#41789 = CARTESIAN_POINT ( 'NONE',  ( -1.193521905106661674, 2.660739321503277841E-15, -0.3464511005275191513 ) ) ;
#41790 = CARTESIAN_POINT ( 'NONE',  ( -0.03443470937339728616, 0.2929341459200028863, -1.635441089090149402 ) ) ;
#41791 = CARTESIAN_POINT ( 'NONE',  ( -0.3917322834645670104, -0.1049643490035307020, -1.774953698983938954 ) ) ;
#41792 = CARTESIAN_POINT ( 'NONE',  ( 0.9317585301837276734, 0.05413385826771626580, -0.4176697321401330321 ) ) ;
#41793 = CARTESIAN_POINT ( 'NONE',  ( 0.07217847769028949700, -0.05778040916215560624, -0.4822834645669293319 ) ) ;
#41794 = CARTESIAN_POINT ( 'NONE',  ( -0.9711286089238838626, 0.2306618581243847221, -0.2411417322834647770 ) ) ;
#41795 = CARTESIAN_POINT ( 'NONE',  ( 1.069553805774278610, -0.6692913385826771977, 0.1292274648535927661 ) ) ;
#41796 = CARTESIAN_POINT ( 'NONE',  ( 0.4199475065616805614, 0.2306618581243848609, 0.2411417322834645549 ) ) ;
#41797 = CARTESIAN_POINT ( 'NONE',  ( 0.3917322834645670104, 2.398668435337828261E-17, -0.8326771653543307838 ) ) ;
#41798 = CARTESIAN_POINT ( 'NONE',  ( -0.4527559055118102749, 0.1660481256975885056, 0.3530559997133364547 ) ) ;
#41799 = CARTESIAN_POINT ( 'NONE',  ( 0.7742782152230979209, 0.05413385826771626580, -0.4176697321401330321 ) ) ;
#41800 = CARTESIAN_POINT ( 'NONE',  ( -0.05905511811023545637, 0.1660481256975885056, 0.3530559997133364547 ) ) ;
#41801 = CARTESIAN_POINT ( 'NONE',  ( 0.7545931758530189937, 0.1771653543307087075, -0.09757992244046823083 ) ) ;
#41802 = CARTESIAN_POINT ( 'NONE',  ( -1.430446194225721390, -0.4281496062992124485, 0.4176697321401328655 ) ) ;
#41803 = CARTESIAN_POINT ( 'NONE',  ( -1.686351706036744558, 0.2952755905511810774, -0.1292274648535930714 ) ) ;
#41804 = CARTESIAN_POINT ( 'NONE',  ( 0.4527559055118117182, -0.5400638737290844871, 0.3530559997133364547 ) ) ;
#41805 = EDGE_CURVE ( 'NONE', #71856, #73064, #4911, .T. ) ;
#41806 = CARTESIAN_POINT ( 'NONE',  ( 0.2867679344610365999, 0.2867679344610365999, -2.334645669291338432 ) ) ;
#41807 = VERTEX_POINT ( 'NONE', #35373 ) ;
#41808 = VERTEX_POINT ( 'NONE', #64973 ) ;
#41809 = CARTESIAN_POINT ( 'NONE',  ( 1.161417322834646493, -0.5400638737290844871, 0.3530559997133364547 ) ) ;
#41810 = CARTESIAN_POINT ( 'NONE',  ( 0.4527559055118117182, -0.4536011799217367080, 0.2665933059059888421 ) ) ;
#41812 = DIRECTION ( 'NONE',  ( -3.491481338843132961E-15, -0.000000000000000000, 1.000000000000000000 ) ) ;
#41811 = LINE ( 'NONE', #20916, #33728 ) ;
#41813 = CARTESIAN_POINT ( 'NONE',  ( 0.2867679344610365999, 0.2867679344610365999, -0.8523622047244096001 ) ) ;
#41814 = CARTESIAN_POINT ( 'NONE',  ( -0.4744094488189106174, 1.537401574803149984, 3.908320185825790105 ) ) ;
#41815 = SURFACE_STYLE_FILL_AREA ( #9842 ) ;
#41816 = CARTESIAN_POINT ( 'NONE',  ( -0.3917322834645671215, 0.1049643490035301469, -1.377296587926508664 ) ) ;
#41817 = CARTESIAN_POINT ( 'NONE',  ( -0.3996062992125986590, 0.1070741851644051723, -2.471784776902887337 ) ) ;
#41818 = CARTESIAN_POINT ( 'NONE',  ( 0.9973753280839902091, 0.2306618581243847221, -0.2411417322834647770 ) ) ;
#41819 = CARTESIAN_POINT ( 'NONE',  ( -0.7020997375328074108, -0.05778040916215522460, 0.4822834645669289988 ) ) ;
#41820 = CARTESIAN_POINT ( 'NONE',  ( -0.8530183727034112984, -0.4281496062992127816, -0.4176697321401328100 ) ) ;
#41821 = CARTESIAN_POINT ( 'NONE',  ( 0.6758530183727039509, 0.2952755905511810774, -0.1292274648535930714 ) ) ;
#41822 = ORIENTED_EDGE ( 'NONE', *, *, #38303, .F. ) ;
#41823 = CIRCLE ( 'NONE', #47171, 1.122047244094488194 ) ;
#41824 = CARTESIAN_POINT ( 'NONE',  ( 1.259842519685040019, -0.1870078740157479769, 0.4822834645669291653 ) ) ;
#41825 = CARTESIAN_POINT ( 'NONE',  ( -1.028258860871784197, 1.383740025641660543, 0.4491090030276655432 ) ) ;
#41826 = PRODUCT_CONTEXT ( 'NONE', #9492, 'mechanical' ) ;
#41827 = DIRECTION ( 'NONE',  ( 1.000000000000000000, -0.000000000000000000, -0.000000000000000000 ) ) ;
#41828 = CARTESIAN_POINT ( 'NONE',  ( -3.937007874015748143, 2.559055118110236560, 0.3149606299212596716 ) ) ;
#41829 = CARTESIAN_POINT ( 'NONE',  ( -1.187664041994749731, -0.2845877964562159024, 0.3641732283464567677 ) ) ;
#41830 = CARTESIAN_POINT ( 'NONE',  ( -0.3917322834645669549, -0.1049643490035306603, 0.1194225721784776956 ) ) ;
#41831 = CARTESIAN_POINT ( 'NONE',  ( 0.1181102362204730916, 0.2952755905511811885, 0.000000000000000000 ) ) ;
#41833 = DIRECTION ( 'NONE',  ( -0.000000000000000000, -1.000000000000000000, -0.000000000000000000 ) ) ;
#41832 = CARTESIAN_POINT ( 'NONE',  ( 1.555118110236221041, 0.1660481256975883668, -0.3530559997133364547 ) ) ;
#41834 = CARTESIAN_POINT ( 'NONE',  ( -1.286089238845143479, -0.5023911411419708095, 0.1820866141732285504 ) ) ;
#41835 = CARTESIAN_POINT ( 'NONE',  ( 0.2230971128608932319, -0.4281496062992124485, 0.4176697321401328655 ) ) ;
#41836 = CARTESIAN_POINT ( 'NONE',  ( 1.167979002624672580, -0.004921259842519870586, -0.3153832671262229437 ) ) ;
#41837 = CARTESIAN_POINT ( 'NONE',  ( 0.1958661417322836162, -0.3392501089628018329, -1.431739214401887894 ) ) ;
#41838 = CARTESIAN_POINT ( 'NONE',  ( -1.266404199475064773, -0.2845877964562159024, 0.3641732283464567677 ) ) ;
#41839 = CARTESIAN_POINT ( 'NONE',  ( 1.568241469816273659, -0.05778040916215560624, -0.4822834645669293319 ) ) ;
#41840 = CARTESIAN_POINT ( 'NONE',  ( 0.2710477321170861043, 1.856769674693915295, 0.1570371412841552461 ) ) ;
#41841 = CARTESIAN_POINT ( 'NONE',  ( -0.3477690288713905509, -0.6692913385826771977, 0.1292274648535927661 ) ) ;
#41842 = CARTESIAN_POINT ( 'NONE',  ( -1.456692913385826182, 0.1771653543307087630, 0.000000000000000000 ) ) ;
#41843 = CARTESIAN_POINT ( 'NONE',  ( -0.5118110236220466680, -0.5511811023622047445, 6.969142054262312111E-17 ) ) ;
#41844 = VECTOR ( 'NONE', #7052, 39.37007874015748143 ) ;
#41845 = CARTESIAN_POINT ( 'NONE',  ( -0.6496062992125976043, -0.5400638737290844871, 0.3530559997133364547 ) ) ;
#41846 = CARTESIAN_POINT ( 'NONE',  ( -1.574803149606298192, -0.1870078740157480601, -0.3641732283464567677 ) ) ;
#41847 = CARTESIAN_POINT ( 'NONE',  ( -0.2867679344610367109, 0.2867679344610365444, -0.6463447750994246732 ) ) ;
#41848 = CARTESIAN_POINT ( 'NONE',  ( 0.3477690288713918276, 0.2952755905511811885, 0.1292274648535926551 ) ) ;
#41849 = DIRECTION ( 'NONE',  ( 0.000000000000000000, 1.000000000000000000, 0.000000000000000000 ) ) ;
#41850 = CARTESIAN_POINT ( 'NONE',  ( -0.2362204724409447953, -0.4091458600556404646, -2.032152230971128848 ) ) ;
#41851 = CARTESIAN_POINT ( 'NONE',  ( -1.154855643044618851, -0.6046776061558809534, -0.2411417322834644161 ) ) ;
#41852 = CARTESIAN_POINT ( 'NONE',  ( -0.6561679790026240244, -0.5023911411419708095, 0.1820866141732285504 ) ) ;
#41853 = CARTESIAN_POINT ( 'NONE',  ( 1.171093442848939681, -8.644661201599092366E-16, -0.4445507791589066171 ) ) ;
#41854 = CARTESIAN_POINT ( 'NONE',  ( 0.2230971128608932319, -0.4281496062992124485, 0.4176697321401328655 ) ) ;
#41855 = CARTESIAN_POINT ( 'NONE',  ( 0.2624671916010504757, 0.1283753931104748280, 0.1820866141732283561 ) ) ;
#41856 = CARTESIAN_POINT ( 'NONE',  ( -0.6430446194225716283, -0.3690944881889763329, 0.3153832671262228327 ) ) ;
#41857 = CARTESIAN_POINT ( 'NONE',  ( -1.332020997375327642, -0.3162353388693409650, -0.4822834645669289433 ) ) ;
#41858 = CARTESIAN_POINT ( 'NONE',  ( -1.397637795275589623, 0.1660481256975885056, 0.3530559997133364547 ) ) ;
#41859 = CARTESIAN_POINT ( 'NONE',  ( 1.318897637795276356, -0.5400638737290844871, 0.3530559997133364547 ) ) ;
#41860 = DIRECTION ( 'NONE',  ( -3.491481338843132961E-15, -0.000000000000000000, 1.000000000000000000 ) ) ;
#41861 = CARTESIAN_POINT ( 'NONE',  ( 0.5314960629921267055, -0.4536011799217367080, 0.2665933059059888421 ) ) ;
#41862 = CARTESIAN_POINT ( 'NONE',  ( 0.9645669291338591078, -0.5400638737290845981, -0.3530559997133363437 ) ) ;
#41863 = CARTESIAN_POINT ( 'NONE',  ( 0.7086614173228347191, 0.000000000000000000, 0.000000000000000000 ) ) ;
#41864 = CARTESIAN_POINT ( 'NONE',  ( 1.377952755905512472, -0.5511811023622047445, 6.969142054262312111E-17 ) ) ;
#41865 = VERTEX_POINT ( 'NONE', #61038 ) ;
#41867 = B_SPLINE_CURVE_WITH_KNOTS ( 'NONE', 3,
 ( #58980, #19847, #3401, #34974 ),
 .UNSPECIFIED., .F., .F.,
 ( 4, 4 ),
 ( 0.02793953716399259421, 0.02824248980525632252 ),
 .UNSPECIFIED. ) ;
#41866 = CARTESIAN_POINT ( 'NONE',  ( -1.056430446194224881, -0.6692913385826771977, 0.1292274648535927661 ) ) ;
#41868 = CARTESIAN_POINT ( 'NONE',  ( -0.8398950131233585692, 0.2306618581243848609, 0.2411417322834645549 ) ) ;
#41869 = CARTESIAN_POINT ( 'NONE',  ( 0.1902887139107617975, 0.2952755905511811885, 0.1292274648535926551 ) ) ;
#41870 = CARTESIAN_POINT ( 'NONE',  ( -1.279527559055116948, -0.4536011799217367080, 0.2665933059059888421 ) ) ;
#41871 = CARTESIAN_POINT ( 'NONE',  ( -0.3996062992125984925, -0.1070741851644056858, -2.169947506561679340 ) ) ;
#41872 = CARTESIAN_POINT ( 'NONE',  ( 1.535433070866142335, -0.5511811023622047445, 6.969142054262312111E-17 ) ) ;
#41873 = CARTESIAN_POINT ( 'NONE',  ( 0.5577427821522316087, -0.05778040916215522460, 0.4822834645669289988 ) ) ;
#41874 = CARTESIAN_POINT ( 'NONE',  ( 0.7152230971128614723, -0.3162353388693409650, -0.4822834645669289433 ) ) ;
#41875 = CARTESIAN_POINT ( 'NONE',  ( 1.535433070866142558, 0.2952755905511811885, 0.000000000000000000 ) ) ;
#41876 = CARTESIAN_POINT ( 'NONE',  ( 0.2925321140481932369, -0.2925321140481932369, -1.673228346456692828 ) ) ;
#41877 = CARTESIAN_POINT ( 'NONE',  ( 0.3420746716998659953, 0.1974969037888705536, -0.9186351706036742781 ) ) ;
#41878 = CARTESIAN_POINT ( 'NONE',  ( 0.3996062992125986035, 0.1070741851644054776, -2.486876640419947382 ) ) ;
#41879 = CARTESIAN_POINT ( 'NONE',  ( -0.1228903193441467367, -0.2686849592492765448, 0.1574803149606299191 ) ) ;
#41880 = CARTESIAN_POINT ( 'NONE',  ( -0.3917322834645669549, -0.1049643490035306603, -0.03805774278215218187 ) ) ;
#41881 = CARTESIAN_POINT ( 'NONE',  ( -0.1837270341207343505, -0.5023911411419708095, 0.1820866141732285504 ) ) ;
#41882 = AXIS2_PLACEMENT_3D ( 'NONE', #65852, #51518, #8185 ) ;
#41883 = CARTESIAN_POINT ( 'NONE',  ( -0.1771653543307080136, -0.5400638737290844871, 0.3530559997133364547 ) ) ;
#41884 = CARTESIAN_POINT ( 'NONE',  ( 0.8792650918635177559, -0.4281496062992127816, -0.4176697321401328100 ) ) ;
#41885 = CARTESIAN_POINT ( 'NONE',  ( -0.3949938075777409963, -7.255918531996591613E-17, -2.320866141732283339 ) ) ;
#41886 = CARTESIAN_POINT ( 'NONE',  ( -0.1902887139107604098, 0.1771653543307087075, -0.09757992244046823083 ) ) ;
#41887 = CARTESIAN_POINT ( 'NONE',  ( -1.259842519685038686, -0.1870078740157480879, -0.4822834645669291653 ) ) ;
#41888 = CARTESIAN_POINT ( 'NONE',  ( 1.135170603674541256, 0.2952755905511811885, 0.1292274648535926551 ) ) ;
#41889 = CARTESIAN_POINT ( 'NONE',  ( 0.4724409448818896462, 0.1265901696524990294, -2.329396325459317296 ) ) ;
#41890 = CARTESIAN_POINT ( 'NONE',  ( 0.3460692066303959757, -0.1998031496062991907, -1.679790026246719137 ) ) ;
#41891 = CARTESIAN_POINT ( 'NONE',  ( 0.4498537592782897998, 0.000000000000000000, -2.118110236220472675 ) ) ;
#41892 = ORIENTED_EDGE ( 'NONE', *, *, #40415, .F. ) ;
#41893 = VERTEX_POINT ( 'NONE', #45169 ) ;
#41894 = CARTESIAN_POINT ( 'NONE',  ( 0.8530183727034126306, 0.05413385826771626580, -0.4176697321401330321 ) ) ;
#41895 = CARTESIAN_POINT ( 'NONE',  ( 1.614173228346457378, 0.1771653543307087630, 0.000000000000000000 ) ) ;
#41897 = CARTESIAN_POINT ( 'NONE',  ( -1.633858267716534529, 0.1660481256975885056, 0.3530559997133364547 ) ) ;
#41896 = CARTESIAN_POINT ( 'NONE',  ( -1.469816272965878357, 0.1283753931104748280, 0.1820866141732283561 ) ) ;
#41898 = CARTESIAN_POINT ( 'NONE',  ( -0.1958661417322836718, 0.3392501089628017219, 0.2171916010498686767 ) ) ;
#41899 = FACE_OUTER_BOUND ( 'NONE', #2999, .T. ) ;
#41900 = CARTESIAN_POINT ( 'NONE',  ( 1.325459317585302665, -0.4281496062992124485, 0.4176697321401328655 ) ) ;
#41901 = CARTESIAN_POINT ( 'NONE',  ( -1.456692913385826182, -0.6692913385826771977, 8.415575281601705876E-17 ) ) ;
#41902 = CARTESIAN_POINT ( 'NONE',  ( 0.04593175853018440641, 0.2952755905511810774, -0.1292274648535930714 ) ) ;
#41903 = CARTESIAN_POINT ( 'NONE',  ( -0.7349081364829390672, 0.2306618581243847221, -0.2411417322834647770 ) ) ;
#41904 = CARTESIAN_POINT ( 'NONE',  ( -1.614173228346455824, 0.2952755905511811885, 0.000000000000000000 ) ) ;
#41905 = CARTESIAN_POINT ( 'NONE',  ( -0.3392501089628019995, 0.1958661417322832277, -0.1108923884514436548 ) ) ;
#41906 = CARTESIAN_POINT ( 'NONE',  ( 0.03937007874015806264, 0.2952755905511811885, 0.000000000000000000 ) ) ;
#41907 = CARTESIAN_POINT ( 'NONE',  ( -0.2867679344610365999, 0.2867679344610364889, -2.216535433070866201 ) ) ;
#41908 = CARTESIAN_POINT ( 'NONE',  ( -1.174540682414697335, -0.08942795157527998196, 0.3641732283464567121 ) ) ;
#41909 = ORIENTED_EDGE ( 'NONE', *, *, #30007, .F. ) ;
#41910 = CARTESIAN_POINT ( 'NONE',  ( 0.2891555358219910499, -0.2891555358219909944, -2.145669291338582862 ) ) ;
#41911 = ORIENTED_EDGE ( 'NONE', *, *, #74772, .F. ) ;
#41912 = CARTESIAN_POINT ( 'NONE',  ( 0.3149606299212184823, 2.165354330708661568, 3.924389226575471845 ) ) ;
#41913 = CARTESIAN_POINT ( 'NONE',  ( -1.568241469816272105, -0.05778040916215522460, 0.4822834645669289988 ) ) ;
#41914 = CARTESIAN_POINT ( 'NONE',  ( -0.3996062992125987146, 0.1070741851644051862, -1.135170603674540590 ) ) ;
#41915 = CARTESIAN_POINT ( 'NONE',  ( 1.646981627296588035, -0.2845877964562159024, 0.3641732283464567677 ) ) ;
#41916 = CARTESIAN_POINT ( 'NONE',  ( -1.706036745406823485, 0.2306618581243848609, 0.2411417322834645549 ) ) ;
#41917 = DIRECTION ( 'NONE',  ( 0.000000000000000000, 1.408710688920637755E-15, -1.000000000000000000 ) ) ;
#41918 = CARTESIAN_POINT ( 'NONE',  ( 0.001150535885519430191, -0.3985446848723403490, -2.755905511811024500 ) ) ;
#41919 = EDGE_CURVE ( 'NONE', #27207, #69303, #32558, .T. ) ;
#41920 = CARTESIAN_POINT ( 'NONE',  ( 0.2867679344610365999, 0.2867679344610365999, 0.09251968503937001154 ) ) ;
#41921 = CARTESIAN_POINT ( 'NONE',  ( -0.1312335958005241554, -0.5023911411419708095, -0.1820866141732282451 ) ) ;
#41922 = CARTESIAN_POINT ( 'NONE',  ( -0.8858267716535425107, 0.07958543189024071263, -0.2665933059059888421 ) ) ;
#41923 = CARTESIAN_POINT ( 'NONE',  ( -1.358267716535432434, -0.5400638737290844871, 0.3530559997133364547 ) ) ;
#41924 = EDGE_CURVE ( 'NONE', #1065, #20923, #2072, .T. ) ;
#41925 = CARTESIAN_POINT ( 'NONE',  ( 0.3805774278215230400, 0.05413385826771626580, -0.4176697321401330321 ) ) ;
#41926 = CARTESIAN_POINT ( 'NONE',  ( -1.430446194225720724, 0.05413385826771626580, -0.4176697321401330321 ) ) ;
#41927 = CARTESIAN_POINT ( 'NONE',  ( 0.3392501089628018884, -0.1958661417322834220, 0.06036745406824151755 ) ) ;
#41928 = ORIENTED_EDGE ( 'NONE', *, *, #79506, .T. ) ;
#41929 = CARTESIAN_POINT ( 'NONE',  ( -1.574803149606298192, -0.1870078740157480879, -0.4822834645669291653 ) ) ;
#41930 = CARTESIAN_POINT ( 'NONE',  ( -1.646051170424378096, 0.000000000000000000, 0.3464511005275205946 ) ) ;
#41931 = CARTESIAN_POINT ( 'NONE',  ( 5.785732909357575061E-17, -0.4724409448818898682, -1.496062992125984259 ) ) ;
#41932 = CARTESIAN_POINT ( 'NONE',  ( 2.077234194078037000, 1.326002914239475805, -0.4256865378621398355 ) ) ;
#41933 = CARTESIAN_POINT ( 'NONE',  ( 0.3917322834645669549, 0.1049643490035304660, -0.7467191601049868455 ) ) ;
#41934 = CARTESIAN_POINT ( 'NONE',  ( -0.3392501089628017219, -0.1958661417322836718, -2.656824146981627166 ) ) ;
#41935 = CARTESIAN_POINT ( 'NONE',  ( -0.7020997375328074108, -0.05778040916215522460, 0.4822834645669289988 ) ) ;
#41936 = CARTESIAN_POINT ( 'NONE',  ( 1.535433070866142558, 0.2952755905511811885, 0.000000000000000000 ) ) ;
#41938 = CARTESIAN_POINT ( 'NONE',  ( -0.4724409448818898682, -8.678599364036362592E-17, -0.1968503937007874127 ) ) ;
#41937 = CARTESIAN_POINT ( 'NONE',  ( -1.686351706036744558, 0.2952755905511810774, -0.1292274648535930714 ) ) ;
#41939 = CARTESIAN_POINT ( 'NONE',  ( -1.561679790026246017, 0.05413385826771666132, 0.4176697321401328100 ) ) ;
#41940 = CARTESIAN_POINT ( 'NONE',  ( -1.003937007874015297, -0.5400638737290845981, -0.3530559997133363437 ) ) ;
#41941 = CARTESIAN_POINT ( 'NONE',  ( -0.3917322834645669549, -7.196005306013483243E-17, -0.1194032563966385962 ) ) ;
#41942 = CARTESIAN_POINT ( 'NONE',  ( 0.03937007874015806264, 0.1771653543307087630, 0.000000000000000000 ) ) ;
#41943 = CARTESIAN_POINT ( 'NONE',  ( -0.3917322834645669549, -0.1049643490035306603, -0.4455380577427822120 ) ) ;
#41944 = CARTESIAN_POINT ( 'NONE',  ( 0.01968503937007957949, -0.4536011799217368745, -0.2665933059059886201 ) ) ;
#41945 = CARTESIAN_POINT ( 'NONE',  ( 0.9186351706036751663, -0.5023911411419708095, 0.1820866141732285504 ) ) ;
#41946 = CARTESIAN_POINT ( 'NONE',  ( 0.4986876640419954376, 0.2306618581243848609, 0.2411417322834645549 ) ) ;
#41947 = PRODUCT_DEFINITION_CONTEXT ( 'detailed design', #6766, 'design' ) ;
#41948 = CARTESIAN_POINT ( 'NONE',  ( -0.3543307086614165824, 0.1771653543307087630, 0.000000000000000000 ) ) ;
#41949 = CARTESIAN_POINT ( 'NONE',  ( 0.1049643490035303689, 0.3917322834645670104, -2.347769028871391050 ) ) ;
#41950 = CARTESIAN_POINT ( 'NONE',  ( 1.601049868766404982, 0.2306618581243848609, 0.2411417322834645549 ) ) ;
#41951 = EDGE_CURVE ( 'NONE', #8180, #55534, #13516, .T. ) ;
#41952 = CARTESIAN_POINT ( 'NONE',  ( -1.423884514435694859, -0.08942795157528024563, -0.3641732283464568787 ) ) ;
#41953 = CARTESIAN_POINT ( 'NONE',  ( 0.4724409448818898682, 2.892866454678787531E-17, -0.1948818897637795422 ) ) ;
#41954 = CARTESIAN_POINT ( 'NONE',  ( 0.2034120734908142214, 0.2952755905511810774, -0.1292274648535930714 ) ) ;
#41955 = CARTESIAN_POINT ( 'NONE',  ( -0.6299212598425188991, -0.1870078740157480879, -0.4822834645669291653 ) ) ;
#41956 = FACE_OUTER_BOUND ( 'NONE', #6941, .T. ) ;
#41957 = EDGE_CURVE ( 'NONE', #51378, #53614, #4664, .T. ) ;
#41958 = CARTESIAN_POINT ( 'NONE',  ( 0.5446194225721792126, -0.08942795157528024563, -0.3641732283464568787 ) ) ;
#41959 = CARTESIAN_POINT ( 'NONE',  ( -0.07874015748031421014, -0.1870078740157480601, -0.3641732283464567677 ) ) ;
#41960 = CARTESIAN_POINT ( 'NONE',  ( -0.5249343832020990641, 0.2306618581243848609, 0.2411417322834645549 ) ) ;
#41961 = CARTESIAN_POINT ( 'NONE',  ( -3.892860353355074299, 2.712196231959916659, 0.5314960629921260393 ) ) ;
#41962 = CARTESIAN_POINT ( 'NONE',  ( 0.1938976377952755792, -0.1938976377952756069, 0.07874015748031495954 ) ) ;
#41963 = CARTESIAN_POINT ( 'NONE',  ( 0.2624671916010504757, 0.2306618581243848609, 0.2411417322834645549 ) ) ;
#41964 = CARTESIAN_POINT ( 'NONE',  ( -0.1998031496062994405, 0.3460692066303957537, -1.507217847769029007 ) ) ;
#41965 = ADVANCED_FACE ( 'NONE', ( #11829 ), #36652, .T. ) ;
#41966 = CARTESIAN_POINT ( 'NONE',  ( 1.496062992125984703, -0.1870078740157480879, -0.4822834645669291653 ) ) ;
#41967 = CARTESIAN_POINT ( 'NONE',  ( -0.2690288713910754526, 0.1771653543307087075, -0.09757992244046823083 ) ) ;
#41968 = CARTESIAN_POINT ( 'NONE',  ( -0.6036745406824141069, 0.2306618581243848609, 0.2411417322834645549 ) ) ;
#41969 = CARTESIAN_POINT ( 'NONE',  ( -1.581364829396324945, -0.08942795157528024563, -0.3641732283464568787 ) ) ;
#41970 = CARTESIAN_POINT ( 'NONE',  ( 1.286089238845145033, -0.6046776061558809534, -0.2411417322834644161 ) ) ;
#41971 = LINE ( 'NONE', #62577, #74791 ) ;
#41972 = CARTESIAN_POINT ( 'NONE',  ( -0.7939632545931754048, -0.2845877964562159024, 0.3641732283464567677 ) ) ;
#41973 = CARTESIAN_POINT ( 'NONE',  ( 4.893765752498283308E-17, -0.3996062992125985480, -0.1555118110236220763 ) ) ;
#41974 = CARTESIAN_POINT ( 'NONE',  ( 0.1070741851644054915, -0.3996062992125986035, -0.5577427821522309426 ) ) ;
#41975 = CARTESIAN_POINT ( 'NONE',  ( -0.3949938075777409408, -0.1058382717557502933, 0.1115485564304461441 ) ) ;
#41976 = CARTESIAN_POINT ( 'NONE',  ( 1.614173228346457378, -0.5511811023622047445, 6.969142054262312111E-17 ) ) ;
#41977 = CARTESIAN_POINT ( 'NONE',  ( 1.069553805774278610, -0.5511811023622046335, 0.09757992244046803654 ) ) ;
#41978 = CARTESIAN_POINT ( 'NONE',  ( 0.9908136482939640111, 0.2952755905511810774, -0.1292274648535930714 ) ) ;
#41979 = CARTESIAN_POINT ( 'NONE',  ( 0.4596682205436344870, 0.004960608223779807216, -0.3437734562760184631 ) ) ;
#41980 = CARTESIAN_POINT ( 'NONE',  ( 0.9317585301837276734, -0.4281496062992124485, 0.4176697321401328655 ) ) ;
#41981 = CARTESIAN_POINT ( 'NONE',  ( -0.3420746716998662729, 0.1974969037888702206, -1.047900262467191590 ) ) ;
#41982 = CARTESIAN_POINT ( 'NONE',  ( 1.023622047244095334, -0.1870078740157479769, 0.3641732283464567677 ) ) ;
#41983 = CARTESIAN_POINT ( 'NONE',  ( 0.2099737532808405305, -0.6046776061558807314, 0.2411417322834647770 ) ) ;
#41984 = CARTESIAN_POINT ( 'NONE',  ( -0.6167979002624665030, -0.4281496062992127816, -0.4176697321401328100 ) ) ;
#41985 = CARTESIAN_POINT ( 'NONE',  ( 1.607611548556431069, -0.6692913385826773087, -0.1292274648535924053 ) ) ;
#41986 = CARTESIAN_POINT ( 'NONE',  ( 0.2362204724409451007, -0.4091458600556402980, -1.194225721784776928 ) ) ;
#41987 = CARTESIAN_POINT ( 'NONE',  ( 0.3996062992125986035, -0.1070741851644053111, -2.158792650918635037 ) ) ;
#41988 = CARTESIAN_POINT ( 'NONE',  ( 0.4921259842519691285, 0.07958543189024085140, 0.2665933059059887866 ) ) ;
#41989 = ORIENTED_EDGE ( 'NONE', *, *, #76459, .T. ) ;
#41990 = CARTESIAN_POINT ( 'NONE',  ( -9.594673741351313045E-17, 0.3917322834645670659, -0.3116991058080859078 ) ) ;
#41991 = ORIENTED_EDGE ( 'NONE', *, *, #13707, .F. ) ;
#41992 = CIRCLE ( 'NONE', #19156, 0.5118110236220471121 ) ;
#41993 = CARTESIAN_POINT ( 'NONE',  ( -0.5118110236220466680, -0.6692913385826771977, 8.415575281601705876E-17 ) ) ;
#41994 = CARTESIAN_POINT ( 'NONE',  ( -0.2296587926509179312, -0.05778040916215522460, 0.4822834645669289988 ) ) ;
#41995 = CARTESIAN_POINT ( 'NONE',  ( -0.4199475065616791736, -0.6046776061558807314, 0.2411417322834647770 ) ) ;
#41996 = CARTESIAN_POINT ( 'NONE',  ( 0.5905511811023629321, 0.2952755905511811885, 0.000000000000000000 ) ) ;
#41997 = CARTESIAN_POINT ( 'NONE',  ( -0.9120734908136475250, -0.6692913385826773087, -0.1292274648535924053 ) ) ;
#41998 = CARTESIAN_POINT ( 'NONE',  ( -0.2099737532808391705, -0.6046776061558809534, -0.2411417322834644161 ) ) ;
#41999 = CARTESIAN_POINT ( 'NONE',  ( 1.220472440944882386, -0.6692913385826771977, 8.415575281601705876E-17 ) ) ;
#42000 = CIRCLE ( 'NONE', #5705, 0.2165354330708659791 ) ;
#42001 = CARTESIAN_POINT ( 'NONE',  ( 0.9645669291338588858, 0.1660481256975885056, 0.3530559997133364547 ) ) ;
#42002 = CARTESIAN_POINT ( 'NONE',  ( 0.6758530183727039509, -0.6692913385826771977, 0.1292274648535927661 ) ) ;
#42003 = CARTESIAN_POINT ( 'NONE',  ( -0.1049643490035307020, 0.3917322834645669549, -1.101049868766403872 ) ) ;
#42004 = CARTESIAN_POINT ( 'NONE',  ( -0.04593175853018302557, 0.1771653543307087630, 0.09757992244046791164 ) ) ;
#42005 = EDGE_LOOP ( 'NONE', ( #32268, #44777, #53240, #31043 ) ) ;
#42006 = CARTESIAN_POINT ( 'NONE',  ( -0.2891555358219908833, -0.2891555358219912164, -1.161417322834645827 ) ) ;
#42007 = EDGE_LOOP ( 'NONE', ( #75211, #20066, #68588, #17411 ) ) ;
#42008 = CARTESIAN_POINT ( 'NONE',  ( -0.6758530183727028406, -0.5511811023622048555, -0.09757992244046775898 ) ) ;
#42009 = CARTESIAN_POINT ( 'NONE',  ( -0.6692913385826764205, 0.2952755905511811885, 0.000000000000000000 ) ) ;
#42010 = CARTESIAN_POINT ( 'NONE',  ( -2.362204724409448620, 1.929133858267716661, -0.5118110236220719811 ) ) ;
#42011 = CARTESIAN_POINT ( 'NONE',  ( -0.7414698162729651543, 0.2952755905511810774, -0.1292274648535930714 ) ) ;
#42012 = CARTESIAN_POINT ( 'NONE',  ( -0.4396325459317579898, 0.2952755905511811885, 0.1292274648535926551 ) ) ;
#42013 = CARTESIAN_POINT ( 'NONE',  ( -1.187664041994749731, -0.3162353388693405765, 0.4822834645669290543 ) ) ;
#42014 = EDGE_CURVE ( 'NONE', #15840, #4749, #64136, .T. ) ;
#42015 = CARTESIAN_POINT ( 'NONE',  ( -1.312335958005248715, -0.6046776061558809534, -0.2411417322834644161 ) ) ;
#42016 = CARTESIAN_POINT ( 'NONE',  ( 0.8923884514435703741, 0.1283753931104748280, 0.1820866141732283561 ) ) ;
#42017 = DIRECTION ( 'NONE',  ( 1.000000000000000000, -0.000000000000000000, -0.000000000000000000 ) ) ;
#42018 = PLANE ( 'NONE',  #74692 ) ;
#42019 = CARTESIAN_POINT ( 'NONE',  ( 0.2755905511811031494, -0.5511811023622047445, 6.969142054262312111E-17 ) ) ;
#42020 = CARTESIAN_POINT ( 'NONE',  ( -0.09186351706036663400, -0.4281496062992124485, 0.4176697321401328655 ) ) ;
#42021 = CARTESIAN_POINT ( 'NONE',  ( -0.1246719160104980823, -0.6692913385826773087, -0.1292274648535924053 ) ) ;
#42022 = EDGE_LOOP ( 'NONE', ( #51606, #1636 ) ) ;
#42023 = CARTESIAN_POINT ( 'NONE',  ( 0.1998031496062992740, 0.3460692066303959757, -1.719160104986876769 ) ) ;
#42024 = CARTESIAN_POINT ( 'NONE',  ( 1.076935383196057527, 2.165354330708661568, 0.3149606299212600047 ) ) ;
#42025 = EDGE_LOOP ( 'NONE', ( #48593, #29789, #20826, #57004 ) ) ;
#42026 = CARTESIAN_POINT ( 'NONE',  ( -0.3460692066303960313, 0.1998031496062989965, -1.047900262467191590 ) ) ;
#42027 = CARTESIAN_POINT ( 'NONE',  ( 1.522309711286089939, -0.6046776061558809534, -0.2411417322834644161 ) ) ;
#42028 = CARTESIAN_POINT ( 'NONE',  ( -0.8595800524934373854, -0.2845877964562161244, -0.3641732283464567121 ) ) ;
#42029 = CARTESIAN_POINT ( 'NONE',  ( -1.003937007874015297, -0.5400638737290845981, -0.3530559997133363437 ) ) ;
#42030 = CARTESIAN_POINT ( 'NONE',  ( 0.4724409448818898682, 2.892866454678787531E-17, -0.2755905511811023723 ) ) ;
#42031 =( BOUNDED_CURVE ( )  B_SPLINE_CURVE ( 3, ( #23779, #22129, #22953, #49034 ),
 .UNSPECIFIED., .F., .F. ) 
 B_SPLINE_CURVE_WITH_KNOTS ( ( 4, 4 ),
 ( 1.780411317419258177, 1.780674070178078994 ),
 .UNSPECIFIED. ) 
 CURVE ( )  GEOMETRIC_REPRESENTATION_ITEM ( )  RATIONAL_B_SPLINE_CURVE ( ( 1.000000000000000000, 0.9999999942467490133, 0.9999999942467490133, 1.000000000000000000 ) ) 
 REPRESENTATION_ITEM ( '' )  );
#42032 = CARTESIAN_POINT ( 'NONE',  ( 0.3392501089628018884, -0.1958661417322834220, -2.551837270341207109 ) ) ;
#42033 = CARTESIAN_POINT ( 'NONE',  ( -1.482939632545930975, -0.004921259842519576551, 0.3153832671262227771 ) ) ;
#42034 = CARTESIAN_POINT ( 'NONE',  ( 0.3477690288713918276, 0.2952755905511811885, 0.1292274648535926551 ) ) ;
#42035 = CARTESIAN_POINT ( 'NONE',  ( 0.6299212598425204535, -0.1870078740157480879, -0.4822834645669291653 ) ) ;
#42036 = CARTESIAN_POINT ( 'NONE',  ( -0.7152230971128602510, -0.2845877964562159024, 0.3641732283464567677 ) ) ;
#42037 = CARTESIAN_POINT ( 'NONE',  ( -0.03280839895013062252, -0.6692913385826771977, 0.1292274648535927661 ) ) ;
#42038 = CARTESIAN_POINT ( 'NONE',  ( -1.157146581871515012E-16, 0.4724409448818898682, -2.281496062992125928 ) ) ;
#42039 = CARTESIAN_POINT ( 'NONE',  ( -0.4396325459317577122, -0.5511811023622048555, -0.09757992244046775898 ) ) ;
#42040 = CARTESIAN_POINT ( 'NONE',  ( -0.5249343832020990641, -0.6046776061558809534, -0.2411417322834644161 ) ) ;
#42041 = CARTESIAN_POINT ( 'NONE',  ( 0.3949938075777409408, -0.1058382717557499186, -1.920603674540682260 ) ) ;
#42042 = CARTESIAN_POINT ( 'NONE',  ( -1.522309711286088607, 0.2306618581243847221, -0.2411417322834647770 ) ) ;
#42043 = CARTESIAN_POINT ( 'NONE',  ( -0.006561679790025524116, -0.2845877964562159024, 0.3641732283464567677 ) ) ;
#42044 = CARTESIAN_POINT ( 'NONE',  ( 1.148293963254593875, -0.5511811023622046335, 0.09757992244046803654 ) ) ;
#42045 = CARTESIAN_POINT ( 'NONE',  ( -1.312335958005248715, -0.6046776061558809534, -0.2411417322834644161 ) ) ;
#42046 = CARTESIAN_POINT ( 'NONE',  ( -0.7283464566929126471, -0.4536011799217367080, 0.2665933059059888421 ) ) ;
#42047 = CARTESIAN_POINT ( 'NONE',  ( -0.1265901696524993347, 0.4724409448818896462, -2.288057742782152015 ) ) ;
#42048 = CARTESIAN_POINT ( 'NONE',  ( -0.9711286089238838626, -0.6046776061558807314, 0.2411417322834647770 ) ) ;
#42049 = CARTESIAN_POINT ( 'NONE',  ( -0.5774278215223089816, -0.6046776061558807314, 0.2411417322834647770 ) ) ;
#42050 = CARTESIAN_POINT ( 'NONE',  ( 0.2755905511811031494, 0.2952755905511811885, 0.000000000000000000 ) ) ;
#42051 = CARTESIAN_POINT ( 'NONE',  ( 4.797336870675655290E-17, -0.3917322834645669549, -2.520978059546244765 ) ) ;
#42052 = CARTESIAN_POINT ( 'NONE',  ( -1.973869084197696910, 1.199841186584403863, -0.3336616047370135063 ) ) ;
#42053 = CARTESIAN_POINT ( 'NONE',  ( 0.4855643044619430415, -0.3690944881889765550, -0.3153832671262227771 ) ) ;
#42054 = CARTESIAN_POINT ( 'NONE',  ( 1.062992125984252745, -0.6692913385826771977, 8.415575281601705876E-17 ) ) ;
#42055 = CARTESIAN_POINT ( 'NONE',  ( -1.141732283464566011, -0.5511811023622047445, 6.969142054262312111E-17 ) ) ;
#42056 = CARTESIAN_POINT ( 'NONE',  ( 1.154855643044620184, -0.6046776061558807314, 0.2411417322834647770 ) ) ;
#42057 = CARTESIAN_POINT ( 'NONE',  ( -1.679790026246718693, 0.1283753931104746893, -0.1820866141732285504 ) ) ;
#42058 = VECTOR ( 'NONE', #40020, 39.37007874015748143 ) ;
#42059 = CARTESIAN_POINT ( 'NONE',  ( 1.601049868766404982, 0.1283753931104748280, 0.1820866141732283561 ) ) ;
#42060 = CARTESIAN_POINT ( 'NONE',  ( -1.003937007874015297, -0.5400638737290845981, -0.3530559997133363437 ) ) ;
#42061 = CARTESIAN_POINT ( 'NONE',  ( 0.03937007874015833325, -0.5511811023622047445, 6.969142054262312111E-17 ) ) ;
#42062 = FACE_OUTER_BOUND ( 'NONE', #66545, .T. ) ;
#42063 = CARTESIAN_POINT ( 'NONE',  ( 0.6233595800524939223, -0.2845877964562159024, 0.3641732283464567677 ) ) ;
#42064 = CARTESIAN_POINT ( 'NONE',  ( -0.06561679790026180015, 0.05413385826771666132, 0.4176697321401328100 ) ) ;
#42065 = CARTESIAN_POINT ( 'NONE',  ( -0.1998031496062994405, 0.3460692066303957537, -0.2473753280839895152 ) ) ;
#42066 = CARTESIAN_POINT ( 'NONE',  ( -1.233595800524933894, 0.2306618581243848609, 0.2411417322834645549 ) ) ;
#42067 = CARTESIAN_POINT ( 'NONE',  ( -9.594673741351313045E-17, 0.3917322834645670104, -1.659448818897637734 ) ) ;
#42068 = CARTESIAN_POINT ( 'NONE',  ( 1.062992125984252745, -0.5511811023622047445, 6.969142054262312111E-17 ) ) ;
#42069 = CARTESIAN_POINT ( 'NONE',  ( -0.09186351706036663400, -0.4281496062992124485, 0.4176697321401328655 ) ) ;
#42070 = CARTESIAN_POINT ( 'NONE',  ( -0.4002624671916004129, -0.3162353388693405765, 0.4822834645669290543 ) ) ;
#42071 = CARTESIAN_POINT ( 'NONE',  ( -0.3346456692913377662, 0.07958543189024071263, -0.2665933059059888421 ) ) ;
#42072 = CARTESIAN_POINT ( 'NONE',  ( 0.000000000000000000, 2.755905511811024056, 0.000000000000000000 ) ) ;
#42073 = CARTESIAN_POINT ( 'NONE',  ( -0.2755905511811015396, -0.5511811023622047445, 6.969142054262312111E-17 ) ) ;
#42074 = CARTESIAN_POINT ( 'NONE',  ( 0.3543307086614181922, -0.6692913385826771977, 8.415575281601705876E-17 ) ) ;
#42075 = CARTESIAN_POINT ( 'NONE',  ( -1.062992125984250968, 0.1771653543307087630, 0.000000000000000000 ) ) ;
#42076 = CARTESIAN_POINT ( 'NONE',  ( 0.1070741851644054776, -0.3996062992125984925, -1.106955380577427706 ) ) ;
#42077 = CARTESIAN_POINT ( 'NONE',  ( -1.345144356955379816, -0.3162353388693405765, 0.4822834645669290543 ) ) ;
#42078 = LINE ( 'NONE', #17666, #43413 ) ;
#42079 = ORIENTED_EDGE ( 'NONE', *, *, #82598, .F. ) ;
#42080 = CARTESIAN_POINT ( 'NONE',  ( -1.686351706036744558, 0.1771653543307087075, -0.09757992244046823083 ) ) ;
#42081 = CARTESIAN_POINT ( 'NONE',  ( -0.6299212598425188991, -0.1870078740157479769, 0.4822834645669291653 ) ) ;
#42082 = DIRECTION ( 'NONE',  ( 0.000000000000000000, -1.000000000000000000, 0.000000000000000000 ) ) ;
#42083 = CARTESIAN_POINT ( 'NONE',  ( -1.384514435695537005, -0.6692913385826773087, -0.1292274648535924053 ) ) ;
#42084 = CARTESIAN_POINT ( 'NONE',  ( -0.3392501089628019995, 0.1958661417322832277, -1.528215223097112885 ) ) ;
#42085 = CARTESIAN_POINT ( 'NONE',  ( 0.3594585737333455544, 0.1614515132151695398, -1.220472440944881720 ) ) ;
#42086 = CARTESIAN_POINT ( 'NONE',  ( 1.305774278215223960, -0.6692913385826771977, 0.1292274648535927661 ) ) ;
#42087 = CARTESIAN_POINT ( 'NONE',  ( 0.3412073490813655186, -0.6046776061558809534, -0.2411417322834644161 ) ) ;
#42088 = CARTESIAN_POINT ( 'NONE',  ( -0.3018372703412066094, 0.009842519685039463617, 0.3409548833797002576 ) ) ;
#42089 = CARTESIAN_POINT ( 'NONE',  ( -0.1070741851644057135, 0.3996062992125984925, -2.603018372703412187 ) ) ;
#42090 = CARTESIAN_POINT ( 'NONE',  ( -1.541994750656167090, 0.2952755905511811885, 0.1292274648535926551 ) ) ;
#42091 = CARTESIAN_POINT ( 'NONE',  ( -0.3996062992125986035, -0.1070741851644056997, -0.5183727034120735322 ) ) ;
#42092 = VERTEX_POINT ( 'NONE', #36250 ) ;
#42093 = CARTESIAN_POINT ( 'NONE',  ( -0.7349081364829387342, -0.5023911411419708095, 0.1820866141732285504 ) ) ;
#42094 = CARTESIAN_POINT ( 'NONE',  ( -0.3917322834645669549, -0.1049643490035306603, -2.242782152230970993 ) ) ;
#42095 = VERTEX_POINT ( 'NONE', #55587 ) ;
#42096 = CARTESIAN_POINT ( 'NONE',  ( 0.9383202099737536495, -0.3162353388693405765, 0.4822834645669290543 ) ) ;
#42097 = CARTESIAN_POINT ( 'NONE',  ( -0.2821522309711278487, 0.2952755905511811885, 0.1292274648535926551 ) ) ;
#42098 = CARTESIAN_POINT ( 'NONE',  ( -1.141732283464566011, 0.2952755905511811885, 0.000000000000000000 ) ) ;
#42099 = CARTESIAN_POINT ( 'NONE',  ( 1.161417322834646493, -0.5400638737290844871, 0.3530559997133364547 ) ) ;
#42100 = CARTESIAN_POINT ( 'NONE',  ( -1.292650918635170010, 0.1771653543307087075, -0.09757992244046823083 ) ) ;
#42101 = DIRECTION ( 'NONE',  ( -0.4043106043482690426, -0.6467352376403840974, -0.6467352376403910919 ) ) ;
#42102 = CARTESIAN_POINT ( 'NONE',  ( 0.4921259842519691285, -0.5400638737290845981, -0.3530559997133363437 ) ) ;
#42103 = CARTESIAN_POINT ( 'NONE',  ( -0.8464566929133852113, 0.1660481256975885056, 0.3530559997133364547 ) ) ;
#42104 = CARTESIAN_POINT ( 'NONE',  ( -0.3392501089628018329, -0.1958661417322836440, -1.392369135661730262 ) ) ;
#42105 = CARTESIAN_POINT ( 'NONE',  ( -1.266404199475064773, -0.05778040916215560624, -0.4822834645669293319 ) ) ;
#42106 = LINE ( 'NONE', #48831, #70808 ) ;
#42107 = CARTESIAN_POINT ( 'NONE',  ( 0.9514435695538062676, -0.3162353388693409650, -0.4822834645669289433 ) ) ;
#42108 = CARTESIAN_POINT ( 'NONE',  ( -0.2867679344610365999, 0.2867679344610364889, 0.1456692913385827237 ) ) ;
#42109 = CARTESIAN_POINT ( 'NONE',  ( 1.456692913385827515, -0.5511811023622047445, 6.969142054262312111E-17 ) ) ;
#42110 = ORIENTED_EDGE ( 'NONE', *, *, #39780, .F. ) ;
#42111 = CARTESIAN_POINT ( 'NONE',  ( 0.2867679344610366554, -0.2867679344610365999, -2.929809342028559360 ) ) ;
#42112 = CARTESIAN_POINT ( 'NONE',  ( -0.2690288713910754526, -0.6692913385826771977, 0.1292274648535927661 ) ) ;
#42113 = ORIENTED_EDGE ( 'NONE', *, *, #52589, .F. ) ;
#42114 = CARTESIAN_POINT ( 'NONE',  ( 0.3346456692913390985, 0.07958543189024085140, 0.2665933059059887866 ) ) ;
#42115 = CARTESIAN_POINT ( 'NONE',  ( -1.482939632545930975, -0.4281496062992127816, -0.4176697321401328100 ) ) ;
#42116 = CARTESIAN_POINT ( 'NONE',  ( 1.161417322834646271, 0.1660481256975883668, -0.3530559997133364547 ) ) ;
#42117 = CARTESIAN_POINT ( 'NONE',  ( 0.8530183727034126306, 0.05413385826771626580, -0.4176697321401330321 ) ) ;
#42118 = ADVANCED_FACE ( 'NONE', ( #10991 ), #17330, .T. ) ;
#42119 = CARTESIAN_POINT ( 'NONE',  ( -0.07217847769028813698, -0.3162353388693409650, -0.4822834645669289433 ) ) ;
#42120 = CIRCLE ( 'NONE', #5817, 0.1279527559055117503 ) ;
#42121 = CARTESIAN_POINT ( 'NONE',  ( -0.1049643490035307158, 0.3917322834645670104, -1.263142675361891731 ) ) ;
#42122 = CARTESIAN_POINT ( 'NONE',  ( -0.7939632545931750718, -0.05778040916215560624, -0.4822834645669293319 ) ) ;
#42123 = CARTESIAN_POINT ( 'NONE',  ( 0.2867679344610365999, 0.2867679344610365999, -2.427165354330708347 ) ) ;
#42124 = CARTESIAN_POINT ( 'NONE',  ( 1.607611548556431069, 0.1771653543307087630, 0.09757992244046791164 ) ) ;
#42125 = CARTESIAN_POINT ( 'NONE',  ( -1.115485564304461219, 0.05413385826771626580, -0.4176697321401330321 ) ) ;
#42126 = CARTESIAN_POINT ( 'NONE',  ( 1.443569553805774897, -0.6046776061558809534, -0.2411417322834644161 ) ) ;
#42127 = CARTESIAN_POINT ( 'NONE',  ( 0.3392501089628018884, -0.1958661417322834220, -2.931758530183726563 ) ) ;
#42128 = CARTESIAN_POINT ( 'NONE',  ( -0.8727034120734901146, -0.05778040916215560624, -0.4822834645669293319 ) ) ;
#42129 = CARTESIAN_POINT ( 'NONE',  ( -0.2925321140481930149, -0.2925321140481933480, 0.1791338582677165503 ) ) ;
#42130 = CARTESIAN_POINT ( 'NONE',  ( 0.2887139107611556010, -0.6046776061558807314, 0.2411417322834647770 ) ) ;
#42131 = CARTESIAN_POINT ( 'NONE',  ( -0.3460692066303960868, 0.1998031496062990242, -2.230971128608923770 ) ) ;
#42132 = CARTESIAN_POINT ( 'NONE',  ( -0.3543307086614165824, 0.2952755905511811885, 0.000000000000000000 ) ) ;
#42133 = CARTESIAN_POINT ( 'NONE',  ( -1.463254593175852492, 0.1771653543307087630, 0.09757992244046791164 ) ) ;
#42134 = CARTESIAN_POINT ( 'NONE',  ( 0.7545931758530189937, 0.1771653543307087075, -0.09757992244046823083 ) ) ;
#42135 = CARTESIAN_POINT ( 'NONE',  ( 1.318897637795276356, 0.1660481256975883668, -0.3530559997133364547 ) ) ;
#42136 = CARTESIAN_POINT ( 'NONE',  ( -0.4724409448818895907, -0.1265901696524993070, -1.225065616797899937 ) ) ;
#42137 = CARTESIAN_POINT ( 'NONE',  ( 0.6102362204724416372, 0.07958543189024071263, -0.2665933059059888421 ) ) ;
#42138 = CARTESIAN_POINT ( 'NONE',  ( 1.010498687664042716, 0.05413385826771626580, -0.4176697321401330321 ) ) ;
#42139 = CARTESIAN_POINT ( 'NONE',  ( 0.1974969037888706092, -0.3420746716998660508, -0.4835958005249345049 ) ) ;
#42140 = CARTESIAN_POINT ( 'NONE',  ( -0.5643044619422565855, 0.05413385826771626580, -0.4176697321401330321 ) ) ;
#42141 = DIRECTION ( 'NONE',  ( -8.805702923740138355E-17, 1.000000000000000000, 0.000000000000000000 ) ) ;
#42142 = CARTESIAN_POINT ( 'NONE',  ( 1.555118110236221041, -0.4536011799217367080, 0.2665933059059888421 ) ) ;
#42143 = CARTESIAN_POINT ( 'NONE',  ( -0.7217847769028863381, 0.05413385826771626580, -0.4176697321401330321 ) ) ;
#42144 = CARTESIAN_POINT ( 'NONE',  ( 0.2891555358219910499, 0.2891555358219910499, -0.5295275590551180578 ) ) ;
#42145 = CARTESIAN_POINT ( 'NONE',  ( 1.299212598425197429, -0.6692913385826771977, 8.415575281601705876E-17 ) ) ;
#42146 = CARTESIAN_POINT ( 'NONE',  ( 0.2230971128608929543, 0.05413385826771626580, -0.4176697321401330321 ) ) ;
#42147 = CARTESIAN_POINT ( 'NONE',  ( 0.3543307086614181922, -0.5511811023622047445, 6.969142054262312111E-17 ) ) ;
#42148 = CYLINDRICAL_SURFACE ( 'NONE', #2323, 0.1771653543307088186 ) ;
#42149 = CARTESIAN_POINT ( 'NONE',  ( -0.1377952755905504645, -0.4536011799217368745, -0.2665933059059886201 ) ) ;
#42150 = CARTESIAN_POINT ( 'NONE',  ( 0.9055118110236227702, -0.5511811023622047445, 6.969142054262312111E-17 ) ) ;
#42151 = FACE_OUTER_BOUND ( 'NONE', #38601, .T. ) ;
#42152 = CARTESIAN_POINT ( 'NONE',  ( 0.3460692066303959202, -0.1998031496062991630, -1.284120734908136496 ) ) ;
#42153 = CARTESIAN_POINT ( 'NONE',  ( 0.7480314960629927956, 0.2952755905511811885, 0.000000000000000000 ) ) ;
#42154 = CARTESIAN_POINT ( 'NONE',  ( 0.3392501089628018329, 0.1958661417322835607, -1.068241469816272771 ) ) ;
#42155 = CARTESIAN_POINT ( 'NONE',  ( 1.469816272965879911, -0.5023911411419708095, 0.1820866141732285504 ) ) ;
#42156 = CARTESIAN_POINT ( 'NONE',  ( -0.3698506310978935119, 0.1308238996069450155, -1.587495037872345741E-17 ) ) ;
#42157 = CARTESIAN_POINT ( 'NONE',  ( -0.1246719160104980823, 0.1771653543307087630, 0.09757992244046791164 ) ) ;
#42158 = B_SPLINE_CURVE_WITH_KNOTS ( 'NONE', 3,
 ( #63449, #81178, #49987, #42843 ),
 .UNSPECIFIED., .F., .F.,
 ( 4, 4 ),
 ( 0.1666213495636641451, 0.1680035684901380333 ),
 .UNSPECIFIED. ) ;
#42159 = CARTESIAN_POINT ( 'NONE',  ( 0.2952755905511819101, 0.1660481256975883668, -0.3530559997133364547 ) ) ;
#42160 = CARTESIAN_POINT ( 'NONE',  ( 1.443569553805774897, -0.5023911411419708095, -0.1820866141732282451 ) ) ;
#42161 = CARTESIAN_POINT ( 'NONE',  ( -1.476377952755905110, -0.4536011799217368745, -0.2665933059059886201 ) ) ;
#42162 = CARTESIAN_POINT ( 'NONE',  ( -1.384514435695537005, 0.2952755905511811885, 0.1292274648535926551 ) ) ;
#42163 = AXIS2_PLACEMENT_3D ( 'NONE', #70628, #26434, #1607 ) ;
#42164 = CARTESIAN_POINT ( 'NONE',  ( 0.2034120734908144990, -0.6692913385826771977, 0.1292274648535927661 ) ) ;
#42165 = CARTESIAN_POINT ( 'NONE',  ( 1.043307086614173818, 0.1660481256975885056, 0.3530559997133364547 ) ) ;
#42166 = CARTESIAN_POINT ( 'NONE',  ( 0.4724409448818898682, 2.892866454678787531E-17, -0.1948818897637795422 ) ) ;
#42167 = CARTESIAN_POINT ( 'NONE',  ( -0.05249343832020938322, -0.6046776061558809534, -0.2411417322834644161 ) ) ;
#42168 = CARTESIAN_POINT ( 'NONE',  ( 1.115485564304462551, -0.4281496062992127816, -0.4176697321401328100 ) ) ;
#42169 = CARTESIAN_POINT ( 'NONE',  ( 0.8267716535433078384, -0.6692913385826771977, 8.415575281601705876E-17 ) ) ;
#42170 = CARTESIAN_POINT ( 'NONE',  ( 0.4744094488188900782, 1.537401574803149984, 2.170146923806596906 ) ) ;
#42171 = CARTESIAN_POINT ( 'NONE',  ( 0.6167979002624679463, -0.004921259842519870586, -0.3153832671262229437 ) ) ;
#42172 = CARTESIAN_POINT ( 'NONE',  ( 1.620734908136483465, -0.6692913385826771977, 0.1292274648535927661 ) ) ;
#42173 = CARTESIAN_POINT ( 'NONE',  ( -0.03937007874015669567, -0.5511811023622047445, 6.969142054262312111E-17 ) ) ;
#42174 = CIRCLE ( 'NONE', #24679, 0.09842519685039351207 ) ;
#42175 = CARTESIAN_POINT ( 'NONE',  ( -0.05905511811023545637, 0.1660481256975885056, 0.3530559997133364547 ) ) ;
#42176 = CARTESIAN_POINT ( 'NONE',  ( 0.8333333333333340365, 0.2952755905511810774, -0.1292274648535930714 ) ) ;
#42177 = CARTESIAN_POINT ( 'NONE',  ( -0.1771653543307080136, 0.1660481256975883668, -0.3530559997133364547 ) ) ;
#42178 = CARTESIAN_POINT ( 'NONE',  ( -0.2034120734908131112, -0.5511811023622048555, -0.09757992244046775898 ) ) ;
#42179 = CARTESIAN_POINT ( 'NONE',  ( 1.003937007874016185, 0.1660481256975883668, -0.3530559997133364547 ) ) ;
#42180 = CARTESIAN_POINT ( 'NONE',  ( 0.7545931758530189937, 0.1771653543307087075, -0.09757992244046823083 ) ) ;
#42181 = CARTESIAN_POINT ( 'NONE',  ( 0.4606732211678742361, 1.778019097314512686, 0.5309055118110234117 ) ) ;
#42183 = CARTESIAN_POINT ( 'NONE',  ( -0.2925321140481930704, -0.2925321140481933480, -1.161417322834645605 ) ) ;
#42182 = CARTESIAN_POINT ( 'NONE',  ( -0.2952755905511810774, 0.000000000000000000, 0.1574803149606299191 ) ) ;
#42184 = DIRECTION ( 'NONE',  ( 1.000000000000000000, 0.000000000000000000, 0.000000000000000000 ) ) ;
#42185 = CARTESIAN_POINT ( 'NONE',  ( -1.148293963254592542, 0.2952755905511811885, 0.1292274648535926551 ) ) ;
#42186 = CARTESIAN_POINT ( 'NONE',  ( -0.4461942257217840213, 0.2306618581243848609, 0.2411417322834645549 ) ) ;
#42187 = CARTESIAN_POINT ( 'NONE',  ( 0.4724409448818898682, 2.892866454678787531E-17, -0.1181102362204724532 ) ) ;
#42188 = CARTESIAN_POINT ( 'NONE',  ( -0.1058382717557503211, 0.3949938075777409408, -2.526246719160105236 ) ) ;
#42189 = ORIENTED_EDGE ( 'NONE', *, *, #52769, .F. ) ;
#42190 = CARTESIAN_POINT ( 'NONE',  ( 0.8661417322834653598, -0.1870078740157479769, 0.3641732283464567677 ) ) ;
#42191 = CARTESIAN_POINT ( 'NONE',  ( -0.1049643490035307020, 0.3917322834645669549, -0.7860892388451442558 ) ) ;
#42192 = CARTESIAN_POINT ( 'NONE',  ( 1.187664041994751285, -0.3162353388693409650, -0.4822834645669289433 ) ) ;
#42193 = CARTESIAN_POINT ( 'NONE',  ( 0.3458507752293908943, -0.3458507752293908943, -2.303149606299212060 ) ) ;
#42194 = CARTESIAN_POINT ( 'NONE',  ( -0.03443470937339725840, 0.2755905511811023723, -1.320480459168889897 ) ) ;
#42195 = CARTESIAN_POINT ( 'NONE',  ( -1.371391076115484831, 0.1771653543307087075, -0.09757992244046823083 ) ) ;
#42196 = CARTESIAN_POINT ( 'NONE',  ( -2.795275590551184131, 1.023622047244095556, -2.654250759839014936E-16 ) ) ;
#42197 = CARTESIAN_POINT ( 'NONE',  ( 1.338582677165355062, -0.1870078740157480601, -0.3641732283464567677 ) ) ;
#42198 = CARTESIAN_POINT ( 'NONE',  ( 0.2427821522309719648, -0.05778040916215522460, 0.4822834645669289988 ) ) ;
#42199 = CARTESIAN_POINT ( 'NONE',  ( -0.1958661417322834497, -0.3392501089628018884, -0.1456499755567436105 ) ) ;
#42200 = CARTESIAN_POINT ( 'NONE',  ( 0.1640419947506569498, -0.3162353388693409650, -0.4822834645669289433 ) ) ;
#42201 = CARTESIAN_POINT ( 'NONE',  ( -0.8989501312335946848, 0.1771653543307087075, -0.09757992244046823083 ) ) ;
#42203 = EDGE_CURVE ( 'NONE', #80344, #23166, #17126, .T. ) ;
#42202 = CARTESIAN_POINT ( 'NONE',  ( 0.6167979002624678353, -0.4281496062992124485, 0.4176697321401328655 ) ) ;
#42204 = CARTESIAN_POINT ( 'NONE',  ( -0.2493438320209966919, 0.05413385826771626580, -0.4176697321401330321 ) ) ;
#42205 = CARTESIAN_POINT ( 'NONE',  ( 0.5411721830064198935, 8.471767977567108961E-16, -0.4445507791589058955 ) ) ;
#42206 = CARTESIAN_POINT ( 'NONE',  ( 0.000000000000000000, 2.677165354330708791, 0.000000000000000000 ) ) ;
#42207 = CARTESIAN_POINT ( 'NONE',  ( 0.1049643490035303967, 0.3917322834645670659, -1.564979945703099062 ) ) ;
#42208 = CARTESIAN_POINT ( 'NONE',  ( 0.8858267716535438430, 0.1660481256975885056, 0.3530559997133364547 ) ) ;
#42209 = CARTESIAN_POINT ( 'NONE',  ( -0.1574803149606292529, -0.1870078740157479769, 0.4822834645669291653 ) ) ;
#42210 = CARTESIAN_POINT ( 'NONE',  ( -1.108923884514435132, -0.05778040916215560624, -0.4822834645669293319 ) ) ;
#42211 = CARTESIAN_POINT ( 'NONE',  ( 1.272965879265092637, 0.05413385826771666132, 0.4176697321401328100 ) ) ;
#42212 = CARTESIAN_POINT ( 'NONE',  ( 0.3346456692913393205, -0.5400638737290845981, -0.3530559997133363437 ) ) ;
#42213 = CARTESIAN_POINT ( 'NONE',  ( 0.3917322834645669549, 0.1049643490035304660, -0.8392388451443569819 ) ) ;
#42214 = CARTESIAN_POINT ( 'NONE',  ( -0.5380577427821514602, -0.4281496062992127816, -0.4176697321401328100 ) ) ;
#42215 = CARTESIAN_POINT ( 'NONE',  ( 0.2755905511811031494, 0.2952755905511811885, 0.000000000000000000 ) ) ;
#42216 = CARTESIAN_POINT ( 'NONE',  ( -0.3608923884514428360, 0.2952755905511811885, 0.1292274648535926551 ) ) ;
#42217 = AXIS2_PLACEMENT_3D ( 'NONE', #73512, #35609, #65944 ) ;
#42218 = CARTESIAN_POINT ( 'NONE',  ( 0.8464566929133866546, -0.4536011799217367080, 0.2665933059059888421 ) ) ;
#42219 = CARTESIAN_POINT ( 'NONE',  ( -1.712598425196849572, 0.1660481256975885056, 0.3530559997133364547 ) ) ;
#42220 = CARTESIAN_POINT ( 'NONE',  ( 0.4855643044619428750, 0.05413385826771666132, 0.4176697321401328100 ) ) ;
#42221 = SURFACE_STYLE_FILL_AREA ( #36326 ) ;
#42222 = CARTESIAN_POINT ( 'NONE',  ( -0.1049643490035307020, 0.3917322834645669549, -2.360892388451444113 ) ) ;
#42223 = ORIENTED_EDGE ( 'NONE', *, *, #56444, .F. ) ;
#42224 = ORIENTED_EDGE ( 'NONE', *, *, #36884, .F. ) ;
#42225 = CARTESIAN_POINT ( 'NONE',  ( 0.8727034120734913358, -0.05778040916215522460, 0.4822834645669289988 ) ) ;
#42226 = CARTESIAN_POINT ( 'NONE',  ( 0.6036745406824153282, -0.5023911411419708095, 0.1820866141732285504 ) ) ;
#42228 = DIRECTION ( 'NONE',  ( 0.000000000000000000, 0.000000000000000000, -1.000000000000000000 ) ) ;
#42227 = CARTESIAN_POINT ( 'NONE',  ( 0.9552210167251751205, -9.595573933774993207E-16, 0.4281989832122458095 ) ) ;
#42229 = CARTESIAN_POINT ( 'NONE',  ( 0.3392501089628018329, 0.1958661417322835607, -0.6883202099737534274 ) ) ;
#42230 = DIRECTION ( 'NONE',  ( 0.000000000000000000, -1.000000000000000000, 0.000000000000000000 ) ) ;
#42231 =( LENGTH_UNIT ( ) NAMED_UNIT ( * ) SI_UNIT ( $, .METRE. ) );
#42232 = CARTESIAN_POINT ( 'NONE',  ( -0.3460692066303960313, 0.1998031496062989965, -2.622703412073490892 ) ) ;
#42233 = CARTESIAN_POINT ( 'NONE',  ( 0.8070866141732288002, 0.1660481256975885056, 0.3530559997133364547 ) ) ;
#42234 = CARTESIAN_POINT ( 'NONE',  ( -0.8267716535433065062, 0.2952755905511811885, 0.000000000000000000 ) ) ;
#42235 = CARTESIAN_POINT ( 'NONE',  ( -0.6299212598425188991, -0.1870078740157479769, 0.4822834645669291653 ) ) ;
#42236 = CARTESIAN_POINT ( 'NONE',  ( 0.6692913385826777528, 0.2952755905511811885, 0.000000000000000000 ) ) ;
#42237 = CARTESIAN_POINT ( 'NONE',  ( 1.410761154855643795, -0.3162353388693405765, 0.4822834645669290543 ) ) ;
#42238 = CARTESIAN_POINT ( 'NONE',  ( -1.030578161883458410, 1.368986870467494565, 0.4437799316085911383 ) ) ;
#42239 = CARTESIAN_POINT ( 'NONE',  ( 1.404199475065617708, -0.004921259842519870586, -0.3153832671262229437 ) ) ;
#42240 = LINE ( 'NONE', #47724, #37157 ) ;
#42241 = CARTESIAN_POINT ( 'NONE',  ( -1.318897637795274802, 0.07958543189024085140, 0.2665933059059887866 ) ) ;
#42242 = CARTESIAN_POINT ( 'NONE',  ( -0.1958661417322836718, 0.3392501089628017219, -0.005249343832020952200 ) ) ;
#42243 = CARTESIAN_POINT ( 'NONE',  ( -0.02624671916010428221, 0.2306618581243847221, -0.2411417322834647770 ) ) ;
#42245 = DIRECTION ( 'NONE',  ( 0.000000000000000000, 1.000000000000000000, 0.000000000000000000 ) ) ;
#42244 = CARTESIAN_POINT ( 'NONE',  ( 1.220472440944882608, 0.2952755905511811885, 0.000000000000000000 ) ) ;
#42246 = CARTESIAN_POINT ( 'NONE',  ( -1.351706036745406347, -0.004921259842519870586, -0.3153832671262229437 ) ) ;
#42247 = CARTESIAN_POINT ( 'NONE',  ( 0.4790026246719168435, -0.3162353388693409650, -0.4822834645669289433 ) ) ;
#42248 = CARTESIAN_POINT ( 'NONE',  ( 1.305774278215223960, 0.1771653543307087075, -0.09757992244046823083 ) ) ;
#42249 = CARTESIAN_POINT ( 'NONE',  ( -0.3917322834645669549, -7.196005306013483243E-17, -1.536726091042307951 ) ) ;
#42250 = CARTESIAN_POINT ( 'NONE',  ( -1.233595800524933894, 0.1283753931104748280, 0.1820866141732283561 ) ) ;
#42251 = CARTESIAN_POINT ( 'NONE',  ( 1.200787401574803681, 0.1660481256975885056, 0.3530559997133364547 ) ) ;
#42252 = CARTESIAN_POINT ( 'NONE',  ( 2.565525098582239316, 1.606100245667704929, -0.4697171261335975623 ) ) ;
#42253 = CARTESIAN_POINT ( 'NONE',  ( -0.3740157480314953431, -0.5400638737290845981, -0.3530559997133363437 ) ) ;
#42254 = CARTESIAN_POINT ( 'NONE',  ( -1.528871391076114250, -0.5511811023622046335, 0.09757992244046803654 ) ) ;
#42255 = CARTESIAN_POINT ( 'NONE',  ( -0.8070866141732276899, -0.5400638737290844871, 0.3530559997133364547 ) ) ;
#42256 = CARTESIAN_POINT ( 'NONE',  ( -1.364829396325458521, -0.5023911411419708095, 0.1820866141732285504 ) ) ;
#42257 = CARTESIAN_POINT ( 'NONE',  ( 0.1958661417322834775, 0.3392501089628018884, -0.4560560611886632087 ) ) ;
#42258 = CARTESIAN_POINT ( 'NONE',  ( 0.3280839895013130669, 0.05413385826771666132, 0.4176697321401328100 ) ) ;
#42259 = DIRECTION ( 'NONE',  ( 0.000000000000000000, 0.000000000000000000, 1.000000000000000000 ) ) ;
#42260 = CARTESIAN_POINT ( 'NONE',  ( 1.482939632545932307, 0.05413385826771626580, -0.4176697321401330321 ) ) ;
#42261 = CARTESIAN_POINT ( 'NONE',  ( 0.2362204724409449064, 0.4091458600556404646, -2.110892388451443225 ) ) ;
#42262 = CARTESIAN_POINT ( 'NONE',  ( -1.049868766404198794, 0.2306618581243847221, -0.2411417322834647770 ) ) ;
#42263 = CARTESIAN_POINT ( 'NONE',  ( -0.5249343832020990641, -0.5023911411419708095, -0.1820866141732282451 ) ) ;
#42264 = CARTESIAN_POINT ( 'NONE',  ( -0.4986876640419939388, 0.1539470093639521697, -0.1968503937007875793 ) ) ;
#42265 = CARTESIAN_POINT ( 'NONE',  ( 0.1377952755905518800, 0.1660481256975883668, -0.3530559997133364547 ) ) ;
#42266 = CARTESIAN_POINT ( 'NONE',  ( 0.2034120734908144990, -0.5511811023622046335, 0.09757992244046803654 ) ) ;
#42267 = CARTESIAN_POINT ( 'NONE',  ( -1.128608923884513837, -0.5023911411419708095, 0.1820866141732285504 ) ) ;
#42268 = CARTESIAN_POINT ( 'NONE',  ( -1.522309711286088607, 0.2306618581243847221, -0.2411417322834647770 ) ) ;
#42269 = CARTESIAN_POINT ( 'NONE',  ( 1.200787401574803681, -0.4536011799217368745, -0.2665933059059886201 ) ) ;
#42270 = CARTESIAN_POINT ( 'NONE',  ( 1.528871391076116026, 0.2952755905511811885, 0.1292274648535926551 ) ) ;
#42271 = CARTESIAN_POINT ( 'NONE',  ( -0.2262115530851587786, -2.191421614605370878E-15, 0.4445507791589071167 ) ) ;
#42272 = CARTESIAN_POINT ( 'NONE',  ( 0.3215223097112867578, -0.2845877964562161244, -0.3641732283464567121 ) ) ;
#42273 = CARTESIAN_POINT ( 'NONE',  ( 1.017060367454068803, -0.3162353388693405765, 0.4822834645669290543 ) ) ;
#42274 = CARTESIAN_POINT ( 'NONE',  ( 0.1474713956048451791, 8.471767977567108961E-16, -0.4445507791589058955 ) ) ;
#42275 = CARTESIAN_POINT ( 'NONE',  ( 1.010498687664042716, -0.004921259842519870586, -0.3153832671262229437 ) ) ;
#42276 = VERTEX_POINT ( 'NONE', #63155 ) ;
#42277 = CARTESIAN_POINT ( 'NONE',  ( -1.161417322834644716, 0.1660481256975885056, 0.3530559997133364547 ) ) ;
#42278 = CARTESIAN_POINT ( 'NONE',  ( -0.9251968503937002541, -0.5400638737290845981, -0.3530559997133363437 ) ) ;
#42279 = CARTESIAN_POINT ( 'NONE',  ( 0.1706036745406830368, 0.05413385826771666132, 0.4176697321401328100 ) ) ;
#42280 = CARTESIAN_POINT ( 'NONE',  ( 0.5404819259526921771, 1.809133623825372073E-16, -0.4118484887281974038 ) ) ;
#42281 = CARTESIAN_POINT ( 'NONE',  ( -0.1070741851644056997, 0.3996062992125984925, -2.288057742782152459 ) ) ;
#42282 = CARTESIAN_POINT ( 'NONE',  ( 0.7939632545931766261, -0.05778040916215522460, 0.4822834645669289988 ) ) ;
#42283 = CARTESIAN_POINT ( 'NONE',  ( -1.712598425196849572, 0.1660481256975885056, 0.3530559997133364547 ) ) ;
#42284 = CARTESIAN_POINT ( 'NONE',  ( -0.01312335958005186876, 0.05413385826771626580, -0.4176697321401330321 ) ) ;
#42285 = CARTESIAN_POINT ( 'NONE',  ( 0.8136482939632553313, 0.2306618581243848609, 0.2411417322834645549 ) ) ;
#42286 = CARTESIAN_POINT ( 'NONE',  ( -0.3460692066303960868, 0.1998031496062990242, -1.758530183727034180 ) ) ;
#42287 = AXIS2_PLACEMENT_3D ( 'NONE', #50571, #5558, #19011 ) ;
#42288 = CARTESIAN_POINT ( 'NONE',  ( -0.2891555358219911054, 0.2891555358219909388, -1.279527559055118280 ) ) ;
#42289 = CARTESIAN_POINT ( 'NONE',  ( 4.893765752498283924E-17, -0.3996062992125986035, -2.283464566929133799 ) ) ;
#42290 = CARTESIAN_POINT ( 'NONE',  ( -1.157146581871515012E-16, 0.4724409448818898682, -0.6299212598425196763 ) ) ;
#42291 = CARTESIAN_POINT ( 'NONE',  ( 4.797336870675656522E-17, -0.3917322834645670104, -0.2283464566929133410 ) ) ;
#42292 = CARTESIAN_POINT ( 'NONE',  ( -0.2296587926509179312, -0.2845877964562161244, -0.3641732283464567121 ) ) ;
#42293 = CARTESIAN_POINT ( 'NONE',  ( -0.7349081364829390672, 0.2306618581243847221, -0.2411417322834647770 ) ) ;
#42294 = CARTESIAN_POINT ( 'NONE',  ( 0.7480314960629927956, -0.6692913385826771977, 8.415575281601705876E-17 ) ) ;
#42295 = CARTESIAN_POINT ( 'NONE',  ( -0.3949938075777411073, 0.1058382717557497660, -2.314304461942256808 ) ) ;
#42296 = CARTESIAN_POINT ( 'NONE',  ( 0.1312335958005257930, 0.1283753931104746893, -0.1820866141732285504 ) ) ;
#42297 = CARTESIAN_POINT ( 'NONE',  ( -1.338582677165353729, -0.1870078740157479769, 0.4822834645669291653 ) ) ;
#42298 = CARTESIAN_POINT ( 'NONE',  ( 1.187664041994751285, -0.3162353388693409650, -0.4822834645669289433 ) ) ;
#42299 = CARTESIAN_POINT ( 'NONE',  ( -0.4724409448818895907, -0.1265901696524993070, -2.250656167979002920 ) ) ;
#42300 = CARTESIAN_POINT ( 'NONE',  ( -0.3996062992125986035, -0.1070741851644056997, -1.778215223097112663 ) ) ;
#42301 = CARTESIAN_POINT ( 'NONE',  ( -0.7426113562972000981, 2.793565526369265584, 0.5309055118110235227 ) ) ;
#42302 = ORIENTED_EDGE ( 'NONE', *, *, #45132, .F. ) ;
#42303 = CARTESIAN_POINT ( 'NONE',  ( 1.167979002624672580, 0.05413385826771626580, -0.4176697321401330321 ) ) ;
#42304 = CARTESIAN_POINT ( 'NONE',  ( 1.207349081364829990, -0.5023911411419708095, -0.1820866141732282451 ) ) ;
#42306 = CARTESIAN_POINT ( 'NONE',  ( -1.653543307086613234, -0.1870078740157479769, 0.4822834645669291653 ) ) ;
#42305 = CARTESIAN_POINT ( 'NONE',  ( -1.515748031496062076, -0.4536011799217367080, 0.2665933059059888421 ) ) ;
#42307 = CARTESIAN_POINT ( 'NONE',  ( 0.3917322834645669549, 0.1049643490035304660, 0.1056430446194224632 ) ) ;
#42308 = CARTESIAN_POINT ( 'NONE',  ( 1.192200019340703188, 4.598214627222820490E-16, 0.3954985857520057491 ) ) ;
#42309 = CARTESIAN_POINT ( 'NONE',  ( 1.377952755905512472, 0.2952755905511811885, 0.000000000000000000 ) ) ;
#42310 = CARTESIAN_POINT ( 'NONE',  ( -1.706036745406823485, 0.2306618581243848609, 0.2411417322834645549 ) ) ;
#42311 = CARTESIAN_POINT ( 'NONE',  ( -0.4199475065616791736, 0.2306618581243847221, -0.2411417322834647770 ) ) ;
#42312 = CARTESIAN_POINT ( 'NONE',  ( -0.7217847769028863381, 0.05413385826771626580, -0.4176697321401330321 ) ) ;
#42313 = CARTESIAN_POINT ( 'NONE',  ( 1.574803149606299746, -0.1870078740157479769, 0.4822834645669291653 ) ) ;
#42314 = CARTESIAN_POINT ( 'NONE',  ( -0.1049643490035302024, -0.3917322834645671215, 0.0006561679790025351077 ) ) ;
#42315 = CARTESIAN_POINT ( 'NONE',  ( 0.07874015748031558404, -0.1870078740157480879, -0.4822834645669291653 ) ) ;
#42316 = CARTESIAN_POINT ( 'NONE',  ( 0.1958661417322834775, 0.3392501089628018884, -2.341207349081364963 ) ) ;
#42317 = CARTESIAN_POINT ( 'NONE',  ( -1.620734908136482577, 0.1771653543307087630, 0.09757992244046791164 ) ) ;
#42318 = VERTEX_POINT ( 'NONE', #29924 ) ;
#42319 = CARTESIAN_POINT ( 'NONE',  ( 0.2891555358219910499, -0.2891555358219909944, -2.775590551181102317 ) ) ;
#42320 = EDGE_LOOP ( 'NONE', ( #28967, #3805, #11360, #34741 ) ) ;
#42321 = CARTESIAN_POINT ( 'NONE',  ( 0.4177787735907000366, 0.3937007874015748254, -1.874132239285499324 ) ) ;
#42322 = CARTESIAN_POINT ( 'NONE',  ( -1.706036745406823485, 0.2306618581243848609, 0.2411417322834645549 ) ) ;
#42323 = CARTESIAN_POINT ( 'NONE',  ( 0.2925321140481932369, -0.2925321140481932369, -0.8858267716535430658 ) ) ;
#42324 = CARTESIAN_POINT ( 'NONE',  ( 1.653543307086614789, -0.1870078740157479769, 0.3641732283464567677 ) ) ;
#42325 = LINE ( 'NONE', #4860, #15512 ) ;
#42326 = PLANE ( 'NONE',  #28839 ) ;
#42327 = CARTESIAN_POINT ( 'NONE',  ( -0.6199123404867337150, -2.191421614605370878E-15, 0.4445507791589071167 ) ) ;
#42328 = CARTESIAN_POINT ( 'NONE',  ( -0.2867679344610365999, 0.2867679344610364889, -0.1043307086614174151 ) ) ;
#42329 = CARTESIAN_POINT ( 'NONE',  ( -0.5183727034120726440, 0.1771653543307087630, 0.09757992244046791164 ) ) ;
#42330 = CARTESIAN_POINT ( 'NONE',  ( -1.043307086614172707, 0.07958543189024071263, -0.2665933059059888421 ) ) ;
#42331 = CARTESIAN_POINT ( 'NONE',  ( -0.3917322834645671215, 0.1049643490035301469, -2.794619422572177658 ) ) ;
#42332 = CARTESIAN_POINT ( 'NONE',  ( -1.469816272965878357, 0.2306618581243848609, 0.2411417322834645549 ) ) ;
#42333 = CARTESIAN_POINT ( 'NONE',  ( 0.6430446194225728496, 0.05413385826771666132, 0.4176697321401328100 ) ) ;
#42334 = CARTESIAN_POINT ( 'NONE',  ( -1.305774278215222184, 0.2952755905511811885, 0.1292274648535926551 ) ) ;
#42335 = CARTESIAN_POINT ( 'NONE',  ( 0.1049643490035304938, -0.3917322834645669549, -0.2349081364829396223 ) ) ;
#42336 = ORIENTED_EDGE ( 'NONE', *, *, #71870, .T. ) ;
#42337 = EDGE_CURVE ( 'NONE', #312, #41865, #46353, .T. ) ;
#42338 = CARTESIAN_POINT ( 'NONE',  ( -1.443569553805773564, 0.2306618581243847221, -0.2411417322834647770 ) ) ;
#42339 = CARTESIAN_POINT ( 'NONE',  ( -1.813482582612293559, 2.755905511811024056, 0.5314960629921260393 ) ) ;
#42340 = CARTESIAN_POINT ( 'NONE',  ( 0.1265901696524990294, -0.4724409448818896462, -1.502624671916010346 ) ) ;
#42341 = CARTESIAN_POINT ( 'NONE',  ( 0.1588297147722000091, 0.2491186766705762723, 0.1541304905092664712 ) ) ;
#42342 = ADVANCED_FACE ( 'NONE', ( #17733 ), #56003, .F. ) ;
#42343 = CARTESIAN_POINT ( 'NONE',  ( 0.3458507752293908943, 0.3458507752293908943, -0.9251968503937008093 ) ) ;
#42344 = CARTESIAN_POINT ( 'NONE',  ( -0.5708661417322825615, -0.5400638737290844871, 0.3530559997133364547 ) ) ;
#42345 = CARTESIAN_POINT ( 'NONE',  ( 1.614173228346457378, -0.6692913385826771977, 8.415575281601705876E-17 ) ) ;
#42347 = PLANE ( 'NONE',  #37153 ) ;
#42346 = CARTESIAN_POINT ( 'NONE',  ( 2.372150492836605294E-17, -1.268531780058464091E-17, 0.1937007874015748143 ) ) ;
#42348 = CARTESIAN_POINT ( 'NONE',  ( 1.601049868766404982, -0.6046776061558809534, -0.2411417322834644161 ) ) ;
#42349 = CARTESIAN_POINT ( 'NONE',  ( -0.8464566929133852113, -0.5400638737290845981, -0.3530559997133363437 ) ) ;
#42350 = CARTESIAN_POINT ( 'NONE',  ( -0.3392501089628018329, -0.1958661417322836440, 0.02495369898393883651 ) ) ;
#42351 = CARTESIAN_POINT ( 'NONE',  ( -0.006561679790025524116, -0.2845877964562159024, 0.3641732283464567677 ) ) ;
#42352 = CARTESIAN_POINT ( 'NONE',  ( -0.1958661417322836718, 0.3392501089628017219, -0.4127296587926510552 ) ) ;
#42353 = CARTESIAN_POINT ( 'NONE',  ( -0.1181102362204717315, -0.5511811023622047445, 6.969142054262312111E-17 ) ) ;
#42354 = CARTESIAN_POINT ( 'NONE',  ( 0.7808398950131240079, -0.2845877964562159024, 0.3641732283464567677 ) ) ;
#42355 = CARTESIAN_POINT ( 'NONE',  ( 0.5839895013123367340, -0.6692913385826773087, -0.1292274648535924053 ) ) ;
#42356 = CARTESIAN_POINT ( 'NONE',  ( -0.1902887139107604098, 0.1771653543307087075, -0.09757992244046823083 ) ) ;
#42357 = CARTESIAN_POINT ( 'NONE',  ( 0.1958661417322834775, 0.3392501089628018884, -2.498687664041994605 ) ) ;
#42358 = CARTESIAN_POINT ( 'NONE',  ( -1.653543307086613234, -0.1870078740157479769, 0.4822834645669291653 ) ) ;
#42359 = EDGE_CURVE ( 'NONE', #46767, #36200, #36137, .T. ) ;
#42360 = CARTESIAN_POINT ( 'NONE',  ( -1.043307086614172041, -0.5400638737290844871, 0.3530559997133364547 ) ) ;
#42361 = CARTESIAN_POINT ( 'NONE',  ( 0.4724409448818896462, 0.1265901696524990294, -0.8313648293963252778 ) ) ;
#42362 = CARTESIAN_POINT ( 'NONE',  ( -0.05905511811023545637, -0.5400638737290845981, -0.3530559997133363437 ) ) ;
#42363 = EDGE_CURVE ( 'NONE', #20676, #69946, #31196, .T. ) ;
#42364 = CARTESIAN_POINT ( 'NONE',  ( -0.3937007874015740483, -0.1870078740157479769, 0.4822834645669291653 ) ) ;
#42365 = CARTESIAN_POINT ( 'NONE',  ( 0.5314960629921156032, 2.755905511811024056, 0.9881811337016697117 ) ) ;
#42366 = CARTESIAN_POINT ( 'NONE',  ( 0.1377952755905518800, -0.4536011799217367080, 0.2665933059059888421 ) ) ;
#42367 = CARTESIAN_POINT ( 'NONE',  ( -0.3346456692913377662, -0.5400638737290844871, 0.3530559997133364547 ) ) ;
#42368 = CARTESIAN_POINT ( 'NONE',  ( -0.5446194225721777693, -0.05778040916215522460, 0.4822834645669289988 ) ) ;
#42369 = DIRECTION ( 'NONE',  ( -0.7071067811865461294, -0.000000000000000000, -0.7071067811865490160 ) ) ;
#42370 = CARTESIAN_POINT ( 'NONE',  ( 1.620734908136483465, -0.5511811023622046335, 0.09757992244046803654 ) ) ;
#42371 = CARTESIAN_POINT ( 'NONE',  ( 0.3215223097112867578, -0.3162353388693409650, -0.4822834645669289433 ) ) ;
#42372 = VERTEX_POINT ( 'NONE', #26927 ) ;
#42373 = CARTESIAN_POINT ( 'NONE',  ( -9.787531504996566615E-17, 0.3996062992125985480, -1.966535433070865979 ) ) ;
#42374 = DIRECTION ( 'NONE',  ( 0.000000000000000000, 0.000000000000000000, -1.000000000000000000 ) ) ;
#42375 = CARTESIAN_POINT ( 'NONE',  ( -0.7808398950131225646, -0.08942795157527998196, 0.3641732283464567121 ) ) ;
#42376 = CARTESIAN_POINT ( 'NONE',  ( -0.4921259842519677963, -0.5400638737290844871, 0.3530559997133364547 ) ) ;
#42377 = CARTESIAN_POINT ( 'NONE',  ( 1.587926509186352586, -0.4281496062992127816, -0.4176697321401328100 ) ) ;
#42378 = CARTESIAN_POINT ( 'NONE',  ( 1.535433070866142558, 0.2952755905511811885, 0.000000000000000000 ) ) ;
#42379 = LINE ( 'NONE', #49107, #68059 ) ;
#42380 = CARTESIAN_POINT ( 'NONE',  ( -1.305774278215222184, -0.5511811023622048555, -0.09757992244046775898 ) ) ;
#42381 = CARTESIAN_POINT ( 'NONE',  ( -0.2925321140481932369, 0.2925321140481930704, -0.4114173228346456046 ) ) ;
#42382 = CARTESIAN_POINT ( 'NONE',  ( -0.1998031496062991907, -0.3460692066303959757, -0.5380577427821522374 ) ) ;
#42383 = CARTESIAN_POINT ( 'NONE',  ( 0.1049643490035303967, 0.3917322834645670659, -2.824822465388138415 ) ) ;
#42384 = PLANE ( 'NONE',  #39114 ) ;
#42385 = CARTESIAN_POINT ( 'NONE',  ( 1.082677165354331228, -0.4536011799217367080, 0.2665933059059888421 ) ) ;
#42386 = CARTESIAN_POINT ( 'NONE',  ( 1.030183727034121421, -0.3162353388693409650, -0.4822834645669289433 ) ) ;
#42387 = DIRECTION ( 'NONE',  ( -1.000000000000000000, -0.000000000000000000, -0.000000000000000000 ) ) ;
#42388 = CARTESIAN_POINT ( 'NONE',  ( 0.7217847769028878924, -0.4281496062992127816, -0.4176697321401328100 ) ) ;
#42389 = CARTESIAN_POINT ( 'NONE',  ( 4.837279021331061486E-17, -0.3949938075777409963, -0.7854330708661416693 ) ) ;
#42390 = CARTESIAN_POINT ( 'NONE',  ( 1.351706036745407680, -0.004921259842519576551, 0.3153832671262227771 ) ) ;
#42391 = CARTESIAN_POINT ( 'NONE',  ( 0.1443569553805781891, 0.05413385826771626580, -0.4176697321401330321 ) ) ;
#42392 = CARTESIAN_POINT ( 'NONE',  ( -0.8727034120734901146, -0.3162353388693405765, 0.4822834645669290543 ) ) ;
#42393 = CARTESIAN_POINT ( 'NONE',  ( 1.469816272965879911, -0.6046776061558807314, 0.2411417322834647770 ) ) ;
#42394 = CARTESIAN_POINT ( 'NONE',  ( 0.4724409448818898682, 2.892866454678787531E-17, -1.062992125984252079 ) ) ;
#42395 = CARTESIAN_POINT ( 'NONE',  ( -0.1998031496062991907, -0.3460692066303959757, -2.427821522309711266 ) ) ;
#42396 = CIRCLE ( 'NONE', #66637, 1.220472440944881942 ) ;
#42397 = CARTESIAN_POINT ( 'NONE',  ( 0.5446194225721792126, -0.08942795157528024563, -0.3641732283464568787 ) ) ;
#42398 = ORIENTED_EDGE ( 'NONE', *, *, #55727, .F. ) ;
#42399 = CARTESIAN_POINT ( 'NONE',  ( 0.2867679344610366554, 0.2867679344610366554, -0.9219353262805269900 ) ) ;
#42400 = ORIENTED_EDGE ( 'NONE', *, *, #20715, .T. ) ;
#42401 = CARTESIAN_POINT ( 'NONE',  ( -0.9055118110236215490, 0.2952755905511811885, 0.000000000000000000 ) ) ;
#42402 = CARTESIAN_POINT ( 'NONE',  ( 0.006561679790026889343, -0.3162353388693409650, -0.4822834645669289433 ) ) ;
#42403 = CARTESIAN_POINT ( 'NONE',  ( -0.4855643044619415427, 0.05413385826771626580, -0.4176697321401330321 ) ) ;
#42404 = CARTESIAN_POINT ( 'NONE',  ( 0.9973753280839902091, -0.6046776061558807314, 0.2411417322834647770 ) ) ;
#42405 = CARTESIAN_POINT ( 'NONE',  ( -1.272965879265091305, 0.05413385826771626580, -0.4176697321401330321 ) ) ;
#42406 = CARTESIAN_POINT ( 'NONE',  ( -0.3149606299212590610, -0.1870078740157479769, 0.4822834645669291653 ) ) ;
#42407 = CARTESIAN_POINT ( 'NONE',  ( 1.148293963254593653, 0.2952755905511810774, -0.1292274648535930714 ) ) ;
#42408 = CARTESIAN_POINT ( 'NONE',  ( 0.4986876640419954376, 0.2306618581243848609, 0.2411417322834645549 ) ) ;
#42409 = EDGE_CURVE ( 'NONE', #19971, #26979, #16273, .T. ) ;
#42410 = CARTESIAN_POINT ( 'NONE',  ( 0.6627296587926517768, -0.6692913385826773087, -0.1292274648535924053 ) ) ;
#42411 = CARTESIAN_POINT ( 'NONE',  ( -0.2867679344610365999, 0.2867679344610364889, -1.114173228346456712 ) ) ;
#42412 = CARTESIAN_POINT ( 'NONE',  ( -0.5971128608923877978, -0.5511811023622048555, -0.09757992244046775898 ) ) ;
#42413 = ORIENTED_EDGE ( 'NONE', *, *, #37207, .F. ) ;
#42414 = CARTESIAN_POINT ( 'NONE',  ( 0.1974969037888704704, 0.3420746716998660508, -1.246719160104986734 ) ) ;
#42415 = VERTEX_POINT ( 'NONE', #77873 ) ;
#42416 = CARTESIAN_POINT ( 'NONE',  ( -0.7020997375328076329, -0.2845877964562161244, -0.3641732283464567121 ) ) ;
#42417 = CARTESIAN_POINT ( 'NONE',  ( -0.5774278215223089816, -0.6046776061558807314, 0.2411417322834647770 ) ) ;
#42418 = CARTESIAN_POINT ( 'NONE',  ( -0.2925321140481932924, 0.2925321140481931814, 0.1377952755905511584 ) ) ;
#42419 = CARTESIAN_POINT ( 'NONE',  ( -0.8595800524934373854, -0.3162353388693409650, -0.4822834645669289433 ) ) ;
#42420 = CARTESIAN_POINT ( 'NONE',  ( -0.7742782152230965886, 0.05413385826771666132, 0.4176697321401328100 ) ) ;
#42421 = CARTESIAN_POINT ( 'NONE',  ( -1.161417322834644716, 0.1660481256975885056, 0.3530559997133364547 ) ) ;
#42422 = CARTESIAN_POINT ( 'NONE',  ( -1.463254593175852492, -0.6692913385826773087, -0.1292274648535924053 ) ) ;
#42423 = CARTESIAN_POINT ( 'NONE',  ( 1.148293963254593875, -0.5511811023622046335, 0.09757992244046803654 ) ) ;
#42424 = CARTESIAN_POINT ( 'NONE',  ( 5.785732909357575061E-17, -0.4724409448818898682, -1.023622047244094446 ) ) ;
#42425 = CARTESIAN_POINT ( 'NONE',  ( 0.2362204724409451007, -0.4091458600556402980, -0.6410761154855643129 ) ) ;
#42426 = CARTESIAN_POINT ( 'NONE',  ( -0.01968503937007793844, -0.4536011799217367080, 0.2665933059059888421 ) ) ;
#42427 = CARTESIAN_POINT ( 'NONE',  ( 0.05249343832021075018, -0.6046776061558807314, 0.2411417322834647770 ) ) ;
#42428 = CARTESIAN_POINT ( 'NONE',  ( -0.2296587926509179312, -0.05778040916215522460, 0.4822834645669289988 ) ) ;
#42429 = ORIENTED_EDGE ( 'NONE', *, *, #57908, .F. ) ;
#42430 = CARTESIAN_POINT ( 'NONE',  ( -0.1070741851644051862, -0.3996062992125987146, -1.646981627296587591 ) ) ;
#42431 = CARTESIAN_POINT ( 'NONE',  ( 0.5314960629920997270, 2.755905511811024056, 2.503252890251021601 ) ) ;
#42432 = ORIENTED_EDGE ( 'NONE', *, *, #49711, .T. ) ;
#42433 = CARTESIAN_POINT ( 'NONE',  ( -0.1070741851644056997, 0.3996062992125984925, -1.185695538057742526 ) ) ;
#42434 = CARTESIAN_POINT ( 'NONE',  ( 1.581364829396326277, -0.05778040916215522460, 0.4822834645669289988 ) ) ;
#42435 = CARTESIAN_POINT ( 'NONE',  ( -0.8727034120734901146, -0.08942795157528024563, -0.3641732283464568787 ) ) ;
#42436 = CARTESIAN_POINT ( 'NONE',  ( -1.076115485564303809, 0.2306618581243848609, 0.2411417322834645549 ) ) ;
#42437 = CARTESIAN_POINT ( 'NONE',  ( -0.1265901696524993347, 0.4724409448818895907, -0.4790026246719158998 ) ) ;
#42438 = CARTESIAN_POINT ( 'NONE',  ( 0.6983222978630806432, 4.257495641787552160E-16, -0.4281993546915526805 ) ) ;
#42439 = CARTESIAN_POINT ( 'NONE',  ( 0.3917322834645669549, 0.1049643490035304660, -2.571522309711286258 ) ) ;
#42440 = CARTESIAN_POINT ( 'NONE',  ( 1.646981627296588035, -0.3162353388693405765, 0.4822834645669290543 ) ) ;
#42441 = CARTESIAN_POINT ( 'NONE',  ( 0.4133858267716541968, -0.5400638737290845981, -0.3530559997133363437 ) ) ;
#42442 = CARTESIAN_POINT ( 'NONE',  ( 0.4593175853018380828, 0.05413385826771626580, -0.4176697321401330321 ) ) ;
#42443 = CARTESIAN_POINT ( 'NONE',  ( -0.8005249343832011588, -0.004921259842519870586, -0.3153832671262229437 ) ) ;
#42444 = AXIS2_PLACEMENT_3D ( 'NONE', #49288, #74991, #68660 ) ;
#42445 = CARTESIAN_POINT ( 'NONE',  ( -0.08530183727034056085, -0.05778040916215560624, -0.4822834645669293319 ) ) ;
#42446 = CARTESIAN_POINT ( 'NONE',  ( 0.4724409448818898682, 2.892866454678787531E-17, -2.242125984251968518 ) ) ;
#42447 = CARTESIAN_POINT ( 'NONE',  ( -0.5971128608923877978, 0.2952755905511811885, 0.1292274648535926551 ) ) ;
#42448 = CARTESIAN_POINT ( 'NONE',  ( -0.3420746716998662729, 0.1974969037888702206, -1.677821522309711710 ) ) ;
#42449 = CARTESIAN_POINT ( 'NONE',  ( 1.246719160104987623, -0.3690944881889763329, 0.3153832671262228327 ) ) ;
#42450 = CARTESIAN_POINT ( 'NONE',  ( 0.2559055118110243332, -0.4536011799217368745, -0.2665933059059886201 ) ) ;
#42451 = CARTESIAN_POINT ( 'NONE',  ( 0.9973753280839902091, -0.5023911411419708095, 0.1820866141732285504 ) ) ;
#42452 = CARTESIAN_POINT ( 'NONE',  ( -1.233595800524933894, 0.2306618581243848609, 0.2411417322834645549 ) ) ;
#42453 = CARTESIAN_POINT ( 'NONE',  ( -1.351706036745406347, -0.3690944881889763329, 0.3153832671262228327 ) ) ;
#42454 = DIRECTION ( 'NONE',  ( -0.000000000000000000, -1.000000000000000000, -0.000000000000000000 ) ) ;
#42455 = CARTESIAN_POINT ( 'NONE',  ( -1.102362204724408601, -0.1870078740157479769, 0.4822834645669291653 ) ) ;
#42456 = CARTESIAN_POINT ( 'NONE',  ( -0.6102362204724400829, -0.5400638737290845981, -0.3530559997133363437 ) ) ;
#42457 = CARTESIAN_POINT ( 'NONE',  ( 0.5118110236220480003, -0.6692913385826771977, 8.415575281601705876E-17 ) ) ;
#42458 = CARTESIAN_POINT ( 'NONE',  ( 0.2867679344610365999, 0.2867679344610365999, -2.580033177656481325 ) ) ;
#42459 = CIRCLE ( 'NONE', #80109, 3.228346456692913424 ) ;
#42460 = CARTESIAN_POINT ( 'NONE',  ( -1.867828664896301616, 1.081851677178498949, 0.1334749385307871794 ) ) ;
#42461 = CARTESIAN_POINT ( 'NONE',  ( 0.2165354330708668673, -0.4536011799217367080, 0.2665933059059888421 ) ) ;
#42462 = CARTESIAN_POINT ( 'NONE',  ( -1.555118110236219930, 0.07958543189024085140, 0.2665933059059887866 ) ) ;
#42463 = CARTESIAN_POINT ( 'NONE',  ( 0.8792650918635177559, 0.05413385826771666132, 0.4176697321401328100 ) ) ;
#42464 = DIRECTION ( 'NONE',  ( -1.000000000000000000, -0.000000000000000000, -0.000000000000000000 ) ) ;
#42465 = CARTESIAN_POINT ( 'NONE',  ( 1.299212598425197429, 0.1771653543307087630, 0.000000000000000000 ) ) ;
#42466 = CARTESIAN_POINT ( 'NONE',  ( -0.9842519685039365918, -0.6692913385826771977, 8.415575281601705876E-17 ) ) ;
#42467 = CARTESIAN_POINT ( 'NONE',  ( -0.1968503937007867743, 0.1771653543307087630, 0.000000000000000000 ) ) ;
#42468 = LINE ( 'NONE', #36164, #81173 ) ;
#42469 = CARTESIAN_POINT ( 'NONE',  ( 0.5446194225721792126, -0.08942795157528024563, -0.3641732283464568787 ) ) ;
#42470 = CARTESIAN_POINT ( 'NONE',  ( -0.2034120734908128059, 0.2952755905511811885, 0.1292274648535926551 ) ) ;
#42471 = CARTESIAN_POINT ( 'NONE',  ( -0.3996062992125984925, -0.1070741851644056858, -0.7526246719160103460 ) ) ;
#42472 = CARTESIAN_POINT ( 'NONE',  ( 0.2867679344610365999, 0.2867679344610365999, -1.639763779527558807 ) ) ;
#42473 = CARTESIAN_POINT ( 'NONE',  ( 1.049868766404200127, -0.5023911411419708095, -0.1820866141732282451 ) ) ;
#42474 = CARTESIAN_POINT ( 'NONE',  ( 0.01968503937007957949, -0.5400638737290845981, -0.3530559997133363437 ) ) ;
#42475 = CARTESIAN_POINT ( 'NONE',  ( -0.3280839895013117347, 0.05413385826771626580, -0.4176697321401330321 ) ) ;
#42476 = CARTESIAN_POINT ( 'NONE',  ( -0.3608923884514428360, 0.1771653543307087630, 0.09757992244046791164 ) ) ;
#42477 = CARTESIAN_POINT ( 'NONE',  ( 0.4724409448818898682, 0.000000000000000000, -2.755905511811024056 ) ) ;
#42478 = CARTESIAN_POINT ( 'NONE',  ( -0.4986876640419939388, 0.1283753931104746893, -0.1820866141732285504 ) ) ;
#42479 = CARTESIAN_POINT ( 'NONE',  ( 0.4724409448818904789, -0.1870078740157480879, -0.4822834645669291653 ) ) ;
#42480 = EDGE_CURVE ( 'NONE', #35701, #10674, #19786, .T. ) ;
#42481 = CARTESIAN_POINT ( 'NONE',  ( -0.9645669291338575535, -0.4536011799217367080, 0.2665933059059888421 ) ) ;
#42482 = CARTESIAN_POINT ( 'NONE',  ( 0.1998031496062992463, 0.3460692066303959202, -1.480971128608923992 ) ) ;
#42483 = CARTESIAN_POINT ( 'NONE',  ( -1.548556430446193399, -0.6046776061558809534, -0.2411417322834644161 ) ) ;
#42484 = CARTESIAN_POINT ( 'NONE',  ( -0.3458507752293909498, 0.3458507752293908388, -2.224409448818897683 ) ) ;
#42485 = ORIENTED_EDGE ( 'NONE', *, *, #33290, .T. ) ;
#42486 = EDGE_CURVE ( 'NONE', #9936, #6582, #143, .T. ) ;
#42487 = CARTESIAN_POINT ( 'NONE',  ( -1.476377952755905110, -0.4536011799217368745, -0.2665933059059886201 ) ) ;
#42488 = CARTESIAN_POINT ( 'NONE',  ( -0.5052493438320203589, -0.6692913385826771977, 0.1292274648535927661 ) ) ;
#42489 = CARTESIAN_POINT ( 'NONE',  ( -1.318897637795274802, 0.1660481256975885056, 0.3530559997133364547 ) ) ;
#42490 = CARTESIAN_POINT ( 'NONE',  ( -9.594673741351313045E-17, 0.3917322834645670104, -1.659448818897637734 ) ) ;
#42491 = DIRECTION ( 'NONE',  ( 0.000000000000000000, 1.000000000000000000, 0.000000000000000000 ) ) ;
#42492 = CARTESIAN_POINT ( 'NONE',  ( 1.259842519685040019, -0.1870078740157480879, -0.4822834645669291653 ) ) ;
#42493 = CARTESIAN_POINT ( 'NONE',  ( 0.6430446194225729606, -0.4281496062992127816, -0.4176697321401328100 ) ) ;
#42494 = CARTESIAN_POINT ( 'NONE',  ( 3.908320185825791881, 1.537401574803149984, -0.4744094488188970171 ) ) ;
#42495 = CIRCLE ( 'NONE', #822, 1.122047244094488194 ) ;
#42496 = CONICAL_SURFACE ( 'NONE', #77419, 0.1771653543307085410, 1.029744258676653645 ) ;
#42498 = CARTESIAN_POINT ( 'NONE',  ( -0.3460692066303960313, 0.1998031496062989965, -2.465223097112860806 ) ) ;
#42497 = AXIS2_PLACEMENT_3D ( 'NONE', #26352, #70136, #37335 ) ;
#42499 = CARTESIAN_POINT ( 'NONE',  ( -1.673228346456691717, 0.1660481256975883668, -0.3530559997133364547 ) ) ;
#42500 = CARTESIAN_POINT ( 'NONE',  ( -0.2925321140481930704, -0.2925321140481933480, -0.8464566929133857665 ) ) ;
#42501 = VERTEX_POINT ( 'NONE', #71552 ) ;
#42502 = CARTESIAN_POINT ( 'NONE',  ( -0.9448818897637790704, -0.1870078740157480601, -0.3641732283464567677 ) ) ;
#42503 = CARTESIAN_POINT ( 'NONE',  ( 0.3917322834645670104, 2.398668435337828261E-17, -2.629921259842519898 ) ) ;
#42504 = ORIENTED_EDGE ( 'NONE', *, *, #28103, .F. ) ;
#42505 = CARTESIAN_POINT ( 'NONE',  ( 0.6561679790026253567, 0.2306618581243848609, 0.2411417322834645549 ) ) ;
#42506 = CARTESIAN_POINT ( 'NONE',  ( -0.3871391076115479057, -0.3162353388693409650, -0.4822834645669289433 ) ) ;
#42507 = CARTESIAN_POINT ( 'NONE',  ( -1.187664041994749731, -0.3162353388693405765, 0.4822834645669290543 ) ) ;
#42508 = CARTESIAN_POINT ( 'NONE',  ( 1.023622047244095334, -0.1870078740157479769, 0.4822834645669291653 ) ) ;
#42509 = CARTESIAN_POINT ( 'NONE',  ( -1.200787401574802349, -0.4536011799217367080, 0.2665933059059888421 ) ) ;
#42510 = CYLINDRICAL_SURFACE ( 'NONE', #60174, 1.122047244094488194 ) ;
#42511 = CARTESIAN_POINT ( 'NONE',  ( 0.4724409448818904789, -0.1870078740157480879, -0.4822834645669291653 ) ) ;
#42512 = CARTESIAN_POINT ( 'NONE',  ( -0.8923884514435688198, -0.6046776061558807314, 0.2411417322834647770 ) ) ;
#42513 = CARTESIAN_POINT ( 'NONE',  ( -0.1049643490035306742, 0.3917322834645668994, -1.661398007052806269 ) ) ;
#42514 = CARTESIAN_POINT ( 'NONE',  ( 1.541994750656168645, -0.6692913385826771977, 0.1292274648535927661 ) ) ;
#42515 = FACE_OUTER_BOUND ( 'NONE', #73681, .T. ) ;
#42516 =( BOUNDED_CURVE ( )  B_SPLINE_CURVE ( 1, ( #72168, #77230 ),
 .UNSPECIFIED., .F., .F. ) 
 B_SPLINE_CURVE_WITH_KNOTS ( ( 2, 2 ),
 ( 5.204170427930421283E-18, 0.002000000000000006981 ),
 .UNSPECIFIED. ) 
 CURVE ( )  GEOMETRIC_REPRESENTATION_ITEM ( )  RATIONAL_B_SPLINE_CURVE ( ( 0.9875488213027530104, 0.9875488213027530104 ) ) 
 REPRESENTATION_ITEM ( '' )  );
#42517 = CARTESIAN_POINT ( 'NONE',  ( 1.003937007874016407, -0.5400638737290844871, 0.3530559997133364547 ) ) ;
#42518 = CARTESIAN_POINT ( 'NONE',  ( -0.1958661417322834220, -0.3392501089628018884, -2.827427821522309426 ) ) ;
#42519 = CARTESIAN_POINT ( 'NONE',  ( 1.397637795275591177, 0.07958543189024071263, -0.2665933059059888421 ) ) ;
#42520 = ORIENTED_EDGE ( 'NONE', *, *, #49112, .F. ) ;
#42521 = CARTESIAN_POINT ( 'NONE',  ( -0.1049643490035302301, -0.3917322834645671770, -2.746082307907824038 ) ) ;
#42522 = CARTESIAN_POINT ( 'NONE',  ( -0.3083989501312330295, -0.3162353388693409650, -0.4822834645669289433 ) ) ;
#42523 = ORIENTED_EDGE ( 'NONE', *, *, #64962, .F. ) ;
#42525 = AXIS2_PLACEMENT_3D ( 'NONE', #76002, #69681, #18344 ) ;
#42524 = CARTESIAN_POINT ( 'NONE',  ( 0.5380577427821529035, -0.004921259842519870586, -0.3153832671262229437 ) ) ;
#42526 = CARTESIAN_POINT ( 'NONE',  ( -1.699475065616797398, 0.2952755905511811885, 0.1292274648535926551 ) ) ;
#42527 = CARTESIAN_POINT ( 'NONE',  ( 0.6561679790026253567, 0.2306618581243848609, 0.2411417322834645549 ) ) ;
#42528 = CARTESIAN_POINT ( 'NONE',  ( 0.4855643044619428750, 0.05413385826771666132, 0.4176697321401328100 ) ) ;
#42529 = CARTESIAN_POINT ( 'NONE',  ( 0.006561679790026889343, -0.05778040916215522460, 0.4822834645669289988 ) ) ;
#42530 = CARTESIAN_POINT ( 'NONE',  ( 0.3917322834645670104, 0.1049643490035304660, -1.381252911582363962 ) ) ;
#42531 = CARTESIAN_POINT ( 'NONE',  ( -0.8202099737532799750, 0.2952755905511810774, -0.1292274648535930714 ) ) ;
#42532 = CARTESIAN_POINT ( 'NONE',  ( 0.1049643490035303689, 0.3917322834645670104, -2.125328083989501682 ) ) ;
#42533 = CARTESIAN_POINT ( 'NONE',  ( -1.646981627296586703, -0.3162353388693409650, -0.4822834645669289433 ) ) ;
#42534 = CARTESIAN_POINT ( 'NONE',  ( -1.135170603674539924, 0.2952755905511810774, -0.1292274648535930714 ) ) ;
#42535 = CARTESIAN_POINT ( 'NONE',  ( 1.312335958005250269, -0.6046776061558807314, 0.2411417322834647770 ) ) ;
#42536 = CARTESIAN_POINT ( 'NONE',  ( 1.207349081364829990, 0.2306618581243848609, 0.2411417322834645549 ) ) ;
#42537 = CARTESIAN_POINT ( 'NONE',  ( -0.2925321140481932924, 0.2925321140481931814, -0.4921259842519684624 ) ) ;
#42538 = CARTESIAN_POINT ( 'NONE',  ( -0.8530183727034112984, -0.4281496062992127816, -0.4176697321401328100 ) ) ;
#42539 = CARTESIAN_POINT ( 'NONE',  ( -0.2925321140481932369, 0.2925321140481931259, 0.2185039370078740162 ) ) ;
#42540 = CARTESIAN_POINT ( 'NONE',  ( 0.4855643044619428750, 0.05413385826771666132, 0.4176697321401328100 ) ) ;
#42541 = CARTESIAN_POINT ( 'NONE',  ( 0.3996062992125986035, 2.446882876249141962E-17, -2.322834645669291209 ) ) ;
#42542 = CARTESIAN_POINT ( 'NONE',  ( -0.4790026246719152336, -0.05778040916215560624, -0.4822834645669293319 ) ) ;
#42543 = CARTESIAN_POINT ( 'NONE',  ( -1.410761154855641575, -0.2845877964562161244, -0.3641732283464567121 ) ) ;
#42544 = CARTESIAN_POINT ( 'NONE',  ( 0.7217847769028878924, -0.004921259842519576551, 0.3153832671262227771 ) ) ;
#42545 = CARTESIAN_POINT ( 'NONE',  ( 1.194225721784777594, -0.4281496062992127816, -0.4176697321401328100 ) ) ;
#42546 = CARTESIAN_POINT ( 'NONE',  ( 5.785732909357575061E-17, -0.4724409448818898682, -1.100393700787401619 ) ) ;
#42547 = CARTESIAN_POINT ( 'NONE',  ( 0.5708661417322842269, 0.07958543189024085140, 0.2665933059059887866 ) ) ;
#42548 = CARTESIAN_POINT ( 'NONE',  ( 0.6167979002624678353, -0.4281496062992124485, 0.4176697321401328655 ) ) ;
#42549 = CARTESIAN_POINT ( 'NONE',  ( -0.1058382717557503072, 0.3949938075777408852, -0.7132545931758530466 ) ) ;
#42550 = CARTESIAN_POINT ( 'NONE',  ( -0.6692913385826764205, -0.6692913385826771977, 8.415575281601705876E-17 ) ) ;
#42551 = CARTESIAN_POINT ( 'NONE',  ( 2.583694225513480713, 2.755905511811024056, 0.5314960629921260393 ) ) ;
#42552 = CARTESIAN_POINT ( 'NONE',  ( 1.220472440944882386, -0.5511811023622047445, 6.969142054262312111E-17 ) ) ;
#42553 = CARTESIAN_POINT ( 'NONE',  ( -0.6889763779527552368, -0.5400638737290845981, -0.3530559997133363437 ) ) ;
#42554 = CARTESIAN_POINT ( 'NONE',  ( 0.04593175853018440641, 0.2952755905511810774, -0.1292274648535930714 ) ) ;
#42555 = CARTESIAN_POINT ( 'NONE',  ( 0.2887139107611556010, -0.6046776061558807314, 0.2411417322834647770 ) ) ;
#42556 = CARTESIAN_POINT ( 'NONE',  ( -0.006561679790025524116, -0.08942795157528024563, -0.3641732283464568787 ) ) ;
#42557 = CARTESIAN_POINT ( 'NONE',  ( -2.647193076292303715, 1.325969025732688600, 0.4256800600601930440 ) ) ;
#42558 = CARTESIAN_POINT ( 'NONE',  ( 0.1443569553805781891, -0.004921259842519870586, -0.3153832671262229437 ) ) ;
#42559 = CARTESIAN_POINT ( 'NONE',  ( 0.8661417322834652488, -0.1870078740157480601, -0.3641732283464567677 ) ) ;
#42560 = CARTESIAN_POINT ( 'NONE',  ( -0.1109416432469456093, 1.076146463964301692, -1.548361104749216510 ) ) ;
#42561 = CARTESIAN_POINT ( 'NONE',  ( 0.1998031496062992463, 0.3460692066303959202, -1.953412073490813805 ) ) ;
#42562 = CARTESIAN_POINT ( 'NONE',  ( 0.2952755905511819101, 0.1660481256975883668, -0.3530559997133364547 ) ) ;
#42563 = CIRCLE ( 'NONE', #13011, 1.122047244094488194 ) ;
#42564 = CARTESIAN_POINT ( 'NONE',  ( 0.1049643490035303689, 0.3917322834645670104, -1.245406824146981561 ) ) ;
#42565 = AXIS2_PLACEMENT_3D ( 'NONE', #35657, #61320, #23021 ) ;
#42566 = AXIS2_PLACEMENT_3D ( 'NONE', #30510, #37641, #24187 ) ;
#42567 = CARTESIAN_POINT ( 'NONE',  ( 1.404199475065617708, -0.004921259842519870586, -0.3153832671262229437 ) ) ;
#42568 = CARTESIAN_POINT ( 'NONE',  ( 0.1049868766404206816, 0.2306618581243848609, 0.2411417322834645549 ) ) ;
#42569 = CARTESIAN_POINT ( 'NONE',  ( -0.5446194225721777693, -0.2845877964562161244, -0.3641732283464567121 ) ) ;
#42570 = CARTESIAN_POINT ( 'NONE',  ( -0.01968503937007793844, 0.1660481256975883668, -0.3530559997133364547 ) ) ;
#42571 = CARTESIAN_POINT ( 'NONE',  ( 1.377952755905512472, 0.1771653543307087630, 0.000000000000000000 ) ) ;
#42572 = CARTESIAN_POINT ( 'NONE',  ( -1.417322834645668772, -0.1870078740157479769, 0.3641732283464567677 ) ) ;
#42573 = CARTESIAN_POINT ( 'NONE',  ( -1.594488188976377563, -0.5400638737290844871, 0.3530559997133364547 ) ) ;
#42574 = CARTESIAN_POINT ( 'NONE',  ( 0.1968503937007881344, -0.6692913385826771977, 8.415575281601705876E-17 ) ) ;
#42575 = CARTESIAN_POINT ( 'NONE',  ( 1.345144356955381593, -0.05778040916215522460, 0.4822834645669289988 ) ) ;
#42576 = LINE ( 'NONE', #35867, #59890 ) ;
#42577 = CARTESIAN_POINT ( 'NONE',  ( 0.1574803149606306130, -0.1870078740157479769, 0.4822834645669291653 ) ) ;
#42578 = B_SPLINE_CURVE_WITH_KNOTS ( 'NONE', 3,
 ( #33459, #30449, #3548, #68358 ),
 .UNSPECIFIED., .F., .F.,
 ( 4, 4 ),
 ( 1.999999999897049408E-07, 0.006970199999999935128 ),
 .UNSPECIFIED. ) ;
#42579 = CARTESIAN_POINT ( 'NONE',  ( 1.496062992125985147, -0.1870078740157479769, 0.4822834645669291653 ) ) ;
#42580 = CARTESIAN_POINT ( 'NONE',  ( 1.010498687664042716, -0.4281496062992124485, 0.4176697321401328655 ) ) ;
#42581 = DIRECTION ( 'NONE',  ( 0.000000000000000000, 1.000000000000000000, 0.000000000000000000 ) ) ;
#42582 = CARTESIAN_POINT ( 'NONE',  ( 0.8136482939632553313, -0.5023911411419708095, -0.1820866141732282451 ) ) ;
#42583 = CARTESIAN_POINT ( 'NONE',  ( 1.450131233595801428, -0.6692913385826773087, -0.1292274648535924053 ) ) ;
#42584 = EDGE_CURVE ( 'NONE', #32057, #12593, #20627, .T. ) ;
#42585 = CARTESIAN_POINT ( 'NONE',  ( -0.09842519685039295696, 0.07958543189024071263, -0.2665933059059888421 ) ) ;
#42586 = CARTESIAN_POINT ( 'NONE',  ( -0.1377952755905504645, -0.5400638737290845981, -0.3530559997133363437 ) ) ;
#42587 = CARTESIAN_POINT ( 'NONE',  ( 0.8070866141732288002, 0.1660481256975885056, 0.3530559997133364547 ) ) ;
#42588 = CARTESIAN_POINT ( 'NONE',  ( -0.5380577427821514602, 0.05413385826771666132, 0.4176697321401328100 ) ) ;
#42589 = CARTESIAN_POINT ( 'NONE',  ( 0.2867679344610366554, -0.2867679344610365999, -1.984927452264778847 ) ) ;
#42590 = CARTESIAN_POINT ( 'NONE',  ( -0.2690288713910754526, 0.1771653543307087075, -0.09757992244046823083 ) ) ;
#42591 = CARTESIAN_POINT ( 'NONE',  ( 0.7480314960629927956, -0.6692913385826771977, 8.415575281601705876E-17 ) ) ;
#42592 = CARTESIAN_POINT ( 'NONE',  ( 1.102362204724410155, -0.1870078740157480601, -0.3641732283464567677 ) ) ;
#42593 = CARTESIAN_POINT ( 'NONE',  ( -1.736178228450298011, 1.299212598425196985, 0.4102808022082834460 ) ) ;
#42594 = DIRECTION ( 'NONE',  ( 0.000000000000000000, 0.000000000000000000, 1.000000000000000000 ) ) ;
#42595 = CARTESIAN_POINT ( 'NONE',  ( 2.112686649479616374, 1.697109554835843914, -0.4469779880792056348 ) ) ;
#42596 = CARTESIAN_POINT ( 'NONE',  ( -1.253280839895012377, -0.3162353388693409650, -0.4822834645669289433 ) ) ;
#42597 = CARTESIAN_POINT ( 'NONE',  ( -0.5118110236220466680, -0.6692913385826771977, 8.415575281601705876E-17 ) ) ;
#42598 = CARTESIAN_POINT ( 'NONE',  ( 0.3460692066303959757, -0.1998031496062991907, -2.939632545931758489 ) ) ;
#42599 = CARTESIAN_POINT ( 'NONE',  ( 0.1974969037888704704, 0.3420746716998660508, -2.664041994750656173 ) ) ;
#42600 = ORIENTED_EDGE ( 'NONE', *, *, #46038, .T. ) ;
#42601 = CARTESIAN_POINT ( 'NONE',  ( 0.3083989501312343062, -0.08942795157528024563, -0.3641732283464568787 ) ) ;
#42602 = CARTESIAN_POINT ( 'NONE',  ( 0.3917322834645669549, 0.1049643490035304660, -0.9041994750656167090 ) ) ;
#42603 = CARTESIAN_POINT ( 'NONE',  ( 1.220472440944882386, -0.6692913385826771977, 8.415575281601705876E-17 ) ) ;
#42604 = CARTESIAN_POINT ( 'NONE',  ( 0.4724409448818897572, -0.1265901696524988906, -2.473753280839894764 ) ) ;
#42605 = CARTESIAN_POINT ( 'NONE',  ( -1.220472440944882830, 0.2066929133858268208, 2.389277853677468338E-14 ) ) ;
#42606 = CARTESIAN_POINT ( 'NONE',  ( -1.601049868766403650, -0.5023911411419708095, 0.1820866141732285504 ) ) ;
#42607 = CARTESIAN_POINT ( 'NONE',  ( 1.627296587926509996, -0.6046776061558807314, 0.2411417322834647770 ) ) ;
#42608 = CARTESIAN_POINT ( 'NONE',  ( 1.318897637795276356, 0.07958543189024071263, -0.2665933059059888421 ) ) ;
#42609 = CARTESIAN_POINT ( 'NONE',  ( 0.5249343832021005074, -0.6046776061558807314, 0.2411417322834647770 ) ) ;
#42610 = CIRCLE ( 'NONE', #64126, 2.306288321832234978 ) ;
#42611 = CARTESIAN_POINT ( 'NONE',  ( 0.2867679344610365999, 0.2867679344610365999, -0.3753087682076623466 ) ) ;
#42612 = CARTESIAN_POINT ( 'NONE',  ( -0.1049868766404193215, -0.6046776061558807314, 0.2411417322834647770 ) ) ;
#42613 = CARTESIAN_POINT ( 'NONE',  ( -0.9514435695538050464, -0.2845877964562159024, 0.3641732283464567677 ) ) ;
#42614 = CARTESIAN_POINT ( 'NONE',  ( 0.3805774278215230400, 0.05413385826771626580, -0.4176697321401330321 ) ) ;
#42615 = CARTESIAN_POINT ( 'NONE',  ( -0.1509186351706028884, -0.05778040916215522460, 0.4822834645669289988 ) ) ;
#42616 = CARTESIAN_POINT ( 'NONE',  ( -1.614173228346457378, 2.094556775020298023, 0.1372047244094476981 ) ) ;
#42617 = VECTOR ( 'NONE', #18863, 39.37007874015748143 ) ;
#42618 = CARTESIAN_POINT ( 'NONE',  ( 0.000000000000000000, 1.929133858267716661, -2.874015748031495843 ) ) ;
#42619 = CARTESIAN_POINT ( 'NONE',  ( -0.2867679344610365444, -0.2867679344610367664, -1.788077058563991795 ) ) ;
#42620 = CARTESIAN_POINT ( 'NONE',  ( 0.6824146981627303710, -0.6046776061558807314, 0.2411417322834647770 ) ) ;
#42621 = AXIS2_PLACEMENT_3D ( 'NONE', #13564, #59005, #26173 ) ;
#42622 = AXIS2_PLACEMENT_3D ( 'NONE', #81714, #50506, #11412 ) ;
#42623 = CARTESIAN_POINT ( 'NONE',  ( -0.3477690288713905509, -0.6692913385826771977, 0.1292274648535927661 ) ) ;
#42624 = CARTESIAN_POINT ( 'NONE',  ( -1.272965879265091305, 0.05413385826771626580, -0.4176697321401330321 ) ) ;
#42625 = CARTESIAN_POINT ( 'NONE',  ( 0.9908136482939640111, 0.2952755905511810774, -0.1292274648535930714 ) ) ;
#42626 = CARTESIAN_POINT ( 'NONE',  ( 0.6758530183727039509, -0.6692913385826771977, 0.1292274648535927661 ) ) ;
#42627 = CARTESIAN_POINT ( 'NONE',  ( 0.3917322834645670104, -0.1049643490035303411, -0.9835958005249345604 ) ) ;
#42628 = CARTESIAN_POINT ( 'NONE',  ( -0.2165354330708654795, -0.5400638737290845981, -0.3530559997133363437 ) ) ;
#42629 = CARTESIAN_POINT ( 'NONE',  ( 0.1246719160104994284, 0.2952755905511810774, -0.1292274648535930714 ) ) ;
#42630 = CARTESIAN_POINT ( 'NONE',  ( -0.5314960629921250401, 0.1660481256975885056, 0.3530559997133364547 ) ) ;
#42631 = CARTESIAN_POINT ( 'NONE',  ( 0.1377952755905518800, 0.07958543189024071263, -0.2665933059059888421 ) ) ;
#42632 = CARTESIAN_POINT ( 'NONE',  ( 1.601049868766404982, -0.5023911411419708095, -0.1820866141732282451 ) ) ;
#42633 = CARTESIAN_POINT ( 'NONE',  ( -0.7210809602247715278, -2.613618158232546091E-15, -0.3464511005275220379 ) ) ;
#42634 = CARTESIAN_POINT ( 'NONE',  ( 0.4790026246719167324, -0.05778040916215522460, 0.4822834645669289988 ) ) ;
#42635 = CARTESIAN_POINT ( 'NONE',  ( 1.450131233595801428, 0.2952755905511811885, 0.1292274648535926551 ) ) ;
#42636 = CARTESIAN_POINT ( 'NONE',  ( -0.3917322834645670104, -7.196005306013484475E-17, -2.236220472440944906 ) ) ;
#42637 = EDGE_LOOP ( 'NONE', ( #72684, #41374, #33615, #75178 ) ) ;
#42638 = ORIENTED_EDGE ( 'NONE', *, *, #20291, .F. ) ;
#42639 = CARTESIAN_POINT ( 'NONE',  ( 0.8989501312335964611, 0.2952755905511811885, 0.1292274648535926551 ) ) ;
#42640 = CARTESIAN_POINT ( 'NONE',  ( 0.03280839895013198948, 0.1771653543307087630, 0.09757992244046791164 ) ) ;
#42642 = FACE_OUTER_BOUND ( 'NONE', #65624, .T. ) ;
#42641 = FACE_OUTER_BOUND ( 'NONE', #22102, .T. ) ;
#42643 = CARTESIAN_POINT ( 'NONE',  ( -0.1049643490035302024, -0.3917322834645671215, -0.6292650918635172008 ) ) ;
#42644 = CARTESIAN_POINT ( 'NONE',  ( -0.9559795740584949852, -3.764720552277026557E-15, -0.3954974714151476278 ) ) ;
#42645 = CARTESIAN_POINT ( 'NONE',  ( 0.3049517105654749871, 8.471767977567108961E-16, -0.4445507791589058955 ) ) ;
#42646 = CARTESIAN_POINT ( 'NONE',  ( -0.1998031496062991630, -0.3460692066303959202, -2.347112860892388575 ) ) ;
#42647 = CARTESIAN_POINT ( 'NONE',  ( 1.076115485564305141, -0.6046776061558807314, 0.2411417322834647770 ) ) ;
#42648 = CARTESIAN_POINT ( 'NONE',  ( -0.7414698162729651543, -0.6692913385826771977, 0.1292274648535927661 ) ) ;
#42649 = CARTESIAN_POINT ( 'NONE',  ( -0.8464566929133852113, -0.5400638737290845981, -0.3530559997133363437 ) ) ;
#42650 = CARTESIAN_POINT ( 'NONE',  ( 0.7020997375328090762, -0.05778040916215560624, -0.4822834645669293319 ) ) ;
#42651 = CARTESIAN_POINT ( 'NONE',  ( 1.469816272965879911, 0.2306618581243847221, -0.2411417322834647770 ) ) ;
#42652 = CARTESIAN_POINT ( 'NONE',  ( 1.194225721784777594, 0.009842519685039467087, 0.3409548833797002021 ) ) ;
#42653 = APPLICATION_PROTOCOL_DEFINITION ( 'draft international standard', 'automotive_design', 1998, #61604 ) ;
#42654 = CARTESIAN_POINT ( 'NONE',  ( 1.174540682414699111, -0.2845877964562159024, 0.3641732283464567677 ) ) ;
#42655 = CARTESIAN_POINT ( 'NONE',  ( -0.7020997375328074108, -0.05778040916215522460, 0.4822834645669289988 ) ) ;
#42656 = CARTESIAN_POINT ( 'NONE',  ( 1.581364829396326277, -0.3162353388693409650, -0.4822834645669289433 ) ) ;
#42657 = CARTESIAN_POINT ( 'NONE',  ( 0.1049643490035304938, -0.3917322834645669549, 0.08005249343832024356 ) ) ;
#42658 = CARTESIAN_POINT ( 'NONE',  ( 0.01968503937007957949, -0.5400638737290845981, -0.3530559997133363437 ) ) ;
#42660 = DIRECTION ( 'NONE',  ( 0.000000000000000000, 0.000000000000000000, -1.000000000000000000 ) ) ;
#42659 = CARTESIAN_POINT ( 'NONE',  ( 1.030183727034121421, -0.05778040916215522460, 0.4822834645669289988 ) ) ;
#42661 = CARTESIAN_POINT ( 'NONE',  ( -1.128608923884513837, -0.5023911411419708095, 0.1820866141732285504 ) ) ;
#42662 = CARTESIAN_POINT ( 'NONE',  ( 0.2165354330708668673, -0.5400638737290844871, 0.3530559997133364547 ) ) ;
#42663 = CARTESIAN_POINT ( 'NONE',  ( 1.417322834645670104, -0.1870078740157479769, 0.3641732283464567677 ) ) ;
#42664 = CARTESIAN_POINT ( 'NONE',  ( -0.2867679344610364334, -0.2867679344610368219, -1.556411130412386656 ) ) ;
#42665 = CARTESIAN_POINT ( 'NONE',  ( -1.397637795275589623, 0.07958543189024085140, 0.2665933059059887866 ) ) ;
#42666 = CARTESIAN_POINT ( 'NONE',  ( 1.397637795275591177, 0.1660481256975883668, -0.3530559997133364547 ) ) ;
#42667 = CARTESIAN_POINT ( 'NONE',  ( 0.2223504907588284285, 1.906774035320677685, 0.2207610229706957194 ) ) ;
#42668 = CARTESIAN_POINT ( 'NONE',  ( -0.006561679790025524116, -0.2845877964562159024, 0.3641732283464567677 ) ) ;
#42669 = CARTESIAN_POINT ( 'NONE',  ( 0.01968503937007930540, 0.1660481256975885056, 0.3530559997133364547 ) ) ;
#42670 = CARTESIAN_POINT ( 'NONE',  ( -1.371391076115484609, -0.5511811023622046335, 0.09757992244046803654 ) ) ;
#42671 = CARTESIAN_POINT ( 'NONE',  ( -0.5774278215223089816, 0.2306618581243847221, -0.2411417322834647770 ) ) ;
#42672 = CARTESIAN_POINT ( 'NONE',  ( 1.437007874015748810, -0.5400638737290845981, -0.3530559997133363437 ) ) ;
#42673 = CARTESIAN_POINT ( 'NONE',  ( -0.1958661417322833942, -0.3392501089628018884, -0.3773159037083483325 ) ) ;
#42674 = EDGE_CURVE ( 'NONE', #70238, #60047, #53373, .T. ) ;
#42675 = LINE ( 'NONE', #35963, #7675 ) ;
#42676 = CARTESIAN_POINT ( 'NONE',  ( 1.404199475065617264, -0.4281496062992124485, 0.4176697321401328655 ) ) ;
#42677 = CARTESIAN_POINT ( 'NONE',  ( -0.4724409448818899238, 0.1265901696524986686, -1.841863517060367439 ) ) ;
#42678 = CARTESIAN_POINT ( 'NONE',  ( -1.200787401574802349, 0.1660481256975883668, -0.3530559997133364547 ) ) ;
#42679 = CARTESIAN_POINT ( 'NONE',  ( -1.056430446194224881, -0.5511811023622046335, 0.09757992244046803654 ) ) ;
#42680 = CARTESIAN_POINT ( 'NONE',  ( -0.4921259842519677963, -0.4536011799217367080, 0.2665933059059888421 ) ) ;
#42681 = CARTESIAN_POINT ( 'NONE',  ( -1.204164820379008294, 2.401574803149606474, -0.4915354330708643360 ) ) ;
#42682 = CARTESIAN_POINT ( 'NONE',  ( -0.1049868766404193215, -0.6046776061558807314, 0.2411417322834647770 ) ) ;
#42683 = CARTESIAN_POINT ( 'NONE',  ( -0.1115485564304453947, -0.5511811023622046335, 0.09757992244046803654 ) ) ;
#42684 = CARTESIAN_POINT ( 'NONE',  ( -1.069553805774277722, 0.1771653543307087630, 0.09757992244046791164 ) ) ;
#42685 = CARTESIAN_POINT ( 'NONE',  ( -1.679790026246718693, 0.2306618581243847221, -0.2411417322834647770 ) ) ;
#42686 = CARTESIAN_POINT ( 'NONE',  ( 1.502624671916010790, -0.2845877964562161244, -0.3641732283464567121 ) ) ;
#42687 = EDGE_CURVE ( 'NONE', #51714, #80, #38719, .T. ) ;
#42688 = CARTESIAN_POINT ( 'NONE',  ( 1.305774278215223960, -0.6692913385826771977, 0.1292274648535927661 ) ) ;
#42689 = CARTESIAN_POINT ( 'NONE',  ( 0.3634034883589535303, 1.231066118352841521, 2.000797776986567467 ) ) ;
#42690 = CARTESIAN_POINT ( 'NONE',  ( 0.5905511811023629321, 0.1771653543307087630, 0.000000000000000000 ) ) ;
#42691 = CARTESIAN_POINT ( 'NONE',  ( 0.8858267716535438430, 0.1660481256975885056, 0.3530559997133364547 ) ) ;
#42692 = CARTESIAN_POINT ( 'NONE',  ( 1.095800524934383846, -0.2845877964562159024, 0.3641732283464567677 ) ) ;
#42693 = VERTEX_POINT ( 'NONE', #6733 ) ;
#42694 = CARTESIAN_POINT ( 'NONE',  ( -1.108923884514435132, -0.05778040916215560624, -0.4822834645669293319 ) ) ;
#42695 = CARTESIAN_POINT ( 'NONE',  ( -1.056430446194224881, -0.6692913385826771977, 0.1292274648535927661 ) ) ;
#42696 = CARTESIAN_POINT ( 'NONE',  ( 0.05905511811023681640, 0.1660481256975883668, -0.3530559997133364547 ) ) ;
#42697 = CARTESIAN_POINT ( 'NONE',  ( -2.103514684734978601, 1.710972922415816999, -0.4417590601942929518 ) ) ;
#42698 = CARTESIAN_POINT ( 'NONE',  ( 0.1070741851644054776, -0.3996062992125984925, -2.366797900262467280 ) ) ;
#42699 = CARTESIAN_POINT ( 'NONE',  ( 0.7808398950131240079, -0.3162353388693405765, 0.4822834645669290543 ) ) ;
#42700 = CARTESIAN_POINT ( 'NONE',  ( -1.653543307086613234, -0.1870078740157480879, -0.4822834645669291653 ) ) ;
#42701 = CARTESIAN_POINT ( 'NONE',  ( -0.09186351706036663400, -0.4281496062992124485, 0.4176697321401328655 ) ) ;
#42702 = CARTESIAN_POINT ( 'NONE',  ( 0.8530183727034126306, 0.05413385826771626580, -0.4176697321401330321 ) ) ;
#42703 = CARTESIAN_POINT ( 'NONE',  ( -0.1998031496062994683, 0.3460692066303958092, -1.587926509186351698 ) ) ;
#42704 = CARTESIAN_POINT ( 'NONE',  ( 0.3420746716998660508, -0.1974969037888703871, -1.049868766404199460 ) ) ;
#42705 = CARTESIAN_POINT ( 'NONE',  ( 0.2925321140481932369, 0.2925321140481932369, -2.500000000000000444 ) ) ;
#42706 = CARTESIAN_POINT ( 'NONE',  ( -0.1830245018656607436, -0.2318981092368783414, 0.1465342031617537788 ) ) ;
#42707 = CARTESIAN_POINT ( 'NONE',  ( 0.2867679344610366554, 0.2867679344610366554, -0.7598425196850391306 ) ) ;
#42708 = CARTESIAN_POINT ( 'NONE',  ( -0.4068241469816267775, -0.004921259842519870586, -0.3153832671262229437 ) ) ;
#42709 = CARTESIAN_POINT ( 'NONE',  ( -0.7742782152230965886, 0.05413385826771666132, 0.4176697321401328100 ) ) ;
#42710 = CARTESIAN_POINT ( 'NONE',  ( 0.4527559055118117182, -0.5400638737290844871, 0.3530559997133364547 ) ) ;
#42711 = CARTESIAN_POINT ( 'NONE',  ( 4.837279021331061486E-17, -0.3949938075777409963, -2.360236220472441193 ) ) ;
#42712 = CARTESIAN_POINT ( 'NONE',  ( 1.548556430446194954, -0.6046776061558807314, 0.2411417322834647770 ) ) ;
#42713 = CARTESIAN_POINT ( 'NONE',  ( 1.345144356955381593, -0.3162353388693409650, -0.4822834645669289433 ) ) ;
#42714 = CARTESIAN_POINT ( 'NONE',  ( -0.1265901696524993347, 0.4724409448818895907, -2.526246719160104792 ) ) ;
#42715 = CARTESIAN_POINT ( 'NONE',  ( -0.3460692066303960868, 0.1998031496062990242, -1.758530183727034180 ) ) ;
#42716 = DIRECTION ( 'NONE',  ( 0.000000000000000000, 0.000000000000000000, -1.000000000000000000 ) ) ;
#42717 = CARTESIAN_POINT ( 'NONE',  ( 0.9317585301837276734, -0.4281496062992124485, 0.4176697321401328655 ) ) ;
#42718 = CARTESIAN_POINT ( 'NONE',  ( 1.410761154855643795, -0.2845877964562159024, 0.3641732283464567677 ) ) ;
#42720 = CARTESIAN_POINT ( 'NONE',  ( -1.384514435695537005, -0.6692913385826773087, -0.1292274648535924053 ) ) ;
#42719 = CARTESIAN_POINT ( 'NONE',  ( 1.528871391076116026, 0.2952755905511811885, 0.1292274648535926551 ) ) ;
#42721 = CARTESIAN_POINT ( 'NONE',  ( -0.3917322834645670659, 0.1049643490035301607, -2.632526615976691353 ) ) ;
#42722 = LINE ( 'NONE', #10758, #4735 ) ;
#42723 = CARTESIAN_POINT ( 'NONE',  ( 0.8858267716535438430, 0.1660481256975885056, 0.3530559997133364547 ) ) ;
#42724 = CARTESIAN_POINT ( 'NONE',  ( 1.469816272965879911, -0.5023911411419708095, 0.1820866141732285504 ) ) ;
#42725 = CARTESIAN_POINT ( 'NONE',  ( -0.4593175853018366950, 0.05413385826771666132, 0.4176697321401328100 ) ) ;
#42726 = CARTESIAN_POINT ( 'NONE',  ( -0.6036745406824141069, 0.2306618581243848609, 0.2411417322834645549 ) ) ;
#42727 = CARTESIAN_POINT ( 'NONE',  ( 1.463254593175853824, 0.2952755905511810774, -0.1292274648535930714 ) ) ;
#42728 = CARTESIAN_POINT ( 'NONE',  ( -9.594673741351313045E-17, 0.3917322834645670104, -0.08464566929133868212 ) ) ;
#42729 = CARTESIAN_POINT ( 'NONE',  ( 0.2493438320209980519, -0.4281496062992127816, -0.4176697321401328100 ) ) ;
#42730 = CARTESIAN_POINT ( 'NONE',  ( 0.3917322834645670104, -0.1049643490035303411, -2.465879265091863282 ) ) ;
#42731 = CARTESIAN_POINT ( 'NONE',  ( 1.633858267716535639, -0.5400638737290844871, 0.3530559997133364547 ) ) ;
#42732 = EDGE_LOOP ( 'NONE', ( #81892, #83, #18514 ) ) ;
#42733 = CARTESIAN_POINT ( 'NONE',  ( 0.3949938075777409408, 0.1058382717557500574, -2.644356955380577912 ) ) ;
#42734 = ORIENTED_EDGE ( 'NONE', *, *, #75585, .F. ) ;
#42735 = LINE ( 'NONE', #42321, #75816 ) ;
#42736 = CARTESIAN_POINT ( 'NONE',  ( -1.410761154855642463, -0.05778040916215522460, 0.4822834645669289988 ) ) ;
#42737 = CARTESIAN_POINT ( 'NONE',  ( -0.1070741851644051862, -0.3996062992125987146, -1.174540682414698001 ) ) ;
#42738 = CARTESIAN_POINT ( 'NONE',  ( -3.886287458032462006, 2.755905511811024056, -0.6299212598425202314 ) ) ;
#42739 = DIRECTION ( 'NONE',  ( -3.491481338843132961E-15, -0.000000000000000000, 1.000000000000000000 ) ) ;
#42740 = FACE_OUTER_BOUND ( 'NONE', #10941, .T. ) ;
#42741 = DIRECTION ( 'NONE',  ( 0.000000000000000000, 0.000000000000000000, 1.000000000000000000 ) ) ;
#42742 = CARTESIAN_POINT ( 'NONE',  ( 4.797336870675656522E-17, -0.3917322834645670104, -0.6358267716535433989 ) ) ;
#42743 = CARTESIAN_POINT ( 'NONE',  ( -0.3083989501312330295, -0.2845877964562161244, -0.3641732283464567121 ) ) ;
#42744 = EDGE_CURVE ( 'NONE', #48835, #10673, #39559, .T. ) ;
#42745 = CARTESIAN_POINT ( 'NONE',  ( -1.332020997375327642, -0.2845877964562161244, -0.3641732283464567121 ) ) ;
#42746 = CARTESIAN_POINT ( 'NONE',  ( -1.620734908136482577, 0.2952755905511811885, 0.1292274648535926551 ) ) ;
#42747 = CARTESIAN_POINT ( 'NONE',  ( 0.4068241469816279987, -0.4281496062992127816, -0.4176697321401328100 ) ) ;
#42748 = CARTESIAN_POINT ( 'NONE',  ( -1.358267716535432434, -0.5400638737290844871, 0.3530559997133364547 ) ) ;
#42749 = CARTESIAN_POINT ( 'NONE',  ( 0.3917322834645670104, -0.1049643490035303411, -0.2611548556430445256 ) ) ;
#42750 = ORIENTED_EDGE ( 'NONE', *, *, #39775, .F. ) ;
#42751 = CARTESIAN_POINT ( 'NONE',  ( 1.482939632545932307, 0.05413385826771626580, -0.4176697321401330321 ) ) ;
#42752 = CARTESIAN_POINT ( 'NONE',  ( 0.1574803149606299746, 0.5905511811023621549, 0.000000000000000000 ) ) ;
#42753 =( NAMED_UNIT ( * ) SI_UNIT ( $, .STERADIAN. ) SOLID_ANGLE_UNIT ( ) );
#42754 = CARTESIAN_POINT ( 'NONE',  ( -0.1265901696524986964, -0.4724409448818899238, -1.804461942257217677 ) ) ;
#42755 = CARTESIAN_POINT ( 'NONE',  ( 0.1752652180395700143, 0.2378425880835044193, 0.1496354662858539741 ) ) ;
#42756 = FACE_OUTER_BOUND ( 'NONE', #75938, .T. ) ;
#42757 = CARTESIAN_POINT ( 'NONE',  ( -0.6824146981627288167, 0.2306618581243848609, 0.2411417322834645549 ) ) ;
#42758 = CARTESIAN_POINT ( 'NONE',  ( 1.476377952755906442, -0.5400638737290844871, 0.3530559997133364547 ) ) ;
#42760 = CARTESIAN_POINT ( 'NONE',  ( 0.6496062992125991586, 0.1012011053420777407, 0.2882089793578257453 ) ) ;
#42759 = CARTESIAN_POINT ( 'NONE',  ( 0.7186703366786206804, -1.374501131054255944E-15, 0.4445507791589066726 ) ) ;
#42761 = CARTESIAN_POINT ( 'NONE',  ( 1.489501312335958172, -0.3162353388693405765, 0.4822834645669290543 ) ) ;
#42762 = CARTESIAN_POINT ( 'NONE',  ( -0.6824146981627291497, -0.6046776061558809534, -0.2411417322834644161 ) ) ;
#42763 = CARTESIAN_POINT ( 'NONE',  ( 0.1958661417322834497, 0.3392501089628018329, -0.3818704479976884336 ) ) ;
#42764 = CARTESIAN_POINT ( 'NONE',  ( -0.08530183727034056085, -0.08942795157528024563, -0.3641732283464568787 ) ) ;
#42765 = CARTESIAN_POINT ( 'NONE',  ( -0.3917322834645671215, 0.1049643490035301469, -0.2749343832020998413 ) ) ;
#42766 = CARTESIAN_POINT ( 'NONE',  ( -0.006561679790025524116, -0.08942795157528024563, -0.3641732283464568787 ) ) ;
#42767 = CARTESIAN_POINT ( 'NONE',  ( 0.5380577427821529035, -0.004921259842519870586, -0.3153832671262229437 ) ) ;
#42768 = CARTESIAN_POINT ( 'NONE',  ( 0.4658792650918640033, -0.3162353388693405765, 0.4822834645669290543 ) ) ;
#42769 = CARTESIAN_POINT ( 'NONE',  ( -0.7020997375328074108, -0.08942795157527998196, 0.3641732283464567121 ) ) ;
#42770 = CARTESIAN_POINT ( 'NONE',  ( 0.3917322834645670104, -0.1049643490035303411, -2.150918635170603554 ) ) ;
#42771 = CARTESIAN_POINT ( 'NONE',  ( -1.541994750656167090, -0.6692913385826773087, -0.1292274648535924053 ) ) ;
#42772 = CARTESIAN_POINT ( 'NONE',  ( -0.9251968503937002541, -0.5400638737290845981, -0.3530559997133363437 ) ) ;
#42773 = CARTESIAN_POINT ( 'NONE',  ( -0.4724409448818895907, -0.1265901696524993070, -0.7526246719160103460 ) ) ;
#42774 = CARTESIAN_POINT ( 'NONE',  ( 0.1968503937007881344, 0.2952755905511811885, 0.000000000000000000 ) ) ;
#42775 = CARTESIAN_POINT ( 'NONE',  ( -0.6561679790026240244, 0.2306618581243847221, -0.2411417322834647770 ) ) ;
#42776 = CARTESIAN_POINT ( 'NONE',  ( 1.141732283464567788, -0.5511811023622047445, 6.969142054262312111E-17 ) ) ;
#42777 = CARTESIAN_POINT ( 'NONE',  ( 0.06561679790026316017, -0.004921259842519870586, -0.3153832671262229437 ) ) ;
#42778 = CARTESIAN_POINT ( 'NONE',  ( -0.09842519685039295696, 0.1660481256975883668, -0.3530559997133364547 ) ) ;
#42779 = CARTESIAN_POINT ( 'NONE',  ( -0.7611548556430438595, -0.6046776061558809534, -0.2411417322834644161 ) ) ;
#42780 = CARTESIAN_POINT ( 'NONE',  ( -0.5944687039322197331, 1.968503937007873850, -0.4915354330708654462 ) ) ;
#42781 = CARTESIAN_POINT ( 'NONE',  ( -1.011202504342156416, -2.294479370626195693E-15, 0.3464511005275217603 ) ) ;
#42782 =( REPRESENTATION_RELATIONSHIP ('NONE','NONE', #79348, #82043 ) REPRESENTATION_RELATIONSHIP_WITH_TRANSFORMATION ( #36345 )SHAPE_REPRESENTATION_RELATIONSHIP( ) );
#42783 = CARTESIAN_POINT ( 'NONE',  ( 0.1312335958005257930, 0.2306618581243847221, -0.2411417322834647770 ) ) ;
#42784 = EDGE_LOOP ( 'NONE', ( #45674, #31022, #5284, #60240 ) ) ;
#42785 = CARTESIAN_POINT ( 'NONE',  ( -9.787531504996566615E-17, 0.3996062992125985480, -2.124015748031495843 ) ) ;
#42786 = CARTESIAN_POINT ( 'NONE',  ( 1.135170603674541256, 0.2952755905511811885, 0.1292274648535926551 ) ) ;
#42787 = CARTESIAN_POINT ( 'NONE',  ( -0.7414698162729651543, 0.1771653543307087075, -0.09757992244046823083 ) ) ;
#42788 = CARTESIAN_POINT ( 'NONE',  ( -0.4002624671916004129, -0.05778040916215560624, -0.4822834645669293319 ) ) ;
#42789 = CARTESIAN_POINT ( 'NONE',  ( 1.253280839895013710, -0.05778040916215560624, -0.4822834645669293319 ) ) ;
#42790 = CARTESIAN_POINT ( 'NONE',  ( 0.9776902887139113929, -0.6692913385826773087, -0.1292274648535924053 ) ) ;
#42791 = CARTESIAN_POINT ( 'NONE',  ( -1.509186351706035767, -0.4281496062992124485, 0.4176697321401328655 ) ) ;
#42792 = CARTESIAN_POINT ( 'NONE',  ( -1.043307086614172707, 0.07958543189024071263, -0.2665933059059888421 ) ) ;
#42793 = CARTESIAN_POINT ( 'NONE',  ( 4.893765752498283308E-17, -0.3996062992125985480, -0.3129921259842520231 ) ) ;
#42794 = CARTESIAN_POINT ( 'NONE',  ( -0.3996062992125987146, 0.1070741851644051862, -0.6627296587926508886 ) ) ;
#42795 = CARTESIAN_POINT ( 'NONE',  ( -0.3420746716998659953, -0.1974969037888706647, 0.1049868766404198905 ) ) ;
#42796 = CARTESIAN_POINT ( 'NONE',  ( 1.607611548556431069, -0.5511811023622048555, -0.09757992244046775898 ) ) ;
#42797 = EDGE_CURVE ( 'NONE', #4140, #82716, #58919, .T. ) ;
#42798 = CARTESIAN_POINT ( 'NONE',  ( 1.010498687664042716, -0.004921259842519870586, -0.3153832671262229437 ) ) ;
#42799 = CARTESIAN_POINT ( 'NONE',  ( 0.3608923884514443348, 0.2952755905511810774, -0.1292274648535930714 ) ) ;
#42800 = CARTESIAN_POINT ( 'NONE',  ( -1.666666666666665853, 0.05413385826771626580, -0.4176697321401330321 ) ) ;
#42801 = CARTESIAN_POINT ( 'NONE',  ( -0.2891555358219909388, -0.2891555358219912164, -1.080708661417322913 ) ) ;
#42802 = CARTESIAN_POINT ( 'NONE',  ( 0.8727034120734913358, -0.08942795157527998196, 0.3641732283464567121 ) ) ;
#42803 = CARTESIAN_POINT ( 'NONE',  ( -0.4133858267716528645, -0.5400638737290844871, 0.3530559997133364547 ) ) ;
#42804 = CARTESIAN_POINT ( 'NONE',  ( -0.7874015748031489847, -0.1870078740157480879, -0.4822834645669291653 ) ) ;
#42805 = CARTESIAN_POINT ( 'NONE',  ( 1.266404199475066328, -0.3162353388693409650, -0.4822834645669289433 ) ) ;
#42806 = CARTESIAN_POINT ( 'NONE',  ( -0.4724409448818898682, -8.678599364036362592E-17, -0.9842519685039369248 ) ) ;
#42807 = CARTESIAN_POINT ( 'NONE',  ( 4.893765752498283924E-17, -0.3996062992125986035, -2.440944881889763884 ) ) ;
#42808 = CARTESIAN_POINT ( 'NONE',  ( 0.1049868766404206816, -0.5023911411419708095, -0.1820866141732282451 ) ) ;
#42809 = ORIENTED_EDGE ( 'NONE', *, *, #16767, .T. ) ;
#42810 = CARTESIAN_POINT ( 'NONE',  ( 0.3917322834645670659, -0.1049643490035303273, -0.8956886071204221977 ) ) ;
#42811 = ORIENTED_EDGE ( 'NONE', *, *, #1873, .F. ) ;
#42812 = CARTESIAN_POINT ( 'NONE',  ( -1.010498687664041384, -0.4281496062992127816, -0.4176697321401328100 ) ) ;
#42813 = CARTESIAN_POINT ( 'NONE',  ( -0.2559055118110227234, -0.5400638737290844871, 0.3530559997133364547 ) ) ;
#42814 = CARTESIAN_POINT ( 'NONE',  ( -0.4593175853018364174, -0.4281496062992127816, -0.4176697321401328100 ) ) ;
#42815 = CARTESIAN_POINT ( 'NONE',  ( 0.8530183727034128527, -0.4281496062992124485, 0.4176697321401328655 ) ) ;
#42816 = CARTESIAN_POINT ( 'NONE',  ( -0.3871391076115476282, -0.05778040916215522460, 0.4822834645669289988 ) ) ;
#42817 = CARTESIAN_POINT ( 'NONE',  ( -1.259842519685038686, -0.1870078740157480879, -0.4822834645669291653 ) ) ;
#42818 = CARTESIAN_POINT ( 'NONE',  ( -0.5249343832020990641, -0.6046776061558809534, -0.2411417322834644161 ) ) ;
#42819 = CARTESIAN_POINT ( 'NONE',  ( 0.8595800524934390507, -0.05778040916215560624, -0.4822834645669293319 ) ) ;
#42820 = CARTESIAN_POINT ( 'NONE',  ( 0.5314960629921264834, 0.1660481256975883668, -0.3530559997133364547 ) ) ;
#42821 = ADVANCED_FACE ( 'NONE', ( #57652 ), #14, .T. ) ;
#42822 = CARTESIAN_POINT ( 'NONE',  ( 0.1958661417322834775, 0.3392501089628018884, -0.9238845144356954142 ) ) ;
#42823 = CARTESIAN_POINT ( 'NONE',  ( -0.2296587926509179312, -0.08942795157527998196, 0.3641732283464567121 ) ) ;
#42824 = ORIENTED_EDGE ( 'NONE', *, *, #23015, .T. ) ;
#42825 = CARTESIAN_POINT ( 'NONE',  ( -0.1974969037888706647, 0.3420746716998658843, -1.272965879265091749 ) ) ;
#42826 = ORIENTED_EDGE ( 'NONE', *, *, #36816, .T. ) ;
#42827 = CARTESIAN_POINT ( 'NONE',  ( -1.463254593175852492, -0.5511811023622048555, -0.09757992244046775898 ) ) ;
#42828 = CARTESIAN_POINT ( 'NONE',  ( -0.4461942257217840213, -0.6046776061558809534, -0.2411417322834644161 ) ) ;
#42829 = CARTESIAN_POINT ( 'NONE',  ( 0.7773926554473647998, 8.471767977567108961E-16, -0.4445507791589058955 ) ) ;
#42830 = CARTESIAN_POINT ( 'NONE',  ( -0.8202099737532801971, -0.6692913385826771977, 0.1292274648535927661 ) ) ;
#42831 = CARTESIAN_POINT ( 'NONE',  ( -0.9317585301837263412, 0.05413385826771666132, 0.4176697321401328100 ) ) ;
#42832 = CARTESIAN_POINT ( 'NONE',  ( -1.456692913385826182, 0.2952755905511811885, 0.000000000000000000 ) ) ;
#42833 = CARTESIAN_POINT ( 'NONE',  ( -1.646981627296586703, -0.3162353388693409650, -0.4822834645669289433 ) ) ;
#42834 = CARTESIAN_POINT ( 'NONE',  ( 1.069553805774278832, 0.1771653543307087075, -0.09757992244046823083 ) ) ;
#42835 = CARTESIAN_POINT ( 'NONE',  ( 1.171093442848939681, -8.644661201599092366E-16, -0.4445507791589066171 ) ) ;
#42836 = CARTESIAN_POINT ( 'NONE',  ( 0.3917322834645669549, 0.1049643490035304660, -0.05183727034120744204 ) ) ;
#42837 = CARTESIAN_POINT ( 'NONE',  ( 0.2034120734908142214, 0.1771653543307087075, -0.09757992244046823083 ) ) ;
#42838 = CARTESIAN_POINT ( 'NONE',  ( -0.3674540682414689785, 0.2306618581243848609, 0.2411417322834645549 ) ) ;
#42839 = DIRECTION ( 'NONE',  ( -0.000000000000000000, 1.000000000000000000, -0.000000000000000000 ) ) ;
#42840 = CARTESIAN_POINT ( 'NONE',  ( -0.2362204724409440182, -0.1870078740157479769, 0.4822834645669291653 ) ) ;
#42841 = ORIENTED_EDGE ( 'NONE', *, *, #20396, .T. ) ;
#42842 = CARTESIAN_POINT ( 'NONE',  ( -0.1998031496062994683, 0.3460692066303958092, -2.060367454068241511 ) ) ;
#42843 = CARTESIAN_POINT ( 'NONE',  ( -0.5314960629921169355, 2.755905511811024056, -2.583694225513482490 ) ) ;
#42844 = ORIENTED_EDGE ( 'NONE', *, *, #1933, .T. ) ;
#42845 = CARTESIAN_POINT ( 'NONE',  ( -0.2925321140481932369, 0.2925321140481931259, -1.513779527559054872 ) ) ;
#42846 = CARTESIAN_POINT ( 'NONE',  ( 1.141392835773559211, 0.4110443821404751730, 0.9642274814428540841 ) ) ;
#42847 = CARTESIAN_POINT ( 'NONE',  ( -0.7283464566929126471, 0.07958543189024071263, -0.2665933059059888421 ) ) ;
#42848 = CARTESIAN_POINT ( 'NONE',  ( -0.9842519685039365918, -0.6692913385826771977, 8.415575281601705876E-17 ) ) ;
#42849 = CARTESIAN_POINT ( 'NONE',  ( 0.4724409448818896462, 0.1265901696524990294, -0.4396325459317584339 ) ) ;
#42850 = CARTESIAN_POINT ( 'NONE',  ( -0.4256212168908878879, 1.327274814196968133, 3.913940744879238487 ) ) ;
#42851 = CARTESIAN_POINT ( 'NONE',  ( 0.1958661417322834775, 0.3392501089628018884, -2.433727034120734878 ) ) ;
#42852 = CARTESIAN_POINT ( 'NONE',  ( 1.410761154855643795, -0.05778040916215560624, -0.4822834645669293319 ) ) ;
#42853 = CARTESIAN_POINT ( 'NONE',  ( 0.3215223097112867578, -0.05778040916215522460, 0.4822834645669289988 ) ) ;
#42854 = CARTESIAN_POINT ( 'NONE',  ( 0.4855643044619430415, -0.4281496062992127816, -0.4176697321401328100 ) ) ;
#42855 = CARTESIAN_POINT ( 'NONE',  ( -0.4986876640419939388, 0.1283753931104746893, -0.1820866141732285504 ) ) ;
#42856 = CARTESIAN_POINT ( 'NONE',  ( -0.5118110236220466680, -0.6692913385826771977, 8.415575281601705876E-17 ) ) ;
#42857 = CARTESIAN_POINT ( 'NONE',  ( -0.3458507752293906723, -0.3458507752293910609, -2.183070866141731958 ) ) ;
#42858 = CARTESIAN_POINT ( 'NONE',  ( -0.9580052493438311334, -0.4281496062992124485, 0.4176697321401328655 ) ) ;
#42859 = CARTESIAN_POINT ( 'NONE',  ( -0.1974969037888704149, -0.3420746716998661063, -2.347112860892388575 ) ) ;
#42860 = CARTESIAN_POINT ( 'NONE',  ( 1.364829396325459854, -0.5023911411419708095, -0.1820866141732282451 ) ) ;
#42861 = CARTESIAN_POINT ( 'NONE',  ( -0.2427821522309703550, -0.08942795157528024563, -0.3641732283464568787 ) ) ;
#42862 = CARTESIAN_POINT ( 'NONE',  ( 1.141732283464567788, -0.5511811023622047445, 6.969142054262312111E-17 ) ) ;
#42863 = CARTESIAN_POINT ( 'NONE',  ( -1.377952755905511140, 0.2952755905511811885, 0.000000000000000000 ) ) ;
#42864 = CARTESIAN_POINT ( 'NONE',  ( -1.227034120734907141, -0.5511811023622048555, -0.09757992244046775898 ) ) ;
#42865 = CARTESIAN_POINT ( 'NONE',  ( 0.1133856558944468795, -0.2726377952755905665, 0.1574803149606299191 ) ) ;
#42866 = CARTESIAN_POINT ( 'NONE',  ( -1.312335958005248715, -0.6046776061558809534, -0.2411417322834644161 ) ) ;
#42867 = CARTESIAN_POINT ( 'NONE',  ( -0.4461942257217840213, -0.6046776061558809534, -0.2411417322834644161 ) ) ;
#42868 = CARTESIAN_POINT ( 'NONE',  ( -2.131054703900732150, 1.408268389154270883, 0.4567427728026676181 ) ) ;
#42869 = CARTESIAN_POINT ( 'NONE',  ( 0.03280839895013198948, -0.5511811023622048555, -0.09757992244046775898 ) ) ;
#42870 = CARTESIAN_POINT ( 'NONE',  ( -1.601049868766403650, -0.5023911411419708095, 0.1820866141732285504 ) ) ;
#42871 =( BOUNDED_CURVE ( )  B_SPLINE_CURVE ( 2, ( #61564, #80936, #29975, #55639, #17783, #75850, #43417, #5139, #43825, #48922, #17380, #69115, #4716 ),
 .UNSPECIFIED., .F., .F. ) 
 B_SPLINE_CURVE_WITH_KNOTS ( ( 3, 2, 2, 2, 2, 2, 3 ),
 ( 0.1733310946348008696, 0.1742424242424242542, 0.1780303030303030387, 0.1818181818181818232, 0.1856060606060606077, 0.1893939393939393923, 0.1903052690015628601 ),
 .UNSPECIFIED. ) 
 CURVE ( )  GEOMETRIC_REPRESENTATION_ITEM ( )  RATIONAL_B_SPLINE_CURVE ( ( 0.9875488213027527884, 0.9918020599134683701, 1.000000000000000000, 0.9659258262890683122, 1.000000000000000000, 0.9659258262890683122, 1.000000000000000000, 0.9659258262890683122, 1.000000000000000000, 0.9659258262890683122, 1.000000000000000000, 0.9918020599134675930, 0.9875488213027519002 ) ) 
 REPRESENTATION_ITEM ( '' )  );
#42872 = CARTESIAN_POINT ( 'NONE',  ( 0.5905511811023629321, 0.2952755905511811885, 0.000000000000000000 ) ) ;
#42873 = CARTESIAN_POINT ( 'NONE',  ( 3.937007874015748143, 2.559055118110236560, -0.3149606299212596716 ) ) ;
#42874 = CARTESIAN_POINT ( 'NONE',  ( 1.535433070866142335, -0.5511811023622047445, 6.969142054262312111E-17 ) ) ;
#42875 = CARTESIAN_POINT ( 'NONE',  ( -0.8398950131233589023, -0.6046776061558809534, -0.2411417322834644161 ) ) ;
#42876 = CARTESIAN_POINT ( 'NONE',  ( -0.2165354330708654795, 0.07958543189024085140, 0.2665933059059887866 ) ) ;
#42877 = CARTESIAN_POINT ( 'NONE',  ( 1.141392835773559211, 1.299212598425196985, 1.318558190104271333 ) ) ;
#42878 = CARTESIAN_POINT ( 'NONE',  ( 0.1377952755905518800, -0.4536011799217367080, 0.2665933059059888421 ) ) ;
#42879 = CARTESIAN_POINT ( 'NONE',  ( -0.2755905511811015396, -0.6692913385826771977, 8.415575281601705876E-17 ) ) ;
#42880 = CARTESIAN_POINT ( 'NONE',  ( -9.787531504996566615E-17, 0.3996062992125985480, -0.8641732283464567121 ) ) ;
#42881 = CARTESIAN_POINT ( 'NONE',  ( -0.3917322834645670104, -7.196005306013484475E-17, -2.171259842519685179 ) ) ;
#42882 = CARTESIAN_POINT ( 'NONE',  ( 0.6889763779527563470, 0.07958543189024071263, -0.2665933059059888421 ) ) ;
#42883 = CARTESIAN_POINT ( 'NONE',  ( 0.07874015748031558404, -0.1870078740157479769, 0.4822834645669291653 ) ) ;
#42884 = CARTESIAN_POINT ( 'NONE',  ( -0.6758530183727028406, 0.2952755905511811885, 0.1292274648535926551 ) ) ;
#42885 = CARTESIAN_POINT ( 'NONE',  ( -0.7677165354330699465, -0.4536011799217368745, -0.2665933059059886201 ) ) ;
#42886 = CARTESIAN_POINT ( 'NONE',  ( 0.5314960629920993940, 2.716535433070866645, 2.543486866223394482 ) ) ;
#42887 = CARTESIAN_POINT ( 'NONE',  ( -0.4921259842519677963, 0.07958543189024071263, -0.2665933059059888421 ) ) ;
#42888 = CARTESIAN_POINT ( 'NONE',  ( 0.1049868766404206816, 0.2306618581243848609, 0.2411417322834645549 ) ) ;
#42889 = VECTOR ( 'NONE', #59860, 39.37007874015748143 ) ;
#42890 = CARTESIAN_POINT ( 'NONE',  ( -1.345144356955379816, -0.08942795157528024563, -0.3641732283464568787 ) ) ;
#42891 = CARTESIAN_POINT ( 'NONE',  ( 4.893765752498283308E-17, -0.3996062992125985480, -1.572834645669291431 ) ) ;
#42892 = CARTESIAN_POINT ( 'NONE',  ( -1.476377952755905110, 0.1660481256975885056, 0.3530559997133364547 ) ) ;
#42893 = VERTEX_POINT ( 'NONE', #25668 ) ;
#42894 = EDGE_CURVE ( 'NONE', #65196, #15966, #58142, .T. ) ;
#42895 = CARTESIAN_POINT ( 'NONE',  ( -1.673228346456691717, 0.07958543189024071263, -0.2665933059059888421 ) ) ;
#42896 = CARTESIAN_POINT ( 'NONE',  ( -0.3543307086614165824, -0.6692913385826771977, 8.415575281601705876E-17 ) ) ;
#42897 = CARTESIAN_POINT ( 'NONE',  ( -1.049868766404198794, -0.6046776061558807314, 0.2411417322834647770 ) ) ;
#42898 = CARTESIAN_POINT ( 'NONE',  ( 0.2867679344610365999, 0.2867679344610365999, -1.482283464566929387 ) ) ;
#42899 = CYLINDRICAL_SURFACE ( 'NONE', #25667, 0.4744094488188972947 ) ;
#42900 = CARTESIAN_POINT ( 'NONE',  ( 0.9383202099737538715, -0.05778040916215560624, -0.4822834645669293319 ) ) ;
#42901 = CARTESIAN_POINT ( 'NONE',  ( 0.5708661417322842269, 0.1660481256975885056, 0.3530559997133364547 ) ) ;
#42902 = DIRECTION ( 'NONE',  ( -0.000000000000000000, 1.000000000000000000, -0.000000000000000000 ) ) ;
#42903 = CARTESIAN_POINT ( 'NONE',  ( -0.2925321140481932369, 0.2925321140481930704, -2.301181102362204633 ) ) ;
#42904 = CARTESIAN_POINT ( 'NONE',  ( -1.706036745406823485, 0.2306618581243848609, 0.2411417322834645549 ) ) ;
#42905 = CARTESIAN_POINT ( 'NONE',  ( 0.3996062992125986590, -0.1070741851644053111, -0.8989501312335956840 ) ) ;
#42906 = ORIENTED_EDGE ( 'NONE', *, *, #41175, .T. ) ;
#42907 = CARTESIAN_POINT ( 'NONE',  ( -0.8070866141732276899, 0.07958543189024071263, -0.2665933059059888421 ) ) ;
#42908 = CARTESIAN_POINT ( 'NONE',  ( 0.3917322834645670104, -0.1049643490035303411, -2.465879265091863282 ) ) ;
#42909 = ORIENTED_EDGE ( 'NONE', *, *, #80976, .F. ) ;
#42910 = CARTESIAN_POINT ( 'NONE',  ( 0.2559055118110243332, -0.5400638737290845981, -0.3530559997133363437 ) ) ;
#42911 = CARTESIAN_POINT ( 'NONE',  ( -0.5839895013123351797, 0.2952755905511810774, -0.1292274648535930714 ) ) ;
#42912 = CARTESIAN_POINT ( 'NONE',  ( -1.246719160104985846, -0.4281496062992127816, -0.4176697321401328100 ) ) ;
#42913 = CARTESIAN_POINT ( 'NONE',  ( 1.102362204724410155, -0.1870078740157480879, -0.4822834645669291653 ) ) ;
#42914 = CARTESIAN_POINT ( 'NONE',  ( -1.148293963254592542, 0.1771653543307087630, 0.09757992244046791164 ) ) ;
#42915 = DIRECTION ( 'NONE',  ( 0.000000000000000000, -0.4999999999999998890, 0.8660254037844385966 ) ) ;
#42916 = CARTESIAN_POINT ( 'NONE',  ( 0.09186351706036827158, 0.05413385826771666132, 0.4176697321401328100 ) ) ;
#42917 = CARTESIAN_POINT ( 'NONE',  ( -1.122047244094487306, 0.1660481256975883668, -0.3530559997133364547 ) ) ;
#42918 = CARTESIAN_POINT ( 'NONE',  ( 0.3392501089628018329, 0.1958661417322835052, -1.786069923063305032 ) ) ;
#42919 = CARTESIAN_POINT ( 'NONE',  ( -1.528871391076114250, -0.6692913385826771977, 0.1292274648535927661 ) ) ;
#42920 = CARTESIAN_POINT ( 'NONE',  ( -1.614173228346456712, 0.7166040191147899918, -0.1372047244094478091 ) ) ;
#42921 = CARTESIAN_POINT ( 'NONE',  ( 0.2867679344610365999, -0.2867679344610365444, 0.06692913385826775030 ) ) ;
#42922 = CARTESIAN_POINT ( 'NONE',  ( 0.8333333333333340365, -0.5511811023622046335, 0.09757992244046803654 ) ) ;
#42923 = ORIENTED_EDGE ( 'NONE', *, *, #46991, .T. ) ;
#42924 = CARTESIAN_POINT ( 'NONE',  ( 0.3949938075777409408, 0.1058382717557500574, -0.2821522309711286813 ) ) ;
#42925 = CARTESIAN_POINT ( 'NONE',  ( -1.023622047244093558, -0.1870078740157479769, 0.4822834645669291653 ) ) ;
#42926 = ORIENTED_EDGE ( 'NONE', *, *, #16862, .F. ) ;
#42927 = CARTESIAN_POINT ( 'NONE',  ( 0.09186351706036799403, -0.3690944881889765550, -0.3153832671262227771 ) ) ;
#42928 = LINE ( 'NONE', #69449, #13955 ) ;
#42929 = CARTESIAN_POINT ( 'NONE',  ( 0.4068241469816279987, -0.4281496062992127816, -0.4176697321401328100 ) ) ;
#42930 = CARTESIAN_POINT ( 'NONE',  ( 0.6299212598425204535, -0.1870078740157479769, 0.4822834645669291653 ) ) ;
#42931 = CARTESIAN_POINT ( 'NONE',  ( -0.7808398950131225646, -0.05778040916215522460, 0.4822834645669289988 ) ) ;
#42932 = CARTESIAN_POINT ( 'NONE',  ( -0.3917322834645670659, -7.196005306013484475E-17, -1.138470759351392969 ) ) ;
#42933 = CARTESIAN_POINT ( 'NONE',  ( -0.9055118110236215490, -0.6692913385826771977, 8.415575281601705876E-17 ) ) ;
#42934 = EDGE_CURVE ( 'NONE', #18593, #949, #3132, .T. ) ;
#42935 = CARTESIAN_POINT ( 'NONE',  ( 0.3392501089628018884, -0.1958661417322834220, -2.709317585301837195 ) ) ;
#42936 = CARTESIAN_POINT ( 'NONE',  ( 1.384514435695538337, -0.5511811023622046335, 0.09757992244046803654 ) ) ;
#42937 = CARTESIAN_POINT ( 'NONE',  ( -1.167979002624671470, 0.05413385826771666132, 0.4176697321401328100 ) ) ;
#42938 = CARTESIAN_POINT ( 'NONE',  ( 0.9251968503937015864, 0.1660481256975883668, -0.3530559997133364547 ) ) ;
#42939 = CARTESIAN_POINT ( 'NONE',  ( 1.023622047244095334, -0.1870078740157479769, 0.4822834645669291653 ) ) ;
#42940 = CARTESIAN_POINT ( 'NONE',  ( 0.3996062992125986590, -0.1070741851644053111, -1.056430446194225992 ) ) ;
#42941 = CARTESIAN_POINT ( 'NONE',  ( -1.003937007874015297, -0.5400638737290845981, -0.3530559997133363437 ) ) ;
#42942 = CARTESIAN_POINT ( 'NONE',  ( -0.3996062992125984925, -0.1070741851644056858, -0.4376640419947506744 ) ) ;
#42943 = CARTESIAN_POINT ( 'NONE',  ( 0.2165354330708668673, 0.1660481256975883668, -0.3530559997133364547 ) ) ;
#42944 = CARTESIAN_POINT ( 'NONE',  ( -0.1070741851644056997, 0.3996062992125986035, -2.211286089238845065 ) ) ;
#42945 = CARTESIAN_POINT ( 'NONE',  ( -0.6102362204724400829, -0.5400638737290845981, -0.3530559997133363437 ) ) ;
#42946 = CARTESIAN_POINT ( 'NONE',  ( -1.384514435695537005, -0.5511811023622048555, -0.09757992244046775898 ) ) ;
#42947 = CARTESIAN_POINT ( 'NONE',  ( 0.4724409448818904789, -0.1870078740157480601, -0.3641732283464567677 ) ) ;
#42948 = CARTESIAN_POINT ( 'NONE',  ( 0.9186351706036751663, -0.6046776061558807314, 0.2411417322834647770 ) ) ;
#42949 = CARTESIAN_POINT ( 'NONE',  ( 0.1265901696524990294, -0.4724409448818896462, -1.264435695538057569 ) ) ;
#42950 = CARTESIAN_POINT ( 'NONE',  ( 0.9120734908136490793, 0.1771653543307087075, -0.09757992244046823083 ) ) ;
#42951 = ADVANCED_FACE ( 'NONE', ( #14742 ), #2932, .T. ) ;
#42952 = CARTESIAN_POINT ( 'NONE',  ( 0.7217847769028878924, -0.4281496062992127816, -0.4176697321401328100 ) ) ;
#42953 = CARTESIAN_POINT ( 'NONE',  ( -9.674558042662122972E-17, 0.3949938075777409963, -0.5492125984251968740 ) ) ;
#42954 = CARTESIAN_POINT ( 'NONE',  ( -0.6430446194225716283, -0.4281496062992124485, 0.4176697321401328655 ) ) ;
#42955 = CARTESIAN_POINT ( 'NONE',  ( 1.348312163386739426, 0.2929341459200028863, 0.6402614161801758463 ) ) ;
#42956 = CARTESIAN_POINT ( 'NONE',  ( 1.102362204724410155, -0.1870078740157479769, 0.3641732283464567677 ) ) ;
#42957 = CARTESIAN_POINT ( 'NONE',  ( -0.4199475065616791736, 0.2306618581243847221, -0.2411417322834647770 ) ) ;
#42958 = EDGE_CURVE ( 'NONE', #18885, #58371, #21628, .T. ) ;
#42959 = CARTESIAN_POINT ( 'NONE',  ( -0.09842519685039295696, 0.1660481256975883668, -0.3530559997133364547 ) ) ;
#42960 = CARTESIAN_POINT ( 'NONE',  ( 0.4735649329124898554, 1.569965579892641960, -1.017216587056824162 ) ) ;
#42961 = CARTESIAN_POINT ( 'NONE',  ( 0.3018372703412079971, -0.4281496062992124485, 0.4176697321401328655 ) ) ;
#42962 = CARTESIAN_POINT ( 'NONE',  ( 0.04593175853018440641, -0.5511811023622046335, 0.09757992244046803654 ) ) ;
#42963 = CARTESIAN_POINT ( 'NONE',  ( -2.867261597185507327, 1.070284760220065579, -0.08454815954496505692 ) ) ;
#42964 = CARTESIAN_POINT ( 'NONE',  ( -0.1115485564304453947, -0.5511811023622046335, 0.09757992244046803654 ) ) ;
#42965 = CARTESIAN_POINT ( 'NONE',  ( 0.9448818897637802916, -0.1870078740157479769, 0.3641732283464567677 ) ) ;
#42966 = CARTESIAN_POINT ( 'NONE',  ( -0.1021718162100117705, 1.074111179983719744, -1.580847797370428687 ) ) ;
#42967 = CARTESIAN_POINT ( 'NONE',  ( -0.3996062992125984925, -0.1070741851644056858, -1.697506561679790194 ) ) ;
#42968 = CARTESIAN_POINT ( 'NONE',  ( 0.1968503937007881344, -0.6692913385826771977, 8.415575281601705876E-17 ) ) ;
#42969 = CARTESIAN_POINT ( 'NONE',  ( -0.1049643490035302024, -0.3917322834645671215, -1.324146981627296826 ) ) ;
#42970 = CARTESIAN_POINT ( 'NONE',  ( -0.2749078412854699671, -0.2798680777847345480, 3.457013956890523347E-17 ) ) ;
#42971 = CARTESIAN_POINT ( 'NONE',  ( -0.4265091863517051496, 0.1771653543307087075, -0.09757992244046823083 ) ) ;
#42972 = CARTESIAN_POINT ( 'NONE',  ( -0.1771653543307080136, 0.1660481256975883668, -0.3530559997133364547 ) ) ;
#42973 = CARTESIAN_POINT ( 'NONE',  ( 0.8858267716535438430, 0.07958543189024085140, 0.2665933059059887866 ) ) ;
#42974 = CARTESIAN_POINT ( 'NONE',  ( 0.06247320855440641890, 1.066079912482593262, -1.120731204487458665 ) ) ;
#42975 = CARTESIAN_POINT ( 'NONE',  ( 1.325459317585302665, -0.004921259842519870586, -0.3153832671262229437 ) ) ;
#42976 = CARTESIAN_POINT ( 'NONE',  ( -0.03937007874015669567, 0.2952755905511811885, 0.000000000000000000 ) ) ;
#42977 = ADVANCED_FACE ( 'NONE', ( #21453 ), #24803, .F. ) ;
#42978 = CARTESIAN_POINT ( 'NONE',  ( 0.9776902887139113929, -0.6692913385826773087, -0.1292274648535924053 ) ) ;
#42979 = CARTESIAN_POINT ( 'NONE',  ( 0.06838555148300280717, 1.067631514832606543, -1.854691556240662731 ) ) ;
#42980 = CARTESIAN_POINT ( 'NONE',  ( 0.2099737532808405305, 0.2306618581243847221, -0.2411417322834647770 ) ) ;
#42981 = CARTESIAN_POINT ( 'NONE',  ( 1.259842519685040019, -0.1870078740157480879, -0.4822834645669291653 ) ) ;
#42982 = CARTESIAN_POINT ( 'NONE',  ( 0.5314960629921267055, -0.5400638737290844871, 0.3530559997133364547 ) ) ;
#42983 = CARTESIAN_POINT ( 'NONE',  ( -0.4724409448818898682, -8.678599364036362592E-17, -0.2736220472440945017 ) ) ;
#42984 = CARTESIAN_POINT ( 'NONE',  ( 0.7874015748031503170, -0.1870078740157480601, -0.3641732283464567677 ) ) ;
#42985 = CARTESIAN_POINT ( 'NONE',  ( 1.108923884514436686, -0.3162353388693409650, -0.4822834645669289433 ) ) ;
#42986 = EDGE_CURVE ( 'NONE', #11874, #37974, #44233, .T. ) ;
#42987 = CARTESIAN_POINT ( 'NONE',  ( 0.05905511811023681640, 0.07958543189024071263, -0.2665933059059888421 ) ) ;
#42988 = CARTESIAN_POINT ( 'NONE',  ( -0.2559055118110227234, -0.5400638737290844871, 0.3530559997133364547 ) ) ;
#42989 = CARTESIAN_POINT ( 'NONE',  ( 0.4855643044619428750, 0.05413385826771666132, 0.4176697321401328100 ) ) ;
#42990 = CARTESIAN_POINT ( 'NONE',  ( -0.7677165354330699465, -0.5400638737290845981, -0.3530559997133363437 ) ) ;
#42991 = CARTESIAN_POINT ( 'NONE',  ( -0.2230971128608915943, -0.3690944881889765550, -0.3153832671262227771 ) ) ;
#42992 = CARTESIAN_POINT ( 'NONE',  ( 0.7086614173228352742, -0.1870078740157480879, -0.4822834645669291653 ) ) ;
#42993 = CARTESIAN_POINT ( 'NONE',  ( 1.154855643044620184, -0.5023911411419708095, 0.1820866141732285504 ) ) ;
#42994 = CARTESIAN_POINT ( 'NONE',  ( -0.006561679790025524116, -0.05778040916215560624, -0.4822834645669293319 ) ) ;
#42995 =( BOUNDED_SURFACE ( )  B_SPLINE_SURFACE ( 1, 2, ( 
 ( #53949, #28287, #79662, #73335, #48056, #10189, #3453, #16512, #73758, #61523, #35026, #67022, #29120, #68665, #29934, #54788, #48464, #41343, #21978, #74165, #36261, #16093, #60690, #23212, #11004, #61930, #3869, #29528, #41738, #28705, #22807, #9766, #55191, #80898, #42155, #35437, #67850, #80079, #36663, #61102, #48882, #74582, #47640, #16927, #42567, #4273, #55598, #11837, #81724, #37490, #18956, #31165, #70724, #6329, #5098, #19373, #69889, #82943, #30765, #30347, #11422, #50110, #70300, #12652, #51337, #49702, #75807, #63165, #69073, #38313, #25261, #37077, #13078, #63988, #43373, #5503, #62765, #32002, #56016, #17744, #57661, #43782, #77041, #37899, #45023, #24, #56427, #24848, #63575, #82127, #24442, #18149, #38731, #25677, #75398, #69488, #50926, #4675, #18555, #57239, #56832, #5910, #82530, #50515, #24033, #76625, #44604, #76223, #31583, #44199, #12243, #21051, #71563, #13913, #47121, #78305, #15159, #59754, #58929, #1696, #19799, #34091, #1288, #2109, #64408, #58077, #443, #65686, #71145, #20637, #39570, #26098, #65260, #78727, #7596, #72810, #66087, #64827, #79146, #46289, #59339, #7166, #6743, #13487, #26527, #46711, #72403, #27774, #51759, #52181, #33270, #45448, #14752, #27354, #39143, #32415, #40406, #32837, #26937, #58506, #8423, #77461, #869, #53438, #20216, #21463, #14338, #77884, #45865, #52599, #71985, #39998, #8013, #33677, #53013, #29835, #10504, #28188, #60591, #61414, #74477, #54680, #10083, #66925, #42053, #15579, #2530, #34512, #29428, #55086, #47537, #74061, #28605, #53846, #80795, #47952, #73655, #23522, #80392, #74893, #36157, #35337, #3764, #79559, #61831, #61001, #4171, #40817, #60177, #21872, #67749, #73228, #66501, #8836, #41237, #34929, #22704, #15997, #29015, #2941, #48362, #9257, #54262, #41644, #55498, #42461, #67335, #3349, #79978, #22291, #16407, #23112, #9668, #35747, #48778, #81207, #16824, #68160, #49192, #30671, #75299, #11743, #56332, #50421, #24753, #31069, #62661, #75712, #4578, #31902, #82031, #12145, #24345, #42869, #76121, #51241, #50833, #18462, #82435, #50014, #17643, #37399, #18053, #44106, #69798, #56738, #5001, #43686, #30249, #57563, #69390, #37802, #63071, #68563, #63480, #17241, #76534, #5814, #5408, #10905, #31484, #57145, #82844, #83254, #18862, #43275, #25577, #25164, #44511, #68972, #36563, #23937, #70199, #12554, #38213, #63888, #62240, #6227, #55913, #81625, #49605, #11322, #36980, #59654, #27254, #32315, #26425, #343, #59239, #44922, #6643, #1599, #32736, #40308, #26839, #8326, #52913, #19693, #13811, #52497, #77361, #13391, #51657, #65988, #46609, #64309, #39044, #14235, #78627, #7494, #46188, #45350, #78206, #71047, #38631, #70619, #65581, #7915, #26000, #20537, #64728, #57978, #33576, #763, #52077, #2010, #33163, #27673, #72305, #71464, #39894, #7067, #14651, #39470, #33992, #76943, #12975, #58404, #71885, #77785, #19269, #20118, #45765, #65157, #58831, #1189, #20952, #47436, #62042, #60077, #8739, #54162, #69183, #56127, #28504, #73556, #66401, #47020, #15900, #36775, #73129, #2432, #49405, #49814, #11118, #15480, #28089, #75099, #75514, #62451, #4379, #36368, #66827, #53746, #47852, #9159, #30047, #55709, #67237, #41137, #79876, #40716, #11534, #34832, #17447, #60491, #79048, #81418, #5207, #4787, #10711, #2841, #72713, #22194, #68774, #41548, #37191, #81833, #79455, #62871, #23734, #43077, #21774, #21366, #30464, #24143, #17853, #43487, #53339, #15060, #34410, #6027, #11945, #38842, #51452, #37599, #13605, #64522, #69598, #63688, #63274, #13193, #82239, #43901, #6859, #69999, #77581, #64109, #45563, #32528, #56946, #51038, #6444, #31281, #50629, #5613, #19913, #560, #18259, #76334, #77155, #58192, #44717, #136, #82643, #32115, #24956, #75920, #24558, #19487, #45140, #18664, #57773, #44309, #12354, #70844, #38010, #31697, #39259, #70414, #64941, #26213, #25375, #51875, #57356, #71259, #76739, #30871, #56537, #50224, #83052, #25791, #19069, #12770, #38427, #52294, #1396, #72510, #65791, #78837, #27051, #14859, #14027, #45980, #8124, #21988, #8950, #33790, #27468, #20328, #985 ),
 ( #52710, #59454, #77999, #47649, #20750, #2221, #46400, #32951, #66200, #41350, #40933, #21163, #14452, #26640, #40103, #21570, #1806, #73344, #34625, #7711, #15692, #40521, #27887, #33378, #58617, #39684, #78422, #72921, #15273, #53958, #71676, #72093, #53126, #65376, #66613, #53547, #59042, #7281, #60289, #46819, #8538, #34205, #2639, #59868, #79255, #28296, #47232, #79670, #16935, #81733, #75003, #9774, #3877, #42575, #67441, #3463, #41746, #56025, #36671, #54377, #29129, #4281, #17350, #80907, #36269, #35446, #68277, #61111, #28714, #60699, #55607, #81318, #73766, #10613, #54796, #80087, #23631, #74174, #16520, #49713, #23220, #17753, #62347, #61532, #29943, #22407, #4685, #29536, #30356, #67031, #3048, #48064, #61938, #16101, #9363, #35034, #80499, #22815, #48890, #42165, #55199, #48472, #74591, #67859, #10197, #35866, #24042, #68673, #49302, #42978, #11013, #75409, #63586, #25686, #63174, #50119, #26108, #77050, #82138, #76231, #75817, #51347, #11432, #56435, #19383, #82540, #6752, #76634, #58087, #45035, #69497, #5921, #18965, #43791, #5512, #18160, #32424, #13088, #30774, #31177, #63997, #70734, #57248, #12664, #11846, #44614, #37499, #5107, #37087, #32011, #57671, #56842, #70309, #24857, #24453, #33, #50525, #18565, #51769, #82952, #77472, #38740, #37909, #6338, #44208, #64417, #31593, #452, #43382, #62773, #69898, #38324, #12252, #69084, #25270, #50937, #13923, #1706, #78316, #8024, #39580, #27362, #26538, #58515, #20646, #34521, #21472, #46300, #40007, #32846, #13496, #65694, #2118, #65269, #52191, #14760, #15171, #59764, #53022, #78736, #33279, #77895, #14347, #58940, #21059, #46719, #33687, #7605, #71994, #7175, #60188, #1298, #40416, #26947, #45458, #72411, #53856, #53447, #59348, #52609, #39152, #66097, #34102, #8433, #2539, #47130, #20225, #28197, #27784, #79155, #45874, #71155, #71572, #72821, #40827, #66512, #8845, #64837, #19809, #878, #60601, #4182, #16835, #2950, #49201, #79568, #73239, #15588, #80806, #28615, #21884, #30258, #41247, #73665, #61426, #54692, #67759, #16006, #3775, #54273, #34938, #80401, #10914, #81216, #22714, #16417, #9267, #66934, #42064, #61840, #41653, #79989, #74488, #74902, #36167, #29438, #55098, #9677, #22301, #74072, #35348, #23122, #48790, #10094, #67344, #48372, #47962, #36572, #61010, #42470, #3361, #47548, #68172, #29025, #29844, #35759, #10514, #55508, #23532, #17251, #42879, #62250, #68573, #4587, #70629, #37813, #50844, #56342, #81636, #62671, #18063, #38223, #63899, #19281, #17654, #43696, #31081, #36991, #6236, #76544, #5011, #38641, #31912, #11331, #5419, #30681, #57573, #23946, #68983, #83265, #11753, #44932, #5823, #12986, #25588, #82042, #76131, #31495, #24356, #75723, #50025, #64319, #51251, #43285, #69401, #18872, #76953, #69808, #25175, #37409, #57155, #63081, #56748, #49614, #44521, #70209, #82447, #82855, #24763, #50431, #12565, #18473, #44116, #6653, #12157, #55922, #75308, #63489, #39905, #45361, #20962, #65169, #65593, #71057, #78217, #7926, #46621, #1609, #13401, #774, #14247, #59252, #72316, #57988, #27265, #32327, #26436, #39055, #7505, #13823, #39482, #14663, #40320, #20549, #46201, #33587, #71896, #32748, #33174, #65999, #52509, #52925, #58842, #34004, #353, #8338, #59666, #26010, #71475, #64739, #78639, #7077, #51668, #77371, #19703, #58415, #52087, #77797, #20129, #45777, #1200, #26850, #44789, #18336, #11611, #30943, #6930, #5281, #38083, #32187, #49887, #77226, #45214, #18736, #64594, #69673, #44378, #63348, #82713, #25446, #70070, #43976, #75588, #19139, #38501, #64183, #70915, #5683, #19555, #32601, #56610, #13264, #43563, #31352, #69264, #37671, #58264, #37270, #57018, #38914, #6098, #24216, #57433, #76405, #82310, #12425, #17927, #12016, #76808, #31772, #6517, #24630, #63757, #62946, #50296, #210, #75994, #57843, #83126, #25033, #50706, #51111, #70485, #12842, #25863, #51523, #2292, #59106, #20814, #13676, #77650, #46469, #66264, #20399, #7349, #78906, #79319, #40583, #33855, #14518, #53193, #72163, #41004, #628, #47299, #72988, #66687, #14098, #71328, #8188, #65014 ) ),
 .UNSPECIFIED., .F., .F., .F. ) 
 B_SPLINE_SURFACE_WITH_KNOTS ( ( 2, 2 ),
 ( 3, 2, 2, 2, 2, 2, 2, 2, 2, 2, 2, 2, 2, 2, 2, 2, 2, 2, 2, 2, 2, 2, 2, 2, 2, 2, 2, 2, 2, 2, 2, 2, 2, 2, 2, 2, 2, 2, 2, 2, 2, 2, 2, 2, 2, 2, 2, 2, 2, 2, 2, 2, 2, 2, 2, 2, 2, 2, 2, 2, 2, 2, 2, 2, 2, 2, 2, 2, 2, 2, 2, 2, 2, 2, 2, 2, 2, 2, 2, 2, 2, 2, 2, 2, 2, 2, 2, 2, 2, 2, 2, 2, 2, 2, 2, 2, 2, 2, 2, 2, 2, 2, 2, 2, 2, 2, 2, 2, 2, 2, 2, 2, 2, 2, 2, 2, 2, 2, 2, 2, 2, 2, 2, 2, 2, 2, 2, 2, 2, 2, 2, 2, 2, 2, 2, 2, 2, 2, 2, 2, 2, 2, 2, 2, 2, 2, 2, 2, 2, 2, 2, 2, 2, 2, 2, 2, 2, 2, 2, 2, 2, 2, 2, 2, 2, 2, 2, 2, 2, 2, 2, 2, 2, 2, 2, 2, 2, 2, 2, 2, 2, 2, 2, 2, 2, 2, 2, 2, 2, 2, 2, 2, 2, 2, 2, 2, 2, 2, 2, 2, 2, 2, 2, 2, 2, 2, 2, 2, 2, 2, 2, 2, 2, 2, 2, 2, 2, 2, 2, 2, 2, 2, 2, 2, 2, 2, 2, 2, 2, 2, 2, 2, 2, 2, 2, 2, 2, 2, 2, 2, 2, 2, 2, 2, 2, 2, 2, 2, 2, 2, 2, 2, 2, 2, 2, 3 ),
 ( 0.000000000000000000, 1.000000000000000000 ),
 ( 0.000000000000000000, 0.003787878787878787984, 0.007575757575757575968, 0.01136363636363636395, 0.01515151515151515194, 0.01893939393939393992, 0.02272727272727272790, 0.02651515151515151589, 0.03030303030303030387, 0.03409090909090908839, 0.03787878787878787984, 0.04166666666666666435, 0.04545454545454545581, 0.04924242424242424032, 0.05303030303030303177, 0.05681818181818181629, 0.06060606060606060774, 0.06439393939393939226, 0.06818181818181817677, 0.07196969696969697516, 0.07575757575757575968, 0.07954545454545454419, 0.08333333333333332871, 0.08712121212121212710, 0.09090909090909091161, 0.09469696969696969613, 0.09848484848484848064, 0.1022727272727272790, 0.1060606060606060635, 0.1098484848484848481, 0.1136363636363636326, 0.1174242424242424310, 0.1212121212121212155, 0.1250000000000000000, 0.1287878787878787845, 0.1325757575757575690, 0.1363636363636363535, 0.1401515151515151381, 0.1439393939393939503, 0.1477272727272727348, 0.1515151515151515194, 0.1553030303030303039, 0.1590909090909090884, 0.1628787878787878729, 0.1666666666666666574, 0.1704545454545454419, 0.1742424242424242542, 0.1780303030303030387, 0.1818181818181818232, 0.1856060606060606077, 0.1893939393939393923, 0.1931818181818181768, 0.1969696969696969613, 0.2007575757575757458, 0.2045454545454545581, 0.2083333333333333426, 0.2121212121212121271, 0.2159090909090909116, 0.2196969696969696961, 0.2234848484848484806, 0.2272727272727272652, 0.2310606060606060497, 0.2348484848484848619, 0.2386363636363636465, 0.2424242424242424310, 0.2462121212121212155, 0.2500000000000000000, 0.2537878787878787845, 0.2575757575757575690, 0.2613636363636363535, 0.2651515151515151381, 0.2689393939393939226, 0.2727272727272727071, 0.2765151515151514916, 0.2803030303030302761, 0.2840909090909091161, 0.2878787878787879007, 0.2916666666666666852, 0.2954545454545454697, 0.2992424242424242542, 0.3030303030303030387, 0.3068181818181818232, 0.3106060606060606077, 0.3143939393939393923, 0.3181818181818181768, 0.3219696969696969613, 0.3257575757575757458, 0.3295454545454545303, 0.3333333333333333148, 0.3371212121212120993, 0.3409090909090908839, 0.3446969696969697239, 0.3484848484848485084, 0.3522727272727272929, 0.3560606060606060774, 0.3598484848484848619, 0.3636363636363636465, 0.3674242424242424310, 0.3712121212121212155, 0.3750000000000000000, 0.3787878787878787845, 0.3825757575757575690, 0.3863636363636363535, 0.3901515151515151381, 0.3939393939393939226, 0.3977272727272727071, 0.4015151515151514916, 0.4053030303030302761, 0.4090909090909091161, 0.4128787878787879007, 0.4166666666666666852, 0.4204545454545454697, 0.4242424242424242542, 0.4280303030303030387, 0.4318181818181818232, 0.4356060606060606077, 0.4393939393939393923, 0.4431818181818181768, 0.4469696969696969613, 0.4507575757575757458, 0.4545454545454545303, 0.4583333333333333148, 0.4621212121212120993, 0.4659090909090908839, 0.4696969696969697239, 0.4734848484848485084, 0.4772727272727272929, 0.4810606060606060774, 0.4848484848484848619, 0.4886363636363636465, 0.4924242424242424310, 0.4962121212121212155, 0.5000000000000000000, 0.5037878787878787845, 0.5075757575757575690, 0.5113636363636363535, 0.5151515151515151381, 0.5189393939393939226, 0.5227272727272727071, 0.5265151515151514916, 0.5303030303030302761, 0.5340909090909090606, 0.5378787878787878451, 0.5416666666666666297, 0.5454545454545454142, 0.5492424242424241987, 0.5530303030303029832, 0.5568181818181817677, 0.5606060606060605522, 0.5643939393939394478, 0.5681818181818182323, 0.5719696969696970168, 0.5757575757575758013, 0.5795454545454545858, 0.5833333333333333703, 0.5871212121212121549, 0.5909090909090909394, 0.5946969696969697239, 0.5984848484848485084, 0.6022727272727272929, 0.6060606060606060774, 0.6098484848484848619, 0.6136363636363636465, 0.6174242424242424310, 0.6212121212121212155, 0.6250000000000000000, 0.6287878787878787845, 0.6325757575757575690, 0.6363636363636363535, 0.6401515151515151381, 0.6439393939393939226, 0.6477272727272727071, 0.6515151515151514916, 0.6553030303030302761, 0.6590909090909090606, 0.6628787878787878451, 0.6666666666666666297, 0.6704545454545454142, 0.6742424242424241987, 0.6780303030303029832, 0.6818181818181817677, 0.6856060606060605522, 0.6893939393939394478, 0.6931818181818182323, 0.6969696969696970168, 0.7007575757575758013, 0.7045454545454545858, 0.7083333333333333703, 0.7121212121212121549, 0.7159090909090909394, 0.7196969696969697239, 0.7234848484848485084, 0.7272727272727272929, 0.7310606060606060774, 0.7348484848484848619, 0.7386363636363636465, 0.7424242424242424310, 0.7462121212121212155, 0.7500000000000000000, 0.7537878787878787845, 0.7575757575757575690, 0.7613636363636363535, 0.7651515151515151381, 0.7689393939393939226, 0.7727272727272727071, 0.7765151515151514916, 0.7803030303030302761, 0.7840909090909090606, 0.7878787878787878451, 0.7916666666666666297, 0.7954545454545454142, 0.7992424242424241987, 0.8030303030303029832, 0.8068181818181817677, 0.8106060606060605522, 0.8143939393939394478, 0.8181818181818182323, 0.8219696969696970168, 0.8257575757575758013, 0.8295454545454545858, 0.8333333333333333703, 0.8371212121212121549, 0.8409090909090909394, 0.8446969696969697239, 0.8484848484848485084, 0.8522727272727272929, 0.8560606060606060774, 0.8598484848484848619, 0.8636363636363636465, 0.8674242424242424310, 0.8712121212121212155, 0.8750000000000000000, 0.8787878787878787845, 0.8825757575757575690, 0.8863636363636363535, 0.8901515151515151381, 0.8939393939393939226, 0.8977272727272727071, 0.9015151515151514916, 0.9053030303030302761, 0.9090909090909090606, 0.9128787878787878451, 0.9166666666666666297, 0.9204545454545454142, 0.9242424242424241987, 0.9280303030303029832, 0.9318181818181817677, 0.9356060606060605522, 0.9393939393939394478, 0.9431818181818182323, 0.9469696969696970168, 0.9507575757575758013, 0.9545454545454545858, 0.9583333333333333703, 0.9621212121212121549, 0.9659090909090909394 ),
 .UNSPECIFIED. ) 
 GEOMETRIC_REPRESENTATION_ITEM ( )  RATIONAL_B_SPLINE_SURFACE ( (
 ( 1.000000000000000000, 0.9659258262890683122, 1.000000000000000000, 0.9659258262890683122, 1.000000000000000000, 0.9659258262890683122, 1.000000000000000000, 0.9659258262890683122, 1.000000000000000000, 0.9659258262890683122, 1.000000000000000000, 0.9659258262890683122, 1.000000000000000000, 0.9659258262890683122, 1.000000000000000000, 0.9659258262890683122, 1.000000000000000000, 0.9659258262890683122, 1.000000000000000000, 0.9659258262890683122, 1.000000000000000000, 0.9659258262890683122, 1.000000000000000000, 0.9659258262890683122, 1.000000000000000000, 0.9659258262890683122, 1.000000000000000000, 0.9659258262890683122, 1.000000000000000000, 0.9659258262890683122, 1.000000000000000000, 0.9659258262890683122, 1.000000000000000000, 0.9659258262890683122, 1.000000000000000000, 0.9659258262890683122, 1.000000000000000000, 0.9659258262890683122, 1.000000000000000000, 0.9659258262890683122, 1.000000000000000000, 0.9659258262890683122, 1.000000000000000000, 0.9659258262890683122, 1.000000000000000000, 0.9659258262890683122, 1.000000000000000000, 0.9659258262890683122, 1.000000000000000000, 0.9659258262890683122, 1.000000000000000000, 0.9659258262890683122, 1.000000000000000000, 0.9659258262890683122, 1.000000000000000000, 0.9659258262890683122, 1.000000000000000000, 0.9659258262890683122, 1.000000000000000000, 0.9659258262890683122, 1.000000000000000000, 0.9659258262890683122, 1.000000000000000000, 0.9659258262890683122, 1.000000000000000000, 0.9659258262890683122, 1.000000000000000000, 0.9659258262890683122, 1.000000000000000000, 0.9659258262890683122, 1.000000000000000000, 0.9659258262890683122, 1.000000000000000000, 0.9659258262890683122, 1.000000000000000000, 0.9659258262890683122, 1.000000000000000000, 0.9659258262890683122, 1.000000000000000000, 0.9659258262890683122, 1.000000000000000000, 0.9659258262890683122, 1.000000000000000000, 0.9659258262890683122, 1.000000000000000000, 0.9659258262890683122, 1.000000000000000000, 0.9659258262890683122, 1.000000000000000000, 0.9659258262890683122, 1.000000000000000000, 0.9659258262890683122, 1.000000000000000000, 0.9659258262890683122, 1.000000000000000000, 0.9659258262890683122, 1.000000000000000000, 0.9659258262890683122, 1.000000000000000000, 0.9659258262890683122, 1.000000000000000000, 0.9659258262890683122, 1.000000000000000000, 0.9659258262890683122, 1.000000000000000000, 0.9659258262890683122, 1.000000000000000000, 0.9659258262890683122, 1.000000000000000000, 0.9659258262890683122, 1.000000000000000000, 0.9659258262890683122, 1.000000000000000000, 0.9659258262890683122, 1.000000000000000000, 0.9659258262890683122, 1.000000000000000000, 0.9659258262890683122, 1.000000000000000000, 0.9659258262890683122, 1.000000000000000000, 0.9659258262890683122, 1.000000000000000000, 0.9659258262890683122, 1.000000000000000000, 0.9659258262890683122, 1.000000000000000000, 0.9659258262890683122, 1.000000000000000000, 0.9659258262890683122, 1.000000000000000000, 0.9659258262890683122, 1.000000000000000000, 0.9659258262890683122, 1.000000000000000000, 0.9659258262890683122, 1.000000000000000000, 0.9659258262890683122, 1.000000000000000000, 0.9659258262890683122, 1.000000000000000000, 0.9659258262890683122, 1.000000000000000000, 0.9659258262890683122, 1.000000000000000000, 0.9659258262890683122, 1.000000000000000000, 0.9659258262890683122, 1.000000000000000000, 0.9659258262890683122, 1.000000000000000000, 0.9659258262890683122, 1.000000000000000000, 0.9659258262890683122, 1.000000000000000000, 0.9659258262890683122, 1.000000000000000000, 0.9659258262890683122, 1.000000000000000000, 0.9659258262890683122, 1.000000000000000000, 0.9659258262890683122, 1.000000000000000000, 0.9659258262890683122, 1.000000000000000000, 0.9659258262890683122, 1.000000000000000000, 0.9659258262890683122, 1.000000000000000000, 0.9659258262890683122, 1.000000000000000000, 0.9659258262890683122, 1.000000000000000000, 0.9659258262890683122, 1.000000000000000000, 0.9659258262890683122, 1.000000000000000000, 0.9659258262890683122, 1.000000000000000000, 0.9659258262890683122, 1.000000000000000000, 0.9659258262890683122, 1.000000000000000000, 0.9659258262890683122, 1.000000000000000000, 0.9659258262890683122, 1.000000000000000000, 0.9659258262890683122, 1.000000000000000000, 0.9659258262890683122, 1.000000000000000000, 0.9659258262890683122, 1.000000000000000000, 0.9659258262890683122, 1.000000000000000000, 0.9659258262890683122, 1.000000000000000000, 0.9659258262890683122, 1.000000000000000000, 0.9659258262890683122, 1.000000000000000000, 0.9659258262890683122, 1.000000000000000000, 0.9659258262890683122, 1.000000000000000000, 0.9659258262890683122, 1.000000000000000000, 0.9659258262890683122, 1.000000000000000000, 0.9659258262890683122, 1.000000000000000000, 0.9659258262890683122, 1.000000000000000000, 0.9659258262890683122, 1.000000000000000000, 0.9659258262890683122, 1.000000000000000000, 0.9659258262890683122, 1.000000000000000000, 0.9659258262890683122, 1.000000000000000000, 0.9659258262890683122, 1.000000000000000000, 0.9659258262890683122, 1.000000000000000000, 0.9659258262890683122, 1.000000000000000000, 0.9659258262890683122, 1.000000000000000000, 0.9659258262890683122, 1.000000000000000000, 0.9659258262890683122, 1.000000000000000000, 0.9659258262890683122, 1.000000000000000000, 0.9659258262890683122, 1.000000000000000000, 0.9659258262890683122, 1.000000000000000000, 0.9659258262890683122, 1.000000000000000000, 0.9659258262890683122, 1.000000000000000000, 0.9659258262890683122, 1.000000000000000000, 0.9659258262890683122, 1.000000000000000000, 0.9659258262890683122, 1.000000000000000000, 0.9659258262890683122, 1.000000000000000000, 0.9659258262890683122, 1.000000000000000000, 0.9659258262890683122, 1.000000000000000000, 0.9659258262890683122, 1.000000000000000000, 0.9659258262890683122, 1.000000000000000000, 0.9659258262890683122, 1.000000000000000000, 0.9659258262890683122, 1.000000000000000000, 0.9659258262890683122, 1.000000000000000000, 0.9659258262890683122, 1.000000000000000000, 0.9659258262890683122, 1.000000000000000000, 0.9659258262890683122, 1.000000000000000000, 0.9659258262890683122, 1.000000000000000000, 0.9659258262890683122, 1.000000000000000000, 0.9659258262890683122, 1.000000000000000000, 0.9659258262890683122, 1.000000000000000000, 0.9659258262890683122, 1.000000000000000000, 0.9659258262890683122, 1.000000000000000000, 0.9659258262890683122, 1.000000000000000000, 0.9659258262890683122, 1.000000000000000000, 0.9659258262890683122, 1.000000000000000000, 0.9659258262890683122, 1.000000000000000000, 0.9659258262890683122, 1.000000000000000000, 0.9659258262890683122, 1.000000000000000000, 0.9659258262890683122, 1.000000000000000000, 0.9659258262890683122, 1.000000000000000000, 0.9659258262890683122, 1.000000000000000000, 0.9659258262890683122, 1.000000000000000000, 0.9659258262890683122, 1.000000000000000000, 0.9659258262890683122, 1.000000000000000000, 0.9659258262890683122, 1.000000000000000000, 0.9659258262890683122, 1.000000000000000000, 0.9659258262890683122, 1.000000000000000000, 0.9659258262890683122, 1.000000000000000000, 0.9659258262890683122, 1.000000000000000000, 0.9659258262890683122, 1.000000000000000000, 0.9659258262890683122, 1.000000000000000000, 0.9659258262890683122, 1.000000000000000000, 0.9659258262890683122, 1.000000000000000000, 0.9659258262890683122, 1.000000000000000000, 0.9659258262890683122, 1.000000000000000000, 0.9659258262890683122, 1.000000000000000000, 0.9659258262890683122, 1.000000000000000000, 0.9659258262890683122, 1.000000000000000000, 0.9659258262890683122, 1.000000000000000000, 0.9659258262890683122, 1.000000000000000000, 0.9659258262890683122, 1.000000000000000000, 0.9659258262890683122, 1.000000000000000000, 0.9659258262890683122, 1.000000000000000000, 0.9659258262890683122, 1.000000000000000000, 0.9659258262890683122, 1.000000000000000000, 0.9659258262890683122, 1.000000000000000000, 0.9659258262890683122, 1.000000000000000000, 0.9659258262890683122, 1.000000000000000000, 0.9659258262890683122, 1.000000000000000000, 0.9659258262890683122, 1.000000000000000000, 0.9659258262890683122, 1.000000000000000000, 0.9659258262890683122, 1.000000000000000000, 0.9659258262890683122, 1.000000000000000000, 0.9659258262890683122, 1.000000000000000000, 0.9659258262890683122, 1.000000000000000000, 0.9659258262890683122, 1.000000000000000000, 0.9659258262890683122, 1.000000000000000000, 0.9659258262890683122, 1.000000000000000000, 0.9659258262890683122, 1.000000000000000000, 0.9659258262890683122, 1.000000000000000000, 0.9659258262890683122, 1.000000000000000000, 0.9659258262890683122, 1.000000000000000000, 0.9659258262890683122, 1.000000000000000000, 0.9659258262890683122, 1.000000000000000000, 0.9659258262890683122, 1.000000000000000000, 0.9659258262890683122, 1.000000000000000000, 0.9659258262890683122, 1.000000000000000000, 0.9659258262890683122, 1.000000000000000000, 0.9659258262890683122, 1.000000000000000000, 0.9659258262890683122, 1.000000000000000000, 0.9659258262890683122, 1.000000000000000000, 0.9659258262890683122, 1.000000000000000000, 0.9659258262890683122, 1.000000000000000000, 0.9659258262890683122, 1.000000000000000000, 0.9659258262890683122, 1.000000000000000000, 0.9659258262890683122, 1.000000000000000000, 0.9659258262890683122, 1.000000000000000000, 0.9659258262890683122, 1.000000000000000000, 0.9659258262890683122, 1.000000000000000000, 0.9659258262890683122, 1.000000000000000000, 0.9659258262890683122, 1.000000000000000000, 0.9659258262890683122, 1.000000000000000000, 0.9659258262890683122, 1.000000000000000000, 0.9659258262890683122, 1.000000000000000000, 0.9659258262890683122, 1.000000000000000000, 0.9659258262890683122, 1.000000000000000000, 0.9659258262890683122, 1.000000000000000000, 0.9659258262890683122, 1.000000000000000000, 0.9659258262890683122, 1.000000000000000000, 0.9659258262890683122, 1.000000000000000000, 0.9659258262890683122, 1.000000000000000000, 0.9659258262890683122, 1.000000000000000000, 0.9659258262890683122, 1.000000000000000000, 0.9659258262890683122, 1.000000000000000000, 0.9659258262890683122, 1.000000000000000000, 0.9659258262890683122, 1.000000000000000000, 0.9659258262890683122, 1.000000000000000000, 0.9659258262890683122, 1.000000000000000000, 0.9659258262890683122, 1.000000000000000000, 0.9659258262890683122, 1.000000000000000000, 0.9659258262890683122, 1.000000000000000000, 0.9659258262890683122, 1.000000000000000000, 0.9659258262890683122, 1.000000000000000000, 0.9659258262890683122, 1.000000000000000000, 0.9659258262890683122, 1.000000000000000000, 0.9659258262890683122, 1.000000000000000000, 0.9659258262890683122, 1.000000000000000000, 0.9659258262890683122, 1.000000000000000000, 0.9659258262890683122, 1.000000000000000000, 0.9659258262890683122, 1.000000000000000000, 0.9659258262890683122, 1.000000000000000000, 0.9659258262890683122, 1.000000000000000000, 0.9659258262890683122, 1.000000000000000000, 0.9659258262890683122, 1.000000000000000000, 0.9659258262890683122, 1.000000000000000000, 0.9659258262890683122, 1.000000000000000000, 0.9659258262890683122, 1.000000000000000000, 0.9659258262890683122, 1.000000000000000000, 0.9659258262890683122, 1.000000000000000000, 0.9659258262890683122, 1.000000000000000000, 0.9659258262890683122, 1.000000000000000000, 0.9659258262890683122, 1.000000000000000000, 0.9659258262890683122, 1.000000000000000000, 0.9659258262890683122, 1.000000000000000000, 0.9659258262890683122, 1.000000000000000000, 0.9659258262890683122, 1.000000000000000000),
 ( 1.000000000000000000, 0.9659258262890683122, 1.000000000000000000, 0.9659258262890683122, 1.000000000000000000, 0.9659258262890683122, 1.000000000000000000, 0.9659258262890683122, 1.000000000000000000, 0.9659258262890683122, 1.000000000000000000, 0.9659258262890683122, 1.000000000000000000, 0.9659258262890683122, 1.000000000000000000, 0.9659258262890683122, 1.000000000000000000, 0.9659258262890683122, 1.000000000000000000, 0.9659258262890683122, 1.000000000000000000, 0.9659258262890683122, 1.000000000000000000, 0.9659258262890683122, 1.000000000000000000, 0.9659258262890683122, 1.000000000000000000, 0.9659258262890683122, 1.000000000000000000, 0.9659258262890683122, 1.000000000000000000, 0.9659258262890683122, 1.000000000000000000, 0.9659258262890683122, 1.000000000000000000, 0.9659258262890683122, 1.000000000000000000, 0.9659258262890683122, 1.000000000000000000, 0.9659258262890683122, 1.000000000000000000, 0.9659258262890683122, 1.000000000000000000, 0.9659258262890683122, 1.000000000000000000, 0.9659258262890683122, 1.000000000000000000, 0.9659258262890683122, 1.000000000000000000, 0.9659258262890683122, 1.000000000000000000, 0.9659258262890683122, 1.000000000000000000, 0.9659258262890683122, 1.000000000000000000, 0.9659258262890683122, 1.000000000000000000, 0.9659258262890683122, 1.000000000000000000, 0.9659258262890683122, 1.000000000000000000, 0.9659258262890683122, 1.000000000000000000, 0.9659258262890683122, 1.000000000000000000, 0.9659258262890683122, 1.000000000000000000, 0.9659258262890683122, 1.000000000000000000, 0.9659258262890683122, 1.000000000000000000, 0.9659258262890683122, 1.000000000000000000, 0.9659258262890683122, 1.000000000000000000, 0.9659258262890683122, 1.000000000000000000, 0.9659258262890683122, 1.000000000000000000, 0.9659258262890683122, 1.000000000000000000, 0.9659258262890683122, 1.000000000000000000, 0.9659258262890683122, 1.000000000000000000, 0.9659258262890683122, 1.000000000000000000, 0.9659258262890683122, 1.000000000000000000, 0.9659258262890683122, 1.000000000000000000, 0.9659258262890683122, 1.000000000000000000, 0.9659258262890683122, 1.000000000000000000, 0.9659258262890683122, 1.000000000000000000, 0.9659258262890683122, 1.000000000000000000, 0.9659258262890683122, 1.000000000000000000, 0.9659258262890683122, 1.000000000000000000, 0.9659258262890683122, 1.000000000000000000, 0.9659258262890683122, 1.000000000000000000, 0.9659258262890683122, 1.000000000000000000, 0.9659258262890683122, 1.000000000000000000, 0.9659258262890683122, 1.000000000000000000, 0.9659258262890683122, 1.000000000000000000, 0.9659258262890683122, 1.000000000000000000, 0.9659258262890683122, 1.000000000000000000, 0.9659258262890683122, 1.000000000000000000, 0.9659258262890683122, 1.000000000000000000, 0.9659258262890683122, 1.000000000000000000, 0.9659258262890683122, 1.000000000000000000, 0.9659258262890683122, 1.000000000000000000, 0.9659258262890683122, 1.000000000000000000, 0.9659258262890683122, 1.000000000000000000, 0.9659258262890683122, 1.000000000000000000, 0.9659258262890683122, 1.000000000000000000, 0.9659258262890683122, 1.000000000000000000, 0.9659258262890683122, 1.000000000000000000, 0.9659258262890683122, 1.000000000000000000, 0.9659258262890683122, 1.000000000000000000, 0.9659258262890683122, 1.000000000000000000, 0.9659258262890683122, 1.000000000000000000, 0.9659258262890683122, 1.000000000000000000, 0.9659258262890683122, 1.000000000000000000, 0.9659258262890683122, 1.000000000000000000, 0.9659258262890683122, 1.000000000000000000, 0.9659258262890683122, 1.000000000000000000, 0.9659258262890683122, 1.000000000000000000, 0.9659258262890683122, 1.000000000000000000, 0.9659258262890683122, 1.000000000000000000, 0.9659258262890683122, 1.000000000000000000, 0.9659258262890683122, 1.000000000000000000, 0.9659258262890683122, 1.000000000000000000, 0.9659258262890683122, 1.000000000000000000, 0.9659258262890683122, 1.000000000000000000, 0.9659258262890683122, 1.000000000000000000, 0.9659258262890683122, 1.000000000000000000, 0.9659258262890683122, 1.000000000000000000, 0.9659258262890683122, 1.000000000000000000, 0.9659258262890683122, 1.000000000000000000, 0.9659258262890683122, 1.000000000000000000, 0.9659258262890683122, 1.000000000000000000, 0.9659258262890683122, 1.000000000000000000, 0.9659258262890683122, 1.000000000000000000, 0.9659258262890683122, 1.000000000000000000, 0.9659258262890683122, 1.000000000000000000, 0.9659258262890683122, 1.000000000000000000, 0.9659258262890683122, 1.000000000000000000, 0.9659258262890683122, 1.000000000000000000, 0.9659258262890683122, 1.000000000000000000, 0.9659258262890683122, 1.000000000000000000, 0.9659258262890683122, 1.000000000000000000, 0.9659258262890683122, 1.000000000000000000, 0.9659258262890683122, 1.000000000000000000, 0.9659258262890683122, 1.000000000000000000, 0.9659258262890683122, 1.000000000000000000, 0.9659258262890683122, 1.000000000000000000, 0.9659258262890683122, 1.000000000000000000, 0.9659258262890683122, 1.000000000000000000, 0.9659258262890683122, 1.000000000000000000, 0.9659258262890683122, 1.000000000000000000, 0.9659258262890683122, 1.000000000000000000, 0.9659258262890683122, 1.000000000000000000, 0.9659258262890683122, 1.000000000000000000, 0.9659258262890683122, 1.000000000000000000, 0.9659258262890683122, 1.000000000000000000, 0.9659258262890683122, 1.000000000000000000, 0.9659258262890683122, 1.000000000000000000, 0.9659258262890683122, 1.000000000000000000, 0.9659258262890683122, 1.000000000000000000, 0.9659258262890683122, 1.000000000000000000, 0.9659258262890683122, 1.000000000000000000, 0.9659258262890683122, 1.000000000000000000, 0.9659258262890683122, 1.000000000000000000, 0.9659258262890683122, 1.000000000000000000, 0.9659258262890683122, 1.000000000000000000, 0.9659258262890683122, 1.000000000000000000, 0.9659258262890683122, 1.000000000000000000, 0.9659258262890683122, 1.000000000000000000, 0.9659258262890683122, 1.000000000000000000, 0.9659258262890683122, 1.000000000000000000, 0.9659258262890683122, 1.000000000000000000, 0.9659258262890683122, 1.000000000000000000, 0.9659258262890683122, 1.000000000000000000, 0.9659258262890683122, 1.000000000000000000, 0.9659258262890683122, 1.000000000000000000, 0.9659258262890683122, 1.000000000000000000, 0.9659258262890683122, 1.000000000000000000, 0.9659258262890683122, 1.000000000000000000, 0.9659258262890683122, 1.000000000000000000, 0.9659258262890683122, 1.000000000000000000, 0.9659258262890683122, 1.000000000000000000, 0.9659258262890683122, 1.000000000000000000, 0.9659258262890683122, 1.000000000000000000, 0.9659258262890683122, 1.000000000000000000, 0.9659258262890683122, 1.000000000000000000, 0.9659258262890683122, 1.000000000000000000, 0.9659258262890683122, 1.000000000000000000, 0.9659258262890683122, 1.000000000000000000, 0.9659258262890683122, 1.000000000000000000, 0.9659258262890683122, 1.000000000000000000, 0.9659258262890683122, 1.000000000000000000, 0.9659258262890683122, 1.000000000000000000, 0.9659258262890683122, 1.000000000000000000, 0.9659258262890683122, 1.000000000000000000, 0.9659258262890683122, 1.000000000000000000, 0.9659258262890683122, 1.000000000000000000, 0.9659258262890683122, 1.000000000000000000, 0.9659258262890683122, 1.000000000000000000, 0.9659258262890683122, 1.000000000000000000, 0.9659258262890683122, 1.000000000000000000, 0.9659258262890683122, 1.000000000000000000, 0.9659258262890683122, 1.000000000000000000, 0.9659258262890683122, 1.000000000000000000, 0.9659258262890683122, 1.000000000000000000, 0.9659258262890683122, 1.000000000000000000, 0.9659258262890683122, 1.000000000000000000, 0.9659258262890683122, 1.000000000000000000, 0.9659258262890683122, 1.000000000000000000, 0.9659258262890683122, 1.000000000000000000, 0.9659258262890683122, 1.000000000000000000, 0.9659258262890683122, 1.000000000000000000, 0.9659258262890683122, 1.000000000000000000, 0.9659258262890683122, 1.000000000000000000, 0.9659258262890683122, 1.000000000000000000, 0.9659258262890683122, 1.000000000000000000, 0.9659258262890683122, 1.000000000000000000, 0.9659258262890683122, 1.000000000000000000, 0.9659258262890683122, 1.000000000000000000, 0.9659258262890683122, 1.000000000000000000, 0.9659258262890683122, 1.000000000000000000, 0.9659258262890683122, 1.000000000000000000, 0.9659258262890683122, 1.000000000000000000, 0.9659258262890683122, 1.000000000000000000, 0.9659258262890683122, 1.000000000000000000, 0.9659258262890683122, 1.000000000000000000, 0.9659258262890683122, 1.000000000000000000, 0.9659258262890683122, 1.000000000000000000, 0.9659258262890683122, 1.000000000000000000, 0.9659258262890683122, 1.000000000000000000, 0.9659258262890683122, 1.000000000000000000, 0.9659258262890683122, 1.000000000000000000, 0.9659258262890683122, 1.000000000000000000, 0.9659258262890683122, 1.000000000000000000, 0.9659258262890683122, 1.000000000000000000, 0.9659258262890683122, 1.000000000000000000, 0.9659258262890683122, 1.000000000000000000, 0.9659258262890683122, 1.000000000000000000, 0.9659258262890683122, 1.000000000000000000, 0.9659258262890683122, 1.000000000000000000, 0.9659258262890683122, 1.000000000000000000, 0.9659258262890683122, 1.000000000000000000, 0.9659258262890683122, 1.000000000000000000, 0.9659258262890683122, 1.000000000000000000, 0.9659258262890683122, 1.000000000000000000, 0.9659258262890683122, 1.000000000000000000, 0.9659258262890683122, 1.000000000000000000, 0.9659258262890683122, 1.000000000000000000, 0.9659258262890683122, 1.000000000000000000, 0.9659258262890683122, 1.000000000000000000, 0.9659258262890683122, 1.000000000000000000, 0.9659258262890683122, 1.000000000000000000, 0.9659258262890683122, 1.000000000000000000, 0.9659258262890683122, 1.000000000000000000, 0.9659258262890683122, 1.000000000000000000, 0.9659258262890683122, 1.000000000000000000, 0.9659258262890683122, 1.000000000000000000, 0.9659258262890683122, 1.000000000000000000, 0.9659258262890683122, 1.000000000000000000, 0.9659258262890683122, 1.000000000000000000, 0.9659258262890683122, 1.000000000000000000, 0.9659258262890683122, 1.000000000000000000, 0.9659258262890683122, 1.000000000000000000, 0.9659258262890683122, 1.000000000000000000, 0.9659258262890683122, 1.000000000000000000, 0.9659258262890683122, 1.000000000000000000, 0.9659258262890683122, 1.000000000000000000, 0.9659258262890683122, 1.000000000000000000, 0.9659258262890683122, 1.000000000000000000, 0.9659258262890683122, 1.000000000000000000, 0.9659258262890683122, 1.000000000000000000, 0.9659258262890683122, 1.000000000000000000, 0.9659258262890683122, 1.000000000000000000, 0.9659258262890683122, 1.000000000000000000, 0.9659258262890683122, 1.000000000000000000, 0.9659258262890683122, 1.000000000000000000, 0.9659258262890683122, 1.000000000000000000, 0.9659258262890683122, 1.000000000000000000, 0.9659258262890683122, 1.000000000000000000, 0.9659258262890683122, 1.000000000000000000, 0.9659258262890683122, 1.000000000000000000, 0.9659258262890683122, 1.000000000000000000, 0.9659258262890683122, 1.000000000000000000, 0.9659258262890683122, 1.000000000000000000, 0.9659258262890683122, 1.000000000000000000, 0.9659258262890683122, 1.000000000000000000, 0.9659258262890683122, 1.000000000000000000, 0.9659258262890683122, 1.000000000000000000, 0.9659258262890683122, 1.000000000000000000, 0.9659258262890683122, 1.000000000000000000, 0.9659258262890683122, 1.000000000000000000, 0.9659258262890683122, 1.000000000000000000, 0.9659258262890683122, 1.000000000000000000) ) ) 
 REPRESENTATION_ITEM ( '' )  SURFACE ( )  );
#42996 = EDGE_CURVE ( 'NONE', #19860, #69770, #17454, .T. ) ;
#42997 = CARTESIAN_POINT ( 'NONE',  ( -1.710644741211760467, 1.192425108176624615, 0.3257230034225878645 ) ) ;
#42999 = CARTESIAN_POINT ( 'NONE',  ( -0.1070741851644051862, -0.3996062992125986590, -1.174540682414698445 ) ) ;
#42998 = DIRECTION ( 'NONE',  ( 0.000000000000000000, 0.000000000000000000, 1.000000000000000000 ) ) ;
#43000 = CARTESIAN_POINT ( 'NONE',  ( -0.3917322834645670104, -7.196005306013484475E-17, -2.236220472440944906 ) ) ;
#43001 = CARTESIAN_POINT ( 'NONE',  ( -1.437007874015747477, 0.1660481256975883668, -0.3530559997133364547 ) ) ;
#43002 = CARTESIAN_POINT ( 'NONE',  ( -0.2887139107611542133, 0.2306618581243848609, 0.2411417322834645549 ) ) ;
#43003 = CARTESIAN_POINT ( 'NONE',  ( -0.3458507752293909498, 0.3458507752293907833, -0.3346456692913385988 ) ) ;
#43004 = CARTESIAN_POINT ( 'NONE',  ( -0.3420746716998661618, 0.1974969037888702206, -2.860892388451444113 ) ) ;
#43005 = VERTEX_POINT ( 'NONE', #37198 ) ;
#43006 = CARTESIAN_POINT ( 'NONE',  ( 0.3477690288713918276, -0.5511811023622048555, -0.09757992244046775898 ) ) ;
#43007 = CARTESIAN_POINT ( 'NONE',  ( -0.1049643490035307020, 0.3917322834645669549, -1.573490813648293907 ) ) ;
#43008 = CARTESIAN_POINT ( 'NONE',  ( 0.6430446194225728496, 0.05413385826771666132, 0.4176697321401328100 ) ) ;
#43009 = CARTESIAN_POINT ( 'NONE',  ( -0.1265901696524986964, -0.4724409448818899238, -2.591863517060367439 ) ) ;
#43010 = CARTESIAN_POINT ( 'NONE',  ( 2.154527559055117170, 0.03937007874015747977, 0.4677827689124997024 ) ) ;
#43011 = CARTESIAN_POINT ( 'NONE',  ( -1.679790026246718693, 0.1283753931104746893, -0.1820866141732285504 ) ) ;
#43012 = CARTESIAN_POINT ( 'NONE',  ( 1.338582677165355062, -0.1870078740157479769, 0.4822834645669291653 ) ) ;
#43013 = CARTESIAN_POINT ( 'NONE',  ( 1.161417322834646271, 0.07958543189024071263, -0.2665933059059888421 ) ) ;
#43014 = CARTESIAN_POINT ( 'NONE',  ( 0.5314960629921267055, -0.5400638737290844871, 0.3530559997133364547 ) ) ;
#43015 = B_SPLINE_CURVE_WITH_KNOTS ( 'NONE', 3,
 ( #44718, #64111, #43489, #12355, #75515, #62452, #49815, #6028, #50225, #38012, #82644, #4788 ),
 .UNSPECIFIED., .F., .F.,
 ( 4, 2, 2, 2, 2, 4 ),
 ( 0.05454303362711803577, 0.05585633982237159234, 0.05651299291999837410, 0.05716964601762515585, 0.05848295221287872631, 0.05979625840813228982 ),
 .UNSPECIFIED. ) ;
#43016 = CARTESIAN_POINT ( 'NONE',  ( -0.2867679344610366554, 0.2867679344610365444, -0.7296394768690795951 ) ) ;
#43017 = CARTESIAN_POINT ( 'NONE',  ( -0.1968503937007867743, 0.2952755905511811885, 0.000000000000000000 ) ) ;
#43018 = CARTESIAN_POINT ( 'NONE',  ( -1.043307086614172707, 0.07958543189024071263, -0.2665933059059888421 ) ) ;
#43019 = CARTESIAN_POINT ( 'NONE',  ( 0.2493438320209980519, -0.4281496062992127816, -0.4176697321401328100 ) ) ;
#43020 = CARTESIAN_POINT ( 'NONE',  ( -0.09842519685039295696, 0.1660481256975883668, -0.3530559997133364547 ) ) ;
#43021 = CYLINDRICAL_SURFACE ( 'NONE', #73066, 0.4724409448818898682 ) ;
#43022 = CARTESIAN_POINT ( 'NONE',  ( 0.6406204526026253454, -2.592014407703319119E-15, 0.4118477457932993580 ) ) ;
#43023 = CARTESIAN_POINT ( 'NONE',  ( -0.3392501089628019995, 0.1958661417322831999, -2.227709604495750284 ) ) ;
#43024 = CARTESIAN_POINT ( 'NONE',  ( 0.3937007874015754361, -0.1870078740157479769, 0.4822834645669291653 ) ) ;
#43025 = CARTESIAN_POINT ( 'NONE',  ( -0.4396325459317579898, 0.2952755905511811885, 0.1292274648535926551 ) ) ;
#43026 = CARTESIAN_POINT ( 'NONE',  ( -1.286089238845143479, 0.2306618581243847221, -0.2411417322834647770 ) ) ;
#43027 = CARTESIAN_POINT ( 'NONE',  ( 1.213910761154856299, -0.6692913385826773087, -0.1292274648535924053 ) ) ;
#43028 = CARTESIAN_POINT ( 'NONE',  ( 0.3608923884514443348, -0.6692913385826771977, 0.1292274648535927661 ) ) ;
#43029 = CARTESIAN_POINT ( 'NONE',  ( -0.3917322834645670104, -7.196005306013484475E-17, -0.9114173228346457156 ) ) ;
#43030 = CARTESIAN_POINT ( 'NONE',  ( -0.9251968503937002541, 0.1660481256975885056, 0.3530559997133364547 ) ) ;
#43031 = CARTESIAN_POINT ( 'NONE',  ( 0.4396325459317593221, 0.2952755905511810774, -0.1292274648535930714 ) ) ;
#43032 = CARTESIAN_POINT ( 'NONE',  ( -0.4133858267716528645, -0.5400638737290844871, 0.3530559997133364547 ) ) ;
#43033 = CARTESIAN_POINT ( 'NONE',  ( 0.4133858267716541968, 0.07958543189024085140, 0.2665933059059887866 ) ) ;
#43034 = CARTESIAN_POINT ( 'NONE',  ( -1.686351706036744558, 0.2952755905511810774, -0.1292274648535930714 ) ) ;
#43035 = LINE ( 'NONE', #60344, #55725 ) ;
#43036 = CARTESIAN_POINT ( 'NONE',  ( 0.2230971128608929543, 0.05413385826771626580, -0.4176697321401330321 ) ) ;
#43037 = CARTESIAN_POINT ( 'NONE',  ( 0.000000000000000000, 0.000000000000000000, 6.062992125984251857 ) ) ;
#43038 = CARTESIAN_POINT ( 'NONE',  ( 1.404199475065617264, -0.4281496062992124485, 0.4176697321401328655 ) ) ;
#43039 = CARTESIAN_POINT ( 'NONE',  ( 0.1049643490035304938, -0.3917322834645669549, -2.597112860892388131 ) ) ;
#43040 = ORIENTED_EDGE ( 'NONE', *, *, #31271, .T. ) ;
#43041 = ORIENTED_EDGE ( 'NONE', *, *, #61425, .T. ) ;
#43042 = CARTESIAN_POINT ( 'NONE',  ( 0.7742782152230979209, 0.05413385826771626580, -0.4176697321401330321 ) ) ;
#43043 = CARTESIAN_POINT ( 'NONE',  ( 0.09842519685039434474, -0.4536011799217368745, -0.2665933059059886201 ) ) ;
#43045 = DIRECTION ( 'NONE',  ( 1.000000000000000000, 0.000000000000000000, 0.000000000000000000 ) ) ;
#43044 = DIRECTION ( 'NONE',  ( 0.000000000000000000, -1.000000000000000000, 0.000000000000000000 ) ) ;
#43046 = CARTESIAN_POINT ( 'NONE',  ( 0.3917322834645669549, 0.1049643490035304660, -0.9967191601049870675 ) ) ;
#43047 = CARTESIAN_POINT ( 'NONE',  ( -0.9563780557770518165, -3.764720552277026557E-15, -0.3791475997938235643 ) ) ;
#43048 = ADVANCED_FACE ( 'NONE', ( #68781 ), #22509, .F. ) ;
#43049 = CARTESIAN_POINT ( 'NONE',  ( -0.3996062992125984925, -0.1070741851644056858, -2.484908136482939955 ) ) ;
#43050 = CARTESIAN_POINT ( 'NONE',  ( 0.4658792650918640033, -0.3162353388693405765, 0.4822834645669290543 ) ) ;
#43051 = CARTESIAN_POINT ( 'NONE',  ( -0.6496062992125976043, 0.1660481256975883668, -0.3530559997133364547 ) ) ;
#43052 = CARTESIAN_POINT ( 'NONE',  ( -0.9317585301837263412, 0.05413385826771666132, 0.4176697321401328100 ) ) ;
#43053 = CARTESIAN_POINT ( 'NONE',  ( 0.6824146981627303710, 0.2306618581243847221, -0.2411417322834647770 ) ) ;
#43054 = CARTESIAN_POINT ( 'NONE',  ( 1.430446194225722500, 0.05413385826771666132, 0.4176697321401328100 ) ) ;
#43055 = CARTESIAN_POINT ( 'NONE',  ( 1.167979002624672580, -0.3690944881889763329, 0.3153832671262228327 ) ) ;
#43056 = CARTESIAN_POINT ( 'NONE',  ( 1.095800524934383846, -0.08942795157528024563, -0.3641732283464568787 ) ) ;
#43057 = CARTESIAN_POINT ( 'NONE',  ( -0.6692913385826764205, 0.2952755905511811885, 0.000000000000000000 ) ) ;
#43058 = CARTESIAN_POINT ( 'NONE',  ( 0.2925321140481932369, 0.2925321140481932369, -0.3720472440944882497 ) ) ;
#43059 = CARTESIAN_POINT ( 'NONE',  ( 1.528871391076116026, 0.2952755905511811885, 0.1292274648535926551 ) ) ;
#43060 = CARTESIAN_POINT ( 'NONE',  ( 0.3917322834645670104, 2.398668435337828261E-17, -0.1102362204724409156 ) ) ;
#43061 = CARTESIAN_POINT ( 'NONE',  ( -0.2427821522309703550, -0.3162353388693405765, 0.4822834645669290543 ) ) ;
#43063 = DIRECTION ( 'NONE',  ( 1.000000000000000000, 0.000000000000000000, 0.000000000000000000 ) ) ;
#43062 = CARTESIAN_POINT ( 'NONE',  ( 0.9776902887139113929, -0.6692913385826773087, -0.1292274648535924053 ) ) ;
#43064 = CARTESIAN_POINT ( 'NONE',  ( -1.200787401574802349, 0.07958543189024071263, -0.2665933059059888421 ) ) ;
#43065 = CARTESIAN_POINT ( 'NONE',  ( 0.3543307086614181922, -0.6692913385826771977, 8.415575281601705876E-17 ) ) ;
#43066 = CARTESIAN_POINT ( 'NONE',  ( 1.023622047244095112, -0.1870078740157480601, -0.3641732283464567677 ) ) ;
#43067 = CARTESIAN_POINT ( 'NONE',  ( -0.1958661417322836440, 0.3392501089628016664, -1.825440001803462886 ) ) ;
#43068 = CARTESIAN_POINT ( 'NONE',  ( -1.227034120734907585, 0.1771653543307087630, 0.09757992244046791164 ) ) ;
#43069 = CARTESIAN_POINT ( 'NONE',  ( 0.7742782152230979209, 0.05413385826771626580, -0.4176697321401330321 ) ) ;
#43070 = CARTESIAN_POINT ( 'NONE',  ( 0.000000000000000000, 0.03937007874015747977, 0.000000000000000000 ) ) ;
#43071 = CARTESIAN_POINT ( 'NONE',  ( -0.3871391076115479057, -0.2845877964562161244, -0.3641732283464567121 ) ) ;
#43072 = CARTESIAN_POINT ( 'NONE',  ( -0.2362204724409442680, -0.1870078740157480879, -0.4822834645669291653 ) ) ;
#43073 = CARTESIAN_POINT ( 'NONE',  ( -1.200787401574802349, -0.4536011799217367080, 0.2665933059059888421 ) ) ;
#43074 = CARTESIAN_POINT ( 'NONE',  ( -0.7939632545931754048, -0.3162353388693405765, 0.4822834645669290543 ) ) ;
#43075 = CARTESIAN_POINT ( 'NONE',  ( 1.358267716535433323, 0.1660481256975885056, 0.3530559997133364547 ) ) ;
#43076 = CARTESIAN_POINT ( 'NONE',  ( -0.1049643490035307158, 0.3917322834645670104, -0.4757411005587420805 ) ) ;
#43077 = CARTESIAN_POINT ( 'NONE',  ( -1.069553805774277722, -0.5511811023622048555, -0.09757992244046775898 ) ) ;
#43078 = DIRECTION ( 'NONE',  ( -0.000000000000000000, -1.000000000000000000, -0.000000000000000000 ) ) ;
#43079 = CARTESIAN_POINT ( 'NONE',  ( 1.351706036745407458, -0.4281496062992127816, -0.4176697321401328100 ) ) ;
#43080 = CARTESIAN_POINT ( 'NONE',  ( 0.4091458600556404646, -0.2362204724409448231, -1.914041994750656395 ) ) ;
#43081 = CARTESIAN_POINT ( 'NONE',  ( -1.292650918635170010, -0.6692913385826771977, 0.1292274648535927661 ) ) ;
#43082 = CARTESIAN_POINT ( 'NONE',  ( -1.292650918635170010, 0.1771653543307087075, -0.09757992244046823083 ) ) ;
#43083 = CARTESIAN_POINT ( 'NONE',  ( -0.4396325459317579898, 0.1771653543307087630, 0.09757992244046791164 ) ) ;
#43084 = CARTESIAN_POINT ( 'NONE',  ( -1.607611548556429737, 0.2952755905511810774, -0.1292274648535930714 ) ) ;
#43085 = CARTESIAN_POINT ( 'NONE',  ( 0.04593175853018440641, -0.6692913385826771977, 0.1292274648535927661 ) ) ;
#43086 = CARTESIAN_POINT ( 'NONE',  ( 0.08530183727034192087, -0.08942795157527998196, 0.3641732283464567121 ) ) ;
#43087 = CARTESIAN_POINT ( 'NONE',  ( -1.207349081364828880, 0.1283753931104746893, -0.1820866141732285504 ) ) ;
#43088 = CARTESIAN_POINT ( 'NONE',  ( -1.397637795275589623, 0.1660481256975885056, 0.3530559997133364547 ) ) ;
#43089 = CARTESIAN_POINT ( 'NONE',  ( 1.207349081364829990, -0.5023911411419708095, -0.1820866141732282451 ) ) ;
#43090 = CARTESIAN_POINT ( 'NONE',  ( 1.017060367454068803, -0.3162353388693405765, 0.4822834645669290543 ) ) ;
#43091 = CARTESIAN_POINT ( 'NONE',  ( -1.595398199321657939, 0.4829664696085548825, -0.1559797534342468039 ) ) ;
#43092 = CARTESIAN_POINT ( 'NONE',  ( 0.6233595800524942554, -0.08942795157528024563, -0.3641732283464568787 ) ) ;
#43093 = CARTESIAN_POINT ( 'NONE',  ( 0.9383202099737538715, -0.05778040916215560624, -0.4822834645669293319 ) ) ;
#43094 = CONICAL_SURFACE ( 'NONE', #53855, 0.1771653543307085410, 1.029744258676653645 ) ;
#43095 = CARTESIAN_POINT ( 'NONE',  ( 1.069553805774278610, -0.5511811023622046335, 0.09757992244046803654 ) ) ;
#43096 = VERTEX_POINT ( 'NONE', #61639 ) ;
#43097 = CARTESIAN_POINT ( 'NONE',  ( -1.095800524934382292, -0.3162353388693409650, -0.4822834645669289433 ) ) ;
#43098 = CARTESIAN_POINT ( 'NONE',  ( -0.8333333333333323711, 0.2952755905511811885, 0.1292274648535926551 ) ) ;
#43099 = CARTESIAN_POINT ( 'NONE',  ( -0.1246719160104980823, 0.2952755905511811885, 0.1292274648535926551 ) ) ;
#43100 = CARTESIAN_POINT ( 'NONE',  ( 0.5396849562100397568, 1.809133623825372073E-16, -0.3791483426435173776 ) ) ;
#43101 = CARTESIAN_POINT ( 'NONE',  ( -0.1070741851644051862, -0.3996062992125986590, -2.826115485564304475 ) ) ;
#43102 = CARTESIAN_POINT ( 'NONE',  ( 0.6627296587926515548, 0.2952755905511811885, 0.1292274648535926551 ) ) ;
#43103 = CARTESIAN_POINT ( 'NONE',  ( 1.312335958005249825, 0.1283753931104746893, -0.1820866141732285504 ) ) ;
#43104 = CARTESIAN_POINT ( 'NONE',  ( -0.05905511811023545637, 0.1660481256975885056, 0.3530559997133364547 ) ) ;
#43105 = CARTESIAN_POINT ( 'NONE',  ( 0.7874015748031503170, -0.1870078740157479769, 0.4822834645669291653 ) ) ;
#43106 = CARTESIAN_POINT ( 'NONE',  ( -0.1998031496062994683, 0.3460692066303958092, -1.902887139107611647 ) ) ;
#43107 = CARTESIAN_POINT ( 'NONE',  ( -0.3420746716998659953, -0.1974969037888706647, -1.312335958005249159 ) ) ;
#43108 = CARTESIAN_POINT ( 'NONE',  ( -0.1070741851644051862, -0.3996062992125987146, -2.906824146981627610 ) ) ;
#43109 = CARTESIAN_POINT ( 'NONE',  ( 0.4037097067573611753, 1.223219560026271499E-15, 0.4445507791589056734 ) ) ;
#43110 = CARTESIAN_POINT ( 'NONE',  ( -0.1049643490035307020, 0.3917322834645669549, -0.4711286089238844732 ) ) ;
#43111 = CARTESIAN_POINT ( 'NONE',  ( -0.6036745406824141069, 0.1283753931104748280, 0.1820866141732283561 ) ) ;
#43112 = CARTESIAN_POINT ( 'NONE',  ( -0.8989501312335946848, 0.2952755905511810774, -0.1292274648535930714 ) ) ;
#43113 = CARTESIAN_POINT ( 'NONE',  ( 0.5380577427821529035, 0.05413385826771626580, -0.4176697321401330321 ) ) ;
#43114 = CARTESIAN_POINT ( 'NONE',  ( -0.1058382717557497660, -0.3949938075777411073, -2.196194225721785021 ) ) ;
#43115 = CARTESIAN_POINT ( 'NONE',  ( 0.9645669291338591078, -0.5400638737290845981, -0.3530559997133363437 ) ) ;
#43116 = CARTESIAN_POINT ( 'NONE',  ( -1.476377952755905110, 0.1660481256975885056, 0.3530559997133364547 ) ) ;
#43117 = CARTESIAN_POINT ( 'NONE',  ( 1.384514435695538337, -0.6692913385826771977, 0.1292274648535927661 ) ) ;
#43118 = CARTESIAN_POINT ( 'NONE',  ( -0.4724409448818895907, -0.1265901696524993070, -2.565616797900262647 ) ) ;
#43119 = CARTESIAN_POINT ( 'NONE',  ( -0.1998031496062994683, 0.3460692066303958092, -2.217847769028871596 ) ) ;
#43120 = CARTESIAN_POINT ( 'NONE',  ( -0.01881781417526427053, 0.4724409448818898682, -2.754912411187758980 ) ) ;
#43121 = CARTESIAN_POINT ( 'NONE',  ( 0.9514435695538062676, -0.05778040916215522460, 0.4822834645669289988 ) ) ;
#43122 = CARTESIAN_POINT ( 'NONE',  ( 0.5446194225721792126, -0.05778040916215560624, -0.4822834645669293319 ) ) ;
#43123 = CARTESIAN_POINT ( 'NONE',  ( 1.181102362204724976, -0.1870078740157480601, -0.3641732283464567677 ) ) ;
#43125 = CARTESIAN_POINT ( 'NONE',  ( 1.541994750656168645, -0.6692913385826771977, 0.1292274648535927661 ) ) ;
#43124 = CARTESIAN_POINT ( 'NONE',  ( 1.646981627296588035, -0.3162353388693405765, 0.4822834645669290543 ) ) ;
#43126 = CARTESIAN_POINT ( 'NONE',  ( 0.1049643490035304522, -0.3917322834645668994, -2.685020054296901382 ) ) ;
#43127 = CARTESIAN_POINT ( 'NONE',  ( 0.7414698162729663755, 0.2952755905511811885, 0.1292274648535926551 ) ) ;
#43128 = CARTESIAN_POINT ( 'NONE',  ( 1.640419947506562393, -0.3690944881889763329, 0.3153832671262228327 ) ) ;
#43129 = CARTESIAN_POINT ( 'NONE',  ( -0.7086614173228339419, -0.1870078740157480879, -0.4822834645669291653 ) ) ;
#43130 = CARTESIAN_POINT ( 'NONE',  ( -0.4593175853018366950, 0.05413385826771666132, 0.4176697321401328100 ) ) ;
#43131 = VECTOR ( 'NONE', #81075, 39.37007874015748143 ) ;
#43132 = CARTESIAN_POINT ( 'NONE',  ( 1.548556430446194954, -0.6046776061558807314, 0.2411417322834647770 ) ) ;
#43133 = B_SPLINE_CURVE_WITH_KNOTS ( 'NONE', 3,
 ( #63356, #4053, #30130, #30951 ),
 .UNSPECIFIED., .F., .F.,
 ( 4, 4 ),
 ( 3.210432057656183116E-07, 0.001287787053612145412 ),
 .UNSPECIFIED. ) ;
#43134 = CARTESIAN_POINT ( 'NONE',  ( -0.3917322834645669549, -0.1049643490035306603, -0.2880577427821523484 ) ) ;
#43135 = CARTESIAN_POINT ( 'NONE',  ( 0.3392501089628018329, 0.1958661417322835607, -1.698162729658792891 ) ) ;
#43136 = CARTESIAN_POINT ( 'NONE',  ( -0.1958661417322834220, -0.3392501089628018884, -2.262467191601049699 ) ) ;
#43137 = CARTESIAN_POINT ( 'NONE',  ( -1.456692913385826182, 0.1771653543307087630, 0.000000000000000000 ) ) ;
#43138 = ORIENTED_EDGE ( 'NONE', *, *, #64406, .T. ) ;
#43139 = CARTESIAN_POINT ( 'NONE',  ( -0.3949938075777409963, -7.255918531996591613E-17, -2.716535433070866201 ) ) ;
#43140 = VERTEX_POINT ( 'NONE', #36783 ) ;
#43141 = DIRECTION ( 'NONE',  ( -0.000000000000000000, -1.000000000000000000, -0.000000000000000000 ) ) ;
#43142 = CARTESIAN_POINT ( 'NONE',  ( 1.587926509186352142, -0.004921259842519576551, 0.3153832671262227771 ) ) ;
#43143 = CARTESIAN_POINT ( 'NONE',  ( 0.3996062992125986035, 0.1070741851644054776, -1.227034120734908029 ) ) ;
#43144 = CARTESIAN_POINT ( 'NONE',  ( 0.5636006452641431075, 3.421639014772782816E-16, 0.3464511005275203726 ) ) ;
#43145 = FACE_OUTER_BOUND ( 'NONE', #72665, .T. ) ;
#43146 = DIRECTION ( 'NONE',  ( 0.000000000000000000, 1.734723475976808327E-16, -1.000000000000000000 ) ) ;
#43147 = CARTESIAN_POINT ( 'NONE',  ( -0.2908506741759562808, 1.813884536108223866, 0.1160749510518452737 ) ) ;
#43148 = CARTESIAN_POINT ( 'NONE',  ( 0.1958661417322834775, 0.3392501089628018884, -0.2290026246719160941 ) ) ;
#43149 = CARTESIAN_POINT ( 'NONE',  ( -0.6102362204724400829, -0.4536011799217368745, -0.2665933059059886201 ) ) ;
#43150 = CARTESIAN_POINT ( 'NONE',  ( -1.345144356955379816, -0.08942795157528024563, -0.3641732283464568787 ) ) ;
#43151 = CARTESIAN_POINT ( 'NONE',  ( 0.7217847769028878924, -0.4281496062992127816, -0.4176697321401328100 ) ) ;
#43152 = CARTESIAN_POINT ( 'NONE',  ( -1.259842519685038686, -0.1870078740157480879, -0.4822834645669291653 ) ) ;
#43153 = CIRCLE ( 'NONE', #69372, 3.267716535433071279 ) ;
#43154 = CARTESIAN_POINT ( 'NONE',  ( -0.1958661417322834220, -0.3392501089628018884, -0.2152230971128608339 ) ) ;
#43155 = VERTEX_POINT ( 'NONE', #29644 ) ;
#43156 = CARTESIAN_POINT ( 'NONE',  ( 1.587926509186352142, 0.05413385826771666132, 0.4176697321401328100 ) ) ;
#43157 = CARTESIAN_POINT ( 'NONE',  ( -0.4677827689124922084, 0.03937007874015747977, -2.154527559055118946 ) ) ;
#43158 = CARTESIAN_POINT ( 'NONE',  ( 0.3458507752293908943, -0.3458507752293908943, -1.673228346456692828 ) ) ;
#43159 = DIRECTION ( 'NONE',  ( -0.000000000000000000, 0.000000000000000000, 1.000000000000000000 ) ) ;
#43160 = CARTESIAN_POINT ( 'NONE',  ( 0.1958661417322836440, -0.3392501089628017219, -2.696194225721784576 ) ) ;
#43161 = CARTESIAN_POINT ( 'NONE',  ( -0.5971128608923877978, -0.6692913385826773087, -0.1292274648535924053 ) ) ;
#43162 = CARTESIAN_POINT ( 'NONE',  ( 0.8202099737532814183, -0.6692913385826773087, -0.1292274648535924053 ) ) ;
#43164 = CARTESIAN_POINT ( 'NONE',  ( -0.2362204724409447953, -0.4091458600556404646, -1.955380577427821454 ) ) ;
#43163 = CARTESIAN_POINT ( 'NONE',  ( 0.5314960629921063884, 2.729653127095272414, 1.868118615532837756 ) ) ;
#43165 = CARTESIAN_POINT ( 'NONE',  ( 1.646981627296588035, -0.3162353388693405765, 0.4822834645669290543 ) ) ;
#43166 = CARTESIAN_POINT ( 'NONE',  ( -1.122047244094487306, -0.5400638737290844871, 0.3530559997133364547 ) ) ;
#43167 = CARTESIAN_POINT ( 'NONE',  ( 0.2867679344610365999, 0.2867679344610365999, -0.3753087682076623466 ) ) ;
#43168 = CARTESIAN_POINT ( 'NONE',  ( 0.2099737532808405305, 0.1283753931104746893, -0.1820866141732285504 ) ) ;
#43169 = CARTESIAN_POINT ( 'NONE',  ( 0.3392501089628018329, 0.1958661417322835607, -1.003280839895013266 ) ) ;
#43170 = CARTESIAN_POINT ( 'NONE',  ( 8.195543980992789655E-16, -0.1870078740157480601, -0.3641732283464567677 ) ) ;
#43171 = CARTESIAN_POINT ( 'NONE',  ( 0.4330708661417329575, -0.5511811023622047445, 6.969142054262312111E-17 ) ) ;
#43172 = CARTESIAN_POINT ( 'NONE',  ( 0.5971128608923890191, -0.6692913385826771977, 0.1292274648535927661 ) ) ;
#43173 = CARTESIAN_POINT ( 'NONE',  ( -0.6299212598425188991, -0.1870078740157480601, -0.3641732283464567677 ) ) ;
#43174 = CARTESIAN_POINT ( 'NONE',  ( 0.3917322834645670104, 2.398668435337828261E-17, -2.157480314960630086 ) ) ;
#43175 = CARTESIAN_POINT ( 'NONE',  ( 1.502624671916010790, -0.3162353388693409650, -0.4822834645669289433 ) ) ;
#43176 = CARTESIAN_POINT ( 'NONE',  ( -1.036745406824146176, -0.4281496062992124485, 0.4176697321401328655 ) ) ;
#43177 = CARTESIAN_POINT ( 'NONE',  ( 0.4091458600556404646, -0.2362204724409448231, -0.8116797900262466836 ) ) ;
#43178 = CARTESIAN_POINT ( 'NONE',  ( -0.1377952755905504645, 0.1660481256975885056, 0.3530559997133364547 ) ) ;
#43179 = CARTESIAN_POINT ( 'NONE',  ( -0.6955380577427815458, 0.05413385826771666132, 0.4176697321401328100 ) ) ;
#43180 = CARTESIAN_POINT ( 'NONE',  ( 1.279527559055118724, -0.4536011799217368745, -0.2665933059059886201 ) ) ;
#43181 = CARTESIAN_POINT ( 'NONE',  ( 0.07874015748031558404, -0.1870078740157480601, -0.3641732283464567677 ) ) ;
#43182 = CARTESIAN_POINT ( 'NONE',  ( -0.3018372703412066094, 0.05413385826771666132, 0.4176697321401328100 ) ) ;
#43183 = CARTESIAN_POINT ( 'NONE',  ( -1.318897637795274802, 0.1660481256975885056, 0.3530559997133364547 ) ) ;
#43184 = CARTESIAN_POINT ( 'NONE',  ( 1.586334378693442959, 1.535433070866141447, 0.1093658747564338618 ) ) ;
#43185 = DIRECTION ( 'NONE',  ( -0.6537823813707712706, 0.7566826268715064474, 0.000000000000000000 ) ) ;
#43186 = CARTESIAN_POINT ( 'NONE',  ( 0.05905511811023709395, -0.5400638737290844871, 0.3530559997133364547 ) ) ;
#43187 = CONICAL_SURFACE ( 'NONE', #47230, 0.1181102362204724116, 0.7853981633974536081 ) ;
#43188 = ORIENTED_EDGE ( 'NONE', *, *, #14047, .T. ) ;
#43189 = CARTESIAN_POINT ( 'NONE',  ( -0.1998031496062991630, -0.3460692066303959202, -2.032152230971128848 ) ) ;
#43190 = CARTESIAN_POINT ( 'NONE',  ( 0.9645669291338588858, 0.1660481256975885056, 0.3530559997133364547 ) ) ;
#43191 = CARTESIAN_POINT ( 'NONE',  ( -0.5839895013123351797, 0.1771653543307087075, -0.09757992244046823083 ) ) ;
#43192 = CARTESIAN_POINT ( 'NONE',  ( -0.5118110236220466680, -0.6692913385826771977, 8.415575281601705876E-17 ) ) ;
#43193 = CARTESIAN_POINT ( 'NONE',  ( 1.246719160104987623, 0.05413385826771626580, -0.4176697321401330321 ) ) ;
#43194 = CARTESIAN_POINT ( 'NONE',  ( 1.030183727034121421, -0.05778040916215522460, 0.4822834645669289988 ) ) ;
#43195 = B_SPLINE_CURVE_WITH_KNOTS ( 'NONE', 3,
 ( #59981, #60400, #56854, #56447 ),
 .UNSPECIFIED., .F., .F.,
 ( 4, 4 ),
 ( 4.906538933386797396E-18, 0.001730108991777465225 ),
 .UNSPECIFIED. ) ;
#43196 = CARTESIAN_POINT ( 'NONE',  ( -1.568241469816272105, -0.3162353388693409650, -0.4822834645669289433 ) ) ;
#43197 = CARTESIAN_POINT ( 'NONE',  ( -0.9120734908136475250, 0.1771653543307087630, 0.09757992244046791164 ) ) ;
#43198 = CARTESIAN_POINT ( 'NONE',  ( 0.3460692066303958092, 0.1998031496062993018, -0.05052493438320212332 ) ) ;
#43199 = CARTESIAN_POINT ( 'NONE',  ( 4.893765752498283924E-17, -0.3996062992125986035, -0.3937007874015748254 ) ) ;
#43200 = CARTESIAN_POINT ( 'NONE',  ( -0.3420746716998661618, 0.1974969037888702206, -0.3412073490813648524 ) ) ;
#43201 = FACE_OUTER_BOUND ( 'NONE', #39202, .T. ) ;
#43202 = CARTESIAN_POINT ( 'NONE',  ( 0.5380577427821529035, -0.004921259842519870586, -0.3153832671262229437 ) ) ;
#43203 = CARTESIAN_POINT ( 'NONE',  ( 0.3805774278215230400, 0.05413385826771626580, -0.4176697321401330321 ) ) ;
#43204 = CARTESIAN_POINT ( 'NONE',  ( 0.2544983382031790753, -0.1500752278769513504, 0.1555222293686583102 ) ) ;
#43205 = CARTESIAN_POINT ( 'NONE',  ( 0.1974969037888704704, 0.3420746716998660508, -0.8510498687664042050 ) ) ;
#43206 = CARTESIAN_POINT ( 'NONE',  ( 0.8792650918635177559, -0.004921259842519576551, 0.3153832671262227771 ) ) ;
#43207 = CARTESIAN_POINT ( 'NONE',  ( -0.5052493438320203589, 0.2952755905511810774, -0.1292274648535930714 ) ) ;
#43208 = CARTESIAN_POINT ( 'NONE',  ( -0.7677165354330699465, -0.5400638737290845981, -0.3530559997133363437 ) ) ;
#43209 = CARTESIAN_POINT ( 'NONE',  ( 1.384514435695538559, 0.2952755905511810774, -0.1292274648535930714 ) ) ;
#43210 = CARTESIAN_POINT ( 'NONE',  ( 0.4091458600556404646, -0.2362204724409448231, -1.364829396325459188 ) ) ;
#43211 = CARTESIAN_POINT ( 'NONE',  ( 0.2925321140481932369, 0.2925321140481932369, -2.500000000000000000 ) ) ;
#43212 = CARTESIAN_POINT ( 'NONE',  ( -0.2624671916010490880, 0.1283753931104746893, -0.1820866141732285504 ) ) ;
#43213 = ORIENTED_EDGE ( 'NONE', *, *, #9570, .F. ) ;
#43214 = CARTESIAN_POINT ( 'NONE',  ( 0.1958661417322836718, -0.3392501089628017219, -0.8760035677503431595 ) ) ;
#43215 = ORIENTED_EDGE ( 'NONE', *, *, #33608, .F. ) ;
#43216 = CARTESIAN_POINT ( 'NONE',  ( -0.9842519685039365918, -0.6692913385826771977, 8.415575281601705876E-17 ) ) ;
#43217 = CARTESIAN_POINT ( 'NONE',  ( -0.09186351706036663400, -0.4281496062992124485, 0.4176697321401328655 ) ) ;
#43218 = CARTESIAN_POINT ( 'NONE',  ( -0.3477690288713902178, 0.2952755905511810774, -0.1292274648535930714 ) ) ;
#43219 = CARTESIAN_POINT ( 'NONE',  ( 0.3215223097112867578, -0.3162353388693409650, -0.4822834645669289433 ) ) ;
#43220 = CARTESIAN_POINT ( 'NONE',  ( -0.4068241469816264999, -0.4281496062992124485, 0.4176697321401328655 ) ) ;
#43221 = CARTESIAN_POINT ( 'NONE',  ( -1.135170603674539924, 0.2952755905511810774, -0.1292274648535930714 ) ) ;
#43222 = CARTESIAN_POINT ( 'NONE',  ( -0.8530183727034112984, -0.4281496062992127816, -0.4176697321401328100 ) ) ;
#43223 = CARTESIAN_POINT ( 'NONE',  ( 0.8858267716535438430, -0.5400638737290845981, -0.3530559997133363437 ) ) ;
#43224 = CARTESIAN_POINT ( 'NONE',  ( 0.4461942257217855201, -0.6046776061558807314, 0.2411417322834647770 ) ) ;
#43225 = EDGE_CURVE ( 'NONE', #1055, #26552, #56135, .T. ) ;
#43226 = CARTESIAN_POINT ( 'NONE',  ( 0.3392501089628018329, 0.1958661417322835607, -1.225721784776902634 ) ) ;
#43227 = CARTESIAN_POINT ( 'NONE',  ( -0.1968503937007867743, 0.1771653543307087630, 0.000000000000000000 ) ) ;
#43228 = EDGE_LOOP ( 'NONE', ( #35103, #32060, #40039, #15413, #73270, #15533 ) ) ;
#43229 = CARTESIAN_POINT ( 'NONE',  ( 0.3949938075777409408, 0.1058382717557500574, -1.384514435695538337 ) ) ;
#43230 = VERTEX_POINT ( 'NONE', #49414 ) ;
#43231 = CARTESIAN_POINT ( 'NONE',  ( -1.364829396325458521, 0.1283753931104746893, -0.1820866141732285504 ) ) ;
#43232 = CARTESIAN_POINT ( 'NONE',  ( -1.292650918635170010, 0.2952755905511810774, -0.1292274648535930714 ) ) ;
#43233 = CARTESIAN_POINT ( 'NONE',  ( -0.5314960629921250401, 0.1660481256975885056, 0.3530559997133364547 ) ) ;
#43234 = CARTESIAN_POINT ( 'NONE',  ( 0.1998031496062994405, -0.3460692066303958092, 0.06561679790026245240 ) ) ;
#43235 = CARTESIAN_POINT ( 'NONE',  ( -0.6167979002624665030, 0.05413385826771666132, 0.4176697321401328100 ) ) ;
#43236 = CARTESIAN_POINT ( 'NONE',  ( -1.023622047244094002, -0.1870078740157480879, -0.4822834645669291653 ) ) ;
#43237 = CYLINDRICAL_SURFACE ( 'NONE', #76736, 0.5118110236220471121 ) ;
#43238 = CARTESIAN_POINT ( 'NONE',  ( -1.313877454013331780, 0.2755905511811023723, 0.6999040823587869831 ) ) ;
#43239 = CARTESIAN_POINT ( 'NONE',  ( 0.5183727034120741983, -0.5511811023622046335, 0.09757992244046803654 ) ) ;
#43240 = CARTESIAN_POINT ( 'NONE',  ( 0.4768139191967642465, 1.559564387633134874, 0.5050868514466244630 ) ) ;
#43241 = CARTESIAN_POINT ( 'NONE',  ( -0.03280839895013062252, -0.5511811023622046335, 0.09757992244046803654 ) ) ;
#43242 = CARTESIAN_POINT ( 'NONE',  ( -0.3280839895013117347, 0.05413385826771626580, -0.4176697321401330321 ) ) ;
#43243 = DIRECTION ( 'NONE',  ( 0.8479387356305982948, 2.625811289636359704E-16, -0.5300942374872437135 ) ) ;
#43244 = CARTESIAN_POINT ( 'NONE',  ( -0.01312335958005186876, 0.05413385826771626580, -0.4176697321401330321 ) ) ;
#43245 = ORIENTED_EDGE ( 'NONE', *, *, #67561, .F. ) ;
#43246 = CARTESIAN_POINT ( 'NONE',  ( 0.2925321140481932369, 0.2925321140481932369, -2.027559055118109743 ) ) ;
#43247 = CARTESIAN_POINT ( 'NONE',  ( -0.8267716535433065062, 0.2066929133858268208, 0.000000000000000000 ) ) ;
#43248 = EDGE_LOOP ( 'NONE', ( #31543, #60116, #63238, #18682 ) ) ;
#43249 = CARTESIAN_POINT ( 'NONE',  ( -9.787531504996566615E-17, 0.3996062992125985480, -1.494094488188976388 ) ) ;
#43250 = CIRCLE ( 'NONE', #6971, 3.858267716535433323 ) ;
#43251 = CARTESIAN_POINT ( 'NONE',  ( 1.587926509186352142, 0.05413385826771666132, 0.4176697321401328100 ) ) ;
#43252 = CARTESIAN_POINT ( 'NONE',  ( -0.7742782152230965886, -0.004921259842519576551, 0.3153832671262227771 ) ) ;
#43253 = CARTESIAN_POINT ( 'NONE',  ( -0.9383202099737524282, -0.05778040916215522460, 0.4822834645669289988 ) ) ;
#43254 = CARTESIAN_POINT ( 'NONE',  ( -1.157146581871515012E-16, 0.4724409448818898682, -0.3149606299212598381 ) ) ;
#43255 = CARTESIAN_POINT ( 'NONE',  ( 4.821444151489972621E-16, 1.062992125984252745, 3.937007874015748143 ) ) ;
#43256 = CARTESIAN_POINT ( 'NONE',  ( -0.2867679344610364334, -0.2867679344610367109, 0.1062992125984252439 ) ) ;
#43257 = CARTESIAN_POINT ( 'NONE',  ( 1.469816272965879911, -0.6046776061558807314, 0.2411417322834647770 ) ) ;
#43258 = CARTESIAN_POINT ( 'NONE',  ( 0.6036745406824153282, -0.6046776061558807314, 0.2411417322834647770 ) ) ;
#43259 = CARTESIAN_POINT ( 'NONE',  ( 0.4396325459317593221, 0.2952755905511810774, -0.1292274648535930714 ) ) ;
#43260 = CARTESIAN_POINT ( 'NONE',  ( -0.8070866141732276899, 0.07958543189024071263, -0.2665933059059888421 ) ) ;
#43261 = CARTESIAN_POINT ( 'NONE',  ( -0.2559055118110230564, 0.1660481256975883668, -0.3530559997133364547 ) ) ;
#43262 = CARTESIAN_POINT ( 'NONE',  ( -0.4724409448818895907, -0.1265901696524993070, -2.327427821522309426 ) ) ;
#43263 = CARTESIAN_POINT ( 'NONE',  ( -0.7808398950131225646, -0.05778040916215522460, 0.4822834645669289988 ) ) ;
#43264 = CARTESIAN_POINT ( 'NONE',  ( 0.1974969037888704704, 0.3420746716998660508, -2.110892388451443225 ) ) ;
#43265 = CARTESIAN_POINT ( 'NONE',  ( 1.141732283464567566, 0.1771653543307087630, 0.000000000000000000 ) ) ;
#43266 = CARTESIAN_POINT ( 'NONE',  ( -0.4855643044619415427, -0.3690944881889763329, 0.3153832671262228327 ) ) ;
#43267 = CARTESIAN_POINT ( 'NONE',  ( 1.240157480314961314, 0.07958543189024071263, -0.2665933059059888421 ) ) ;
#43269 = EDGE_CURVE ( 'NONE', #31620, #45375, #17041, .T. ) ;
#43268 = CARTESIAN_POINT ( 'NONE',  ( -1.646981627296586703, -0.3162353388693409650, -0.4822834645669289433 ) ) ;
#43270 = CARTESIAN_POINT ( 'NONE',  ( -1.095800524934382292, -0.2845877964562161244, -0.3641732283464567121 ) ) ;
#43271 = CARTESIAN_POINT ( 'NONE',  ( 0.1450607720586929161, 2.784432375088962958E-17, -0.3464511005275205946 ) ) ;
#43272 = CARTESIAN_POINT ( 'NONE',  ( 0.5511811023622055217, -0.1870078740157479769, 0.3641732283464567677 ) ) ;
#43273 = CARTESIAN_POINT ( 'NONE',  ( -0.3018372703412066094, -0.4281496062992127816, -0.4176697321401328100 ) ) ;
#43274 = CARTESIAN_POINT ( 'NONE',  ( 0.000000000000000000, 0.07874015748031502893, 0.000000000000000000 ) ) ;
#43275 = CARTESIAN_POINT ( 'NONE',  ( -0.1771653543307080136, 0.07958543189024071263, -0.2665933059059888421 ) ) ;
#43276 = CARTESIAN_POINT ( 'NONE',  ( 0.4091458600556403535, 0.2362204724409449896, -0.9954068241469815614 ) ) ;
#43277 = CARTESIAN_POINT ( 'NONE',  ( 0.5511811023622055217, -0.1870078740157479769, 0.4822834645669291653 ) ) ;
#43278 = CARTESIAN_POINT ( 'NONE',  ( 0.4849061582275016602, 2.793565526369266028, 0.4921425059946344382 ) ) ;
#43279 = CARTESIAN_POINT ( 'NONE',  ( 1.266404199475066328, -0.08942795157527998196, 0.3641732283464567121 ) ) ;
#43280 = CARTESIAN_POINT ( 'NONE',  ( -1.023622047244094002, -0.1870078740157480879, -0.4822834645669291653 ) ) ;
#43281 = CARTESIAN_POINT ( 'NONE',  ( -0.3215223097112853146, -0.08942795157528024563, -0.3641732283464568787 ) ) ;
#43282 = DIRECTION ( 'NONE',  ( -1.734723475976806848E-16, -1.000000000000000000, 0.000000000000000000 ) ) ;
#43283 = CARTESIAN_POINT ( 'NONE',  ( 0.07874015748031558404, -0.1870078740157480601, -0.3641732283464567677 ) ) ;
#43284 = B_SPLINE_CURVE_WITH_KNOTS ( 'NONE', 3,
 ( #27434, #42438, #78388, #53096, #72064, #8094, #59838 ),
 .UNSPECIFIED., .F., .F.,
 ( 4, 3, 4 ),
 ( 1.540743955509788682E-33, 0.001246232571205247927, 0.002492492258783241162 ),
 .UNSPECIFIED. ) ;
#43285 = CARTESIAN_POINT ( 'NONE',  ( -0.5577427821522301654, -0.3162353388693405765, 0.4822834645669290543 ) ) ;
#43286 = EDGE_CURVE ( 'NONE', #28541, #1243, #81014, .T. ) ;
#43287 = CARTESIAN_POINT ( 'NONE',  ( -0.3460692066303957537, -0.1998031496062994405, -0.9166666666666666297 ) ) ;
#43288 = CARTESIAN_POINT ( 'NONE',  ( -0.2867679344610364334, -0.2867679344610367109, -2.348425196850393970 ) ) ;
#43289 = CARTESIAN_POINT ( 'NONE',  ( 0.7939632545931766261, -0.08942795157527998196, 0.3641732283464567121 ) ) ;
#43290 = CARTESIAN_POINT ( 'NONE',  ( -0.4133858267716528645, -0.5400638737290844871, 0.3530559997133364547 ) ) ;
#43291 = CARTESIAN_POINT ( 'NONE',  ( -0.5511811023622038563, -0.1870078740157479769, 0.4822834645669291653 ) ) ;
#43292 = CARTESIAN_POINT ( 'NONE',  ( -0.9317585301837263412, -0.3690944881889765550, -0.3153832671262227771 ) ) ;
#43293 = DIRECTION ( 'NONE',  ( -0.000000000000000000, -1.000000000000000000, -0.000000000000000000 ) ) ;
#43294 = CARTESIAN_POINT ( 'NONE',  ( 0.08530183727034192087, -0.05778040916215522460, 0.4822834645669289988 ) ) ;
#43295 = CARTESIAN_POINT ( 'NONE',  ( -1.043307086614172707, 0.07958543189024071263, -0.2665933059059888421 ) ) ;
#43296 = CARTESIAN_POINT ( 'NONE',  ( -1.489501312335957062, -0.05778040916215522460, 0.4822834645669289988 ) ) ;
#43297 = CARTESIAN_POINT ( 'NONE',  ( -0.2362204724409451284, 0.4091458600556402425, -2.217847769028871596 ) ) ;
#43298 = ORIENTED_EDGE ( 'NONE', *, *, #10620, .F. ) ;
#43299 = CARTESIAN_POINT ( 'NONE',  ( -1.679790026246718693, 0.1283753931104746893, -0.1820866141732285504 ) ) ;
#43300 = CARTESIAN_POINT ( 'NONE',  ( -1.161417322834644716, -0.5400638737290845981, -0.3530559997133363437 ) ) ;
#43301 = CARTESIAN_POINT ( 'NONE',  ( -0.8136482939632537770, -0.6046776061558807314, 0.2411417322834647770 ) ) ;
#43302 = CARTESIAN_POINT ( 'NONE',  ( -1.450131233595799651, 0.2952755905511810774, -0.1292274648535930714 ) ) ;
#43303 = CARTESIAN_POINT ( 'NONE',  ( 0.3392501089628018884, -0.1958661417322834220, -1.449475065616798064 ) ) ;
#43304 = DIRECTION ( 'NONE',  ( 0.000000000000000000, 0.000000000000000000, 1.000000000000000000 ) ) ;
#43305 = CARTESIAN_POINT ( 'NONE',  ( 1.122047244094488860, -0.5400638737290845981, -0.3530559997133363437 ) ) ;
#43306 = CARTESIAN_POINT ( 'NONE',  ( 0.3674540682414705883, -0.6046776061558807314, 0.2411417322834647770 ) ) ;
#43307 = CARTESIAN_POINT ( 'NONE',  ( -1.313877454013331780, 0.2755905511811023723, 0.9174237673981568975 ) ) ;
#43308 = CARTESIAN_POINT ( 'NONE',  ( 0.3996062992125984925, 0.1070741851644054499, -2.248687664041995049 ) ) ;
#43309 = CARTESIAN_POINT ( 'NONE',  ( 1.141732283464567566, 0.1771653543307087630, 0.000000000000000000 ) ) ;
#43310 = CARTESIAN_POINT ( 'NONE',  ( 4.893765752498283924E-17, -0.3996062992125986035, -1.023622047244094446 ) ) ;
#43311 = ORIENTED_EDGE ( 'NONE', *, *, #53064, .T. ) ;
#43312 = CARTESIAN_POINT ( 'NONE',  ( -1.003937007874014853, 0.07958543189024085140, 0.2665933059059887866 ) ) ;
#43313 = CARTESIAN_POINT ( 'NONE',  ( -0.1049643490035302024, -0.3917322834645671215, -2.583989501312335513 ) ) ;
#43314 = ORIENTED_EDGE ( 'NONE', *, *, #75903, .T. ) ;
#43315 = CARTESIAN_POINT ( 'NONE',  ( 0.3346456692913390985, 0.1660481256975885056, 0.3530559997133364547 ) ) ;
#43316 = CARTESIAN_POINT ( 'NONE',  ( -0.3280839895013117347, -0.4281496062992124485, 0.4176697321401328655 ) ) ;
#43317 = CARTESIAN_POINT ( 'NONE',  ( -0.9645669291338575535, 0.1660481256975883668, -0.3530559997133364547 ) ) ;
#43318 = CARTESIAN_POINT ( 'NONE',  ( 0.9317585301837276734, 0.05413385826771626580, -0.4176697321401330321 ) ) ;
#43319 = CARTESIAN_POINT ( 'NONE',  ( 1.541994750656168645, 0.2952755905511810774, -0.1292274648535930714 ) ) ;
#43320 = CARTESIAN_POINT ( 'NONE',  ( 0.07217847769028949700, -0.3162353388693405765, 0.4822834645669290543 ) ) ;
#43321 = CARTESIAN_POINT ( 'NONE',  ( -1.233595800524933894, -0.6046776061558809534, -0.2411417322834644161 ) ) ;
#43322 = CARTESIAN_POINT ( 'NONE',  ( -1.522309711286088607, -0.6046776061558807314, 0.2411417322834647770 ) ) ;
#43323 = CARTESIAN_POINT ( 'NONE',  ( 0.4252607725274244466, 1.326635381343778120, -2.647232528933507467 ) ) ;
#43324 = CARTESIAN_POINT ( 'NONE',  ( 0.3392501089628018884, -0.1958661417322834220, -2.709317585301837195 ) ) ;
#43325 = CARTESIAN_POINT ( 'NONE',  ( 0.8267716535433078384, -0.5511811023622047445, 6.969142054262312111E-17 ) ) ;
#43326 = VERTEX_POINT ( 'NONE', #42681 ) ;
#43327 = CARTESIAN_POINT ( 'NONE',  ( -0.1974969037888706647, 0.3420746716998658843, -0.01312335958005255224 ) ) ;
#43328 = CARTESIAN_POINT ( 'NONE',  ( -0.6627296587926501115, 0.2952755905511810774, -0.1292274648535930714 ) ) ;
#43329 = ORIENTED_EDGE ( 'NONE', *, *, #72867, .T. ) ;
#43330 = CARTESIAN_POINT ( 'NONE',  ( -0.01968503937007793844, -0.4536011799217367080, 0.2665933059059888421 ) ) ;
#43331 = CARTESIAN_POINT ( 'NONE',  ( -1.653543307086613234, -0.1870078740157480879, -0.4822834645669291653 ) ) ;
#43332 = CARTESIAN_POINT ( 'NONE',  ( 0.4396325459317590445, -0.6692913385826771977, 0.1292274648535927661 ) ) ;
#43333 = CARTESIAN_POINT ( 'NONE',  ( 0.4724409448818904789, -0.1870078740157479769, 0.4822834645669291653 ) ) ;
#43334 = CARTESIAN_POINT ( 'NONE',  ( -0.5577427821522301654, -0.05778040916215560624, -0.4822834645669293319 ) ) ;
#43335 = CARTESIAN_POINT ( 'NONE',  ( -0.3917322834645671770, 0.1049643490035302024, -1.131909079561366882 ) ) ;
#43336 = CARTESIAN_POINT ( 'NONE',  ( -1.358267716535432434, -0.5400638737290844871, 0.3530559997133364547 ) ) ;
#43337 = CARTESIAN_POINT ( 'NONE',  ( -0.3392501089628019995, 0.1958661417322832277, -2.788057742782152459 ) ) ;
#43338 = CARTESIAN_POINT ( 'NONE',  ( 1.246719160104987623, -0.3690944881889763329, 0.3153832671262228327 ) ) ;
#43339 = CARTESIAN_POINT ( 'NONE',  ( -1.200787401574802349, -0.5400638737290844871, 0.3530559997133364547 ) ) ;
#43340 = CARTESIAN_POINT ( 'NONE',  ( 1.043307086614173818, 0.1660481256975885056, 0.3530559997133364547 ) ) ;
#43341 = CARTESIAN_POINT ( 'NONE',  ( 1.213910761154856299, 0.2952755905511811885, 0.1292274648535926551 ) ) ;
#43342 = CARTESIAN_POINT ( 'NONE',  ( 0.3996062992125986590, -0.1070741851644053111, -0.8989501312335956840 ) ) ;
#43343 = CARTESIAN_POINT ( 'NONE',  ( -1.259842519685038686, -0.1870078740157479769, 0.4822834645669291653 ) ) ;
#43344 = CARTESIAN_POINT ( 'NONE',  ( 0.1998031496062992463, 0.3460692066303959202, -0.3786089238845143923 ) ) ;
#43345 = CARTESIAN_POINT ( 'NONE',  ( 0.2755905511811031494, -0.6692913385826771977, 8.415575281601705876E-17 ) ) ;
#43346 = CARTESIAN_POINT ( 'NONE',  ( -0.3996062992125986035, -7.340648628747425578E-17, -2.401574803149606474 ) ) ;
#43347 = CARTESIAN_POINT ( 'NONE',  ( -0.3392501089628017219, -0.1958661417322836718, -1.554461942257217899 ) ) ;
#43348 = CARTESIAN_POINT ( 'NONE',  ( -1.620734908136482577, 0.1771653543307087630, 0.09757992244046791164 ) ) ;
#43349 = CARTESIAN_POINT ( 'NONE',  ( 0.5183727034120741983, -0.5511811023622046335, 0.09757992244046803654 ) ) ;
#43350 = CARTESIAN_POINT ( 'NONE',  ( 0.9580052493438326877, 0.05413385826771666132, 0.4176697321401328100 ) ) ;
#43351 = CARTESIAN_POINT ( 'NONE',  ( 0.1265901696524989462, 0.4724409448818897572, -1.172572178477690352 ) ) ;
#43352 = CARTESIAN_POINT ( 'NONE',  ( 0.8070866141732289112, -0.4536011799217368745, -0.2665933059059886201 ) ) ;
#43353 =( BOUNDED_CURVE ( )  B_SPLINE_CURVE ( 2, ( #67890, #36298, #61972, #29567, #10227, #81765, #24075, #50560, #35894, #50154, #4311, #49744, #30804 ),
 .UNSPECIFIED., .F., .T. ) 
 B_SPLINE_CURVE_WITH_KNOTS ( ( 3, 2, 2, 2, 2, 2, 3 ),
 ( 0.3375000000000000222, 0.3416666666666666741, 0.3458333333333333259, 0.3499999999999999778, 0.3541666666666666852, 0.3583333333333333370, 0.3624999999999999889 ),
 .UNSPECIFIED. ) 
 CURVE ( )  GEOMETRIC_REPRESENTATION_ITEM ( )  RATIONAL_B_SPLINE_CURVE ( ( 1.000000000000000000, 0.9659258262890683122, 1.000000000000000000, 0.9659258262890683122, 1.000000000000000000, 0.9659258262890683122, 1.000000000000000000, 0.9659258262890683122, 1.000000000000000000, 0.9659258262890683122, 1.000000000000000000, 0.9659258262890683122, 1.000000000000000000 ) ) 
 REPRESENTATION_ITEM ( '' )  );
#43354 = CARTESIAN_POINT ( 'NONE',  ( 0.4133858267716541968, -0.5400638737290845981, -0.3530559997133363437 ) ) ;
#43355 = VECTOR ( 'NONE', #76173, 39.37007874015748854 ) ;
#43356 = CARTESIAN_POINT ( 'NONE',  ( 0.1974969037888706092, -0.3420746716998660508, -0.7985564304461942875 ) ) ;
#43357 = CARTESIAN_POINT ( 'NONE',  ( -0.6102362204724400829, 0.1660481256975885056, 0.3530559997133364547 ) ) ;
#43358 = CARTESIAN_POINT ( 'NONE',  ( 0.9285414500055708675, 1.724409448818898127, 0.6299212598425202314 ) ) ;
#43359 = CARTESIAN_POINT ( 'NONE',  ( 0.8464566929133865436, 0.07958543189024071263, -0.2665933059059888421 ) ) ;
#43360 = CARTESIAN_POINT ( 'NONE',  ( -0.01312335958005186876, -0.4281496062992124485, 0.4176697321401328655 ) ) ;
#43361 = CARTESIAN_POINT ( 'NONE',  ( 0.1377952755905518245, 0.1012011053420775880, -0.2882089793578256898 ) ) ;
#43363 = EDGE_CURVE ( 'NONE', #3487, #27293, #70527, .T. ) ;
#43362 = CARTESIAN_POINT ( 'NONE',  ( -0.3543307086614165824, -0.6692913385826771977, 8.415575281601705876E-17 ) ) ;
#43364 = CARTESIAN_POINT ( 'NONE',  ( -0.05905511811023545637, 0.07958543189024085140, 0.2665933059059887866 ) ) ;
#43365 = CARTESIAN_POINT ( 'NONE',  ( -2.619388402063342891, 1.366082762360727454, 0.4426340671871359933 ) ) ;
#43366 = CARTESIAN_POINT ( 'NONE',  ( -0.4986876640419942164, -0.6046776061558807314, 0.2411417322834647770 ) ) ;
#43367 = CARTESIAN_POINT ( 'NONE',  ( 0.8267716535433077274, 0.1771653543307087630, 0.000000000000000000 ) ) ;
#43368 = CARTESIAN_POINT ( 'NONE',  ( -0.7535225988626923499, 2.401574803149606474, 0.4915354330708645025 ) ) ;
#43369 = CARTESIAN_POINT ( 'NONE',  ( 4.893765752498283308E-17, -0.3996062992125985480, -1.730314960629921517 ) ) ;
#43370 = CARTESIAN_POINT ( 'NONE',  ( 0.5183727034120741983, -0.6692913385826771977, 0.1292274648535927661 ) ) ;
#43371 = EDGE_CURVE ( 'NONE', #41294, #46160, #71045, .T. ) ;
#43372 = CARTESIAN_POINT ( 'NONE',  ( -0.3917322834645671215, 0.1049643490035301469, -1.442257217847769057 ) ) ;
#43373 = CARTESIAN_POINT ( 'NONE',  ( 1.207349081364829990, 0.1283753931104748280, 0.1820866141732283561 ) ) ;
#43374 = CARTESIAN_POINT ( 'NONE',  ( -1.191111281560509383, -2.567464376874931580E-15, -0.4445507791589072832 ) ) ;
#43375 = CARTESIAN_POINT ( 'NONE',  ( -0.2034120734908131112, -0.5511811023622048555, -0.09757992244046775898 ) ) ;
#43376 = CARTESIAN_POINT ( 'NONE',  ( -0.7939632545931754048, -0.2845877964562159024, 0.3641732283464567677 ) ) ;
#43377 = CARTESIAN_POINT ( 'NONE',  ( -0.4855643044619415427, 0.05413385826771626580, -0.4176697321401330321 ) ) ;
#43378 = CARTESIAN_POINT ( 'NONE',  ( 1.076115485564305141, 0.1283753931104746893, -0.1820866141732285504 ) ) ;
#43379 = CARTESIAN_POINT ( 'NONE',  ( 0.4744094488189011805, 1.537401574803149984, -1.016821367227981998 ) ) ;
#43380 = CARTESIAN_POINT ( 'NONE',  ( 1.581364829396326277, -0.08942795157527998196, 0.3641732283464567121 ) ) ;
#43381 = CARTESIAN_POINT ( 'NONE',  ( 0.2165354330708668673, -0.5400638737290844871, 0.3530559997133364547 ) ) ;
#43382 = CARTESIAN_POINT ( 'NONE',  ( 0.5905511811023629321, 0.2952755905511811885, 0.000000000000000000 ) ) ;
#43383 = EDGE_CURVE ( 'NONE', #59797, #66145, #55716, .T. ) ;
#43384 = CARTESIAN_POINT ( 'NONE',  ( 0.4258029703577317915, 1.326239216270299393, -2.077409958192426132 ) ) ;
#43385 = CARTESIAN_POINT ( 'NONE',  ( 0.3543307086614179147, 0.2952755905511811885, 0.000000000000000000 ) ) ;
#43386 = CARTESIAN_POINT ( 'NONE',  ( -0.1049643490035307020, 0.3917322834645669549, -0.8786089238845143923 ) ) ;
#43387 = CARTESIAN_POINT ( 'NONE',  ( 0.6889763779527566800, -0.5400638737290844871, 0.3530559997133364547 ) ) ;
#43388 = CARTESIAN_POINT ( 'NONE',  ( 0.6889763779527566800, -0.5400638737290844871, 0.3530559997133364547 ) ) ;
#43389 = ADVANCED_FACE ( 'NONE', ( #75927 ), #13835, .T. ) ;
#43390 = CARTESIAN_POINT ( 'NONE',  ( 1.881759016064405099, 2.742776604255995565, -0.5314960629921260393 ) ) ;
#43391 = CARTESIAN_POINT ( 'NONE',  ( 0.4133858267716541968, 0.07958543189024085140, 0.2665933059059887866 ) ) ;
#43392 = CARTESIAN_POINT ( 'NONE',  ( 1.069553805774278832, 0.2952755905511810774, -0.1292274648535930714 ) ) ;
#43393 = CARTESIAN_POINT ( 'NONE',  ( 0.09842519685039434474, -0.4536011799217368745, -0.2665933059059886201 ) ) ;
#43394 = CARTESIAN_POINT ( 'NONE',  ( -0.1771653543307080136, 0.1660481256975883668, -0.3530559997133364547 ) ) ;
#43395 = CARTESIAN_POINT ( 'NONE',  ( 0.3871391076115492380, -0.05778040916215560624, -0.4822834645669293319 ) ) ;
#43396 = CARTESIAN_POINT ( 'NONE',  ( -0.5971128608923877978, -0.6692913385826773087, -0.1292274648535924053 ) ) ;
#43397 = VECTOR ( 'NONE', #30478, 39.37007874015748143 ) ;
#43398 = CARTESIAN_POINT ( 'NONE',  ( -0.4593175853018366950, -0.004921259842519576551, 0.3153832671262227771 ) ) ;
#43399 = CARTESIAN_POINT ( 'NONE',  ( 0.9383202099737536495, -0.3162353388693405765, 0.4822834645669290543 ) ) ;
#43400 = CARTESIAN_POINT ( 'NONE',  ( 1.023622047244095334, -0.1870078740157479769, 0.3641732283464567677 ) ) ;
#43401 = CARTESIAN_POINT ( 'NONE',  ( 0.006561679790026889343, -0.3162353388693409650, -0.4822834645669289433 ) ) ;
#43403 = CARTESIAN_POINT ( 'NONE',  ( -0.3460692066303958092, -0.1998031496062994683, -1.154855643044619518 ) ) ;
#43402 = CARTESIAN_POINT ( 'NONE',  ( 1.220472440944879722, 2.401574803149606474, 0.5309055118110233007 ) ) ;
#43404 = CARTESIAN_POINT ( 'NONE',  ( -0.3836918680457887532, -2.191421614605370878E-15, 0.4445507791589071167 ) ) ;
#43405 = CARTESIAN_POINT ( 'NONE',  ( -0.3392501089628017219, -0.1958661417322836718, -2.249343832020997525 ) ) ;
#43406 = CARTESIAN_POINT ( 'NONE',  ( -1.030183727034119867, -0.3162353388693405765, 0.4822834645669290543 ) ) ;
#43407 = B_SPLINE_CURVE_WITH_KNOTS ( 'NONE', 3,
 ( #25678, #24443, #12653, #11423, #37900, #63576, #38314 ),
 .UNSPECIFIED., .F., .F.,
 ( 4, 3, 4 ),
 ( 3.642919299551295515E-17, 0.001246232571205268744, 0.002492492258783277591 ),
 .UNSPECIFIED. ) ;
#43408 = CARTESIAN_POINT ( 'NONE',  ( -0.7874015748031489847, -0.1870078740157479769, 0.4822834645669291653 ) ) ;
#43409 = CARTESIAN_POINT ( 'NONE',  ( -1.157146581871515012E-16, 0.4724409448818898682, -0.1574803149606299191 ) ) ;
#43410 = CARTESIAN_POINT ( 'NONE',  ( 0.2891555358219910499, 0.2891555358219910499, -2.814960629921259727 ) ) ;
#43411 = ORIENTED_EDGE ( 'NONE', *, *, #51390, .T. ) ;
#43412 = CARTESIAN_POINT ( 'NONE',  ( 0.2690288713910767848, 0.1771653543307087630, 0.09757992244046791164 ) ) ;
#43414 = CARTESIAN_POINT ( 'NONE',  ( -0.1958661417322834220, -0.3392501089628018884, -1.475065616797900381 ) ) ;
#43413 = VECTOR ( 'NONE', #80821, 39.37007874015748143 ) ;
#43415 = CARTESIAN_POINT ( 'NONE',  ( 0.4921259842519691285, 0.1660481256975885056, 0.3530559997133364547 ) ) ;
#43416 = CARTESIAN_POINT ( 'NONE',  ( 0.4724409448818898682, 2.892866454678787531E-17, -2.322834645669291209 ) ) ;
#43417 = CARTESIAN_POINT ( 'NONE',  ( 0.9842519685039375910, 0.2952755905511811885, 0.000000000000000000 ) ) ;
#43418 = ADVANCED_FACE ( 'NONE', ( #18268 ), #38434, .T. ) ;
#43419 = SURFACE_STYLE_FILL_AREA ( #55640 ) ;
#43420 = CARTESIAN_POINT ( 'NONE',  ( 1.371391076115485941, 0.2952755905511811885, 0.1292274648535926551 ) ) ;
#43421 = CARTESIAN_POINT ( 'NONE',  ( 1.502624671916010790, -0.2845877964562161244, -0.3641732283464567121 ) ) ;
#43422 = CARTESIAN_POINT ( 'NONE',  ( -0.08530183727034056085, -0.3162353388693405765, 0.4822834645669290543 ) ) ;
#43423 = CARTESIAN_POINT ( 'NONE',  ( 0.1958661417322836162, -0.3392501089628018329, -0.8018179545593683288 ) ) ;
#43424 = CARTESIAN_POINT ( 'NONE',  ( -0.4002624671916004129, -0.3162353388693405765, 0.4822834645669290543 ) ) ;
#43425 = CARTESIAN_POINT ( 'NONE',  ( -0.8005249343832013809, -0.3690944881889763329, 0.3153832671262228327 ) ) ;
#43426 = CARTESIAN_POINT ( 'NONE',  ( 0.5511811023622054106, -0.1870078740157480879, -0.4822834645669291653 ) ) ;
#43427 = CARTESIAN_POINT ( 'NONE',  ( -0.4855643044619415427, -0.4281496062992124485, 0.4176697321401328655 ) ) ;
#43428 = DIRECTION ( 'NONE',  ( 0.000000000000000000, 1.000000000000000000, 0.000000000000000000 ) ) ;
#43429 = CARTESIAN_POINT ( 'NONE',  ( -0.01706770257043029385, 1.062992125984252967, -1.850393700787401619 ) ) ;
#43430 = ORIENTED_EDGE ( 'NONE', *, *, #43522, .F. ) ;
#43431 = CARTESIAN_POINT ( 'NONE',  ( -0.3917322834645670659, -7.196005306013484475E-17, -2.083352649115172373 ) ) ;
#43432 = CARTESIAN_POINT ( 'NONE',  ( 0.3477690288713918276, -0.6692913385826773087, -0.1292274648535924053 ) ) ;
#43433 = CARTESIAN_POINT ( 'NONE',  ( -0.5183727034120726440, -0.6692913385826773087, -0.1292274648535924053 ) ) ;
#43434 = CARTESIAN_POINT ( 'NONE',  ( -1.627296587926508442, 0.2306618581243848609, 0.2411417322834645549 ) ) ;
#43435 = CARTESIAN_POINT ( 'NONE',  ( 0.6233595800524939223, -0.3162353388693405765, 0.4822834645669290543 ) ) ;
#43436 = CARTESIAN_POINT ( 'NONE',  ( 0.4133858267716541968, 0.1660481256975885056, 0.3530559997133364547 ) ) ;
#43437 = CARTESIAN_POINT ( 'NONE',  ( -0.3392501089628019995, 0.1958661417322832277, -1.213254593175852936 ) ) ;
#43438 = CARTESIAN_POINT ( 'NONE',  ( -0.9645669291338575535, -0.5400638737290844871, 0.3530559997133364547 ) ) ;
#43439 = CARTESIAN_POINT ( 'NONE',  ( 0.1837270341207357105, -0.6046776061558809534, -0.2411417322834644161 ) ) ;
#43440 = CARTESIAN_POINT ( 'NONE',  ( -0.4658792650918627265, -0.3162353388693409650, -0.4822834645669289433 ) ) ;
#43441 = CARTESIAN_POINT ( 'NONE',  ( 0.4593175853018380828, -0.004921259842519870586, -0.3153832671262229437 ) ) ;
#43442 = CARTESIAN_POINT ( 'NONE',  ( -1.679790026246718693, 0.2306618581243847221, -0.2411417322834647770 ) ) ;
#43443 = CARTESIAN_POINT ( 'NONE',  ( -0.2952755905511810774, -0.01200600163628312393, 5.879133660591331356 ) ) ;
#43444 = CARTESIAN_POINT ( 'NONE',  ( 0.03937007874015806264, 0.2952755905511811885, 0.000000000000000000 ) ) ;
#43445 = CARTESIAN_POINT ( 'NONE',  ( 3.909109051758220321, 1.617477308826748228, -0.4678760369123936003 ) ) ;
#43446 = EDGE_CURVE ( 'NONE', #21338, #55552, #51045, .T. ) ;
#43447 = CARTESIAN_POINT ( 'NONE',  ( -1.548556430446193399, -0.6046776061558809534, -0.2411417322834644161 ) ) ;
#43448 = CARTESIAN_POINT ( 'NONE',  ( 0.1049643490035304938, -0.3917322834645669549, -2.912073490813647858 ) ) ;
#43449 = ORIENTED_EDGE ( 'NONE', *, *, #47486, .F. ) ;
#43450 = VERTEX_POINT ( 'NONE', #18671 ) ;
#43451 = CARTESIAN_POINT ( 'NONE',  ( 0.8923884514435703741, 0.2306618581243848609, 0.2411417322834645549 ) ) ;
#43452 = CARTESIAN_POINT ( 'NONE',  ( 0.1181102362204730916, -0.5511811023622047445, 6.969142054262312111E-17 ) ) ;
#43454 = CARTESIAN_POINT ( 'NONE',  ( -1.586052503253847057, 1.574803149606300412, 0.1653254495020574921 ) ) ;
#43453 = CARTESIAN_POINT ( 'NONE',  ( -1.033875059083676939, 1.724409448818897905, 0.4359958488159718093 ) ) ;
#43455 = CARTESIAN_POINT ( 'NONE',  ( 0.2867679344610365999, -0.2867679344610365444, -1.285433070866141669 ) ) ;
#43456 = CARTESIAN_POINT ( 'NONE',  ( -0.9573014326657163231, -2.609869883881465018E-15, -0.3464511005275220379 ) ) ;
#43457 = CARTESIAN_POINT ( 'NONE',  ( 0.3025410870193226964, 2.784432375088962958E-17, -0.3464511005275205946 ) ) ;
#43458 = CARTESIAN_POINT ( 'NONE',  ( 0.2925321140481932369, -0.2925321140481931814, -2.694881889763780070 ) ) ;
#43459 = CARTESIAN_POINT ( 'NONE',  ( 0.6692913385826777528, 0.2952755905511811885, 0.000000000000000000 ) ) ;
#43460 = CARTESIAN_POINT ( 'NONE',  ( -1.292650918635170010, 0.2952755905511810774, -0.1292274648535930714 ) ) ;
#43461 = AXIS2_PLACEMENT_3D ( 'NONE', #1198, #44519, #51250 ) ;
#43462 = CARTESIAN_POINT ( 'NONE',  ( -1.318897637795274802, -0.5400638737290845981, -0.3530559997133363437 ) ) ;
#43463 = CARTESIAN_POINT ( 'NONE',  ( 0.3937007874015754361, -0.1870078740157480879, -0.4822834645669291653 ) ) ;
#43464 = CARTESIAN_POINT ( 'NONE',  ( 1.135170603674541256, 0.2952755905511811885, 0.1292274648535926551 ) ) ;
#43465 = CARTESIAN_POINT ( 'NONE',  ( 1.233595800524935227, 0.1283753931104746893, -0.1820866141732285504 ) ) ;
#43466 = CARTESIAN_POINT ( 'NONE',  ( 1.384514435695538559, 0.1771653543307087075, -0.09757992244046823083 ) ) ;
#43467 = CARTESIAN_POINT ( 'NONE',  ( -0.9908136482939626788, 0.2952755905511811885, 0.1292274648535926551 ) ) ;
#43468 = CARTESIAN_POINT ( 'NONE',  ( 0.1070741851644054776, -0.3996062992125984925, -0.4770341207349080848 ) ) ;
#43469 = CARTESIAN_POINT ( 'NONE',  ( 1.640419947506562393, -0.4281496062992124485, 0.4176697321401328655 ) ) ;
#43470 = EDGE_CURVE ( 'NONE', #27293, #65491, #35339, .T. ) ;
#43471 = CARTESIAN_POINT ( 'NONE',  ( -0.1049643490035302024, -0.3917322834645671215, -0.06430446194225715451 ) ) ;
#43472 = CARTESIAN_POINT ( 'NONE',  ( -0.2099737532808391705, 0.2306618581243848609, 0.2411417322834645549 ) ) ;
#43474 = CARTESIAN_POINT ( 'NONE',  ( 0.5314960629920921775, 2.716535433070866645, 3.224202737261820939 ) ) ;
#43473 = CARTESIAN_POINT ( 'NONE',  ( 1.141732283464567788, -0.6692913385826771977, 8.415575281601705876E-17 ) ) ;
#43475 = CARTESIAN_POINT ( 'NONE',  ( -1.587926509186350810, -0.3690944881889763329, 0.3153832671262228327 ) ) ;
#43476 = CARTESIAN_POINT ( 'NONE',  ( 0.5774278215223104249, 0.2306618581243848609, 0.2411417322834645549 ) ) ;
#43477 = CARTESIAN_POINT ( 'NONE',  ( 0.9186351706036751663, -0.5023911411419708095, 0.1820866141732285504 ) ) ;
#43478 = CARTESIAN_POINT ( 'NONE',  ( -1.377952755905511140, 0.1771653543307087630, 0.000000000000000000 ) ) ;
#43479 = CARTESIAN_POINT ( 'NONE',  ( 0.8070866141732289112, -0.5400638737290845981, -0.3530559997133363437 ) ) ;
#43480 = CARTESIAN_POINT ( 'NONE',  ( -0.5118110236220466680, 0.2952755905511811885, 0.000000000000000000 ) ) ;
#43481 = CARTESIAN_POINT ( 'NONE',  ( -0.5314960629921254842, -0.4536011799217368745, -0.2665933059059886201 ) ) ;
#43482 = CARTESIAN_POINT ( 'NONE',  ( -0.6758530183727028406, -0.6692913385826773087, -0.1292274648535924053 ) ) ;
#43483 = CARTESIAN_POINT ( 'NONE',  ( 1.463254593175853824, -0.6692913385826771977, 0.1292274648535927661 ) ) ;
#43484 = CARTESIAN_POINT ( 'NONE',  ( -0.8398950131233589023, -0.6046776061558809534, -0.2411417322834644161 ) ) ;
#43485 = CARTESIAN_POINT ( 'NONE',  ( 1.568241469816273659, -0.05778040916215560624, -0.4822834645669293319 ) ) ;
#43486 = CARTESIAN_POINT ( 'NONE',  ( 0.1958661417322836718, -0.3392501089628017219, -0.7185232527897132959 ) ) ;
#43487 = CARTESIAN_POINT ( 'NONE',  ( -1.108923884514435132, -0.08942795157528024563, -0.3641732283464568787 ) ) ;
#43488 =( BOUNDED_CURVE ( )  B_SPLINE_CURVE ( 2, ( #31197, #50545, #76249 ),
 .UNSPECIFIED., .F., .F. ) 
 B_SPLINE_CURVE_WITH_KNOTS ( ( 3, 3 ),
 ( 0.4625000000000001332, 0.4631378855240345094 ),
 .UNSPECIFIED. ) 
 CURVE ( )  GEOMETRIC_REPRESENTATION_ITEM ( )  RATIONAL_B_SPLINE_CURVE ( ( 0.9999999999999991118, 0.9947834986831257664, 0.9911642120907997455 ) ) 
 REPRESENTATION_ITEM ( '' )  );
#43489 = CARTESIAN_POINT ( 'NONE',  ( 2.556694656352263006, 1.572145545125845922, 0.4734416007054421116 ) ) ;
#43490 = CARTESIAN_POINT ( 'NONE',  ( 1.397637795275591177, -0.5400638737290844871, 0.3530559997133364547 ) ) ;
#43491 = CARTESIAN_POINT ( 'NONE',  ( 0.4724409448818897572, -0.1265901696524988906, -1.920603674540682038 ) ) ;
#43492 = CARTESIAN_POINT ( 'NONE',  ( -0.08983781461629233855, 1.809133623825372073E-16, -0.3954985857520062487 ) ) ;
#43493 = CARTESIAN_POINT ( 'NONE',  ( -1.541994750656167090, -0.5511811023622048555, -0.09757992244046775898 ) ) ;
#43494 = CARTESIAN_POINT ( 'NONE',  ( -0.4724409448818890911, -0.1870078740157479769, 0.3641732283464567677 ) ) ;
#43495 = CARTESIAN_POINT ( 'NONE',  ( -1.587926509186350810, 0.05413385826771626580, -0.4176697321401330321 ) ) ;
#43496 = CARTESIAN_POINT ( 'NONE',  ( -0.5314960629921250401, 0.1660481256975885056, 0.3530559997133364547 ) ) ;
#43497 = CARTESIAN_POINT ( 'NONE',  ( 0.06561679790026316017, -0.3690944881889763329, 0.3153832671262228327 ) ) ;
#43498 = CARTESIAN_POINT ( 'NONE',  ( -1.108923884514435132, -0.2845877964562159024, 0.3641732283464567677 ) ) ;
#43499 = CARTESIAN_POINT ( 'NONE',  ( 1.456692913385827515, 0.1771653543307087630, 0.000000000000000000 ) ) ;
#43500 = CARTESIAN_POINT ( 'NONE',  ( 0.9186351706036752773, 0.2306618581243847221, -0.2411417322834647770 ) ) ;
#43501 = LINE ( 'NONE', #25805, #78419 ) ;
#43502 = CARTESIAN_POINT ( 'NONE',  ( 0.5577427821522316087, -0.08942795157527998196, 0.3641732283464567121 ) ) ;
#43503 = CARTESIAN_POINT ( 'NONE',  ( 0.2624671916010504757, 0.2306618581243848609, 0.2411417322834645549 ) ) ;
#43504 = CARTESIAN_POINT ( 'NONE',  ( 0.8136482939632553313, 0.1283753931104748280, 0.1820866141732283561 ) ) ;
#43505 = EDGE_LOOP ( 'NONE', ( #27726, #39100, #6529, #75981 ) ) ;
#43506 = CARTESIAN_POINT ( 'NONE',  ( -1.417322834645668772, -0.1870078740157480879, -0.4822834645669291653 ) ) ;
#43507 = CARTESIAN_POINT ( 'NONE',  ( -1.266404199475064773, -0.05778040916215560624, -0.4822834645669293319 ) ) ;
#43508 = CARTESIAN_POINT ( 'NONE',  ( -0.09842519685039295696, 0.1660481256975883668, -0.3530559997133364547 ) ) ;
#43509 = CARTESIAN_POINT ( 'NONE',  ( -2.152711368484068188, 1.622209144264166847, -0.4670403427556032994 ) ) ;
#43510 = CARTESIAN_POINT ( 'NONE',  ( 0.3460692066303958092, 0.1998031496062993018, -2.570209973753280863 ) ) ;
#43511 = CARTESIAN_POINT ( 'NONE',  ( 0.6496062992125991586, 0.1660481256975885056, 0.3530559997133364547 ) ) ;
#43512 = CARTESIAN_POINT ( 'NONE',  ( 1.450131233595801428, 0.1771653543307087630, 0.09757992244046791164 ) ) ;
#43513 = CARTESIAN_POINT ( 'NONE',  ( -0.1443569553805765515, -0.4281496062992127816, -0.4176697321401328100 ) ) ;
#43514 = CARTESIAN_POINT ( 'NONE',  ( 0.5380577427821529035, 0.05413385826771626580, -0.4176697321401330321 ) ) ;
#43515 = ADVANCED_FACE ( 'NONE', ( #30878 ), #5406, .F. ) ;
#43516 = CARTESIAN_POINT ( 'NONE',  ( -0.2925321140481930704, -0.2925321140481933480, -2.106299212598425452 ) ) ;
#43517 = CARTESIAN_POINT ( 'NONE',  ( -0.3949938075777409963, -7.255918531996591613E-17, -1.614173228346456934 ) ) ;
#43518 = CARTESIAN_POINT ( 'NONE',  ( 0.1998031496062992740, 0.3460692066303959757, -2.821522309711286258 ) ) ;
#43519 = FACE_OUTER_BOUND ( 'NONE', #53478, .T. ) ;
#43520 = AXIS2_PLACEMENT_3D ( 'NONE', #59099, #57832, #70060 ) ;
#43521 = CARTESIAN_POINT ( 'NONE',  ( -0.3917322834645671215, 0.1049643490035301469, -0.8123359580052490481 ) ) ;
#43522 = EDGE_CURVE ( 'NONE', #78156, #895, #366, .T. ) ;
#43523 = CARTESIAN_POINT ( 'NONE',  ( -0.4593175853018366950, -0.004921259842519576551, 0.3153832671262227771 ) ) ;
#43524 = CARTESIAN_POINT ( 'NONE',  ( -0.7480314960629914633, 0.2952755905511811885, 0.000000000000000000 ) ) ;
#43525 = CARTESIAN_POINT ( 'NONE',  ( 0.2887139107611556010, -0.6046776061558807314, 0.2411417322834647770 ) ) ;
#43526 = CARTESIAN_POINT ( 'NONE',  ( -0.3949938075777409963, -7.255918531996591613E-17, -2.635826771653543954 ) ) ;
#43527 = CARTESIAN_POINT ( 'NONE',  ( 0.7874015748031503170, -0.1870078740157480879, -0.4822834645669291653 ) ) ;
#43528 = CARTESIAN_POINT ( 'NONE',  ( 1.522309711286089939, -0.6046776061558809534, -0.2411417322834644161 ) ) ;
#43529 = CARTESIAN_POINT ( 'NONE',  ( 0.7283464566929140904, -0.5400638737290845981, -0.3530559997133363437 ) ) ;
#43530 = CARTESIAN_POINT ( 'NONE',  ( 0.4724409448818898682, 2.892866454678787531E-17, -2.795275590551181022 ) ) ;
#43531 = CARTESIAN_POINT ( 'NONE',  ( 0.2925321140481932369, 0.2925321140481932369, -2.027559055118109743 ) ) ;
#43532 = CARTESIAN_POINT ( 'NONE',  ( 1.476377952755906442, -0.5400638737290844871, 0.3530559997133364547 ) ) ;
#43533 = CARTESIAN_POINT ( 'NONE',  ( 0.8005249343832027131, 0.05413385826771666132, 0.4176697321401328100 ) ) ;
#43534 = CARTESIAN_POINT ( 'NONE',  ( 0.5839895013123367340, -0.6692913385826773087, -0.1292274648535924053 ) ) ;
#43535 = CIRCLE ( 'NONE', #54305, 0.5118110236220471121 ) ;
#43536 = CARTESIAN_POINT ( 'NONE',  ( 1.043307086614173818, -0.4536011799217368745, -0.2665933059059886201 ) ) ;
#43538 = CARTESIAN_POINT ( 'NONE',  ( 1.522309711286089939, -0.6046776061558809534, -0.2411417322834644161 ) ) ;
#43537 = CARTESIAN_POINT ( 'NONE',  ( -1.646981627296586703, -0.08942795157527998196, 0.3641732283464567121 ) ) ;
#43539 = CARTESIAN_POINT ( 'NONE',  ( 0.3917322834645670104, 2.398668435337828261E-17, -0.2027559055118111353 ) ) ;
#43540 = FACE_OUTER_BOUND ( 'NONE', #56500, .T. ) ;
#43541 = CARTESIAN_POINT ( 'NONE',  ( 0.8464566929133866546, -0.5400638737290844871, 0.3530559997133364547 ) ) ;
#43542 = CARTESIAN_POINT ( 'NONE',  ( 1.482939632545932307, -0.3690944881889763329, 0.3153832671262228327 ) ) ;
#43543 = CARTESIAN_POINT ( 'NONE',  ( -0.5577427821522301654, -0.05778040916215560624, -0.4822834645669293319 ) ) ;
#43544 = CARTESIAN_POINT ( 'NONE',  ( -0.8923884514435688198, 0.2306618581243847221, -0.2411417322834647770 ) ) ;
#43545 = CARTESIAN_POINT ( 'NONE',  ( 1.076115485564305141, -0.6046776061558807314, 0.2411417322834647770 ) ) ;
#43546 = CARTESIAN_POINT ( 'NONE',  ( -0.1049643490035307020, 0.3917322834645669549, -0.4061679790026246351 ) ) ;
#43547 = CARTESIAN_POINT ( 'NONE',  ( 0.3917322834645670104, -0.1049643490035303411, -1.363517060367453793 ) ) ;
#43548 = CARTESIAN_POINT ( 'NONE',  ( 0.1958661417322834775, 0.3392501089628018884, -2.813648293963254776 ) ) ;
#43549 = CARTESIAN_POINT ( 'NONE',  ( 1.607611548556431069, -0.6692913385826773087, -0.1292274648535924053 ) ) ;
#43550 = ORIENTED_EDGE ( 'NONE', *, *, #30143, .T. ) ;
#43551 = CARTESIAN_POINT ( 'NONE',  ( -0.3949938075777409408, -0.1058382717557502933, -2.880577427821522374 ) ) ;
#43552 = VERTEX_POINT ( 'NONE', #24801 ) ;
#43553 = DIRECTION ( 'NONE',  ( 0.000000000000000000, 0.000000000000000000, 1.000000000000000000 ) ) ;
#43554 = CARTESIAN_POINT ( 'NONE',  ( 1.509186351706037543, -0.3690944881889765550, -0.3153832671262227771 ) ) ;
#43555 = CARTESIAN_POINT ( 'NONE',  ( 0.1070741851644053527, 0.3996062992125986590, -1.253280839895013044 ) ) ;
#43556 = CARTESIAN_POINT ( 'NONE',  ( 0.000000000000000000, 0.000000000000000000, -2.755905511811024056 ) ) ;
#43557 = CARTESIAN_POINT ( 'NONE',  ( -0.5314960629921323676, 2.729664787007372695, 1.840814861705235783 ) ) ;
#43558 = DIRECTION ( 'NONE',  ( 0.000000000000000000, -1.000000000000000000, 0.000000000000000000 ) ) ;
#43559 = CARTESIAN_POINT ( 'NONE',  ( 0.000000000000000000, 2.716535433070866645, 0.000000000000000000 ) ) ;
#43560 = CARTESIAN_POINT ( 'NONE',  ( 0.2867679344610365999, 0.2867679344610365999, -0.5374015748031496509 ) ) ;
#43561 = CARTESIAN_POINT ( 'NONE',  ( -0.8989501312335946848, -0.5511811023622046335, 0.09757992244046803654 ) ) ;
#43562 = CARTESIAN_POINT ( 'NONE',  ( -1.200787401574802349, 0.07958543189024071263, -0.2665933059059888421 ) ) ;
#43563 = CARTESIAN_POINT ( 'NONE',  ( -1.272965879265091305, 0.05413385826771626580, -0.4176697321401330321 ) ) ;
#43564 = CARTESIAN_POINT ( 'NONE',  ( -0.1049868766404193215, 0.2306618581243847221, -0.2411417322834647770 ) ) ;
#43565 = CARTESIAN_POINT ( 'NONE',  ( -1.391076115485563314, -0.6046776061558809534, -0.2411417322834644161 ) ) ;
#43566 = EDGE_LOOP ( 'NONE', ( #631, #82072, #31838, #53075 ) ) ;
#43567 = CARTESIAN_POINT ( 'NONE',  ( 1.614173228346457378, 0.2952755905511811885, 0.000000000000000000 ) ) ;
#43568 = CARTESIAN_POINT ( 'NONE',  ( -1.148293963254592542, 0.2066929133858267931, 0.1054918080437490802 ) ) ;
#43569 = CARTESIAN_POINT ( 'NONE',  ( 0.4724409448818896462, 0.1265901696524990294, -2.171916010498687211 ) ) ;
#43570 = LINE ( 'NONE', #69271, #3546 ) ;
#43571 = CARTESIAN_POINT ( 'NONE',  ( -0.3674540682414689785, 0.1283753931104748280, 0.1820866141732283561 ) ) ;
#43572 = CARTESIAN_POINT ( 'NONE',  ( -1.082677165354329896, -0.5400638737290845981, -0.3530559997133363437 ) ) ;
#43573 = CARTESIAN_POINT ( 'NONE',  ( 1.141732283464567788, -0.6692913385826771977, 8.415575281601705876E-17 ) ) ;
#43574 = ORIENTED_EDGE ( 'NONE', *, *, #50670, .F. ) ;
#43576 = PLANE ( 'NONE',  #70737 ) ;
#43575 = DIRECTION ( 'NONE',  ( -1.408710688920637755E-15, 1.000000000000000000, -4.918487082195260922E-30 ) ) ;
#43577 = CARTESIAN_POINT ( 'NONE',  ( 1.679790026246720025, 0.2306618581243848609, 0.2411417322834645549 ) ) ;
#43578 = CARTESIAN_POINT ( 'NONE',  ( -1.194225721784776262, 0.05413385826771626580, -0.4176697321401330321 ) ) ;
#43579 = CARTESIAN_POINT ( 'NONE',  ( -0.3392501089628018329, -0.1958661417322836440, -0.2900069309373210502 ) ) ;
#43580 = CARTESIAN_POINT ( 'NONE',  ( -0.03280839895013062252, -0.5511811023622046335, 0.09757992244046803654 ) ) ;
#43581 = CARTESIAN_POINT ( 'NONE',  ( -0.1049643490035301885, -0.3917322834645671215, -0.7867454068241470644 ) ) ;
#43582 = CIRCLE ( 'NONE', #14058, 0.3149606299212597271 ) ;
#43583 = CARTESIAN_POINT ( 'NONE',  ( 0.07874015748031558404, -0.1870078740157479769, 0.3641732283464567677 ) ) ;
#43584 = CARTESIAN_POINT ( 'NONE',  ( 0.3937007874015754361, -0.1870078740157480601, -0.3641732283464567677 ) ) ;
#43585 = CARTESIAN_POINT ( 'NONE',  ( 0.4461942257217855201, -0.6046776061558807314, 0.2411417322834647770 ) ) ;
#43586 = CARTESIAN_POINT ( 'NONE',  ( -0.7677165354330699465, -0.4536011799217368745, -0.2665933059059886201 ) ) ;
#43587 = CARTESIAN_POINT ( 'NONE',  ( 4.797336870675656522E-17, -0.3917322834645670104, -2.590551181102362044 ) ) ;
#43588 = CARTESIAN_POINT ( 'NONE',  ( 1.358267716535433323, -0.5400638737290845981, -0.3530559997133363437 ) ) ;
#43589 = CARTESIAN_POINT ( 'NONE',  ( -1.076115485564303809, -0.6046776061558809534, -0.2411417322834644161 ) ) ;
#43590 = CARTESIAN_POINT ( 'NONE',  ( 0.1265901696524990294, -0.4724409448818896462, -0.9494750656167976199 ) ) ;
#43591 = CARTESIAN_POINT ( 'NONE',  ( 0.1246719160104994284, -0.6692913385826771977, 0.1292274648535927661 ) ) ;
#43592 = CARTESIAN_POINT ( 'NONE',  ( -0.5839895013123351797, -0.6692913385826771977, 0.1292274648535927661 ) ) ;
#43593 = CARTESIAN_POINT ( 'NONE',  ( 1.128608923884515169, -0.5023911411419708095, -0.1820866141732282451 ) ) ;
#43594 = CARTESIAN_POINT ( 'NONE',  ( -0.07217847769028813698, -0.2845877964562161244, -0.3641732283464567121 ) ) ;
#43595 = CARTESIAN_POINT ( 'NONE',  ( -0.3412073490813641308, -0.6046776061558807314, 0.2411417322834647770 ) ) ;
#43596 = CARTESIAN_POINT ( 'NONE',  ( -1.003937007874014853, 0.1660481256975885056, 0.3530559997133364547 ) ) ;
#43597 = CARTESIAN_POINT ( 'NONE',  ( 1.595398199321655275, 0.7375059713363275593, -0.1559797534342494130 ) ) ;
#43598 = CARTESIAN_POINT ( 'NONE',  ( 1.568241469816273659, -0.08942795157528024563, -0.3641732283464568787 ) ) ;
#43599 = CARTESIAN_POINT ( 'NONE',  ( -0.2034120734908128059, 0.2952755905511811885, 0.1292274648535926551 ) ) ;
#43600 = CARTESIAN_POINT ( 'NONE',  ( -1.095800524934382292, -0.05778040916215522460, 0.4822834645669289988 ) ) ;
#43601 = VERTEX_POINT ( 'NONE', #49655 ) ;
#43602 = CARTESIAN_POINT ( 'NONE',  ( 0.3460692066303958092, 0.1998031496062993018, -2.097769028871391050 ) ) ;
#43603 = CARTESIAN_POINT ( 'NONE',  ( 1.049868766404200127, -0.6046776061558809534, -0.2411417322834644161 ) ) ;
#43604 = CARTESIAN_POINT ( 'NONE',  ( -0.5708661417322828946, 0.07958543189024071263, -0.2665933059059888421 ) ) ;
#43605 = CARTESIAN_POINT ( 'NONE',  ( -0.4986876640419942164, -0.6046776061558807314, 0.2411417322834647770 ) ) ;
#43606 = CARTESIAN_POINT ( 'NONE',  ( 1.469816272965879911, -0.6046776061558807314, 0.2411417322834647770 ) ) ;
#43607 = CARTESIAN_POINT ( 'NONE',  ( 0.8923884514435703741, 0.2306618581243848609, 0.2411417322834645549 ) ) ;
#43608 = CARTESIAN_POINT ( 'NONE',  ( -1.437007874015747477, 0.1660481256975883668, -0.3530559997133364547 ) ) ;
#43609 = CARTESIAN_POINT ( 'NONE',  ( -0.9580052493438311334, -0.3690944881889763329, 0.3153832671262228327 ) ) ;
#43611 = ADVANCED_FACE ( 'NONE', ( #23572 ), #69845, .F. ) ;
#43610 = CARTESIAN_POINT ( 'NONE',  ( 0.2925321140481931814, 0.2925321140481931814, -0.5295275590551181688 ) ) ;
#43612 = CARTESIAN_POINT ( 'NONE',  ( -0.1070741851644056997, 0.3996062992125986035, -0.9514435695538056015 ) ) ;
#43613 = CARTESIAN_POINT ( 'NONE',  ( 0.1058382717557500713, -0.3949938075777409408, -0.4002624671916010235 ) ) ;
#43614 = CARTESIAN_POINT ( 'NONE',  ( 0.2405914015988345200, 1.128524939042355069, -1.573041762559489687 ) ) ;
#43615 = CARTESIAN_POINT ( 'NONE',  ( 1.167979002624672580, -0.3690944881889763329, 0.3153832671262228327 ) ) ;
#43616 = CARTESIAN_POINT ( 'NONE',  ( 0.6496062992125991586, 0.07958543189024085140, 0.2665933059059887866 ) ) ;
#43617 = CARTESIAN_POINT ( 'NONE',  ( 0.5511811023622054106, -0.1870078740157480879, -0.4822834645669291653 ) ) ;
#43618 = FACE_OUTER_BOUND ( 'NONE', #18486, .T. ) ;
#43619 = CARTESIAN_POINT ( 'NONE',  ( 0.3949938075777408852, 0.1058382717557500435, -1.461286089238844843 ) ) ;
#43620 = CARTESIAN_POINT ( 'NONE',  ( 1.010498687664042716, -0.3690944881889763329, 0.3153832671262228327 ) ) ;
#43621 = CARTESIAN_POINT ( 'NONE',  ( -0.3477690288713902178, 0.2952755905511810774, -0.1292274648535930714 ) ) ;
#43622 = CARTESIAN_POINT ( 'NONE',  ( -0.8202099737532799750, 0.2952755905511810774, -0.1292274648535930714 ) ) ;
#43623 = CARTESIAN_POINT ( 'NONE',  ( 1.194225721784777594, 0.05413385826771666132, 0.4176697321401328100 ) ) ;
#43624 = CARTESIAN_POINT ( 'NONE',  ( 0.3458507752293908943, -0.3458507752293908943, -1.043307086614173151 ) ) ;
#43625 = CARTESIAN_POINT ( 'NONE',  ( -0.03280839895013062252, -0.5511811023622046335, 0.09757992244046803654 ) ) ;
#43626 = EDGE_LOOP ( 'NONE', ( #16681, #41506, #57184, #37740, #1124, #65059, #10125 ) ) ;
#43627 = ORIENTED_EDGE ( 'NONE', *, *, #3457, .T. ) ;
#43628 = CARTESIAN_POINT ( 'NONE',  ( -0.9448818897637790704, -0.1870078740157479769, 0.4822834645669291653 ) ) ;
#43629 = CARTESIAN_POINT ( 'NONE',  ( -0.3215223097112853146, -0.05778040916215560624, -0.4822834645669293319 ) ) ;
#43630 = CARTESIAN_POINT ( 'NONE',  ( -0.4068241469816264999, -0.4281496062992124485, 0.4176697321401328655 ) ) ;
#43631 = AXIS2_PLACEMENT_3D ( 'NONE', #63354, #57024, #6103 ) ;
#43632 = CARTESIAN_POINT ( 'NONE',  ( 0.5052493438320218022, -0.6692913385826773087, -0.1292274648535924053 ) ) ;
#43633 = CARTESIAN_POINT ( 'NONE',  ( -0.4724409448818890911, -0.1870078740157480879, -0.4822834645669291653 ) ) ;
#43634 = CARTESIAN_POINT ( 'NONE',  ( -1.496062992125983815, -0.1870078740157479769, 0.4822834645669291653 ) ) ;
#43635 = CARTESIAN_POINT ( 'NONE',  ( -0.9645669291338575535, -0.5400638737290844871, 0.3530559997133364547 ) ) ;
#43636 = CARTESIAN_POINT ( 'NONE',  ( 0.7283464566929140904, -0.5400638737290845981, -0.3530559997133363437 ) ) ;
#43637 = CARTESIAN_POINT ( 'NONE',  ( -0.3392501089628017219, -0.1958661417322836718, -0.9895013123359579499 ) ) ;
#43638 = CARTESIAN_POINT ( 'NONE',  ( -0.2034120734908128059, 0.1771653543307087630, 0.09757992244046791164 ) ) ;
#43639 = ORIENTED_EDGE ( 'NONE', *, *, #31494, .F. ) ;
#43640 = CARTESIAN_POINT ( 'NONE',  ( -0.3949938075777409963, -7.255918531996591613E-17, -1.299212598425196985 ) ) ;
#43641 = VERTEX_POINT ( 'NONE', #5050 ) ;
#43642 = CARTESIAN_POINT ( 'NONE',  ( -1.141732283464566011, -0.5511811023622047445, 6.969142054262312111E-17 ) ) ;
#43643 = CARTESIAN_POINT ( 'NONE',  ( -0.8792650918635160906, -0.4281496062992124485, 0.4176697321401328655 ) ) ;
#43644 = CARTESIAN_POINT ( 'NONE',  ( -0.9842519685039360366, 0.2952755905511811885, 0.000000000000000000 ) ) ;
#43645 = CARTESIAN_POINT ( 'NONE',  ( 0.1998031496062994405, -0.3460692066303958092, -0.2493438320209973857 ) ) ;
#43646 = CARTESIAN_POINT ( 'NONE',  ( -0.6364829396325453192, -0.3162353388693405765, 0.4822834645669290543 ) ) ;
#43647 = CARTESIAN_POINT ( 'NONE',  ( -0.9055118110236215490, 0.2952755905511811885, 0.000000000000000000 ) ) ;
#43648 = DIRECTION ( 'NONE',  ( -3.096699300667737957E-16, 1.000000000000000000, -0.000000000000000000 ) ) ;
#43649 = CARTESIAN_POINT ( 'NONE',  ( -0.7137454485294953965, 2.001539355558159983, -0.4917280318828584074 ) ) ;
#43650 = CIRCLE ( 'NONE', #10108, 3.858267716535433323 ) ;
#43651 = CARTESIAN_POINT ( 'NONE',  ( 0.4199475065616805614, 0.1283753931104748280, 0.1820866141732283561 ) ) ;
#43652 = CARTESIAN_POINT ( 'NONE',  ( 0.000000000000000000, 0.5905511811023621549, 0.000000000000000000 ) ) ;
#43653 = CARTESIAN_POINT ( 'NONE',  ( -0.1049643490035302024, -0.3917322834645671215, -0.1568241469816273603 ) ) ;
#43654 = CARTESIAN_POINT ( 'NONE',  ( -0.1246719160104980823, 0.1771653543307087630, 0.09757992244046791164 ) ) ;
#43655 = CARTESIAN_POINT ( 'NONE',  ( -0.2034120734908128059, 0.2952755905511811885, 0.1292274648535926551 ) ) ;
#43656 = CARTESIAN_POINT ( 'NONE',  ( 1.174540682414699111, -0.05778040916215560624, -0.4822834645669293319 ) ) ;
#43657 = CARTESIAN_POINT ( 'NONE',  ( -0.2099737532808391705, 0.2306618581243848609, 0.2411417322834645549 ) ) ;
#43658 = ORIENTED_EDGE ( 'NONE', *, *, #67228, .F. ) ;
#43659 = CARTESIAN_POINT ( 'NONE',  ( -0.1070741851644056997, 0.3996062992125986035, -2.211286089238845065 ) ) ;
#43660 = CARTESIAN_POINT ( 'NONE',  ( 0.000000000000000000, 2.755905511811024056, 0.000000000000000000 ) ) ;
#43661 = EDGE_LOOP ( 'NONE', ( #9835, #5559, #44801, #11696 ) ) ;
#43662 = CARTESIAN_POINT ( 'NONE',  ( 0.3996062992125986035, -0.1070741851644052972, -1.763123359580051952 ) ) ;
#43663 = PLANE ( 'NONE',  #47578 ) ;
#43664 = CARTESIAN_POINT ( 'NONE',  ( -1.049868766404198794, 0.1283753931104746893, -0.1820866141732285504 ) ) ;
#43665 = CARTESIAN_POINT ( 'NONE',  ( -1.541994750656167090, 0.2952755905511811885, 0.1292274648535926551 ) ) ;
#43666 = CARTESIAN_POINT ( 'NONE',  ( 0.1265901696524990294, -0.4724409448818896462, -0.4002624671916010235 ) ) ;
#43667 = DIRECTION ( 'NONE',  ( 0.000000000000000000, -1.000000000000000000, 0.000000000000000000 ) ) ;
#43668 = CARTESIAN_POINT ( 'NONE',  ( -0.1958661417322836718, 0.3392501089628017219, -0.005249343832020950465 ) ) ;
#43669 = CARTESIAN_POINT ( 'NONE',  ( 1.456692913385827515, -0.6692913385826771977, 8.415575281601705876E-17 ) ) ;
#43670 = CARTESIAN_POINT ( 'NONE',  ( 0.3805774278215230400, 0.05413385826771626580, -0.4176697321401330321 ) ) ;
#43671 = CARTESIAN_POINT ( 'NONE',  ( 0.2099737532808405305, -0.6046776061558807314, 0.2411417322834647770 ) ) ;
#43672 = CARTESIAN_POINT ( 'NONE',  ( -0.9973753280839886548, 0.1283753931104748280, 0.1820866141732283561 ) ) ;
#43673 = CARTESIAN_POINT ( 'NONE',  ( -0.2099737532808391705, -0.6046776061558809534, -0.2411417322834644161 ) ) ;
#43674 = CARTESIAN_POINT ( 'NONE',  ( -0.3458507752293909498, 0.3458507752293907833, -2.143700787401574548 ) ) ;
#43675 = CARTESIAN_POINT ( 'NONE',  ( -0.9055118110236215490, 0.2952755905511811885, 0.000000000000000000 ) ) ;
#43676 = CARTESIAN_POINT ( 'NONE',  ( 4.837279021331061486E-17, -0.3949938075777409963, -2.360236220472441193 ) ) ;
#43677 = CARTESIAN_POINT ( 'NONE',  ( 1.233595800524935227, -0.5023911411419708095, 0.1820866141732285504 ) ) ;
#43678 = CARTESIAN_POINT ( 'NONE',  ( -0.1706036745406816491, -0.3690944881889763329, 0.3153832671262228327 ) ) ;
#43679 = CARTESIAN_POINT ( 'NONE',  ( 1.102362204724410155, -0.1870078740157480601, -0.3641732283464567677 ) ) ;
#43680 = CARTESIAN_POINT ( 'NONE',  ( -1.555118110236219930, 0.1660481256975885056, 0.3530559997133364547 ) ) ;
#43681 = CARTESIAN_POINT ( 'NONE',  ( -1.010498687664041384, -0.004921259842519576551, 0.3153832671262227771 ) ) ;
#43682 = CARTESIAN_POINT ( 'NONE',  ( -0.9881811337016640495, 2.559055118110236560, 0.5314960629921260393 ) ) ;
#43683 = CARTESIAN_POINT ( 'NONE',  ( 0.3543307086614181922, -0.5511811023622047445, 6.969142054262312111E-17 ) ) ;
#43684 = CARTESIAN_POINT ( 'NONE',  ( -0.4921259842519677963, 0.1660481256975883668, -0.3530559997133364547 ) ) ;
#43685 = CARTESIAN_POINT ( 'NONE',  ( 0.2952755905511819101, 0.1660481256975883391, -0.3530559997133364547 ) ) ;
#43686 = CARTESIAN_POINT ( 'NONE',  ( -0.05905511811023545637, 0.07958543189024085140, 0.2665933059059887866 ) ) ;
#43687 = CARTESIAN_POINT ( 'NONE',  ( -0.2362204724409451284, 0.4091458600556402425, -1.034776902887139194 ) ) ;
#43688 = CARTESIAN_POINT ( 'NONE',  ( 0.7217847769028878924, 0.05413385826771666132, 0.4176697321401328100 ) ) ;
#43689 = LINE ( 'NONE', #50424, #46521 ) ;
#43690 = CARTESIAN_POINT ( 'NONE',  ( 1.489501312335958172, -0.08942795157528024563, -0.3641732283464568787 ) ) ;
#43691 = CARTESIAN_POINT ( 'NONE',  ( -1.135170603674539924, -0.6692913385826771977, 0.1292274648535927661 ) ) ;
#43692 = CARTESIAN_POINT ( 'NONE',  ( -0.1181102362204717315, -0.5511811023622047445, 6.969142054262312111E-17 ) ) ;
#43693 = LINE ( 'NONE', #5008, #24665 ) ;
#43694 = CARTESIAN_POINT ( 'NONE',  ( 0.2099737532808405305, 0.1283753931104746893, -0.1820866141732285504 ) ) ;
#43695 = CARTESIAN_POINT ( 'NONE',  ( -1.036745406824146176, 0.05413385826771626580, -0.4176697321401330321 ) ) ;
#43696 = CARTESIAN_POINT ( 'NONE',  ( -0.3740157480314953431, 0.1660481256975885056, 0.3530559997133364547 ) ) ;
#43697 = CARTESIAN_POINT ( 'NONE',  ( -0.2925321140481930149, -0.2925321140481933480, -0.6082677165354329896 ) ) ;
#43698 = EDGE_CURVE ( 'NONE', #19860, #38268, #37030, .T. ) ;
#43699 = CARTESIAN_POINT ( 'NONE',  ( 0.1049643490035303689, 0.3917322834645670104, -2.282808398950130879 ) ) ;
#43700 = CARTESIAN_POINT ( 'NONE',  ( 0.6758530183727039509, 0.1771653543307087075, -0.09757992244046823083 ) ) ;
#43701 = CARTESIAN_POINT ( 'NONE',  ( -0.3412073490813641308, 0.2306618581243847221, -0.2411417322834647770 ) ) ;
#43702 = TOROIDAL_SURFACE ( 'NONE', #34367, 0.1574803149606295860, 0.01968503937007873988 ) ;
#43703 = CARTESIAN_POINT ( 'NONE',  ( -0.7020997375328074108, -0.05778040916215522460, 0.4822834645669289988 ) ) ;
#43704 = CARTESIAN_POINT ( 'NONE',  ( -0.9842519685039360366, 0.1771653543307087630, 0.000000000000000000 ) ) ;
#43705 = CARTESIAN_POINT ( 'NONE',  ( -3.911274423169837089, 1.384680224527505166, 0.4494265461045906518 ) ) ;
#43706 = CARTESIAN_POINT ( 'NONE',  ( -0.2034120734908128059, 0.2952755905511811885, 0.1292274648535926551 ) ) ;
#43707 = DIRECTION ( 'NONE',  ( -3.096699300667737957E-16, 1.000000000000000000, -0.000000000000000000 ) ) ;
#43708 = CARTESIAN_POINT ( 'NONE',  ( -1.437007874015747477, 0.1660481256975883668, -0.3530559997133364547 ) ) ;
#43709 = CARTESIAN_POINT ( 'NONE',  ( -3.250800430253136586, 2.742781091603911925, 0.5314960629921260393 ) ) ;
#43710 = EDGE_CURVE ( 'NONE', #17817, #57422, #31293, .T. ) ;
#43711 = ORIENTED_EDGE ( 'NONE', *, *, #76884, .T. ) ;
#43712 = CARTESIAN_POINT ( 'NONE',  ( -1.614173228346456712, 2.401574803149606474, -0.1372047244094478091 ) ) ;
#43713 = CARTESIAN_POINT ( 'NONE',  ( -1.423884514435694859, -0.3162353388693405765, 0.4822834645669290543 ) ) ;
#43714 = CARTESIAN_POINT ( 'NONE',  ( -0.7611548556430438595, 0.2306618581243848609, 0.2411417322834645549 ) ) ;
#43715 = CARTESIAN_POINT ( 'NONE',  ( 1.555118110236221041, -0.5400638737290844871, 0.3530559997133364547 ) ) ;
#43716 = CARTESIAN_POINT ( 'NONE',  ( 0.3917322834645670104, -0.1049643490035303411, -1.456036745406824151 ) ) ;
#43717 = CARTESIAN_POINT ( 'NONE',  ( 0.06912221444360695799, 0.3857315817373091482, -1.220472440944881498 ) ) ;
#43718 = CARTESIAN_POINT ( 'NONE',  ( 0.9120734908136490793, 0.2952755905511810774, -0.1292274648535930714 ) ) ;
#43719 = CARTESIAN_POINT ( 'NONE',  ( 0.3937007874015754361, -0.1870078740157479769, 0.4822834645669291653 ) ) ;
#43720 = FACE_OUTER_BOUND ( 'NONE', #71504, .T. ) ;
#43721 = CARTESIAN_POINT ( 'NONE',  ( 0.2925321140481931814, 0.2925321140481931814, -2.576771653543307394 ) ) ;
#43722 = CARTESIAN_POINT ( 'NONE',  ( 1.272965879265092637, -0.004921259842519576551, 0.3153832671262227771 ) ) ;
#43723 = CARTESIAN_POINT ( 'NONE',  ( 0.3460692066303959202, 0.1998031496062993295, -1.076115485564304475 ) ) ;
#43724 = ORIENTED_EDGE ( 'NONE', *, *, #632, .F. ) ;
#43725 = CARTESIAN_POINT ( 'NONE',  ( 0.1958661417322836440, -0.3392501089628017219, -2.446194225721784576 ) ) ;
#43726 = ORIENTED_EDGE ( 'NONE', *, *, #58635, .F. ) ;
#43727 = CARTESIAN_POINT ( 'NONE',  ( 0.4199475065616803948, -0.6046776061558809534, -0.2411417322834644161 ) ) ;
#43728 = CARTESIAN_POINT ( 'NONE',  ( -0.7152230971128602510, -0.05778040916215560624, -0.4822834645669293319 ) ) ;
#43729 = CARTESIAN_POINT ( 'NONE',  ( -1.568241469816272105, -0.3162353388693409650, -0.4822834645669289433 ) ) ;
#43730 = CARTESIAN_POINT ( 'NONE',  ( 0.9580052493438327987, -0.4281496062992127816, -0.4176697321401328100 ) ) ;
#43731 = CARTESIAN_POINT ( 'NONE',  ( 1.522309711286089939, 0.2306618581243848609, 0.2411417322834645549 ) ) ;
#43732 = FACE_OUTER_BOUND ( 'NONE', #75476, .T. ) ;
#43733 = CARTESIAN_POINT ( 'NONE',  ( -0.03937007874015669567, 0.2952755905511811885, 0.000000000000000000 ) ) ;
#43734 = CARTESIAN_POINT ( 'NONE',  ( -1.371391076115484609, -0.6692913385826771977, 0.1292274648535927661 ) ) ;
#43735 = CARTESIAN_POINT ( 'NONE',  ( -1.653543307086613234, -0.1870078740157479769, 0.4822834645669291653 ) ) ;
#43736 = CARTESIAN_POINT ( 'NONE',  ( 1.410761154855643795, -0.05778040916215560624, -0.4822834645669293319 ) ) ;
#43737 = CARTESIAN_POINT ( 'NONE',  ( -0.3392501089628017219, -0.1958661417322836718, -2.814304461942257252 ) ) ;
#43738 = CARTESIAN_POINT ( 'NONE',  ( 0.9055118110236227702, 0.1771653543307087630, 0.000000000000000000 ) ) ;
#43739 = VERTEX_POINT ( 'NONE', #30719 ) ;
#43740 = CARTESIAN_POINT ( 'NONE',  ( -0.2891555358219908833, -0.2891555358219912164, -0.2165354330708662567 ) ) ;
#43741 = ORIENTED_EDGE ( 'NONE', *, *, #24425, .F. ) ;
#43742 = CARTESIAN_POINT ( 'NONE',  ( -0.2099737532808391705, -0.5023911411419708095, -0.1820866141732282451 ) ) ;
#43743 = CARTESIAN_POINT ( 'NONE',  ( -1.686351706036744558, 0.2952755905511810774, -0.1292274648535930714 ) ) ;
#43744 = CARTESIAN_POINT ( 'NONE',  ( 0.4002624671916016896, -0.3162353388693409650, -0.4822834645669289433 ) ) ;
#43745 = CARTESIAN_POINT ( 'NONE',  ( 0.5511811023622054106, -0.1870078740157480879, -0.4822834645669291653 ) ) ;
#43746 = CARTESIAN_POINT ( 'NONE',  ( -0.7349081364829390672, 0.2306618581243847221, -0.2411417322834647770 ) ) ;
#43747 = CARTESIAN_POINT ( 'NONE',  ( -0.3917322834645670659, -7.196005306013484475E-17, -1.610911704233282560 ) ) ;
#43748 = CARTESIAN_POINT ( 'NONE',  ( -1.351706036745406347, -0.4281496062992124485, 0.4176697321401328655 ) ) ;
#43749 = CARTESIAN_POINT ( 'NONE',  ( -0.3392501089628017219, -0.1958661417322836718, -2.656824146981627166 ) ) ;
#43750 = CARTESIAN_POINT ( 'NONE',  ( 1.377952755905512472, -0.5511811023622047445, 6.969142054262312111E-17 ) ) ;
#43751 = CARTESIAN_POINT ( 'NONE',  ( -0.8923884514435688198, -0.6046776061558807314, 0.2411417322834647770 ) ) ;
#43752 = CARTESIAN_POINT ( 'NONE',  ( 0.9842519685039378130, -0.6692913385826771977, 8.415575281601705876E-17 ) ) ;
#43753 = CARTESIAN_POINT ( 'NONE',  ( 1.049868766404200349, 0.2306618581243848609, 0.2411417322834645549 ) ) ;
#43754 = CARTESIAN_POINT ( 'NONE',  ( 0.3996062992125986590, -0.1070741851644053111, -0.7414698162729659314 ) ) ;
#43755 = CARTESIAN_POINT ( 'NONE',  ( -1.253280839895012377, -0.05778040916215522460, 0.4822834645669289988 ) ) ;
#43756 = CARTESIAN_POINT ( 'NONE',  ( 0.1998031496062994128, -0.3460692066303957537, -0.4835958005249343938 ) ) ;
#43757 = CARTESIAN_POINT ( 'NONE',  ( 0.4068241469816279987, -0.4281496062992127816, -0.4176697321401328100 ) ) ;
#43758 = CARTESIAN_POINT ( 'NONE',  ( 0.1998031496062994405, -0.3460692066303958092, -2.139107611548556331 ) ) ;
#43759 = CARTESIAN_POINT ( 'NONE',  ( -0.2867679344610364334, -0.2867679344610367109, -1.561023622047243986 ) ) ;
#43760 = VECTOR ( 'NONE', #27948, 39.37007874015748143 ) ;
#43761 = CARTESIAN_POINT ( 'NONE',  ( -1.371391076115484609, -0.5511811023622046335, 0.09757992244046803654 ) ) ;
#43762 = CARTESIAN_POINT ( 'NONE',  ( 0.2821522309711292364, 0.1771653543307087075, -0.09757992244046823083 ) ) ;
#43763 = CARTESIAN_POINT ( 'NONE',  ( 0.8202099737532813073, 0.2952755905511811885, 0.1292274648535926551 ) ) ;
#43764 = CARTESIAN_POINT ( 'NONE',  ( -0.2362204724409451284, 0.4091458600556402425, -1.034776902887139194 ) ) ;
#43765 = CARTESIAN_POINT ( 'NONE',  ( 0.6167979002624679463, -0.004921259842519870586, -0.3153832671262229437 ) ) ;
#43766 = CARTESIAN_POINT ( 'NONE',  ( 0.3412073490813655186, 0.2306618581243848609, 0.2411417322834645549 ) ) ;
#43767 = CARTESIAN_POINT ( 'NONE',  ( 0.2891555358219910499, -0.2891555358219909944, -1.120078740157480324 ) ) ;
#43768 = ADVANCED_FACE ( 'NONE', ( #16877 ), #28018, .F. ) ;
#43769 = CARTESIAN_POINT ( 'NONE',  ( -0.6955380577427815458, -0.4281496062992127816, -0.4176697321401328100 ) ) ;
#43770 = DIRECTION ( 'NONE',  ( 0.000000000000000000, 0.000000000000000000, 1.000000000000000000 ) ) ;
#43771 = DIMENSIONAL_EXPONENTS ( 1.000000000000000000, 0.000000000000000000, 0.000000000000000000, 0.000000000000000000, 0.000000000000000000, 0.000000000000000000, 0.000000000000000000 ) ;
#43772 = CARTESIAN_POINT ( 'NONE',  ( 1.003937007874016185, 0.07958543189024071263, -0.2665933059059888421 ) ) ;
#43773 = DIRECTION ( 'NONE',  ( 0.000000000000000000, 0.000000000000000000, 1.000000000000000000 ) ) ;
#43774 = CARTESIAN_POINT ( 'NONE',  ( -0.2165354330708654795, -0.5400638737290845981, -0.3530559997133363437 ) ) ;
#43775 = CARTESIAN_POINT ( 'NONE',  ( 0.1640419947506569498, -0.2845877964562161244, -0.3641732283464567121 ) ) ;
#43776 = CARTESIAN_POINT ( 'NONE',  ( -2.872342878167415403, 1.064797240280314083, -0.04222672046125293399 ) ) ;
#43777 = CARTESIAN_POINT ( 'NONE',  ( -0.4724409448818890911, -0.1870078740157479769, 0.4822834645669291653 ) ) ;
#43778 = CARTESIAN_POINT ( 'NONE',  ( 0.8005249343832027131, -0.004921259842519576551, 0.3153832671262227771 ) ) ;
#43779 = B_SPLINE_CURVE_WITH_KNOTS ( 'NONE', 3,
 ( #2860, #34433, #47455, #8346 ),
 .UNSPECIFIED., .F., .F.,
 ( 4, 4 ),
 ( 0.02918618983606361197, 0.02943414011348784165 ),
 .UNSPECIFIED. ) ;
#43780 = CARTESIAN_POINT ( 'NONE',  ( 0.2925321140481932369, 0.2925321140481932369, -1.631889763779527325 ) ) ;
#43781 = CARTESIAN_POINT ( 'NONE',  ( 0.2493438320209980519, 0.05413385826771666132, 0.4176697321401328100 ) ) ;
#43782 = CARTESIAN_POINT ( 'NONE',  ( 1.161417322834646493, -0.4536011799217367080, 0.2665933059059888421 ) ) ;
#43783 = CARTESIAN_POINT ( 'NONE',  ( -0.3503937007874015630, 0.3733313776025731778, -1.512162153811850596 ) ) ;
#43784 = CARTESIAN_POINT ( 'NONE',  ( -0.2362204724409442680, -0.1870078740157480601, -0.3641732283464567677 ) ) ;
#43785 = CARTESIAN_POINT ( 'NONE',  ( -0.6692913385826764205, -0.5511811023622047445, 6.969142054262312111E-17 ) ) ;
#43786 = CARTESIAN_POINT ( 'NONE',  ( -0.2624671916010490880, -0.6046776061558807314, 0.2411417322834647770 ) ) ;
#43787 = CARTESIAN_POINT ( 'NONE',  ( 0.4921259842519691285, 0.1660481256975885056, 0.3530559997133364547 ) ) ;
#43788 = CARTESIAN_POINT ( 'NONE',  ( 0.9186351706036752773, 0.1283753931104746893, -0.1820866141732285504 ) ) ;
#43789 = CARTESIAN_POINT ( 'NONE',  ( -1.666666666666665853, -0.004921259842519870586, -0.3153832671262229437 ) ) ;
#43790 = CARTESIAN_POINT ( 'NONE',  ( -1.686351706036744558, 0.2952755905511810774, -0.1292274648535930714 ) ) ;
#43791 = CARTESIAN_POINT ( 'NONE',  ( 0.8202099737532814183, -0.6692913385826773087, -0.1292274648535924053 ) ) ;
#43792 = LINE ( 'NONE', #62774, #80056 ) ;
#43793 = CARTESIAN_POINT ( 'NONE',  ( -0.06561679790026180015, -0.4281496062992127816, -0.4176697321401328100 ) ) ;
#43794 = CIRCLE ( 'NONE', #72082, 0.3129921259842521897 ) ;
#43795 = CARTESIAN_POINT ( 'NONE',  ( -0.3917322834645669549, -0.1049643490035306603, -1.075459317585301777 ) ) ;
#43796 = CARTESIAN_POINT ( 'NONE',  ( 0.8989501312335964611, 0.2952755905511811885, 0.1292274648535926551 ) ) ;
#43797 = AXIS2_PLACEMENT_3D ( 'NONE', #72599, #71347, #14945 ) ;
#43798 = CARTESIAN_POINT ( 'NONE',  ( 0.3740157480314966754, -0.5400638737290844871, 0.3530559997133364547 ) ) ;
#43799 = CARTESIAN_POINT ( 'NONE',  ( -0.4744094488188833059, 1.537401574803149984, -3.908320185825793658 ) ) ;
#43800 = CARTESIAN_POINT ( 'NONE',  ( 0.4527559055118117182, 0.07958543189024071263, -0.2665933059059888421 ) ) ;
#43801 = CARTESIAN_POINT ( 'NONE',  ( 1.003937007874016407, -0.5400638737290844871, 0.3530559997133364547 ) ) ;
#43802 = CARTESIAN_POINT ( 'NONE',  ( 0.1049868766404206816, -0.5023911411419708095, -0.1820866141732282451 ) ) ;
#43803 = CARTESIAN_POINT ( 'NONE',  ( -0.4724409448818890911, -0.1870078740157480879, -0.4822834645669291653 ) ) ;
#43804 = PLANE ( 'NONE',  #46127 ) ;
#43805 = CARTESIAN_POINT ( 'NONE',  ( 0.06561679790026316017, 0.05413385826771626580, -0.4176697321401330321 ) ) ;
#43806 = CARTESIAN_POINT ( 'NONE',  ( -0.9186351706036736120, -0.6046776061558809534, -0.2411417322834644161 ) ) ;
#43807 = CARTESIAN_POINT ( 'NONE',  ( -0.3412073490813641308, -0.5023911411419708095, 0.1820866141732285504 ) ) ;
#43808 = CARTESIAN_POINT ( 'NONE',  ( 0.3018372703412079971, -0.4281496062992124485, 0.4176697321401328655 ) ) ;
#43809 = CARTESIAN_POINT ( 'NONE',  ( 0.8070866141732289112, -0.4536011799217368745, -0.2665933059059886201 ) ) ;
#43810 = CARTESIAN_POINT ( 'NONE',  ( -0.2690288713910754526, -0.6692913385826771977, 0.1292274648535927661 ) ) ;
#43812 = CARTESIAN_POINT ( 'NONE',  ( 1.417322834645670104, -0.1870078740157479769, 0.4822834645669291653 ) ) ;
#43811 = DIRECTION ( 'NONE',  ( -0.000000000000000000, -1.000000000000000000, -0.000000000000000000 ) ) ;
#43813 = CARTESIAN_POINT ( 'NONE',  ( 1.679790026246720025, 0.2306618581243848609, 0.2411417322834645549 ) ) ;
#43814 = CARTESIAN_POINT ( 'NONE',  ( -0.1958661417322836718, 0.3392501089628017219, -2.209973753280840114 ) ) ;
#43816 = CIRCLE ( 'NONE', #38490, 3.444881889763779625 ) ;
#43815 = CARTESIAN_POINT ( 'NONE',  ( -1.056430446194224881, -0.6692913385826771977, 0.1292274648535927661 ) ) ;
#43817 = CARTESIAN_POINT ( 'NONE',  ( -0.7414698162729651543, 0.2952755905511810774, -0.1292274648535930714 ) ) ;
#43818 = CARTESIAN_POINT ( 'NONE',  ( 5.785732909357575061E-17, -0.4724409448818898682, -0.5511811023622047445 ) ) ;
#43819 = CARTESIAN_POINT ( 'NONE',  ( -0.3949938075777409963, -7.255918531996591613E-17, -2.874015748031495843 ) ) ;
#43820 = ORIENTED_EDGE ( 'NONE', *, *, #52674, .F. ) ;
#43821 = CARTESIAN_POINT ( 'NONE',  ( 0.4265091863517067594, 0.1771653543307087630, 0.09757992244046791164 ) ) ;
#43822 = CARTESIAN_POINT ( 'NONE',  ( -0.1049643490035307020, 0.3917322834645669549, -1.416010498687664043 ) ) ;
#43823 = CARTESIAN_POINT ( 'NONE',  ( 0.7874015748031503170, -0.1870078740157479769, 0.4822834645669291653 ) ) ;
#43824 = CARTESIAN_POINT ( 'NONE',  ( 0.3458507752293908943, 0.3458507752293908943, -2.342519685039369914 ) ) ;
#43825 = CARTESIAN_POINT ( 'NONE',  ( 0.9711286089238851948, 0.2306618581243848609, 0.2411417322834645549 ) ) ;
#43826 = CARTESIAN_POINT ( 'NONE',  ( -0.5118110236220466680, 0.1771653543307087630, 0.000000000000000000 ) ) ;
#43827 = DIRECTION ( 'NONE',  ( 0.000000000000000000, 0.000000000000000000, 1.000000000000000000 ) ) ;
#43828 = CARTESIAN_POINT ( 'NONE',  ( 1.003937007874016407, -0.5400638737290844871, 0.3530559997133364547 ) ) ;
#43829 = ADVANCED_FACE ( 'NONE', ( #76807 ), #19403, .F. ) ;
#43830 = CARTESIAN_POINT ( 'NONE',  ( 1.509186351706037543, -0.3690944881889765550, -0.3153832671262227771 ) ) ;
#43831 = CARTESIAN_POINT ( 'NONE',  ( 0.1902887139107617975, -0.6692913385826773087, -0.1292274648535924053 ) ) ;
#43832 = ADVANCED_FACE ( 'NONE', ( #739, #26814 ), #77759, .T. ) ;
#43833 = CARTESIAN_POINT ( 'NONE',  ( -0.1049643490035306742, 0.3917322834645668994, -0.8739964322496570626 ) ) ;
#43834 = CARTESIAN_POINT ( 'NONE',  ( -0.5708661417322825615, -0.5400638737290844871, 0.3530559997133364547 ) ) ;
#43835 = CARTESIAN_POINT ( 'NONE',  ( -1.299212598425196097, -0.5511811023622047445, 6.969142054262312111E-17 ) ) ;
#43837 = EDGE_CURVE ( 'NONE', #71206, #65960, #75436, .T. ) ;
#43836 = CARTESIAN_POINT ( 'NONE',  ( -0.4593175853018366950, 0.05413385826771666132, 0.4176697321401328100 ) ) ;
#43838 = CARTESIAN_POINT ( 'NONE',  ( -0.03443470937339728616, 1.062992125984252079, -1.537015892239756099 ) ) ;
#43839 = CARTESIAN_POINT ( 'NONE',  ( 4.725015209308685971E-16, 0.07874015748031502893, -3.858267716535433323 ) ) ;
#43840 = ORIENTED_EDGE ( 'NONE', *, *, #29666, .T. ) ;
#43841 = CARTESIAN_POINT ( 'NONE',  ( 0.1049643490035303967, 0.3917322834645670659, -2.194901205545618961 ) ) ;
#43842 = CARTESIAN_POINT ( 'NONE',  ( 0.3149606299212606708, -0.1870078740157480879, -0.4822834645669291653 ) ) ;
#43843 = VERTEX_POINT ( 'NONE', #67210 ) ;
#43844 = CARTESIAN_POINT ( 'NONE',  ( -0.2952755905511804668, 0.1660481256975885056, 0.3530559997133364547 ) ) ;
#43845 = CARTESIAN_POINT ( 'NONE',  ( -1.489501312335957062, -0.05778040916215522460, 0.4822834645669289988 ) ) ;
#43846 = CARTESIAN_POINT ( 'NONE',  ( 0.5643044619422579178, -0.4281496062992127816, -0.4176697321401328100 ) ) ;
#43847 = CARTESIAN_POINT ( 'NONE',  ( 0.1049868766404206816, 0.2306618581243848609, 0.2411417322834645549 ) ) ;
#43848 = CARTESIAN_POINT ( 'NONE',  ( 0.1049643490035304938, -0.3917322834645669549, -1.587270341207349222 ) ) ;
#43849 = CARTESIAN_POINT ( 'NONE',  ( -0.9514435695538050464, -0.3162353388693405765, 0.4822834645669290543 ) ) ;
#43850 = CARTESIAN_POINT ( 'NONE',  ( 0.3149606299212606708, -0.1870078740157480879, -0.4822834645669291653 ) ) ;
#43851 = CARTESIAN_POINT ( 'NONE',  ( -0.2821522309711278487, -0.6692913385826773087, -0.1292274648535924053 ) ) ;
#43852 = CARTESIAN_POINT ( 'NONE',  ( 0.1968503937007881344, -0.5511811023622047445, 6.969142054262312111E-17 ) ) ;
#43853 = CARTESIAN_POINT ( 'NONE',  ( -0.2746809754671077908, -0.1088096450009771038, 5.561685372298315500 ) ) ;
#43854 = CARTESIAN_POINT ( 'NONE',  ( -0.1181102362204717315, 0.2952755905511811885, 0.000000000000000000 ) ) ;
#43855 = CARTESIAN_POINT ( 'NONE',  ( 1.614173228346457378, 0.2753471884572480932, -0.1372047244094471152 ) ) ;
#43856 = CARTESIAN_POINT ( 'NONE',  ( -1.587926509186350810, 0.05413385826771626580, -0.4176697321401330321 ) ) ;
#43857 = CARTESIAN_POINT ( 'NONE',  ( -0.1958661417322836718, 0.3392501089628017219, -2.682414698162729483 ) ) ;
#43858 = ORIENTED_EDGE ( 'NONE', *, *, #46418, .T. ) ;
#43859 = EDGE_CURVE ( 'NONE', #43552, #57099, #9544, .T. ) ;
#43860 = ORIENTED_EDGE ( 'NONE', *, *, #47547, .F. ) ;
#43861 = AXIS2_PLACEMENT_3D ( 'NONE', #5600, #58180, #62857 ) ;
#43862 = CARTESIAN_POINT ( 'NONE',  ( 0.8005249343832028242, -0.4281496062992127816, -0.4176697321401328100 ) ) ;
#43863 = CARTESIAN_POINT ( 'NONE',  ( 0.01312335958005323398, -0.004921259842519576551, 0.3153832671262227771 ) ) ;
#43864 = AXIS2_PLACEMENT_3D ( 'NONE', #41555, #65589, #79883 ) ;
#43865 = AXIS2_PLACEMENT_3D ( 'NONE', #59114, #59527, #20822 ) ;
#43867 = DIRECTION ( 'NONE',  ( 0.000000000000000000, 0.000000000000000000, -1.000000000000000000 ) ) ;
#43866 = CARTESIAN_POINT ( 'NONE',  ( 1.279527559055118724, -0.4536011799217368745, -0.2665933059059886201 ) ) ;
#43868 = CARTESIAN_POINT ( 'NONE',  ( -9.594673741351313045E-17, 0.3917322834645670104, -1.344488188976378007 ) ) ;
#43869 = DIRECTION ( 'NONE',  ( 0.000000000000000000, 0.000000000000000000, 1.000000000000000000 ) ) ;
#43870 = CARTESIAN_POINT ( 'NONE',  ( 0.4177787735907000366, 0.000000000000000000, -1.559171609364239375 ) ) ;
#43871 = CARTESIAN_POINT ( 'NONE',  ( -0.3996062992125984925, -0.1070741851644056858, -2.642388451443570041 ) ) ;
#43872 =( REPRESENTATION_RELATIONSHIP ('NONE','NONE', #79348, #27201 ) REPRESENTATION_RELATIONSHIP_WITH_TRANSFORMATION ( #17013 )SHAPE_REPRESENTATION_RELATIONSHIP( ) );
#43873 = CARTESIAN_POINT ( 'NONE',  ( 0.4133858267716541968, -0.5400638737290845981, -0.3530559997133363437 ) ) ;
#43874 = CARTESIAN_POINT ( 'NONE',  ( -1.082677165354329896, -0.5400638737290845981, -0.3530559997133363437 ) ) ;
#43875 = CARTESIAN_POINT ( 'NONE',  ( -1.082677165354329896, 0.1660481256975885056, 0.3530559997133364547 ) ) ;
#43876 = CARTESIAN_POINT ( 'NONE',  ( 0.2165354330708668673, 0.1660481256975883668, -0.3530559997133364547 ) ) ;
#43877 = CARTESIAN_POINT ( 'NONE',  ( 1.030183727034121421, -0.3162353388693409650, -0.4822834645669289433 ) ) ;
#43878 = CARTESIAN_POINT ( 'NONE',  ( 1.312335958005250269, -0.5023911411419708095, 0.1820866141732285504 ) ) ;
#43879 = ITEM_DEFINED_TRANSFORMATION ( 'NONE', 'NONE', #22161,  #22098 ) ;
#43880 = CARTESIAN_POINT ( 'NONE',  ( 1.154855643044620184, -0.5023911411419708095, 0.1820866141732285504 ) ) ;
#43881 = CARTESIAN_POINT ( 'NONE',  ( -0.8792650918635160906, -0.4281496062992124485, 0.4176697321401328655 ) ) ;
#43882 = CARTESIAN_POINT ( 'NONE',  ( 4.893765752498283308E-17, -0.3996062992125985480, -0.3129921259842520231 ) ) ;
#43883 = CARTESIAN_POINT ( 'NONE',  ( -1.581364829396324945, -0.08942795157528024563, -0.3641732283464568787 ) ) ;
#43884 = CARTESIAN_POINT ( 'NONE',  ( 0.2867679344610365999, -0.2867679344610365444, -0.09055118110236216877 ) ) ;
#43885 = CARTESIAN_POINT ( 'NONE',  ( -0.07217847769028787330, -0.05778040916215522460, 0.4822834645669289988 ) ) ;
#43886 = AXIS2_PLACEMENT_3D ( 'NONE', #15348, #28372, #79326 ) ;
#43888 = DIRECTION ( 'NONE',  ( 0.000000000000000000, 0.000000000000000000, 1.000000000000000000 ) ) ;
#43887 = CARTESIAN_POINT ( 'NONE',  ( 1.358267716535433323, 0.1660481256975885056, 0.3530559997133364547 ) ) ;
#43889 = CARTESIAN_POINT ( 'NONE',  ( -1.437007874015747477, -0.4536011799217367080, 0.2665933059059888421 ) ) ;
#43890 = CARTESIAN_POINT ( 'NONE',  ( 8.195543980992789655E-16, -0.1870078740157480879, -0.4822834645669291653 ) ) ;
#43891 = CARTESIAN_POINT ( 'NONE',  ( 0.6824146981627303710, 0.1283753931104746893, -0.1820866141732285504 ) ) ;
#43892 = CARTESIAN_POINT ( 'NONE',  ( -1.614173228346456268, -0.5511811023622047445, 6.969142054262312111E-17 ) ) ;
#43893 = CARTESIAN_POINT ( 'NONE',  ( 0.8858267716535438430, 0.1660481256975885056, 0.3530559997133364547 ) ) ;
#43894 = CARTESIAN_POINT ( 'NONE',  ( 0.000000000000000000, 2.716535433070866645, 0.000000000000000000 ) ) ;
#43895 = CARTESIAN_POINT ( 'NONE',  ( -0.6561679790026240244, -0.5023911411419708095, 0.1820866141732285504 ) ) ;
#43896 = CARTESIAN_POINT ( 'NONE',  ( -0.7217847769028863381, 0.05413385826771626580, -0.4176697321401330321 ) ) ;
#43897 = CARTESIAN_POINT ( 'NONE',  ( 1.482939632545932307, -0.4281496062992124485, 0.4176697321401328655 ) ) ;
#43898 = CARTESIAN_POINT ( 'NONE',  ( -1.292650918635170010, -0.6692913385826771977, 0.1292274648535927661 ) ) ;
#43899 = CARTESIAN_POINT ( 'NONE',  ( 1.200787401574803681, 0.1660481256975885056, 0.3530559997133364547 ) ) ;
#43900 = CARTESIAN_POINT ( 'NONE',  ( -0.1049643490035307158, 0.3917322834645670104, -0.9481820454406320042 ) ) ;
#43901 = CARTESIAN_POINT ( 'NONE',  ( -1.213910761154854745, -0.5511811023622046335, 0.09757992244046803654 ) ) ;
#43902 = CARTESIAN_POINT ( 'NONE',  ( -1.646051170424378096, 0.8346805926620876059, -0.5309055118110233007 ) ) ;
#43903 = CARTESIAN_POINT ( 'NONE',  ( 1.259842519685040019, -0.1870078740157479769, 0.4822834645669291653 ) ) ;
#43904 = CARTESIAN_POINT ( 'NONE',  ( 0.2362204724409451007, -0.4091458600556402980, -2.530839895013123453 ) ) ;
#43905 = CARTESIAN_POINT ( 'NONE',  ( -1.476377952755905110, -0.5400638737290845981, -0.3530559997133363437 ) ) ;
#43906 = CARTESIAN_POINT ( 'NONE',  ( -1.587926509186350810, -0.004921259842519870586, -0.3153832671262229437 ) ) ;
#43907 = CARTESIAN_POINT ( 'NONE',  ( -1.056430446194224881, 0.1771653543307087075, -0.09757992244046823083 ) ) ;
#43908 = CARTESIAN_POINT ( 'NONE',  ( -0.5314960629921224866, 0.000000000000000000, -0.9881811337016660479 ) ) ;
#43909 = CARTESIAN_POINT ( 'NONE',  ( -0.3346456692913377662, 0.1660481256975883668, -0.3530559997133364547 ) ) ;
#43910 = CARTESIAN_POINT ( 'NONE',  ( -0.05249343832020911260, 0.1283753931104748280, 0.1820866141732283561 ) ) ;
#43911 = CARTESIAN_POINT ( 'NONE',  ( -1.358267716535432434, 0.07958543189024071263, -0.2665933059059888421 ) ) ;
#43913 = B_SPLINE_CURVE_WITH_KNOTS ( 'NONE', 3,
 ( #11086, #61601, #30433, #56098, #36743, #18231, #12324 ),
 .UNSPECIFIED., .F., .F.,
 ( 4, 3, 4 ),
 ( 0.000000000000000000, 0.001246232571205272213, 0.002492492258783270652 ),
 .UNSPECIFIED. ) ;
#43912 = CARTESIAN_POINT ( 'NONE',  ( 1.292650918635171564, 0.1771653543307087630, 0.09757992244046791164 ) ) ;
#43914 = CARTESIAN_POINT ( 'NONE',  ( 1.056430446194226658, 0.2952755905511811885, 0.1292274648535926551 ) ) ;
#43915 = FACE_OUTER_BOUND ( 'NONE', #71821, .T. ) ;
#43916 = CARTESIAN_POINT ( 'NONE',  ( 0.07217847769028949700, -0.2845877964562159024, 0.3641732283464567677 ) ) ;
#43917 = CARTESIAN_POINT ( 'NONE',  ( 0.4724409448818904789, -0.1870078740157480879, -0.4822834645669291653 ) ) ;
#43918 = CARTESIAN_POINT ( 'NONE',  ( 1.108923884514436242, -0.08942795157527998196, 0.3641732283464567121 ) ) ;
#43919 = ORIENTED_EDGE ( 'NONE', *, *, #65648, .T. ) ;
#43921 = CARTESIAN_POINT ( 'NONE',  ( 1.469816272965879911, 0.2306618581243847221, -0.2411417322834647770 ) ) ;
#43920 = CIRCLE ( 'NONE', #29345, 0.09842519685039372024 ) ;
#43922 = EDGE_CURVE ( 'NONE', #29775, #44273, #3641, .T. ) ;
#43923 = CARTESIAN_POINT ( 'NONE',  ( -1.391076115485563314, -0.6046776061558809534, -0.2411417322834644161 ) ) ;
#43924 = CARTESIAN_POINT ( 'NONE',  ( -0.2559055118110230564, 0.1660481256975883668, -0.3530559997133364547 ) ) ;
#43925 = AXIS2_PLACEMENT_3D ( 'NONE', #27255, #48576, #20953 ) ;
#43926 = CARTESIAN_POINT ( 'NONE',  ( 0.2925321140481932369, 0.2925321140481932369, -0.1377952755905512139 ) ) ;
#43927 = CARTESIAN_POINT ( 'NONE',  ( 0.3460692066303959202, -0.1998031496062991630, -2.701443569553806157 ) ) ;
#43928 = CARTESIAN_POINT ( 'NONE',  ( 0.5839895013123367340, -0.6692913385826773087, -0.1292274648535924053 ) ) ;
#43929 = CARTESIAN_POINT ( 'NONE',  ( 1.089238845144357537, -0.3690944881889763329, 0.3153832671262228327 ) ) ;
#43930 = CONICAL_SURFACE ( 'NONE', #7678, 0.09842519685039351207, 1.029744258676651647 ) ;
#43931 = AXIS2_PLACEMENT_3D ( 'NONE', #63717, #69219, #18698 ) ;
#43932 = CARTESIAN_POINT ( 'NONE',  ( -0.1049868766404193215, -0.6046776061558807314, 0.2411417322834647770 ) ) ;
#43933 = CARTESIAN_POINT ( 'NONE',  ( 0.4658792650918640033, -0.3162353388693405765, 0.4822834645669290543 ) ) ;
#43934 = CARTESIAN_POINT ( 'NONE',  ( -0.1998031496062991907, -0.3460692066303959757, -2.112860892388451539 ) ) ;
#43935 = CARTESIAN_POINT ( 'NONE',  ( -0.3420746716998659953, -0.1974969037888706647, -1.469816272965879245 ) ) ;
#43936 = CARTESIAN_POINT ( 'NONE',  ( -0.3132167369146011682, 1.180756483954326752, 1.077514311222549814 ) ) ;
#43937 = CARTESIAN_POINT ( 'NONE',  ( 3.908320185825791881, 1.569734778958133514, 0.4744094488188976277 ) ) ;
#43938 = CARTESIAN_POINT ( 'NONE',  ( 0.1049643490035304799, -0.3917322834645669549, -0.7073490813648293241 ) ) ;
#43939 = CARTESIAN_POINT ( 'NONE',  ( -0.5183727034120726440, -0.5511811023622048555, -0.09757992244046775898 ) ) ;
#43940 = CARTESIAN_POINT ( 'NONE',  ( -0.9186351706036736120, 0.2306618581243848609, 0.2411417322834645549 ) ) ;
#43941 = CARTESIAN_POINT ( 'NONE',  ( 4.837279021331061486E-17, -0.3949938075777409963, -2.517716535433071279 ) ) ;
#43942 = CARTESIAN_POINT ( 'NONE',  ( 0.7086614173228353852, -0.1870078740157479769, 0.4822834645669291653 ) ) ;
#43943 = CARTESIAN_POINT ( 'NONE',  ( -1.489501312335957062, -0.05778040916215522460, 0.4822834645669289988 ) ) ;
#43944 = CARTESIAN_POINT ( 'NONE',  ( 0.8792650918635177559, -0.4281496062992127816, -0.4176697321401328100 ) ) ;
#43945 = CARTESIAN_POINT ( 'NONE',  ( 0.3458507752293908943, -0.3458507752293908943, -2.775590551181101429 ) ) ;
#43946 = CARTESIAN_POINT ( 'NONE',  ( 0.2925321140481932369, 0.2925321140481932369, -2.342519685039369914 ) ) ;
#43947 = CARTESIAN_POINT ( 'NONE',  ( 1.509186351706037543, 0.05413385826771666132, 0.4176697321401328100 ) ) ;
#43948 = CARTESIAN_POINT ( 'NONE',  ( 1.056430446194226436, -0.6692913385826773087, -0.1292274648535924053 ) ) ;
#43949 = CARTESIAN_POINT ( 'NONE',  ( 0.4133858267716541968, -0.5400638737290845981, -0.3530559997133363437 ) ) ;
#43950 = CARTESIAN_POINT ( 'NONE',  ( 1.417322834645670104, -0.1870078740157479769, 0.3641732283464567677 ) ) ;
#43951 = CARTESIAN_POINT ( 'NONE',  ( 1.279527559055118724, -0.5400638737290845981, -0.3530559997133363437 ) ) ;
#43952 = CARTESIAN_POINT ( 'NONE',  ( -9.594673741351313045E-17, 0.3917322834645670104, -0.08464566929133868212 ) ) ;
#43953 = CARTESIAN_POINT ( 'NONE',  ( -0.3149606299212458493, 2.165354330708661568, -3.937007874015763242 ) ) ;
#43954 = CARTESIAN_POINT ( 'NONE',  ( 1.003937007874016407, -0.5400638737290844871, 0.3530559997133364547 ) ) ;
#43955 = CARTESIAN_POINT ( 'NONE',  ( 1.646981627296588035, -0.2845877964562159024, 0.3641732283464567677 ) ) ;
#43956 = CARTESIAN_POINT ( 'NONE',  ( -0.4658792650918627265, -0.05778040916215522460, 0.4822834645669289988 ) ) ;
#43957 = CARTESIAN_POINT ( 'NONE',  ( -1.122047244094487306, -0.5400638737290844871, 0.3530559997133364547 ) ) ;
#43958 = CARTESIAN_POINT ( 'NONE',  ( 1.305774278215223960, 0.2952755905511810774, -0.1292274648535930714 ) ) ;
#43959 = CARTESIAN_POINT ( 'NONE',  ( -0.3392501089628017219, -0.1958661417322836718, -0.6095800524934383846 ) ) ;
#43960 = CARTESIAN_POINT ( 'NONE',  ( 4.797336870675656522E-17, -0.3917322834645670104, -1.645669291338582640 ) ) ;
#43961 = CARTESIAN_POINT ( 'NONE',  ( 4.797336870675656522E-17, -0.3917322834645670104, -2.905511811023621771 ) ) ;
#43962 = CARTESIAN_POINT ( 'NONE',  ( 1.614173228346457378, -0.6692913385826771977, 8.415575281601705876E-17 ) ) ;
#43963 = ORIENTED_EDGE ( 'NONE', *, *, #76698, .T. ) ;
#43964 = CARTESIAN_POINT ( 'NONE',  ( 0.3949938075777409963, 2.418639510665530435E-17, -2.637795275590551380 ) ) ;
#43965 = VERTEX_POINT ( 'NONE', #55792 ) ;
#43966 = CARTESIAN_POINT ( 'NONE',  ( -1.614173228346457378, 0.4410134679336882302, 0.1372047244094476981 ) ) ;
#43967 = CARTESIAN_POINT ( 'NONE',  ( 1.404199475065617264, -0.3690944881889763329, 0.3153832671262228327 ) ) ;
#43968 = CARTESIAN_POINT ( 'NONE',  ( -0.1070741851644051862, -0.3996062992125987146, -1.489501312335957950 ) ) ;
#43969 = CARTESIAN_POINT ( 'NONE',  ( 1.469816272965879911, -0.5023911411419708095, 0.1820866141732285504 ) ) ;
#43970 = CARTESIAN_POINT ( 'NONE',  ( 0.6195821328811250694, 1.702998256715020864E-15, -0.4281989832122452544 ) ) ;
#43971 = CARTESIAN_POINT ( 'NONE',  ( 0.4665770185116075996, 1.519790403714398552, 0.5309055118110234117 ) ) ;
#43972 = DIRECTION ( 'NONE',  ( -3.491481338843132961E-15, -0.000000000000000000, 1.000000000000000000 ) ) ;
#43973 = CARTESIAN_POINT ( 'NONE',  ( -0.2867679344610364334, -0.2867679344610367109, -0.6161417322834646937 ) ) ;
#43974 = CARTESIAN_POINT ( 'NONE',  ( -0.6955380577427815458, -0.004921259842519576551, 0.3153832671262227771 ) ) ;
#43975 = CARTESIAN_POINT ( 'NONE',  ( -1.246719160104986512, -0.004921259842519576551, 0.3153832671262227771 ) ) ;
#43976 = CARTESIAN_POINT ( 'NONE',  ( -1.200787401574802349, -0.5400638737290844871, 0.3530559997133364547 ) ) ;
#43977 = CARTESIAN_POINT ( 'NONE',  ( 0.3018372703412079971, -0.4281496062992124485, 0.4176697321401328655 ) ) ;
#43978 = CARTESIAN_POINT ( 'NONE',  ( 1.574803149606299746, -0.1870078740157479769, 0.4822834645669291653 ) ) ;
#43979 = ORIENTED_EDGE ( 'NONE', *, *, #26454, .F. ) ;
#43980 = CARTESIAN_POINT ( 'NONE',  ( 1.318897637795276356, 0.1660481256975883668, -0.3530559997133364547 ) ) ;
#43981 = CARTESIAN_POINT ( 'NONE',  ( 0.5314960629921156032, 2.559055118110236560, 0.9881811337016696006 ) ) ;
#43982 = DIRECTION ( 'NONE',  ( 0.6771895334375255260, 0.000000000000000000, 0.7358086271597165107 ) ) ;
#43983 = CARTESIAN_POINT ( 'NONE',  ( -0.2362204724409451284, 0.4091458600556402425, -2.217847769028871596 ) ) ;
#43984 = CARTESIAN_POINT ( 'NONE',  ( -1.586052503253848167, 1.023622047244095556, -0.1653254495020564929 ) ) ;
#43985 = CARTESIAN_POINT ( 'NONE',  ( -0.5511811023622038563, -0.1870078740157479769, 0.3641732283464567677 ) ) ;
#43986 = VECTOR ( 'NONE', #28090, 39.37007874015748143 ) ;
#43987 = CARTESIAN_POINT ( 'NONE',  ( -1.030183727034119867, -0.3162353388693405765, 0.4822834645669290543 ) ) ;
#43988 = CARTESIAN_POINT ( 'NONE',  ( 1.167979002624672580, -0.4281496062992124485, 0.4176697321401328655 ) ) ;
#43989 = CIRCLE ( 'NONE', #77604, 0.1771653543307088186 ) ;
#43990 = ORIENTED_EDGE ( 'NONE', *, *, #4442, .F. ) ;
#43992 = CARTESIAN_POINT ( 'NONE',  ( -0.4091458600556402980, -0.2362204724409451284, -2.648950131233595684 ) ) ;
#43991 = DIRECTION ( 'NONE',  ( -1.000000000000000000, 0.000000000000000000, 0.000000000000000000 ) ) ;
#43993 = EDGE_CURVE ( 'NONE', #38787, #36842, #63502, .T. ) ;
#43994 = CARTESIAN_POINT ( 'NONE',  ( -1.586052503253848167, 1.023622047244095556, -0.1653254495020564929 ) ) ;
#43995 = CARTESIAN_POINT ( 'NONE',  ( -1.056430446194224881, 0.2952755905511810774, -0.1292274648535930714 ) ) ;
#43996 = CARTESIAN_POINT ( 'NONE',  ( -0.1049643490035306742, 0.3917322834645668994, -0.2440751724071372475 ) ) ;
#43997 = CARTESIAN_POINT ( 'NONE',  ( -0.5314960629921254842, -0.4536011799217368745, -0.2665933059059886201 ) ) ;
#43998 = CARTESIAN_POINT ( 'NONE',  ( -0.1958661417322836718, 0.3392501089628017219, -0.8851706036745407014 ) ) ;
#43999 = ADVANCED_FACE ( 'NONE', ( #66800, #2816 ), #22168, .T. ) ;
#44000 = CARTESIAN_POINT ( 'NONE',  ( -0.3871391076115476282, -0.08942795157527998196, 0.3641732283464567121 ) ) ;
#44001 = CARTESIAN_POINT ( 'NONE',  ( 0.3608923884514443348, 0.1771653543307087075, -0.09757992244046823083 ) ) ;
#44002 = CARTESIAN_POINT ( 'NONE',  ( 0.05249343832021075018, 0.2306618581243847221, -0.2411417322834647770 ) ) ;
#44003 = CARTESIAN_POINT ( 'NONE',  ( -0.5839895013123351797, -0.5511811023622046335, 0.09757992244046803654 ) ) ;
#44004 = CARTESIAN_POINT ( 'NONE',  ( -0.2867679344610364334, -0.2867679344610367109, -2.885826771653543066 ) ) ;
#44005 = CARTESIAN_POINT ( 'NONE',  ( 0.9711286089238851948, 0.2306618581243848609, 0.2411417322834645549 ) ) ;
#44006 = CARTESIAN_POINT ( 'NONE',  ( -1.135170603674539924, 0.2952755905511810774, -0.1292274648535930714 ) ) ;
#44007 = CARTESIAN_POINT ( 'NONE',  ( 0.4724409448818896462, 0.1265901696524990294, -0.9888451443569553634 ) ) ;
#44008 = CARTESIAN_POINT ( 'NONE',  ( -0.5511811023622041894, -0.1870078740157480879, -0.4822834645669291653 ) ) ;
#44009 = CARTESIAN_POINT ( 'NONE',  ( -0.8136482939632537770, 0.2306618581243847221, -0.2411417322834647770 ) ) ;
#44010 = CARTESIAN_POINT ( 'NONE',  ( 1.194225721784777594, -0.004921259842519576551, 0.3153832671262227771 ) ) ;
#44011 = CARTESIAN_POINT ( 'NONE',  ( 0.1837270341207354329, 0.1283753931104748280, 0.1820866141732283561 ) ) ;
#44012 = CARTESIAN_POINT ( 'NONE',  ( -0.7677165354330699465, 0.1660481256975885056, 0.3530559997133364547 ) ) ;
#44013 = CARTESIAN_POINT ( 'NONE',  ( -1.200787401574802349, -0.5400638737290844871, 0.3530559997133364547 ) ) ;
#44014 = CARTESIAN_POINT ( 'NONE',  ( -0.7974104941589342799, -2.567464376874931580E-15, -0.4445507791589072832 ) ) ;
#44015 = CARTESIAN_POINT ( 'NONE',  ( 0.2362204724409449064, 0.4091458600556404646, -0.3018372703412073310 ) ) ;
#44016 = CARTESIAN_POINT ( 'NONE',  ( -0.3871391076115476282, -0.05778040916215522460, 0.4822834645669289988 ) ) ;
#44017 = CARTESIAN_POINT ( 'NONE',  ( -1.030183727034119867, -0.05778040916215560624, -0.4822834645669293319 ) ) ;
#44018 = VERTEX_POINT ( 'NONE', #42339 ) ;
#44019 = EDGE_CURVE ( 'NONE', #78139, #25753, #36645, .T. ) ;
#44020 = CARTESIAN_POINT ( 'NONE',  ( -0.2925321140481932369, 0.2925321140481931259, -2.143700787401574548 ) ) ;
#44021 = CARTESIAN_POINT ( 'NONE',  ( 1.213910761154856299, -0.6692913385826773087, -0.1292274648535924053 ) ) ;
#44022 = CARTESIAN_POINT ( 'NONE',  ( -0.4921259842519677963, -0.4536011799217367080, 0.2665933059059888421 ) ) ;
#44023 = CARTESIAN_POINT ( 'NONE',  ( -0.7874015748031489847, -0.1870078740157479769, 0.4822834645669291653 ) ) ;
#44024 = CARTESIAN_POINT ( 'NONE',  ( 1.095800524934383846, -0.05778040916215560624, -0.4822834645669293319 ) ) ;
#44025 = CARTESIAN_POINT ( 'NONE',  ( 0.7349081364829403995, 0.2306618581243848609, 0.2411417322834645549 ) ) ;
#44026 = CARTESIAN_POINT ( 'NONE',  ( 0.3458507752293908943, -0.3458507752293908943, -0.09842519685039370636 ) ) ;
#44027 = CARTESIAN_POINT ( 'NONE',  ( -0.9186351706036736120, 0.1283753931104748280, 0.1820866141732283561 ) ) ;
#44028 = CARTESIAN_POINT ( 'NONE',  ( 0.2925321140481931814, 0.2925321140481931814, -0.8444881889763780070 ) ) ;
#44030 = ADVANCED_FACE ( 'NONE', ( #79851, #28893 ), #81086, .T. ) ;
#44029 = CARTESIAN_POINT ( 'NONE',  ( -0.1998031496062994683, 0.3460692066303958092, -1.115485564304461885 ) ) ;
#44031 = CARTESIAN_POINT ( 'NONE',  ( -0.2891555358219908833, -0.2891555358219912164, -0.3740157480314962313 ) ) ;
#44032 = CARTESIAN_POINT ( 'NONE',  ( 0.000000000000000000, 0.4374015748031496176, 0.000000000000000000 ) ) ;
#44033 = CARTESIAN_POINT ( 'NONE',  ( 1.148293963254593875, -0.5511811023622046335, 0.09757992244046803654 ) ) ;
#44034 = CARTESIAN_POINT ( 'NONE',  ( 0.7414698162729663755, -0.5511811023622048555, -0.09757992244046775898 ) ) ;
#44035 = CARTESIAN_POINT ( 'NONE',  ( 0.6364829396325465405, -0.05778040916215522460, 0.4822834645669289988 ) ) ;
#44036 = CARTESIAN_POINT ( 'NONE',  ( 0.3458507752293908943, -0.3458507752293908943, -2.379921259842519898 ) ) ;
#44037 = CARTESIAN_POINT ( 'NONE',  ( 0.1974969037888706092, -0.3420746716998660508, -1.113517060367454015 ) ) ;
#44038 = CARTESIAN_POINT ( 'NONE',  ( 0.9055118110236227702, 0.1771653543307087630, 0.000000000000000000 ) ) ;
#44039 = CARTESIAN_POINT ( 'NONE',  ( -0.3937007874015740483, -0.1870078740157479769, 0.4822834645669291653 ) ) ;
#44040 = CARTESIAN_POINT ( 'NONE',  ( -1.332020997375327642, -0.05778040916215522460, 0.4822834645669289988 ) ) ;
#44041 = CARTESIAN_POINT ( 'NONE',  ( 1.417322834645670104, -0.1870078740157480879, -0.4822834645669291653 ) ) ;
#44042 = CARTESIAN_POINT ( 'NONE',  ( -0.3458507752293909498, 0.3458507752293907833, -1.437007874015747921 ) ) ;
#44043 = VECTOR ( 'NONE', #53864, 39.37007874015748143 ) ;
#44044 = LINE ( 'NONE', #69736, #66742 ) ;
#44045 = CARTESIAN_POINT ( 'NONE',  ( -0.02624671916010428221, -0.5023911411419708095, 0.1820866141732285504 ) ) ;
#44046 = ORIENTED_EDGE ( 'NONE', *, *, #42996, .F. ) ;
#44047 = ORIENTED_EDGE ( 'NONE', *, *, #74342, .F. ) ;
#44048 = CARTESIAN_POINT ( 'NONE',  ( -0.8202099737532801971, -0.6692913385826771977, 0.1292274648535927661 ) ) ;
#44049 = CARTESIAN_POINT ( 'NONE',  ( -0.5183727034120726440, 0.2952755905511811885, 0.1292274648535926551 ) ) ;
#44050 = CARTESIAN_POINT ( 'NONE',  ( -0.7020997375328074108, -0.05778040916215522460, 0.4822834645669289988 ) ) ;
#44051 = CARTESIAN_POINT ( 'NONE',  ( 0.3871391076115493490, -0.3162353388693405765, 0.4822834645669290543 ) ) ;
#44052 = CARTESIAN_POINT ( 'NONE',  ( -0.3083989501312330295, -0.3162353388693409650, -0.4822834645669289433 ) ) ;
#44053 = CARTESIAN_POINT ( 'NONE',  ( -1.535433070866141225, -0.6692913385826771977, 8.415575281601705876E-17 ) ) ;
#44054 = CARTESIAN_POINT ( 'NONE',  ( -0.6955380577427815458, -0.4281496062992127816, -0.4176697321401328100 ) ) ;
#44055 = CARTESIAN_POINT ( 'NONE',  ( 0.8464566929133865436, 0.1660481256975883668, -0.3530559997133364547 ) ) ;
#44056 = CARTESIAN_POINT ( 'NONE',  ( -0.3392501089628017219, -0.1958661417322836718, -1.304461942257217899 ) ) ;
#44057 = CARTESIAN_POINT ( 'NONE',  ( -0.4921259842519677963, 0.07958543189024071263, -0.2665933059059888421 ) ) ;
#44058 = ORIENTED_EDGE ( 'NONE', *, *, #67062, .F. ) ;
#44059 = CARTESIAN_POINT ( 'NONE',  ( -0.3949938075777409408, -0.1058382717557502933, -1.305774278215223072 ) ) ;
#44060 = ORIENTED_EDGE ( 'NONE', *, *, #81623, .T. ) ;
#44061 = CARTESIAN_POINT ( 'NONE',  ( -1.259842519685038686, -0.1870078740157479769, 0.3641732283464567677 ) ) ;
#44062 = CARTESIAN_POINT ( 'NONE',  ( -1.181102362204723644, -0.1870078740157479769, 0.4822834645669291653 ) ) ;
#44063 = CARTESIAN_POINT ( 'NONE',  ( -0.8989501312335946848, -0.6692913385826771977, 0.1292274648535927661 ) ) ;
#44064 = CARTESIAN_POINT ( 'NONE',  ( -0.1070741851644051862, -0.3996062992125987146, -0.07217847769028871985 ) ) ;
#44065 = CARTESIAN_POINT ( 'NONE',  ( -1.272965879265091305, -0.4281496062992124485, 0.4176697321401328655 ) ) ;
#44066 = CARTESIAN_POINT ( 'NONE',  ( -0.9448818897637790704, -0.1870078740157479769, 0.4822834645669291653 ) ) ;
#44067 = FACE_OUTER_BOUND ( 'NONE', #38790, .T. ) ;
#44068 = CARTESIAN_POINT ( 'NONE',  ( 0.1181102362204724532, 0.09842519685039372024, -1.432673802628665356E-17 ) ) ;
#44069 = B_SPLINE_CURVE_WITH_KNOTS ( 'NONE', 3,
 ( #14677, #40333, #79073, #34018, #59678, #21389, #71490, #72737, #60102, #15501, #2034, #47458, #28114, #27699, #8761, #21795 ),
 .UNSPECIFIED., .F., .F.,
 ( 4, 2, 2, 2, 2, 2, 2, 4 ),
 ( 0.000000000000000000, 0.0003923911760484627724, 0.0007847823520969255447, 0.001177173528145388209, 0.001569564704193851089, 0.001961955880242313970, 0.002354347056290776417, 0.003139129408387686133 ),
 .UNSPECIFIED. ) ;
#44070 = CARTESIAN_POINT ( 'NONE',  ( 0.5708661417322842269, 0.07958543189024085140, 0.2665933059059887866 ) ) ;
#44071 = FACE_OUTER_BOUND ( 'NONE', #78580, .T. ) ;
#44072 = CARTESIAN_POINT ( 'NONE',  ( 0.3392501089628018329, 0.1958661417322835607, -0.05839895013123368173 ) ) ;
#44073 = CARTESIAN_POINT ( 'NONE',  ( 0.2559055118110243332, -0.4536011799217368745, -0.2665933059059886201 ) ) ;
#44074 = CARTESIAN_POINT ( 'NONE',  ( -0.4002624671916004129, -0.3162353388693405765, 0.4822834645669290543 ) ) ;
#44075 = CARTESIAN_POINT ( 'NONE',  ( 1.279527559055118724, 0.1660481256975885056, 0.3530559997133364547 ) ) ;
#44076 = CARTESIAN_POINT ( 'NONE',  ( -0.6692913385826764205, 0.2952755905511811885, 0.000000000000000000 ) ) ;
#44077 = VERTEX_POINT ( 'NONE', #54553 ) ;
#44078 = CARTESIAN_POINT ( 'NONE',  ( 0.2925321140481932369, -0.2925321140481932369, -2.145669291338581974 ) ) ;
#44079 = CARTESIAN_POINT ( 'NONE',  ( -0.8202099737532798640, 0.2066929133858267098, -0.1054918080437494132 ) ) ;
#44080 = ORIENTED_EDGE ( 'NONE', *, *, #33686, .T. ) ;
#44081 = CARTESIAN_POINT ( 'NONE',  ( 0.1070741851644054776, -0.3996062992125984925, -1.579396325459317296 ) ) ;
#44082 = CARTESIAN_POINT ( 'NONE',  ( 1.108923884514436242, -0.05778040916215522460, 0.4822834645669289988 ) ) ;
#44083 = CARTESIAN_POINT ( 'NONE',  ( -0.9448818897637790704, -0.1870078740157479769, 0.3641732283464567677 ) ) ;
#44084 = CARTESIAN_POINT ( 'NONE',  ( -1.187664041994750175, -0.05778040916215560624, -0.4822834645669293319 ) ) ;
#44085 = CARTESIAN_POINT ( 'NONE',  ( -0.3458507752293906723, -0.3458507752293910609, -1.003937007874015741 ) ) ;
#44086 = CARTESIAN_POINT ( 'NONE',  ( -0.5314960629921122726, 2.755905511811024056, -3.937007874015763687 ) ) ;
#44087 = CARTESIAN_POINT ( 'NONE',  ( 0.1958661417322834775, 0.3392501089628018884, -2.748687664041994605 ) ) ;
#44088 = CARTESIAN_POINT ( 'NONE',  ( 1.509186351706037543, 0.05413385826771666132, 0.4176697321401328100 ) ) ;
#44089 = CARTESIAN_POINT ( 'NONE',  ( 0.2867679344610366554, 0.2867679344610366554, -2.112204724409449064 ) ) ;
#44090 = CARTESIAN_POINT ( 'NONE',  ( 0.1312335958005257930, 0.2306618581243847221, -0.2411417322834647770 ) ) ;
#44091 = CARTESIAN_POINT ( 'NONE',  ( -0.9776902887139098386, 0.1771653543307087075, -0.09757992244046823083 ) ) ;
#44092 = CARTESIAN_POINT ( 'NONE',  ( -0.3674540682414692561, -0.6046776061558809534, -0.2411417322834644161 ) ) ;
#44093 = CARTESIAN_POINT ( 'NONE',  ( -0.4091458600556405756, 0.2362204724409446288, -2.622703412073490892 ) ) ;
#44094 = CARTESIAN_POINT ( 'NONE',  ( -0.7677165354330699465, 0.1660481256975885056, 0.3530559997133364547 ) ) ;
#44095 = ADVANCED_FACE ( 'NONE', ( #74354 ), #36039, .T. ) ;
#44096 = CARTESIAN_POINT ( 'NONE',  ( 0.2891555358219910499, -0.2891555358219909944, -2.064960629921260171 ) ) ;
#44097 = CARTESIAN_POINT ( 'NONE',  ( 1.102362204724410155, -0.1870078740157479769, 0.3641732283464567677 ) ) ;
#44098 = CARTESIAN_POINT ( 'NONE',  ( -0.1509186351706028884, -0.08942795157527998196, 0.3641732283464567121 ) ) ;
#44099 = CARTESIAN_POINT ( 'NONE',  ( 0.9383202099737538715, -0.08942795157528024563, -0.3641732283464568787 ) ) ;
#44100 = CARTESIAN_POINT ( 'NONE',  ( -1.502624671916009680, -0.05778040916215560624, -0.4822834645669293319 ) ) ;
#44101 = CARTESIAN_POINT ( 'NONE',  ( -0.1265901696524986964, -0.4724409448818899238, -2.196194225721784576 ) ) ;
#44102 = CARTESIAN_POINT ( 'NONE',  ( 0.5708661417322842269, 0.07958543189024085140, 0.2665933059059887866 ) ) ;
#44103 = CARTESIAN_POINT ( 'NONE',  ( -0.9055118110236215490, -0.6692913385826771977, 8.415575281601705876E-17 ) ) ;
#44104 = CIRCLE ( 'NONE', #77718, 0.5120078740157480990 ) ;
#44105 = CARTESIAN_POINT ( 'NONE',  ( 0.5314960629920993940, 2.716535433070866645, 2.543486866223394482 ) ) ;
#44106 = CARTESIAN_POINT ( 'NONE',  ( -0.03280839895013062252, 0.1771653543307087075, -0.09757992244046823083 ) ) ;
#44107 = CARTESIAN_POINT ( 'NONE',  ( -1.699475065616797398, 0.1771653543307087630, 0.09757992244046791164 ) ) ;
#44108 = CARTESIAN_POINT ( 'NONE',  ( 0.6758530183727039509, -0.6692913385826771977, 0.1292274648535927661 ) ) ;
#44109 = CARTESIAN_POINT ( 'NONE',  ( 0.2726377952755905665, 0.1133856558944469489, 0.1574803149606299191 ) ) ;
#44110 = CARTESIAN_POINT ( 'NONE',  ( 1.325459317585302665, -0.004921259842519870586, -0.3153832671262229437 ) ) ;
#44111 = CARTESIAN_POINT ( 'NONE',  ( -1.410761154855642463, -0.05778040916215522460, 0.4822834645669289988 ) ) ;
#44112 = CARTESIAN_POINT ( 'NONE',  ( -0.4002624671916004129, -0.2845877964562159024, 0.3641732283464567677 ) ) ;
#44113 = CYLINDRICAL_SURFACE ( 'NONE', #67713, 0.3937007874015748254 ) ;
#44114 = CARTESIAN_POINT ( 'NONE',  ( 0.02624671916010564918, 0.1283753931104748280, 0.1820866141732283561 ) ) ;
#44115 = CARTESIAN_POINT ( 'NONE',  ( -1.253280839895012377, -0.05778040916215522460, 0.4822834645669289988 ) ) ;
#44116 = CARTESIAN_POINT ( 'NONE',  ( -0.6824146981627288167, 0.2306618581243848609, 0.2411417322834645549 ) ) ;
#44117 = CARTESIAN_POINT ( 'NONE',  ( -0.1070741851644056997, 0.3996062992125984925, -0.5557742782152230721 ) ) ;
#44118 = CARTESIAN_POINT ( 'NONE',  ( -0.1958661417322836718, 0.3392501089628017219, -2.302493438320210029 ) ) ;
#44119 = CARTESIAN_POINT ( 'NONE',  ( 0.6955380577427828781, -0.004921259842519870586, -0.3153832671262229437 ) ) ;
#44120 = CARTESIAN_POINT ( 'NONE',  ( -0.5380577427821514602, 0.05413385826771666132, 0.4176697321401328100 ) ) ;
#44121 = CARTESIAN_POINT ( 'NONE',  ( -0.5380577427821514602, 0.05413385826771666132, 0.4176697321401328100 ) ) ;
#44122 = CARTESIAN_POINT ( 'NONE',  ( -0.8070866141732276899, 0.07958543189024071263, -0.2665933059059888421 ) ) ;
#44123 = CARTESIAN_POINT ( 'NONE',  ( -3.920805145893436539, 1.223994253877878302, -0.3574943889377464323 ) ) ;
#44124 = CARTESIAN_POINT ( 'NONE',  ( 0.1443569553805781891, 0.05413385826771626580, -0.4176697321401330321 ) ) ;
#44125 = CARTESIAN_POINT ( 'NONE',  ( 1.614173228346457156, 1.929133858267716661, -0.5309055118110239668 ) ) ;
#44126 = CARTESIAN_POINT ( 'NONE',  ( -1.430446194225720724, 0.05413385826771626580, -0.4176697321401330321 ) ) ;
#44127 = CARTESIAN_POINT ( 'NONE',  ( -0.4359958488159755841, 1.724409448818897905, 1.033875059083675163 ) ) ;
#44128 = CARTESIAN_POINT ( 'NONE',  ( 0.3392501089628018329, 0.1958661417322835607, -2.175216166175539811 ) ) ;
#44129 = ORIENTED_EDGE ( 'NONE', *, *, #42894, .T. ) ;
#44130 = CARTESIAN_POINT ( 'NONE',  ( 1.614173228346457378, 1.055049524192302579, -0.1372047244094476148 ) ) ;
#44131 = CARTESIAN_POINT ( 'NONE',  ( -1.154855643044618851, -0.6046776061558809534, -0.2411417322834644161 ) ) ;
#44132 = CARTESIAN_POINT ( 'NONE',  ( -1.023622047244094002, -0.1870078740157480879, -0.4822834645669291653 ) ) ;
#44133 = CARTESIAN_POINT ( 'NONE',  ( -1.607611548556429737, 0.2952755905511810774, -0.1292274648535930714 ) ) ;
#44134 = CARTESIAN_POINT ( 'NONE',  ( -0.1958661417322834220, -0.3392501089628018884, -2.040026246719160330 ) ) ;
#44135 = CARTESIAN_POINT ( 'NONE',  ( 3.937007874015748143, 1.537401574803149984, 2.901595197523589142E-16 ) ) ;
#44136 = CARTESIAN_POINT ( 'NONE',  ( 0.7480314960629927956, 0.2952755905511811885, 0.000000000000000000 ) ) ;
#44137 = CARTESIAN_POINT ( 'NONE',  ( 0.1771653543307093182, -0.5400638737290845981, -0.3530559997133363437 ) ) ;
#44138 = CARTESIAN_POINT ( 'NONE',  ( 0.000000000000000000, 0.5905511811023621549, 0.000000000000000000 ) ) ;
#44139 = LINE ( 'NONE', #12180, #8940 ) ;
#44140 = CARTESIAN_POINT ( 'NONE',  ( 1.397637795275591177, -0.4536011799217367080, 0.2665933059059888421 ) ) ;
#44141 = CARTESIAN_POINT ( 'NONE',  ( -0.1070741851644051862, -0.3996062992125987146, -0.8595800524934383846 ) ) ;
#44142 = EDGE_LOOP ( 'NONE', ( #12435, #8466, #60350, #43658, #34154, #13273 ) ) ;
#44143 = CARTESIAN_POINT ( 'NONE',  ( -9.594673741351313045E-17, 0.3917322834645670104, -2.826771653543306506 ) ) ;
#44144 = ORIENTED_EDGE ( 'NONE', *, *, #49461, .F. ) ;
#44145 = CARTESIAN_POINT ( 'NONE',  ( 0.2624671916010504757, -0.6046776061558809534, -0.2411417322834644161 ) ) ;
#44146 = CARTESIAN_POINT ( 'NONE',  ( -0.8136482939632537770, -0.6046776061558807314, 0.2411417322834647770 ) ) ;
#44147 = CARTESIAN_POINT ( 'NONE',  ( -1.430446194225720724, 0.05413385826771626580, -0.4176697321401330321 ) ) ;
#44148 = CARTESIAN_POINT ( 'NONE',  ( 0.5314960629921267055, -0.5400638737290844871, 0.3530559997133364547 ) ) ;
#44149 = CARTESIAN_POINT ( 'NONE',  ( 1.463254593175853824, -0.6692913385826771977, 0.1292274648535927661 ) ) ;
#44150 = CARTESIAN_POINT ( 'NONE',  ( 1.541994750656168645, -0.6692913385826771977, 0.1292274648535927661 ) ) ;
#44151 = CARTESIAN_POINT ( 'NONE',  ( 0.01968503937007957949, -0.5400638737290845981, -0.3530559997133363437 ) ) ;
#44152 = CARTESIAN_POINT ( 'NONE',  ( -1.279527559055116948, 0.1660481256975883668, -0.3530559997133364547 ) ) ;
#44153 = CARTESIAN_POINT ( 'NONE',  ( 1.594488188976378673, 0.1660481256975885056, 0.3530559997133364547 ) ) ;
#44154 = CARTESIAN_POINT ( 'NONE',  ( 1.633858267716535639, -0.5400638737290844871, 0.3530559997133364547 ) ) ;
#44155 = CARTESIAN_POINT ( 'NONE',  ( 0.1049643490035303689, 0.3917322834645670104, -0.3005249343832020470 ) ) ;
#44156 = CARTESIAN_POINT ( 'NONE',  ( 1.030183727034121421, -0.08942795157527998196, 0.3641732283464567121 ) ) ;
#44157 = VERTEX_POINT ( 'NONE', #9135 ) ;
#44158 = CARTESIAN_POINT ( 'NONE',  ( 4.837279021331060870E-17, -0.3949938075777409963, -0.3937007874015748810 ) ) ;
#44159 = ORIENTED_EDGE ( 'NONE', *, *, #16637, .F. ) ;
#44160 = CARTESIAN_POINT ( 'NONE',  ( 0.1640419947506569498, -0.08942795157527998196, 0.3641732283464567121 ) ) ;
#44161 = DIRECTION ( 'NONE',  ( -1.000000000000000000, 0.000000000000000000, 1.692413147294446216E-16 ) ) ;
#44162 = CARTESIAN_POINT ( 'NONE',  ( 0.4330708661417329575, -0.6692913385826771977, 8.415575281601705876E-17 ) ) ;
#44163 = CARTESIAN_POINT ( 'NONE',  ( 0.2165354330708668673, 0.1660481256975883668, -0.3530559997133364547 ) ) ;
#44164 = CARTESIAN_POINT ( 'NONE',  ( -0.4724409448818890911, -0.1870078740157479769, 0.4822834645669291653 ) ) ;
#44165 = CARTESIAN_POINT ( 'NONE',  ( 0.3917322834645670659, -0.1049643490035303273, -1.840570496884201379 ) ) ;
#44166 = CARTESIAN_POINT ( 'NONE',  ( -1.305774278215222184, 0.2952755905511811885, 0.1292274648535926551 ) ) ;
#44167 = CARTESIAN_POINT ( 'NONE',  ( 4.797336870675656522E-17, -0.3917322834645670104, -2.840551181102362044 ) ) ;
#44168 = CARTESIAN_POINT ( 'NONE',  ( 1.364829396325459854, -0.5023911411419708095, -0.1820866141732282451 ) ) ;
#44169 = CARTESIAN_POINT ( 'NONE',  ( -1.410761154855641575, -0.3162353388693409650, -0.4822834645669289433 ) ) ;
#44170 = CARTESIAN_POINT ( 'NONE',  ( 0.7611548556430454138, 0.2306618581243847221, -0.2411417322834647770 ) ) ;
#44171 = CARTESIAN_POINT ( 'NONE',  ( 1.174540682414699111, -0.3162353388693405765, 0.4822834645669290543 ) ) ;
#44172 = CARTESIAN_POINT ( 'NONE',  ( -0.1070741851644056997, 0.3996062992125986035, -0.9514435695538056015 ) ) ;
#44173 = CARTESIAN_POINT ( 'NONE',  ( -1.410761154855642463, -0.05778040916215522460, 0.4822834645669289988 ) ) ;
#44174 = CARTESIAN_POINT ( 'NONE',  ( -0.1070741851644056997, 0.3996062992125984925, -0.3982939632545932085 ) ) ;
#44175 = CARTESIAN_POINT ( 'NONE',  ( 0.1998031496062992463, 0.3460692066303959202, -0.06364829396325462352 ) ) ;
#44176 = CARTESIAN_POINT ( 'NONE',  ( -0.2690288713910754526, 0.2952755905511810774, -0.1292274648535930714 ) ) ;
#44177 = CARTESIAN_POINT ( 'NONE',  ( -0.1998031496062994683, 0.3460692066303958092, -2.847769028871391050 ) ) ;
#44178 = EDGE_CURVE ( 'NONE', #55060, #26586, #24569, .T. ) ;
#44179 = CARTESIAN_POINT ( 'NONE',  ( 0.1049643490035304938, -0.3917322834645669549, -1.587270341207349222 ) ) ;
#44180 = CARTESIAN_POINT ( 'NONE',  ( 1.535433070866142558, 0.2952755905511811885, 0.000000000000000000 ) ) ;
#44181 = CARTESIAN_POINT ( 'NONE',  ( -0.01312335958005186876, -0.004921259842519870586, -0.3153832671262229437 ) ) ;
#44182 = CARTESIAN_POINT ( 'NONE',  ( 0.7283464566929140904, -0.5400638737290845981, -0.3530559997133363437 ) ) ;
#44183 = CARTESIAN_POINT ( 'NONE',  ( -0.2362204724409451284, 0.4091458600556402425, -1.349737532808398921 ) ) ;
#44184 = CARTESIAN_POINT ( 'NONE',  ( 0.4855643044619430415, -0.3690944881889765550, -0.3153832671262227771 ) ) ;
#44185 = CARTESIAN_POINT ( 'NONE',  ( 0.5446194225721792126, -0.05778040916215560624, -0.4822834645669293319 ) ) ;
#44186 = EDGE_CURVE ( 'NONE', #5541, #82322, #9955, .T. ) ;
#44187 = CARTESIAN_POINT ( 'NONE',  ( -0.2891555358219909388, -0.2891555358219912164, -1.080708661417322913 ) ) ;
#44188 = CARTESIAN_POINT ( 'NONE',  ( -0.9776902887139098386, -0.6692913385826771977, 0.1292274648535927661 ) ) ;
#44189 = CARTESIAN_POINT ( 'NONE',  ( -0.4091458600556402980, -0.2362204724409451284, -1.074146981627296604 ) ) ;
#44190 = CARTESIAN_POINT ( 'NONE',  ( 0.7349081364829402885, -0.5023911411419708095, -0.1820866141732282451 ) ) ;
#44191 = CARTESIAN_POINT ( 'NONE',  ( -1.112371124080194340, -2.567464376874931580E-15, -0.4445507791589072832 ) ) ;
#44192 = CARTESIAN_POINT ( 'NONE',  ( -0.3740157480314953431, -0.5400638737290845981, -0.3530559997133363437 ) ) ;
#44193 = CARTESIAN_POINT ( 'NONE',  ( 0.1902887139107617975, -0.5511811023622048555, -0.09757992244046775898 ) ) ;
#44194 = CARTESIAN_POINT ( 'NONE',  ( -2.873989802184792719, 1.063020117359138705, 0.01785754392583522449 ) ) ;
#44195 = CARTESIAN_POINT ( 'NONE',  ( -0.1377952755905504645, 0.1660481256975885056, 0.3530559997133364547 ) ) ;
#44196 = CARTESIAN_POINT ( 'NONE',  ( 0.2952755905511816326, -0.4536011799217367080, 0.2665933059059888421 ) ) ;
#44197 = CARTESIAN_POINT ( 'NONE',  ( 4.893765752498283308E-17, -0.3996062992125985480, -1.887795275590551158 ) ) ;
#44198 = CARTESIAN_POINT ( 'NONE',  ( 0.2559055118110243332, 0.1660481256975885056, 0.3530559997133364547 ) ) ;
#44199 = CARTESIAN_POINT ( 'NONE',  ( 0.9776902887139113929, -0.5511811023622048555, -0.09757992244046775898 ) ) ;
#44200 = DIRECTION ( 'NONE',  ( -0.000000000000000000, -1.000000000000000000, -0.000000000000000000 ) ) ;
#44201 = CARTESIAN_POINT ( 'NONE',  ( -0.2887139107611542133, 0.1283753931104748280, 0.1820866141732283561 ) ) ;
#44202 = CARTESIAN_POINT ( 'NONE',  ( -0.8530183727034112984, -0.3690944881889765550, -0.3153832671262227771 ) ) ;
#44203 = CARTESIAN_POINT ( 'NONE',  ( -0.4002624671916004129, -0.3162353388693405765, 0.4822834645669290543 ) ) ;
#44204 = CARTESIAN_POINT ( 'NONE',  ( 0.2230971128608929543, 0.05413385826771626580, -0.4176697321401330321 ) ) ;
#44205 = CARTESIAN_POINT ( 'NONE',  ( 1.049868766404200349, 0.1283753931104748280, 0.1820866141732283561 ) ) ;
#44206 = DIRECTION ( 'NONE',  ( -3.491481338843133355E-15, -0.000000000000000000, 1.000000000000000000 ) ) ;
#44207 = CARTESIAN_POINT ( 'NONE',  ( -1.732283464566928277, -0.1870078740157479769, 0.4822834645669291653 ) ) ;
#44208 = CARTESIAN_POINT ( 'NONE',  ( 0.6167979002624679463, 0.05413385826771626580, -0.4176697321401330321 ) ) ;
#44209 = CARTESIAN_POINT ( 'NONE',  ( -1.614173228346456712, 1.818966223839196816, -0.1372047244094478091 ) ) ;
#44210 = CARTESIAN_POINT ( 'NONE',  ( -0.4396325459317579898, 0.2952755905511811885, 0.1292274648535926551 ) ) ;
#44211 = CARTESIAN_POINT ( 'NONE',  ( -0.3917322834645671215, 0.1049643490035301469, -1.062335958005249603 ) ) ;
#44212 = CARTESIAN_POINT ( 'NONE',  ( 0.8661417322834653598, -0.1870078740157479769, 0.4822834645669291653 ) ) ;
#44213 = CARTESIAN_POINT ( 'NONE',  ( 0.4265091863517067594, 0.2952755905511811885, 0.1292274648535926551 ) ) ;
#44214 = CARTESIAN_POINT ( 'NONE',  ( 1.868118615532832649, 2.729653127095272414, -0.5314960629921260393 ) ) ;
#44215 = CARTESIAN_POINT ( 'NONE',  ( 0.3149606299212606708, -0.1870078740157480601, -0.3641732283464567677 ) ) ;
#44216 = CARTESIAN_POINT ( 'NONE',  ( 1.220472440944882608, 0.2952755905511811885, 0.000000000000000000 ) ) ;
#44217 = CARTESIAN_POINT ( 'NONE',  ( -0.4461942257217840213, 0.1283753931104748280, 0.1820866141732283561 ) ) ;
#44218 = CARTESIAN_POINT ( 'NONE',  ( -0.2165354330708654795, 0.1660481256975885056, 0.3530559997133364547 ) ) ;
#44219 = DIRECTION ( 'NONE',  ( 0.000000000000000000, -0.4999999999999998335, -0.8660254037844385966 ) ) ;
#44220 = CARTESIAN_POINT ( 'NONE',  ( 0.3543307086614179147, 0.2952755905511811885, 0.000000000000000000 ) ) ;
#44221 = CARTESIAN_POINT ( 'NONE',  ( -0.6299212598425188991, -0.1870078740157480879, -0.4822834645669291653 ) ) ;
#44222 = CARTESIAN_POINT ( 'NONE',  ( -0.6824146981627291497, -0.5023911411419708095, -0.1820866141732282451 ) ) ;
#44223 = CARTESIAN_POINT ( 'NONE',  ( 0.5905511811023629321, -0.6692913385826771977, 8.415575281601705876E-17 ) ) ;
#44224 = CARTESIAN_POINT ( 'NONE',  ( -1.299212598425196097, -0.6692913385826771977, 8.415575281601705876E-17 ) ) ;
#44225 = CARTESIAN_POINT ( 'NONE',  ( -0.1640419947506553400, -0.05778040916215560624, -0.4822834645669293319 ) ) ;
#44226 = CARTESIAN_POINT ( 'NONE',  ( 1.128608923884514947, 0.1539470093639523085, 0.1968503937007873850 ) ) ;
#44228 = CARTESIAN_POINT ( 'NONE',  ( 1.246719160104987623, -0.4281496062992124485, 0.4176697321401328655 ) ) ;
#44227 = FACE_OUTER_BOUND ( 'NONE', #76300, .T. ) ;
#44229 = CARTESIAN_POINT ( 'NONE',  ( 1.187664041994751285, -0.05778040916215522460, 0.4822834645669289988 ) ) ;
#44230 = CARTESIAN_POINT ( 'NONE',  ( -9.594673741351313045E-17, 0.3917322834645670104, -2.196850393700787496 ) ) ;
#44231 = PLANE ( 'NONE',  #44825 ) ;
#44232 = CARTESIAN_POINT ( 'NONE',  ( -0.9973753280839886548, -0.6046776061558809534, -0.2411417322834644161 ) ) ;
#44233 = B_SPLINE_CURVE_WITH_KNOTS ( 'NONE', 3,
 ( #69193, #62459, #62879, #73866, #48170, #48997, #74278 ),
 .UNSPECIFIED., .F., .F.,
 ( 4, 3, 4 ),
 ( 3.469446951953614189E-18, 0.001246230184515571739, 0.002492489877932648097 ),
 .UNSPECIFIED. ) ;
#44234 = CARTESIAN_POINT ( 'NONE',  ( -0.4724409448818899238, 0.1265901696524986686, -0.5052493438320209140 ) ) ;
#44235 = CARTESIAN_POINT ( 'NONE',  ( -0.3949938075777409408, -0.1058382717557502933, -2.723097112860892732 ) ) ;
#44236 = EDGE_LOOP ( 'NONE', ( #65340, #22729, #56790, #72850 ) ) ;
#44237 = CARTESIAN_POINT ( 'NONE',  ( -0.2887139107611542133, -0.5023911411419708095, -0.1820866141732282451 ) ) ;
#44238 = CARTESIAN_POINT ( 'NONE',  ( -0.3392501089628017219, -0.1958661417322836718, -1.461942257217847763 ) ) ;
#44239 = CARTESIAN_POINT ( 'NONE',  ( 0.5314960629921264834, 0.1660481256975883668, -0.3530559997133364547 ) ) ;
#44240 = CARTESIAN_POINT ( 'NONE',  ( -0.3458507752293909498, 0.3458507752293907833, -2.854330708661417138 ) ) ;
#44241 = CARTESIAN_POINT ( 'NONE',  ( -0.5411721830064186722, -2.191421614605370878E-15, 0.4445507791589071167 ) ) ;
#44242 = CARTESIAN_POINT ( 'NONE',  ( -0.5249343832020990641, 0.1283753931104748280, 0.1820866141732283561 ) ) ;
#44243 = CYLINDRICAL_SURFACE ( 'NONE', #45366, 0.4744094488188972947 ) ;
#44244 = CARTESIAN_POINT ( 'NONE',  ( 1.161417322834646493, -0.5400638737290844871, 0.3530559997133364547 ) ) ;
#44245 = CARTESIAN_POINT ( 'NONE',  ( 0.7874015748031503170, -0.1870078740157479769, 0.3641732283464567677 ) ) ;
#44246 = CARTESIAN_POINT ( 'NONE',  ( -0.1837270341207340729, 0.2306618581243847221, -0.2411417322834647770 ) ) ;
#44247 = CARTESIAN_POINT ( 'NONE',  ( 0.3917322834645668994, 0.1049643490035304522, -0.6771460385488696776 ) ) ;
#44248 = CARTESIAN_POINT ( 'NONE',  ( -0.3608923884514428360, 0.2952755905511811885, 0.1292274648535926551 ) ) ;
#44249 = CARTESIAN_POINT ( 'NONE',  ( -1.515748031496062076, 0.07958543189024071263, -0.2665933059059888421 ) ) ;
#44250 = CARTESIAN_POINT ( 'NONE',  ( -0.5118110236220466680, -0.6692913385826771977, 8.415575281601705876E-17 ) ) ;
#44251 = CARTESIAN_POINT ( 'NONE',  ( 1.666666666666667185, 0.05413385826771666132, 0.4176697321401328100 ) ) ;
#44252 = CARTESIAN_POINT ( 'NONE',  ( -0.2516118885077178735, 1.134065313995066493, -1.915546005056554035 ) ) ;
#44253 = ORIENTED_EDGE ( 'NONE', *, *, #61823, .F. ) ;
#44254 = CARTESIAN_POINT ( 'NONE',  ( -0.3392501089628017219, -0.1958661417322836995, -2.253956323655855076 ) ) ;
#44255 = CARTESIAN_POINT ( 'NONE',  ( 0.6102362204724416372, 0.1660481256975883668, -0.3530559997133364547 ) ) ;
#44256 = ORIENTED_EDGE ( 'NONE', *, *, #80061, .F. ) ;
#44257 = CARTESIAN_POINT ( 'NONE',  ( -0.9711286089238838626, -0.6046776061558807314, 0.2411417322834647770 ) ) ;
#44258 = CARTESIAN_POINT ( 'NONE',  ( 1.614173228346457378, 0.2952755905511811885, 0.000000000000000000 ) ) ;
#44259 = CARTESIAN_POINT ( 'NONE',  ( 0.5052493438320215802, 0.2952755905511811885, 0.1292274648535926551 ) ) ;
#44260 = CARTESIAN_POINT ( 'NONE',  ( -0.09842519685039295696, -0.5400638737290844871, 0.3530559997133364547 ) ) ;
#44261 = CARTESIAN_POINT ( 'NONE',  ( -0.1049643490035307020, 0.3917322834645669549, -1.508530183727033736 ) ) ;
#44262 = CARTESIAN_POINT ( 'NONE',  ( -0.7020997375328076329, -0.3162353388693409650, -0.4822834645669289433 ) ) ;
#44263 = CARTESIAN_POINT ( 'NONE',  ( -0.1509186351706028884, -0.3162353388693409650, -0.4822834645669289433 ) ) ;
#44264 = CARTESIAN_POINT ( 'NONE',  ( -0.8136482939632537770, 0.2306618581243847221, -0.2411417322834647770 ) ) ;
#44265 = CARTESIAN_POINT ( 'NONE',  ( 0.2624671916010504757, 0.1283753931104748280, 0.1820866141732283561 ) ) ;
#44266 = CARTESIAN_POINT ( 'NONE',  ( -0.2430399508222474692, -0.1677739497468299645, 5.760042173782278674 ) ) ;
#44267 = CARTESIAN_POINT ( 'NONE',  ( -0.03280839895013062252, -0.6692913385826771977, 0.1292274648535927661 ) ) ;
#44268 = DIRECTION ( 'NONE',  ( 0.000000000000000000, 1.000000000000000000, -0.000000000000000000 ) ) ;
#44269 = CARTESIAN_POINT ( 'NONE',  ( 1.312335958005249825, 0.2306618581243847221, -0.2411417322834647770 ) ) ;
#44270 = CARTESIAN_POINT ( 'NONE',  ( -0.3392501089628017219, -0.1958661417322836718, -2.879265091863516979 ) ) ;
#44271 = ORIENTED_EDGE ( 'NONE', *, *, #35758, .T. ) ;
#44272 = EDGE_CURVE ( 'NONE', #28560, #64172, #2222, .T. ) ;
#44273 = VERTEX_POINT ( 'NONE', #49487 ) ;
#44274 = CARTESIAN_POINT ( 'NONE',  ( 0.2165354330708668673, -0.5400638737290844871, 0.3530559997133364547 ) ) ;
#44275 = CARTESIAN_POINT ( 'NONE',  ( 0.1968503937007881344, 0.1771653543307087630, 0.000000000000000000 ) ) ;
#44277 = CARTESIAN_POINT ( 'NONE',  ( -0.4091458600556402980, -0.2362204724409451284, -0.3674540682414698112 ) ) ;
#44276 = CARTESIAN_POINT ( 'NONE',  ( 1.469816272965879911, -0.5023911411419708095, 0.1820866141732285504 ) ) ;
#44278 = CARTESIAN_POINT ( 'NONE',  ( 0.3917322834645669549, 0.1049643490035304660, -1.154199475065616820 ) ) ;
#44279 = CARTESIAN_POINT ( 'NONE',  ( -0.2362204724409447953, -0.4091458600556404646, 0.01509186351706036204 ) ) ;
#44280 = PLANE ( 'NONE',  #64720 ) ;
#44281 = CARTESIAN_POINT ( 'NONE',  ( 1.548556430446194954, -0.6046776061558807314, 0.2411417322834647770 ) ) ;
#44282 = CARTESIAN_POINT ( 'NONE',  ( -0.1998031496062991630, -0.3460692066303959202, -2.819553805774277944 ) ) ;
#44283 = CARTESIAN_POINT ( 'NONE',  ( 0.5249343832021003964, 0.2306618581243847221, -0.2411417322834647770 ) ) ;
#44284 = CARTESIAN_POINT ( 'NONE',  ( -1.036745406824146176, -0.4281496062992124485, 0.4176697321401328655 ) ) ;
#44285 = CARTESIAN_POINT ( 'NONE',  ( -1.213910761154854745, 0.2952755905511810774, -0.1292274648535930714 ) ) ;
#44286 = CARTESIAN_POINT ( 'NONE',  ( 0.2099737532808405305, 0.2306618581243847221, -0.2411417322834647770 ) ) ;
#44287 = CARTESIAN_POINT ( 'NONE',  ( 1.082677165354331228, -0.5400638737290844871, 0.3530559997133364547 ) ) ;
#44288 = CARTESIAN_POINT ( 'NONE',  ( 1.391076115485564868, 0.1283753931104746893, -0.1820866141732285504 ) ) ;
#44289 = CARTESIAN_POINT ( 'NONE',  ( 0.6364829396325465405, -0.2845877964562161244, -0.3641732283464567121 ) ) ;
#44290 = CARTESIAN_POINT ( 'NONE',  ( -0.9580052493438311334, 0.05413385826771626580, -0.4176697321401330321 ) ) ;
#44291 = CARTESIAN_POINT ( 'NONE',  ( 0.3996062992125984925, 0.1070741851644054637, -0.6738845144356955252 ) ) ;
#44292 = CARTESIAN_POINT ( 'NONE',  ( 1.463254593175853824, -0.6692913385826771977, 0.1292274648535927661 ) ) ;
#44293 = CARTESIAN_POINT ( 'NONE',  ( 4.797336870675656522E-17, -0.3917322834645670104, -0.2283464566929133410 ) ) ;
#44295 = CARTESIAN_POINT ( 'NONE',  ( 1.604771003085129433, 0.7690346235818160681, -0.1466069496707749498 ) ) ;
#44294 = CARTESIAN_POINT ( 'NONE',  ( 0.8202099737532814183, -0.6692913385826773087, -0.1292274648535924053 ) ) ;
#44296 = CARTESIAN_POINT ( 'NONE',  ( -1.594488188976377563, -0.4536011799217367080, 0.2665933059059888421 ) ) ;
#44297 = CARTESIAN_POINT ( 'NONE',  ( 0.07217847769028949700, -0.3162353388693405765, 0.4822834645669290543 ) ) ;
#44298 = CARTESIAN_POINT ( 'NONE',  ( 1.062992125984252745, -0.5511811023622047445, 6.969142054262312111E-17 ) ) ;
#44299 = CARTESIAN_POINT ( 'NONE',  ( -1.732283464566928277, -0.1870078740157479769, 0.3641732283464567677 ) ) ;
#44300 = CARTESIAN_POINT ( 'NONE',  ( 0.8333333333333340365, -0.6692913385826771977, 0.1292274648535927661 ) ) ;
#44301 = DIRECTION ( 'NONE',  ( -3.491481338843132961E-15, -0.000000000000000000, 1.000000000000000000 ) ) ;
#44302 = CARTESIAN_POINT ( 'NONE',  ( -0.6889763779527552368, -0.4536011799217368745, -0.2665933059059886201 ) ) ;
#44303 = CARTESIAN_POINT ( 'NONE',  ( -0.6167979002624665030, 0.05413385826771666132, 0.4176697321401328100 ) ) ;
#44304 = CARTESIAN_POINT ( 'NONE',  ( 1.515748031496063408, 0.1660481256975885056, 0.3530559997133364547 ) ) ;
#44305 = ADVANCED_FACE ( 'NONE', ( #73528 ), #48245, .F. ) ;
#44306 = CARTESIAN_POINT ( 'NONE',  ( -1.325459317585300889, -0.4281496062992127816, -0.4176697321401328100 ) ) ;
#44307 = CARTESIAN_POINT ( 'NONE',  ( 1.351706036745407680, 0.05413385826771666132, 0.4176697321401328100 ) ) ;
#44308 = CARTESIAN_POINT ( 'NONE',  ( 4.797336870675656522E-17, -0.3917322834645670659, -0.8628802081702905413 ) ) ;
#44309 = CARTESIAN_POINT ( 'NONE',  ( -1.410761154855641575, -0.2845877964562161244, -0.3641732283464567121 ) ) ;
#44310 = DIRECTION ( 'NONE',  ( 1.000000000000000000, 0.000000000000000000, 0.000000000000000000 ) ) ;
#44311 = CARTESIAN_POINT ( 'NONE',  ( 1.135170603674541256, 0.2952755905511811885, 0.1292274648535926551 ) ) ;
#44312 = CARTESIAN_POINT ( 'NONE',  ( -0.4091458600556405756, 0.2362204724409446288, -2.465223097112860806 ) ) ;
#44313 = CARTESIAN_POINT ( 'NONE',  ( -1.614173228346456268, -0.6692913385826771977, 8.415575281601705876E-17 ) ) ;
#44314 = CARTESIAN_POINT ( 'NONE',  ( -1.496062992125983815, -0.1870078740157479769, 0.3641732283464567677 ) ) ;
#44315 = CARTESIAN_POINT ( 'NONE',  ( -0.9908136482939626788, -0.5511811023622048555, -0.09757992244046775898 ) ) ;
#44316 = CARTESIAN_POINT ( 'NONE',  ( 1.170403185795211742, -4.479759449472349425E-16, -0.4118484887281964046 ) ) ;
#44317 = CARTESIAN_POINT ( 'NONE',  ( -0.5774278215223089816, -0.6046776061558807314, 0.2411417322834647770 ) ) ;
#44318 = CARTESIAN_POINT ( 'NONE',  ( -0.1246719160104980823, -0.5511811023622048555, -0.09757992244046775898 ) ) ;
#44319 = CARTESIAN_POINT ( 'NONE',  ( -1.627296587926508442, -0.5023911411419708095, -0.1820866141732282451 ) ) ;
#44320 = CARTESIAN_POINT ( 'NONE',  ( 0.9120734908136489683, -0.5511811023622046335, 0.09757992244046803654 ) ) ;
#44321 = CARTESIAN_POINT ( 'NONE',  ( 0.7808398950131241190, -0.05778040916215560624, -0.4822834645669293319 ) ) ;
#44322 = CARTESIAN_POINT ( 'NONE',  ( 1.541994750656168645, -0.6692913385826771977, 0.1292274648535927661 ) ) ;
#44323 = CARTESIAN_POINT ( 'NONE',  ( 0.1312335958005257930, 0.1283753931104746893, -0.1820866141732285504 ) ) ;
#44324 = CARTESIAN_POINT ( 'NONE',  ( 0.4921259842519691285, -0.5400638737290845981, -0.3530559997133363437 ) ) ;
#44325 = CARTESIAN_POINT ( 'NONE',  ( 0.3937007874015754361, -0.1870078740157480601, -0.3641732283464567677 ) ) ;
#44326 = ORIENTED_EDGE ( 'NONE', *, *, #35131, .T. ) ;
#44327 = CARTESIAN_POINT ( 'NONE',  ( -1.568241469816272105, -0.3162353388693409650, -0.4822834645669289433 ) ) ;
#44328 = EDGE_CURVE ( 'NONE', #66982, #69770, #17117, .T. ) ;
#44329 = CARTESIAN_POINT ( 'NONE',  ( -1.325459317585300889, 0.05413385826771666132, 0.4176697321401328100 ) ) ;
#44330 = CARTESIAN_POINT ( 'NONE',  ( -0.5839895013123351797, 0.2952755905511810774, -0.1292274648535930714 ) ) ;
#44331 = CARTESIAN_POINT ( 'NONE',  ( 0.1998031496062994405, -0.3460692066303958092, -0.4068241469816273326 ) ) ;
#44332 = CARTESIAN_POINT ( 'NONE',  ( 0.1998031496062992463, 0.3460692066303959202, -2.583333333333333481 ) ) ;
#44333 = CARTESIAN_POINT ( 'NONE',  ( 0.4002624671916016896, -0.3162353388693409650, -0.4822834645669289433 ) ) ;
#44334 = CARTESIAN_POINT ( 'NONE',  ( 0.9711286089238851948, 0.1283753931104748280, 0.1820866141732283561 ) ) ;
#44335 = CARTESIAN_POINT ( 'NONE',  ( -0.3477690288713902178, 0.2952755905511810774, -0.1292274648535930714 ) ) ;
#44336 = CARTESIAN_POINT ( 'NONE',  ( 0.1509186351706042484, -0.3162353388693405765, 0.4822834645669290543 ) ) ;
#44337 = CARTESIAN_POINT ( 'NONE',  ( -0.3460692066303960868, 0.1998031496062990242, -2.073490813648294129 ) ) ;
#44338 = CARTESIAN_POINT ( 'NONE',  ( 0.3420746716998659953, 0.1974969037888705536, -1.391076115485564424 ) ) ;
#44339 = CARTESIAN_POINT ( 'NONE',  ( 0.1070741851644054915, -0.3996062992125986035, -2.762467191601049255 ) ) ;
#44340 = DIRECTION ( 'NONE',  ( -0.000000000000000000, -0.6853444168423467042, -0.7282190812544145908 ) ) ;
#44341 = CARTESIAN_POINT ( 'NONE',  ( 0.1958661417322836440, -0.3392501089628017219, -0.7139107611548556331 ) ) ;
#44342 = CARTESIAN_POINT ( 'NONE',  ( -0.7349081364829390672, 0.1283753931104746893, -0.1820866141732285504 ) ) ;
#44343 = CARTESIAN_POINT ( 'NONE',  ( -1.161417322834644716, -0.5400638737290845981, -0.3530559997133363437 ) ) ;
#44344 = CARTESIAN_POINT ( 'NONE',  ( 0.2891555358219910499, -0.2891555358219909944, -2.379921259842519898 ) ) ;
#44345 = CARTESIAN_POINT ( 'NONE',  ( 0.6627296587926517768, -0.6692913385826773087, -0.1292274648535924053 ) ) ;
#44346 = CARTESIAN_POINT ( 'NONE',  ( 1.286089238845145033, 0.2306618581243848609, 0.2411417322834645549 ) ) ;
#44347 = CARTESIAN_POINT ( 'NONE',  ( 0.9580052493438326877, 0.05413385826771666132, 0.4176697321401328100 ) ) ;
#44348 = CARTESIAN_POINT ( 'NONE',  ( 0.4724409448818898682, 2.892866454678787531E-17, -0.03740157480314962313 ) ) ;
#44349 = CARTESIAN_POINT ( 'NONE',  ( 0.1070741851644054915, -0.3996062992125986035, -2.132545931758530244 ) ) ;
#44350 = CARTESIAN_POINT ( 'NONE',  ( 1.515748031496063408, 0.1660481256975885056, 0.3530559997133364547 ) ) ;
#44351 = CARTESIAN_POINT ( 'NONE',  ( 0.7742782152230978099, -0.4281496062992124485, 0.4176697321401328655 ) ) ;
#44352 = CARTESIAN_POINT ( 'NONE',  ( 0.4593175853018379162, -0.4281496062992124485, 0.4176697321401328655 ) ) ;
#44353 = CARTESIAN_POINT ( 'NONE',  ( 0.7545931758530188826, -0.5511811023622046335, 0.09757992244046803654 ) ) ;
#44354 = CARTESIAN_POINT ( 'NONE',  ( 1.135170603674541256, -0.6692913385826773087, -0.1292274648535924053 ) ) ;
#44355 = CARTESIAN_POINT ( 'NONE',  ( 0.3917322834645670104, -0.1049643490035303411, -0.1961942257217848817 ) ) ;
#44356 = SURFACE_STYLE_FILL_AREA ( #17085 ) ;
#44357 = CARTESIAN_POINT ( 'NONE',  ( 0.6036745406824154392, 0.2306618581243847221, -0.2411417322834647770 ) ) ;
#44358 = CARTESIAN_POINT ( 'NONE',  ( 1.660104986876641320, -0.08942795157527998196, 0.3641732283464567121 ) ) ;
#44359 = CARTESIAN_POINT ( 'NONE',  ( -0.7939632545931754048, -0.3162353388693405765, 0.4822834645669290543 ) ) ;
#44360 = CARTESIAN_POINT ( 'NONE',  ( -0.9711286089238838626, -0.6046776061558807314, 0.2411417322834647770 ) ) ;
#44361 = CARTESIAN_POINT ( 'NONE',  ( 1.240157480314961314, -0.5400638737290844871, 0.3530559997133364547 ) ) ;
#44362 = CARTESIAN_POINT ( 'NONE',  ( 0.1958661417322836440, -0.3392501089628017219, -0.4914698162729659869 ) ) ;
#44363 = CARTESIAN_POINT ( 'NONE',  ( 0.2867679344610365999, -0.2867679344610365444, -1.350393700787401619 ) ) ;
#44364 = CARTESIAN_POINT ( 'NONE',  ( 0.3917322834645670104, 2.398668435337828261E-17, -2.787401574803149096 ) ) ;
#44365 = ORIENTED_EDGE ( 'NONE', *, *, #20359, .T. ) ;
#44366 = CARTESIAN_POINT ( 'NONE',  ( -0.1070741851644051862, -0.3996062992125987146, 0.08530183727034119923 ) ) ;
#44367 = ORIENTED_EDGE ( 'NONE', *, *, #14488, .T. ) ;
#44368 = CARTESIAN_POINT ( 'NONE',  ( 1.594488188976378673, -0.5400638737290845981, -0.3530559997133363437 ) ) ;
#44369 = CARTESIAN_POINT ( 'NONE',  ( 1.430446194225722500, -0.004921259842519576551, 0.3153832671262227771 ) ) ;
#44370 = CARTESIAN_POINT ( 'NONE',  ( 0.2925321140481932369, 0.2925321140481932369, -1.555118110236220597 ) ) ;
#44371 = CARTESIAN_POINT ( 'NONE',  ( 1.259842519685040019, -0.1870078740157480601, -0.3641732283464567677 ) ) ;
#44372 = CARTESIAN_POINT ( 'NONE',  ( 0.4606732211678798428, 1.541615089183433485, -0.5309055118110237448 ) ) ;
#44373 = DIRECTION ( 'NONE',  ( -3.096699300667737957E-16, 1.000000000000000000, -0.000000000000000000 ) ) ;
#44374 = CARTESIAN_POINT ( 'NONE',  ( -0.01578888928619379128, 1.954428616053096146, 0.3129921259842520787 ) ) ;
#44375 = CARTESIAN_POINT ( 'NONE',  ( -0.3917322834645671215, 0.1049643490035301469, -0.7473753280839893209 ) ) ;
#44376 = CARTESIAN_POINT ( 'NONE',  ( -0.5774278215223089816, -0.5023911411419708095, 0.1820866141732285504 ) ) ;
#44377 = CARTESIAN_POINT ( 'NONE',  ( -1.561679790026246017, -0.004921259842519576551, 0.3153832671262227771 ) ) ;
#44378 = CARTESIAN_POINT ( 'NONE',  ( -1.167979002624671470, 0.05413385826771666132, 0.4176697321401328100 ) ) ;
#44379 = CARTESIAN_POINT ( 'NONE',  ( 0.2099737532808405305, 0.2306618581243847221, -0.2411417322834647770 ) ) ;
#44380 = CARTESIAN_POINT ( 'NONE',  ( 1.358267716535433323, -0.5400638737290845981, -0.3530559997133363437 ) ) ;
#44381 = ORIENTED_EDGE ( 'NONE', *, *, #58316, .F. ) ;
#44382 = DIRECTION ( 'NONE',  ( 1.000000000000000000, 0.000000000000000000, 0.000000000000000000 ) ) ;
#44383 = CARTESIAN_POINT ( 'NONE',  ( -0.3458507752293906723, -0.3458507752293910609, -2.106299212598425452 ) ) ;
#44384 = FACE_OUTER_BOUND ( 'NONE', #18916, .T. ) ;
#44385 =( BOUNDED_SURFACE ( )  B_SPLINE_SURFACE ( 1, 2, ( 
 ( #57786, #11548, #24571, #6040, #38026, #18677, #31295, #6458, #37204, #62885, #51051, #44322, #63288, #64535, #5220, #56551, #82252, #63701, #69612, #150, #57372, #12367, #56959, #50237, #573, #83067, #11958, #75933, #70857, #24971, #32128, #37613, #25388, #5628, #50643, #70012, #70427, #19082, #44731, #12783, #51466, #58206, #19500, #13208, #45154, #38855, #8138, #27899, #45578, #79268, #27481, #72524, #46413, #26226, #53139, #65805, #66626, #21583, #59055, #60302, #1820, #8964, #19928, #39272, #52307, #71271, #1409, #33803, #47246, #78013, #20341, #65389, #78850, #34638, #7724, #58631, #51890, #27065, #59881, #77594, #33393, #40947, #53560, #21177, #72935, #20763, #13618, #64956, #59468, #7294, #46832, #52724, #15287, #32964, #999, #14873, #26653, #45993, #71690, #40534, #8552, #66213, #14041, #34218, #2235, #78436, #39698, #72107, #14465, #40117, #48901, #53971, #68287, #35876, #73777, #2652, #10623, #79684, #60710, #42176, #74184, #29140, #67452, #42587, #22001, #47661, #3887, #54806, #16113, #17360, #73356, #15704, #41361, #16531, #54388, #36279, #67870, #48483, #9786, #67042, #36682, #10208, #80099, #9374, #23642, #35457, #16945, #28727, #61543, #48075, #22418, #3059, #23230, #35045, #28309, #74602, #41757, #11025, #61122, #49312, #29547, #3473, #55209, #4291, #80510, #55618, #80917, #61951, #22825, #29953, #81328, #75014, #42989, #68683, #11858, #13100, #37922, #45048, #56036, #75421, #5118, #24054, #37511, #5525, #12264, #82964, #38337, #43395, #70323, #31190, #63186, #62358, #44220, #63598, #18978, #46, #82150, #5935, #56855, #31605, #69095, #44627, #11443, #64012, #25699, #37099, #57265, #4695, #62784, #50131, #50539, #76243, #24871, #18577, #30369, #69910, #30785, #25282, #19397, #81744, #70749, #77063, #56448, #50950, #49724, #17764, #69509, #24466, #75831, #82553, #51360, #18172, #12678, #32024, #76647, #6353, #43805, #57684, #60915, #13509, #13936, #28927, #19822, #28519, #73568, #34844, #60507, #79889, #54175, #28106, #15493, #3266, #6765, #34428, #60093, #77908, #45887, #79471, #48279, #21787, #47449, #80305, #54596, #7621, #2855, #77487, #53760, #73144, #41151, #15913, #32437, #66839, #22207, #73977, #9582, #22620, #38754, #58100, #894, #26122, #9173, #67250, #47864, #41561, #45471, #64431, #35251, #71169, #64850, #52204, #465, #20239, #51783, #39165, #7187, #32860, #58528, #26551, #71585, #39594, #65282, #2448, #55828, #81536, #35663, #61327, #3681, #42788, #75630, #24259, #36898, #74810, #36482, #80713, #23855, #49932, #50340, #29346, #55005, #23028, #36077, #42376, #43605, #17968, #43192, #37315, #10822, #16323, #82354, #49522, #48694, #75215, #81123, #62988, #74392, #69307, #68888, #67661, #41968, #9998, #4916, #81946, #17560, #24672, #11238, #11657, #17155, #5327, #16736, #62574, #62157, #30584, #68075, #30985, #56250, #4085, #10419, #56653, #61748, #29753, #55416, #4498, #68483, #23440, #49104, #30165, #44023, #77273, #19185, #6142, #7403, #69716, #12060, #37718, #64227, #44422, #678, #6561, #38547, #57477, #31398, #26754, #57891, #70117, #63392, #13726, #83171, #6979, #18779, #32233, #38130, #12468, #76452, #13306, #57063, #76037, #38958, #18382, #1103, #5727, #39380, #258, #82756, #25910, #77699, #25078, #45680, #19602, #64642, #12887, #50752, #45265, #51570, #33072, #71376, #25491, #63804, #70961, #58741, #31817, #51157, #76852, #44834, #70532, #32648, #58313, #26332, #51994, #20029, #65065, #78963, #53249, #52409, #34328, #28005, #9078, #59991, #47770, #20869, #46520, #8242, #53665, #60818, #33908, #1516, #78118, #21282, #2760, #3170, #59572, #67154, #22110, #66318, #21691, #1928, #46937, #73469, #27170, #27591, #41469, #33496, #41054, #28419, #47354, #73043, #34749, #66740, #40636, #79372, #15820, #20451, #72629, #14977, #8657, #2349, #15392, #46104, #60409, #54079, #9483, #35158, #79794, #71797, #7829, #14150, #39804, #65497, #59158, #52832, #78544, #72221, #14572, #40224, #65906, #69212, #80210, #74297, #16225, #42700, #56155, #68799, #75127, #35570, #49839, #30074, #61233, #54917, #42283, #81858, #67981, #30490 ),
 ( #55325, #4814, #36803, #49433, #3999, #49017, #9898, #68397, #62479, #62897, #73885, #48188, #41872, #48601, #80623, #24170, #75538, #16643, #55737, #29663, #81445, #3587, #11144, #29253, #17878, #43512, #22935, #4406, #54498, #10324, #35988, #17061, #10736, #74714, #36393, #28834, #62067, #61658, #23760, #11561, #22526, #37218, #67566, #81034, #17472, #23346, #43103, #76359, #24582, #5639, #38036, #70868, #6882, #32138, #18286, #76763, #50657, #13218, #50249, #51475, #44742, #30896, #5232, #75945, #57795, #162, #51063, #56563, #19093, #77178, #63711, #45163, #82264, #19509, #70437, #38864, #69625, #64545, #6468, #6051, #43929, #32552, #37625, #18691, #64134, #38450, #12794, #57384, #11970, #56970, #31306, #63301, #25815, #82668, #24983, #12378, #70025, #31723, #44334, #83078, #25399, #10997, #42965, #61925, #35849, #31162, #62332, #74577, #42150, #18144, #4267, #11417, #23206, #68659, #42559, #48877, #80893, #17738, #61518, #80486, #43367, #22800, #5500, #16507, #43778, #36657, #48459, #4669, #82123, #67845, #50105, #81719, #69067, #17335, #74159, #24029, #30342, #37487, #75802, #29929, #10184, #56008, #63161, #3863, #29523, #16922, #55185, #55592, #23618, #49697, #37072, #56423, #68263, #5093, #49287, #81304, #10599, #75393, #62757, #30761, #24438, #69481, #36255, #74990, #11834, #58073, #65254, #12647, #5907, #82526, #57657, #7161, #7591, #38309, #71558, #58500, #439, #77879, #51333, #56829, #39565, #64403, #63983, #31579, #24844, #19, #32832, #50511, #6320, #13907, #864, #26094, #20210, #77037, #76215, #18551, #6739, #12240, #32410, #31997, #45860, #44196, #26521, #51754, #69886, #37896, #63572, #45444, #39139, #13071, #57235, #77457, #64820, #25673, #52176, #82936, #19792, #19369, #71140, #25258, #50922, #13482, #44600, #76622, #18953, #70295, #45019, #38726, #70719, #79451, #8323, #66398, #40713, #74683, #23315, #35957, #72710, #34406, #78625, #53743, #48984, #49399, #59236, #33574, #27252, #33989, #40305, #42668, #36361, #59651, #15476, #15057, #41133, #20949, #81001, #46606, #17029, #62036, #72302, #73126, #39892, #14648, #2007, #2429, #28085, #60074, #21771, #14232, #47433, #65985, #66824, #55703, #65579, #81411, #30041, #27669, #10290, #23728, #7913, #21363, #1597, #53335, #8736, #4373, #52911, #55292, #68367, #61626, #3968, #79044, #29631, #47016, #10705, #50218, #64103, #56121, #63682, #25369, #69993, #12348, #31691, #6020, #63266, #50623, #12764, #43071, #69592, #11938, #30865, #82233, #68768, #49807, #31275, #24552, #75508, #37593, #70408, #11112, #36769, #76328, #18253, #5201, #6438, #62445, #4781, #30457, #5607, #43481, #83046, #56940, #82637, #56530, #81827, #25785, #24950, #69177, #24137, #38421, #75914, #57350, #17847, #18658, #37185, #11528, #62864, #38004, #43895, #75093, #51032, #17441, #130, #44302, #32110, #76731, #19063, #44711, #57768, #70839, #21159, #52706, #14448, #71671, #51446, #78417, #7707, #8533, #46815, #980, #2217, #27046, #34201, #45135, #64516, #77576, #13188, #26636, #77995, #1392, #72089, #27464, #32523, #59449, #20323, #52290, #77150, #33374, #20746, #8120, #59038, #72506, #19908, #45558, #7276, #46396, #59864, #32947, #555, #19482, #45976, #1801, #38837, #58613, #66196, #53122, #40099, #14855, #14023, #6853, #58185, #65787, #26208, #33785, #39680, #40516, #51870, #78833, #71254, #13600, #39254, #64936, #65372, #10194, #67437, #36266, #35442, #35863, #3045, #55196, #61935, #74170, #22404, #16517, #79251, #61528, #61108, #15689, #27883, #3874, #48469, #29533, #8946, #80903, #54374, #28710, #53543, #9771, #3460, #67856, #29125, #23217, #79667, #21984, #67028, #54793, #21566, #9360, #60286, #47228, #80084, #48887, #72918, #35031, #42572, #74588, #80496, #16932, #48061, #15269, #10609, #22812, #66610, #42161, #60695, #68274, #40930, #34622, #2636, #28293, #53954, #47646, #73341, #41347, #73763, #16098, #41743, #12250, #62771, #31591, #12660, #50523, #82135, #76229, #55603, #69896, #37497, #75404, #4278, #37906, #81315, #62343, #43789, #37085, #4682, #50117, #82950, #23628, #49299, #5510, #30772, #17750, #18963 ) ),
 .UNSPECIFIED., .F., .F., .F. ) 
 B_SPLINE_SURFACE_WITH_KNOTS ( ( 2, 2 ),
 ( 3, 2, 2, 2, 2, 2, 2, 2, 2, 2, 2, 2, 2, 2, 2, 2, 2, 2, 2, 2, 2, 2, 2, 2, 2, 2, 2, 2, 2, 2, 2, 2, 2, 2, 2, 2, 2, 2, 2, 2, 2, 2, 2, 2, 2, 2, 2, 2, 2, 2, 2, 2, 2, 2, 2, 2, 2, 2, 2, 2, 2, 2, 2, 2, 2, 2, 2, 2, 2, 2, 2, 2, 2, 2, 2, 2, 2, 2, 2, 2, 2, 2, 2, 2, 2, 2, 2, 2, 2, 2, 2, 2, 2, 2, 2, 2, 2, 2, 2, 2, 2, 2, 2, 2, 2, 2, 2, 2, 2, 2, 2, 2, 2, 2, 2, 2, 2, 2, 2, 2, 2, 2, 2, 2, 2, 2, 2, 2, 2, 2, 2, 2, 2, 2, 2, 2, 2, 2, 2, 2, 2, 2, 2, 2, 2, 2, 2, 2, 2, 2, 2, 2, 2, 2, 2, 2, 2, 2, 2, 2, 2, 2, 2, 2, 2, 2, 2, 2, 2, 2, 2, 2, 2, 2, 2, 2, 2, 2, 2, 2, 2, 2, 2, 2, 2, 2, 2, 2, 2, 2, 2, 2, 2, 2, 2, 2, 2, 2, 2, 2, 2, 2, 2, 2, 2, 2, 2, 2, 2, 2, 2, 2, 2, 2, 2, 2, 2, 2, 2, 2, 2, 2, 2, 2, 2, 2, 2, 2, 2, 2, 2, 2, 2, 2, 2, 2, 2, 2, 2, 2, 2, 2, 2, 2, 2, 2, 2, 2, 2, 2, 2, 2, 2, 2, 2, 3 ),
 ( 0.000000000000000000, 1.000000000000000000 ),
 ( 0.000000000000000000, 0.003787878787878787984, 0.007575757575757575968, 0.01136363636363636395, 0.01515151515151515194, 0.01893939393939393992, 0.02272727272727272790, 0.02651515151515151589, 0.03030303030303030387, 0.03409090909090908839, 0.03787878787878787984, 0.04166666666666666435, 0.04545454545454545581, 0.04924242424242424032, 0.05303030303030303177, 0.05681818181818181629, 0.06060606060606060774, 0.06439393939393939226, 0.06818181818181817677, 0.07196969696969697516, 0.07575757575757575968, 0.07954545454545454419, 0.08333333333333332871, 0.08712121212121212710, 0.09090909090909091161, 0.09469696969696969613, 0.09848484848484848064, 0.1022727272727272790, 0.1060606060606060635, 0.1098484848484848481, 0.1136363636363636326, 0.1174242424242424310, 0.1212121212121212155, 0.1250000000000000000, 0.1287878787878787845, 0.1325757575757575690, 0.1363636363636363535, 0.1401515151515151381, 0.1439393939393939503, 0.1477272727272727348, 0.1515151515151515194, 0.1553030303030303039, 0.1590909090909090884, 0.1628787878787878729, 0.1666666666666666574, 0.1704545454545454419, 0.1742424242424242542, 0.1780303030303030387, 0.1818181818181818232, 0.1856060606060606077, 0.1893939393939393923, 0.1931818181818181768, 0.1969696969696969613, 0.2007575757575757458, 0.2045454545454545581, 0.2083333333333333426, 0.2121212121212121271, 0.2159090909090909116, 0.2196969696969696961, 0.2234848484848484806, 0.2272727272727272652, 0.2310606060606060497, 0.2348484848484848619, 0.2386363636363636465, 0.2424242424242424310, 0.2462121212121212155, 0.2500000000000000000, 0.2537878787878787845, 0.2575757575757575690, 0.2613636363636363535, 0.2651515151515151381, 0.2689393939393939226, 0.2727272727272727071, 0.2765151515151514916, 0.2803030303030302761, 0.2840909090909091161, 0.2878787878787879007, 0.2916666666666666852, 0.2954545454545454697, 0.2992424242424242542, 0.3030303030303030387, 0.3068181818181818232, 0.3106060606060606077, 0.3143939393939393923, 0.3181818181818181768, 0.3219696969696969613, 0.3257575757575757458, 0.3295454545454545303, 0.3333333333333333148, 0.3371212121212120993, 0.3409090909090908839, 0.3446969696969697239, 0.3484848484848485084, 0.3522727272727272929, 0.3560606060606060774, 0.3598484848484848619, 0.3636363636363636465, 0.3674242424242424310, 0.3712121212121212155, 0.3750000000000000000, 0.3787878787878787845, 0.3825757575757575690, 0.3863636363636363535, 0.3901515151515151381, 0.3939393939393939226, 0.3977272727272727071, 0.4015151515151514916, 0.4053030303030302761, 0.4090909090909091161, 0.4128787878787879007, 0.4166666666666666852, 0.4204545454545454697, 0.4242424242424242542, 0.4280303030303030387, 0.4318181818181818232, 0.4356060606060606077, 0.4393939393939393923, 0.4431818181818181768, 0.4469696969696969613, 0.4507575757575757458, 0.4545454545454545303, 0.4583333333333333148, 0.4621212121212120993, 0.4659090909090908839, 0.4696969696969697239, 0.4734848484848485084, 0.4772727272727272929, 0.4810606060606060774, 0.4848484848484848619, 0.4886363636363636465, 0.4924242424242424310, 0.4962121212121212155, 0.5000000000000000000, 0.5037878787878787845, 0.5075757575757575690, 0.5113636363636363535, 0.5151515151515151381, 0.5189393939393939226, 0.5227272727272727071, 0.5265151515151514916, 0.5303030303030302761, 0.5340909090909090606, 0.5378787878787878451, 0.5416666666666666297, 0.5454545454545454142, 0.5492424242424241987, 0.5530303030303029832, 0.5568181818181817677, 0.5606060606060605522, 0.5643939393939394478, 0.5681818181818182323, 0.5719696969696970168, 0.5757575757575758013, 0.5795454545454545858, 0.5833333333333333703, 0.5871212121212121549, 0.5909090909090909394, 0.5946969696969697239, 0.5984848484848485084, 0.6022727272727272929, 0.6060606060606060774, 0.6098484848484848619, 0.6136363636363636465, 0.6174242424242424310, 0.6212121212121212155, 0.6250000000000000000, 0.6287878787878787845, 0.6325757575757575690, 0.6363636363636363535, 0.6401515151515151381, 0.6439393939393939226, 0.6477272727272727071, 0.6515151515151514916, 0.6553030303030302761, 0.6590909090909090606, 0.6628787878787878451, 0.6666666666666666297, 0.6704545454545454142, 0.6742424242424241987, 0.6780303030303029832, 0.6818181818181817677, 0.6856060606060605522, 0.6893939393939394478, 0.6931818181818182323, 0.6969696969696970168, 0.7007575757575758013, 0.7045454545454545858, 0.7083333333333333703, 0.7121212121212121549, 0.7159090909090909394, 0.7196969696969697239, 0.7234848484848485084, 0.7272727272727272929, 0.7310606060606060774, 0.7348484848484848619, 0.7386363636363636465, 0.7424242424242424310, 0.7462121212121212155, 0.7500000000000000000, 0.7537878787878787845, 0.7575757575757575690, 0.7613636363636363535, 0.7651515151515151381, 0.7689393939393939226, 0.7727272727272727071, 0.7765151515151514916, 0.7803030303030302761, 0.7840909090909090606, 0.7878787878787878451, 0.7916666666666666297, 0.7954545454545454142, 0.7992424242424241987, 0.8030303030303029832, 0.8068181818181817677, 0.8106060606060605522, 0.8143939393939394478, 0.8181818181818182323, 0.8219696969696970168, 0.8257575757575758013, 0.8295454545454545858, 0.8333333333333333703, 0.8371212121212121549, 0.8409090909090909394, 0.8446969696969697239, 0.8484848484848485084, 0.8522727272727272929, 0.8560606060606060774, 0.8598484848484848619, 0.8636363636363636465, 0.8674242424242424310, 0.8712121212121212155, 0.8750000000000000000, 0.8787878787878787845, 0.8825757575757575690, 0.8863636363636363535, 0.8901515151515151381, 0.8939393939393939226, 0.8977272727272727071, 0.9015151515151514916, 0.9053030303030302761, 0.9090909090909090606, 0.9128787878787878451, 0.9166666666666666297, 0.9204545454545454142, 0.9242424242424241987, 0.9280303030303029832, 0.9318181818181817677, 0.9356060606060605522, 0.9393939393939394478, 0.9431818181818182323, 0.9469696969696970168, 0.9507575757575758013, 0.9545454545454545858, 0.9583333333333333703, 0.9621212121212121549, 0.9659090909090909394 ),
 .UNSPECIFIED. ) 
 GEOMETRIC_REPRESENTATION_ITEM ( )  RATIONAL_B_SPLINE_SURFACE ( (
 ( 1.000000000000000000, 0.9659258262890683122, 1.000000000000000000, 0.9659258262890683122, 1.000000000000000000, 0.9659258262890683122, 1.000000000000000000, 0.9659258262890683122, 1.000000000000000000, 0.9659258262890683122, 1.000000000000000000, 0.9659258262890683122, 1.000000000000000000, 0.9659258262890683122, 1.000000000000000000, 0.9659258262890683122, 1.000000000000000000, 0.9659258262890683122, 1.000000000000000000, 0.9659258262890683122, 1.000000000000000000, 0.9659258262890683122, 1.000000000000000000, 0.9659258262890683122, 1.000000000000000000, 0.9659258262890683122, 1.000000000000000000, 0.9659258262890683122, 1.000000000000000000, 0.9659258262890683122, 1.000000000000000000, 0.9659258262890683122, 1.000000000000000000, 0.9659258262890683122, 1.000000000000000000, 0.9659258262890683122, 1.000000000000000000, 0.9659258262890683122, 1.000000000000000000, 0.9659258262890683122, 1.000000000000000000, 0.9659258262890683122, 1.000000000000000000, 0.9659258262890683122, 1.000000000000000000, 0.9659258262890683122, 1.000000000000000000, 0.9659258262890683122, 1.000000000000000000, 0.9659258262890683122, 1.000000000000000000, 0.9659258262890683122, 1.000000000000000000, 0.9659258262890683122, 1.000000000000000000, 0.9659258262890683122, 1.000000000000000000, 0.9659258262890683122, 1.000000000000000000, 0.9659258262890683122, 1.000000000000000000, 0.9659258262890683122, 1.000000000000000000, 0.9659258262890683122, 1.000000000000000000, 0.9659258262890683122, 1.000000000000000000, 0.9659258262890683122, 1.000000000000000000, 0.9659258262890683122, 1.000000000000000000, 0.9659258262890683122, 1.000000000000000000, 0.9659258262890683122, 1.000000000000000000, 0.9659258262890683122, 1.000000000000000000, 0.9659258262890683122, 1.000000000000000000, 0.9659258262890683122, 1.000000000000000000, 0.9659258262890683122, 1.000000000000000000, 0.9659258262890683122, 1.000000000000000000, 0.9659258262890683122, 1.000000000000000000, 0.9659258262890683122, 1.000000000000000000, 0.9659258262890683122, 1.000000000000000000, 0.9659258262890683122, 1.000000000000000000, 0.9659258262890683122, 1.000000000000000000, 0.9659258262890683122, 1.000000000000000000, 0.9659258262890683122, 1.000000000000000000, 0.9659258262890683122, 1.000000000000000000, 0.9659258262890683122, 1.000000000000000000, 0.9659258262890683122, 1.000000000000000000, 0.9659258262890683122, 1.000000000000000000, 0.9659258262890683122, 1.000000000000000000, 0.9659258262890683122, 1.000000000000000000, 0.9659258262890683122, 1.000000000000000000, 0.9659258262890683122, 1.000000000000000000, 0.9659258262890683122, 1.000000000000000000, 0.9659258262890683122, 1.000000000000000000, 0.9659258262890683122, 1.000000000000000000, 0.9659258262890683122, 1.000000000000000000, 0.9659258262890683122, 1.000000000000000000, 0.9659258262890683122, 1.000000000000000000, 0.9659258262890683122, 1.000000000000000000, 0.9659258262890683122, 1.000000000000000000, 0.9659258262890683122, 1.000000000000000000, 0.9659258262890683122, 1.000000000000000000, 0.9659258262890683122, 1.000000000000000000, 0.9659258262890683122, 1.000000000000000000, 0.9659258262890683122, 1.000000000000000000, 0.9659258262890683122, 1.000000000000000000, 0.9659258262890683122, 1.000000000000000000, 0.9659258262890683122, 1.000000000000000000, 0.9659258262890683122, 1.000000000000000000, 0.9659258262890683122, 1.000000000000000000, 0.9659258262890683122, 1.000000000000000000, 0.9659258262890683122, 1.000000000000000000, 0.9659258262890683122, 1.000000000000000000, 0.9659258262890683122, 1.000000000000000000, 0.9659258262890683122, 1.000000000000000000, 0.9659258262890683122, 1.000000000000000000, 0.9659258262890683122, 1.000000000000000000, 0.9659258262890683122, 1.000000000000000000, 0.9659258262890683122, 1.000000000000000000, 0.9659258262890683122, 1.000000000000000000, 0.9659258262890683122, 1.000000000000000000, 0.9659258262890683122, 1.000000000000000000, 0.9659258262890683122, 1.000000000000000000, 0.9659258262890683122, 1.000000000000000000, 0.9659258262890683122, 1.000000000000000000, 0.9659258262890683122, 1.000000000000000000, 0.9659258262890683122, 1.000000000000000000, 0.9659258262890683122, 1.000000000000000000, 0.9659258262890683122, 1.000000000000000000, 0.9659258262890683122, 1.000000000000000000, 0.9659258262890683122, 1.000000000000000000, 0.9659258262890683122, 1.000000000000000000, 0.9659258262890683122, 1.000000000000000000, 0.9659258262890683122, 1.000000000000000000, 0.9659258262890683122, 1.000000000000000000, 0.9659258262890683122, 1.000000000000000000, 0.9659258262890683122, 1.000000000000000000, 0.9659258262890683122, 1.000000000000000000, 0.9659258262890683122, 1.000000000000000000, 0.9659258262890683122, 1.000000000000000000, 0.9659258262890683122, 1.000000000000000000, 0.9659258262890683122, 1.000000000000000000, 0.9659258262890683122, 1.000000000000000000, 0.9659258262890683122, 1.000000000000000000, 0.9659258262890683122, 1.000000000000000000, 0.9659258262890683122, 1.000000000000000000, 0.9659258262890683122, 1.000000000000000000, 0.9659258262890683122, 1.000000000000000000, 0.9659258262890683122, 1.000000000000000000, 0.9659258262890683122, 1.000000000000000000, 0.9659258262890683122, 1.000000000000000000, 0.9659258262890683122, 1.000000000000000000, 0.9659258262890683122, 1.000000000000000000, 0.9659258262890683122, 1.000000000000000000, 0.9659258262890683122, 1.000000000000000000, 0.9659258262890683122, 1.000000000000000000, 0.9659258262890683122, 1.000000000000000000, 0.9659258262890683122, 1.000000000000000000, 0.9659258262890683122, 1.000000000000000000, 0.9659258262890683122, 1.000000000000000000, 0.9659258262890683122, 1.000000000000000000, 0.9659258262890683122, 1.000000000000000000, 0.9659258262890683122, 1.000000000000000000, 0.9659258262890683122, 1.000000000000000000, 0.9659258262890683122, 1.000000000000000000, 0.9659258262890683122, 1.000000000000000000, 0.9659258262890683122, 1.000000000000000000, 0.9659258262890683122, 1.000000000000000000, 0.9659258262890683122, 1.000000000000000000, 0.9659258262890683122, 1.000000000000000000, 0.9659258262890683122, 1.000000000000000000, 0.9659258262890683122, 1.000000000000000000, 0.9659258262890683122, 1.000000000000000000, 0.9659258262890683122, 1.000000000000000000, 0.9659258262890683122, 1.000000000000000000, 0.9659258262890683122, 1.000000000000000000, 0.9659258262890683122, 1.000000000000000000, 0.9659258262890683122, 1.000000000000000000, 0.9659258262890683122, 1.000000000000000000, 0.9659258262890683122, 1.000000000000000000, 0.9659258262890683122, 1.000000000000000000, 0.9659258262890683122, 1.000000000000000000, 0.9659258262890683122, 1.000000000000000000, 0.9659258262890683122, 1.000000000000000000, 0.9659258262890683122, 1.000000000000000000, 0.9659258262890683122, 1.000000000000000000, 0.9659258262890683122, 1.000000000000000000, 0.9659258262890683122, 1.000000000000000000, 0.9659258262890683122, 1.000000000000000000, 0.9659258262890683122, 1.000000000000000000, 0.9659258262890683122, 1.000000000000000000, 0.9659258262890683122, 1.000000000000000000, 0.9659258262890683122, 1.000000000000000000, 0.9659258262890683122, 1.000000000000000000, 0.9659258262890683122, 1.000000000000000000, 0.9659258262890683122, 1.000000000000000000, 0.9659258262890683122, 1.000000000000000000, 0.9659258262890683122, 1.000000000000000000, 0.9659258262890683122, 1.000000000000000000, 0.9659258262890683122, 1.000000000000000000, 0.9659258262890683122, 1.000000000000000000, 0.9659258262890683122, 1.000000000000000000, 0.9659258262890683122, 1.000000000000000000, 0.9659258262890683122, 1.000000000000000000, 0.9659258262890683122, 1.000000000000000000, 0.9659258262890683122, 1.000000000000000000, 0.9659258262890683122, 1.000000000000000000, 0.9659258262890683122, 1.000000000000000000, 0.9659258262890683122, 1.000000000000000000, 0.9659258262890683122, 1.000000000000000000, 0.9659258262890683122, 1.000000000000000000, 0.9659258262890683122, 1.000000000000000000, 0.9659258262890683122, 1.000000000000000000, 0.9659258262890683122, 1.000000000000000000, 0.9659258262890683122, 1.000000000000000000, 0.9659258262890683122, 1.000000000000000000, 0.9659258262890683122, 1.000000000000000000, 0.9659258262890683122, 1.000000000000000000, 0.9659258262890683122, 1.000000000000000000, 0.9659258262890683122, 1.000000000000000000, 0.9659258262890683122, 1.000000000000000000, 0.9659258262890683122, 1.000000000000000000, 0.9659258262890683122, 1.000000000000000000, 0.9659258262890683122, 1.000000000000000000, 0.9659258262890683122, 1.000000000000000000, 0.9659258262890683122, 1.000000000000000000, 0.9659258262890683122, 1.000000000000000000, 0.9659258262890683122, 1.000000000000000000, 0.9659258262890683122, 1.000000000000000000, 0.9659258262890683122, 1.000000000000000000, 0.9659258262890683122, 1.000000000000000000, 0.9659258262890683122, 1.000000000000000000, 0.9659258262890683122, 1.000000000000000000, 0.9659258262890683122, 1.000000000000000000, 0.9659258262890683122, 1.000000000000000000, 0.9659258262890683122, 1.000000000000000000, 0.9659258262890683122, 1.000000000000000000, 0.9659258262890683122, 1.000000000000000000, 0.9659258262890683122, 1.000000000000000000, 0.9659258262890683122, 1.000000000000000000, 0.9659258262890683122, 1.000000000000000000, 0.9659258262890683122, 1.000000000000000000, 0.9659258262890683122, 1.000000000000000000, 0.9659258262890683122, 1.000000000000000000, 0.9659258262890683122, 1.000000000000000000, 0.9659258262890683122, 1.000000000000000000, 0.9659258262890683122, 1.000000000000000000, 0.9659258262890683122, 1.000000000000000000, 0.9659258262890683122, 1.000000000000000000, 0.9659258262890683122, 1.000000000000000000, 0.9659258262890683122, 1.000000000000000000, 0.9659258262890683122, 1.000000000000000000, 0.9659258262890683122, 1.000000000000000000, 0.9659258262890683122, 1.000000000000000000, 0.9659258262890683122, 1.000000000000000000, 0.9659258262890683122, 1.000000000000000000, 0.9659258262890683122, 1.000000000000000000, 0.9659258262890683122, 1.000000000000000000, 0.9659258262890683122, 1.000000000000000000, 0.9659258262890683122, 1.000000000000000000, 0.9659258262890683122, 1.000000000000000000, 0.9659258262890683122, 1.000000000000000000, 0.9659258262890683122, 1.000000000000000000, 0.9659258262890683122, 1.000000000000000000, 0.9659258262890683122, 1.000000000000000000, 0.9659258262890683122, 1.000000000000000000, 0.9659258262890683122, 1.000000000000000000, 0.9659258262890683122, 1.000000000000000000, 0.9659258262890683122, 1.000000000000000000, 0.9659258262890683122, 1.000000000000000000, 0.9659258262890683122, 1.000000000000000000, 0.9659258262890683122, 1.000000000000000000, 0.9659258262890683122, 1.000000000000000000, 0.9659258262890683122, 1.000000000000000000, 0.9659258262890683122, 1.000000000000000000, 0.9659258262890683122, 1.000000000000000000, 0.9659258262890683122, 1.000000000000000000, 0.9659258262890683122, 1.000000000000000000, 0.9659258262890683122, 1.000000000000000000, 0.9659258262890683122, 1.000000000000000000, 0.9659258262890683122, 1.000000000000000000, 0.9659258262890683122, 1.000000000000000000, 0.9659258262890683122, 1.000000000000000000, 0.9659258262890683122, 1.000000000000000000, 0.9659258262890683122, 1.000000000000000000, 0.9659258262890683122, 1.000000000000000000, 0.9659258262890683122, 1.000000000000000000, 0.9659258262890683122, 1.000000000000000000, 0.9659258262890683122, 1.000000000000000000, 0.9659258262890683122, 1.000000000000000000),
 ( 1.000000000000000000, 0.9659258262890683122, 1.000000000000000000, 0.9659258262890683122, 1.000000000000000000, 0.9659258262890683122, 1.000000000000000000, 0.9659258262890683122, 1.000000000000000000, 0.9659258262890683122, 1.000000000000000000, 0.9659258262890683122, 1.000000000000000000, 0.9659258262890683122, 1.000000000000000000, 0.9659258262890683122, 1.000000000000000000, 0.9659258262890683122, 1.000000000000000000, 0.9659258262890683122, 1.000000000000000000, 0.9659258262890683122, 1.000000000000000000, 0.9659258262890683122, 1.000000000000000000, 0.9659258262890683122, 1.000000000000000000, 0.9659258262890683122, 1.000000000000000000, 0.9659258262890683122, 1.000000000000000000, 0.9659258262890683122, 1.000000000000000000, 0.9659258262890683122, 1.000000000000000000, 0.9659258262890683122, 1.000000000000000000, 0.9659258262890683122, 1.000000000000000000, 0.9659258262890683122, 1.000000000000000000, 0.9659258262890683122, 1.000000000000000000, 0.9659258262890683122, 1.000000000000000000, 0.9659258262890683122, 1.000000000000000000, 0.9659258262890683122, 1.000000000000000000, 0.9659258262890683122, 1.000000000000000000, 0.9659258262890683122, 1.000000000000000000, 0.9659258262890683122, 1.000000000000000000, 0.9659258262890683122, 1.000000000000000000, 0.9659258262890683122, 1.000000000000000000, 0.9659258262890683122, 1.000000000000000000, 0.9659258262890683122, 1.000000000000000000, 0.9659258262890683122, 1.000000000000000000, 0.9659258262890683122, 1.000000000000000000, 0.9659258262890683122, 1.000000000000000000, 0.9659258262890683122, 1.000000000000000000, 0.9659258262890683122, 1.000000000000000000, 0.9659258262890683122, 1.000000000000000000, 0.9659258262890683122, 1.000000000000000000, 0.9659258262890683122, 1.000000000000000000, 0.9659258262890683122, 1.000000000000000000, 0.9659258262890683122, 1.000000000000000000, 0.9659258262890683122, 1.000000000000000000, 0.9659258262890683122, 1.000000000000000000, 0.9659258262890683122, 1.000000000000000000, 0.9659258262890683122, 1.000000000000000000, 0.9659258262890683122, 1.000000000000000000, 0.9659258262890683122, 1.000000000000000000, 0.9659258262890683122, 1.000000000000000000, 0.9659258262890683122, 1.000000000000000000, 0.9659258262890683122, 1.000000000000000000, 0.9659258262890683122, 1.000000000000000000, 0.9659258262890683122, 1.000000000000000000, 0.9659258262890683122, 1.000000000000000000, 0.9659258262890683122, 1.000000000000000000, 0.9659258262890683122, 1.000000000000000000, 0.9659258262890683122, 1.000000000000000000, 0.9659258262890683122, 1.000000000000000000, 0.9659258262890683122, 1.000000000000000000, 0.9659258262890683122, 1.000000000000000000, 0.9659258262890683122, 1.000000000000000000, 0.9659258262890683122, 1.000000000000000000, 0.9659258262890683122, 1.000000000000000000, 0.9659258262890683122, 1.000000000000000000, 0.9659258262890683122, 1.000000000000000000, 0.9659258262890683122, 1.000000000000000000, 0.9659258262890683122, 1.000000000000000000, 0.9659258262890683122, 1.000000000000000000, 0.9659258262890683122, 1.000000000000000000, 0.9659258262890683122, 1.000000000000000000, 0.9659258262890683122, 1.000000000000000000, 0.9659258262890683122, 1.000000000000000000, 0.9659258262890683122, 1.000000000000000000, 0.9659258262890683122, 1.000000000000000000, 0.9659258262890683122, 1.000000000000000000, 0.9659258262890683122, 1.000000000000000000, 0.9659258262890683122, 1.000000000000000000, 0.9659258262890683122, 1.000000000000000000, 0.9659258262890683122, 1.000000000000000000, 0.9659258262890683122, 1.000000000000000000, 0.9659258262890683122, 1.000000000000000000, 0.9659258262890683122, 1.000000000000000000, 0.9659258262890683122, 1.000000000000000000, 0.9659258262890683122, 1.000000000000000000, 0.9659258262890683122, 1.000000000000000000, 0.9659258262890683122, 1.000000000000000000, 0.9659258262890683122, 1.000000000000000000, 0.9659258262890683122, 1.000000000000000000, 0.9659258262890683122, 1.000000000000000000, 0.9659258262890683122, 1.000000000000000000, 0.9659258262890683122, 1.000000000000000000, 0.9659258262890683122, 1.000000000000000000, 0.9659258262890683122, 1.000000000000000000, 0.9659258262890683122, 1.000000000000000000, 0.9659258262890683122, 1.000000000000000000, 0.9659258262890683122, 1.000000000000000000, 0.9659258262890683122, 1.000000000000000000, 0.9659258262890683122, 1.000000000000000000, 0.9659258262890683122, 1.000000000000000000, 0.9659258262890683122, 1.000000000000000000, 0.9659258262890683122, 1.000000000000000000, 0.9659258262890683122, 1.000000000000000000, 0.9659258262890683122, 1.000000000000000000, 0.9659258262890683122, 1.000000000000000000, 0.9659258262890683122, 1.000000000000000000, 0.9659258262890683122, 1.000000000000000000, 0.9659258262890683122, 1.000000000000000000, 0.9659258262890683122, 1.000000000000000000, 0.9659258262890683122, 1.000000000000000000, 0.9659258262890683122, 1.000000000000000000, 0.9659258262890683122, 1.000000000000000000, 0.9659258262890683122, 1.000000000000000000, 0.9659258262890683122, 1.000000000000000000, 0.9659258262890683122, 1.000000000000000000, 0.9659258262890683122, 1.000000000000000000, 0.9659258262890683122, 1.000000000000000000, 0.9659258262890683122, 1.000000000000000000, 0.9659258262890683122, 1.000000000000000000, 0.9659258262890683122, 1.000000000000000000, 0.9659258262890683122, 1.000000000000000000, 0.9659258262890683122, 1.000000000000000000, 0.9659258262890683122, 1.000000000000000000, 0.9659258262890683122, 1.000000000000000000, 0.9659258262890683122, 1.000000000000000000, 0.9659258262890683122, 1.000000000000000000, 0.9659258262890683122, 1.000000000000000000, 0.9659258262890683122, 1.000000000000000000, 0.9659258262890683122, 1.000000000000000000, 0.9659258262890683122, 1.000000000000000000, 0.9659258262890683122, 1.000000000000000000, 0.9659258262890683122, 1.000000000000000000, 0.9659258262890683122, 1.000000000000000000, 0.9659258262890683122, 1.000000000000000000, 0.9659258262890683122, 1.000000000000000000, 0.9659258262890683122, 1.000000000000000000, 0.9659258262890683122, 1.000000000000000000, 0.9659258262890683122, 1.000000000000000000, 0.9659258262890683122, 1.000000000000000000, 0.9659258262890683122, 1.000000000000000000, 0.9659258262890683122, 1.000000000000000000, 0.9659258262890683122, 1.000000000000000000, 0.9659258262890683122, 1.000000000000000000, 0.9659258262890683122, 1.000000000000000000, 0.9659258262890683122, 1.000000000000000000, 0.9659258262890683122, 1.000000000000000000, 0.9659258262890683122, 1.000000000000000000, 0.9659258262890683122, 1.000000000000000000, 0.9659258262890683122, 1.000000000000000000, 0.9659258262890683122, 1.000000000000000000, 0.9659258262890683122, 1.000000000000000000, 0.9659258262890683122, 1.000000000000000000, 0.9659258262890683122, 1.000000000000000000, 0.9659258262890683122, 1.000000000000000000, 0.9659258262890683122, 1.000000000000000000, 0.9659258262890683122, 1.000000000000000000, 0.9659258262890683122, 1.000000000000000000, 0.9659258262890683122, 1.000000000000000000, 0.9659258262890683122, 1.000000000000000000, 0.9659258262890683122, 1.000000000000000000, 0.9659258262890683122, 1.000000000000000000, 0.9659258262890683122, 1.000000000000000000, 0.9659258262890683122, 1.000000000000000000, 0.9659258262890683122, 1.000000000000000000, 0.9659258262890683122, 1.000000000000000000, 0.9659258262890683122, 1.000000000000000000, 0.9659258262890683122, 1.000000000000000000, 0.9659258262890683122, 1.000000000000000000, 0.9659258262890683122, 1.000000000000000000, 0.9659258262890683122, 1.000000000000000000, 0.9659258262890683122, 1.000000000000000000, 0.9659258262890683122, 1.000000000000000000, 0.9659258262890683122, 1.000000000000000000, 0.9659258262890683122, 1.000000000000000000, 0.9659258262890683122, 1.000000000000000000, 0.9659258262890683122, 1.000000000000000000, 0.9659258262890683122, 1.000000000000000000, 0.9659258262890683122, 1.000000000000000000, 0.9659258262890683122, 1.000000000000000000, 0.9659258262890683122, 1.000000000000000000, 0.9659258262890683122, 1.000000000000000000, 0.9659258262890683122, 1.000000000000000000, 0.9659258262890683122, 1.000000000000000000, 0.9659258262890683122, 1.000000000000000000, 0.9659258262890683122, 1.000000000000000000, 0.9659258262890683122, 1.000000000000000000, 0.9659258262890683122, 1.000000000000000000, 0.9659258262890683122, 1.000000000000000000, 0.9659258262890683122, 1.000000000000000000, 0.9659258262890683122, 1.000000000000000000, 0.9659258262890683122, 1.000000000000000000, 0.9659258262890683122, 1.000000000000000000, 0.9659258262890683122, 1.000000000000000000, 0.9659258262890683122, 1.000000000000000000, 0.9659258262890683122, 1.000000000000000000, 0.9659258262890683122, 1.000000000000000000, 0.9659258262890683122, 1.000000000000000000, 0.9659258262890683122, 1.000000000000000000, 0.9659258262890683122, 1.000000000000000000, 0.9659258262890683122, 1.000000000000000000, 0.9659258262890683122, 1.000000000000000000, 0.9659258262890683122, 1.000000000000000000, 0.9659258262890683122, 1.000000000000000000, 0.9659258262890683122, 1.000000000000000000, 0.9659258262890683122, 1.000000000000000000, 0.9659258262890683122, 1.000000000000000000, 0.9659258262890683122, 1.000000000000000000, 0.9659258262890683122, 1.000000000000000000, 0.9659258262890683122, 1.000000000000000000, 0.9659258262890683122, 1.000000000000000000, 0.9659258262890683122, 1.000000000000000000, 0.9659258262890683122, 1.000000000000000000, 0.9659258262890683122, 1.000000000000000000, 0.9659258262890683122, 1.000000000000000000, 0.9659258262890683122, 1.000000000000000000, 0.9659258262890683122, 1.000000000000000000, 0.9659258262890683122, 1.000000000000000000, 0.9659258262890683122, 1.000000000000000000, 0.9659258262890683122, 1.000000000000000000, 0.9659258262890683122, 1.000000000000000000, 0.9659258262890683122, 1.000000000000000000, 0.9659258262890683122, 1.000000000000000000, 0.9659258262890683122, 1.000000000000000000, 0.9659258262890683122, 1.000000000000000000, 0.9659258262890683122, 1.000000000000000000, 0.9659258262890683122, 1.000000000000000000, 0.9659258262890683122, 1.000000000000000000, 0.9659258262890683122, 1.000000000000000000, 0.9659258262890683122, 1.000000000000000000, 0.9659258262890683122, 1.000000000000000000, 0.9659258262890683122, 1.000000000000000000, 0.9659258262890683122, 1.000000000000000000, 0.9659258262890683122, 1.000000000000000000, 0.9659258262890683122, 1.000000000000000000, 0.9659258262890683122, 1.000000000000000000, 0.9659258262890683122, 1.000000000000000000, 0.9659258262890683122, 1.000000000000000000, 0.9659258262890683122, 1.000000000000000000, 0.9659258262890683122, 1.000000000000000000, 0.9659258262890683122, 1.000000000000000000, 0.9659258262890683122, 1.000000000000000000, 0.9659258262890683122, 1.000000000000000000, 0.9659258262890683122, 1.000000000000000000, 0.9659258262890683122, 1.000000000000000000, 0.9659258262890683122, 1.000000000000000000, 0.9659258262890683122, 1.000000000000000000, 0.9659258262890683122, 1.000000000000000000, 0.9659258262890683122, 1.000000000000000000, 0.9659258262890683122, 1.000000000000000000, 0.9659258262890683122, 1.000000000000000000, 0.9659258262890683122, 1.000000000000000000, 0.9659258262890683122, 1.000000000000000000, 0.9659258262890683122, 1.000000000000000000, 0.9659258262890683122, 1.000000000000000000, 0.9659258262890683122, 1.000000000000000000, 0.9659258262890683122, 1.000000000000000000, 0.9659258262890683122, 1.000000000000000000) ) ) 
 REPRESENTATION_ITEM ( '' )  SURFACE ( )  );
#44386 = CARTESIAN_POINT ( 'NONE',  ( -0.4527559055118102749, -0.4536011799217368745, -0.2665933059059886201 ) ) ;
#44387 = CARTESIAN_POINT ( 'NONE',  ( -1.003937007874014853, 0.1660481256975885056, 0.3530559997133364547 ) ) ;
#44388 = CARTESIAN_POINT ( 'NONE',  ( 0.9711286089238851948, -0.6046776061558809534, -0.2411417322834644161 ) ) ;
#44389 = ORIENTED_EDGE ( 'NONE', *, *, #22408, .T. ) ;
#44391 = CARTESIAN_POINT ( 'NONE',  ( -0.4724409448818898682, -8.678599364036362592E-17, -2.635826771653543066 ) ) ;
#44390 = PLANE ( 'NONE',  #46299 ) ;
#44392 = B_SPLINE_CURVE_WITH_KNOTS ( 'NONE', 3,
 ( #63925, #13424, #52947, #52533, #32770, #26032, #64343 ),
 .UNSPECIFIED., .F., .F.,
 ( 4, 3, 4 ),
 ( 7.459310946700270506E-17, 0.001246232571205254649, 0.002492492258783168303 ),
 .UNSPECIFIED. ) ;
#44393 = CARTESIAN_POINT ( 'NONE',  ( 1.240157480314961314, 0.1660481256975883668, -0.3530559997133364547 ) ) ;
#44394 = CARTESIAN_POINT ( 'NONE',  ( -1.181102362204723644, -0.1870078740157480879, -0.4822834645669291653 ) ) ;
#44395 = CARTESIAN_POINT ( 'NONE',  ( 0.3392501089628018329, -0.1958661417322834497, -0.4999806842181608868 ) ) ;
#44396 = CARTESIAN_POINT ( 'NONE',  ( -0.4593175853018366950, -0.004921259842519576551, 0.3153832671262227771 ) ) ;
#44397 = CARTESIAN_POINT ( 'NONE',  ( -9.594673741351313045E-17, 0.3917322834645670104, -0.8720472440944883052 ) ) ;
#44398 = CARTESIAN_POINT ( 'NONE',  ( -0.3018372703412066094, -0.3690944881889765550, -0.3153832671262227771 ) ) ;
#44399 = CARTESIAN_POINT ( 'NONE',  ( 0.5643044619422579178, -0.3690944881889765550, -0.3153832671262227771 ) ) ;
#44400 = CARTESIAN_POINT ( 'NONE',  ( 0.1902887139107617975, 0.2952755905511811885, 0.1292274648535926551 ) ) ;
#44401 = CARTESIAN_POINT ( 'NONE',  ( -0.7611548556430438595, -0.5023911411419708095, -0.1820866141732282451 ) ) ;
#44402 = CARTESIAN_POINT ( 'NONE',  ( -0.1049643490035307158, 0.3917322834645670104, 0.1541801592837776513 ) ) ;
#44403 = CARTESIAN_POINT ( 'NONE',  ( 1.017060367454068581, -0.05778040916215560624, -0.4822834645669293319 ) ) ;
#44404 = CARTESIAN_POINT ( 'NONE',  ( -1.233595800524933894, -0.6046776061558809534, -0.2411417322834644161 ) ) ;
#44405 = CARTESIAN_POINT ( 'NONE',  ( -0.4724409448818898682, -8.678599364036362592E-17, -1.061023622047243986 ) ) ;
#44406 = CARTESIAN_POINT ( 'NONE',  ( -0.5708661417322828946, 0.1660481256975883668, -0.3530559997133364547 ) ) ;
#44407 = CARTESIAN_POINT ( 'NONE',  ( -0.9580052493438311334, 0.05413385826771626580, -0.4176697321401330321 ) ) ;
#44408 = CARTESIAN_POINT ( 'NONE',  ( 1.272965879265092637, -0.3690944881889765550, -0.3153832671262227771 ) ) ;
#44409 = CARTESIAN_POINT ( 'NONE',  ( -0.09842519685039295696, 0.07958543189024071263, -0.2665933059059888421 ) ) ;
#44410 = CARTESIAN_POINT ( 'NONE',  ( -0.6692913385826764205, -0.6692913385826771977, 8.415575281601705876E-17 ) ) ;
#44411 = CARTESIAN_POINT ( 'NONE',  ( -1.299212598425196097, 0.2952755905511811885, 0.000000000000000000 ) ) ;
#44412 = DIRECTION ( 'NONE',  ( 1.000000000000000000, 0.000000000000000000, 0.000000000000000000 ) ) ;
#44413 = CARTESIAN_POINT ( 'NONE',  ( 1.489501312335958172, -0.2845877964562159024, 0.3641732283464567677 ) ) ;
#44414 = CARTESIAN_POINT ( 'NONE',  ( -0.4658792650918627265, -0.3162353388693409650, -0.4822834645669289433 ) ) ;
#44415 = CARTESIAN_POINT ( 'NONE',  ( -1.200787401574802349, 0.1660481256975883668, -0.3530559997133364547 ) ) ;
#44416 = ORIENTED_EDGE ( 'NONE', *, *, #75806, .F. ) ;
#44417 = CARTESIAN_POINT ( 'NONE',  ( 0.3996062992125985480, 2.446882876249141654E-17, -2.242125984251968518 ) ) ;
#44418 = CARTESIAN_POINT ( 'NONE',  ( -0.8661417322834640276, -0.1870078740157479769, 0.3641732283464567677 ) ) ;
#44419 = CARTESIAN_POINT ( 'NONE',  ( 1.220472440944882386, -0.6692913385826771977, 8.415575281601705876E-17 ) ) ;
#44420 = CARTESIAN_POINT ( 'NONE',  ( -1.056430446194224881, 0.1771653543307087075, -0.09757992244046823083 ) ) ;
#44421 = CARTESIAN_POINT ( 'NONE',  ( -0.1070741851644051862, -0.3996062992125986590, -1.251312335958005395 ) ) ;
#44422 = CARTESIAN_POINT ( 'NONE',  ( -0.8464566929133852113, -0.5400638737290845981, -0.3530559997133363437 ) ) ;
#44423 = CARTESIAN_POINT ( 'NONE',  ( 0.9383202099737538715, -0.05778040916215560624, -0.4822834645669293319 ) ) ;
#44424 = CARTESIAN_POINT ( 'NONE',  ( 0.9580052493438327987, -0.4281496062992127816, -0.4176697321401328100 ) ) ;
#44425 = EDGE_CURVE ( 'NONE', #25432, #30707, #80521, .T. ) ;
#44426 = CARTESIAN_POINT ( 'NONE',  ( 1.443569553805774897, 0.2306618581243848609, 0.2411417322834645549 ) ) ;
#44427 = CARTESIAN_POINT ( 'NONE',  ( -1.345144356955379816, -0.08942795157528024563, -0.3641732283464568787 ) ) ;
#44428 = CARTESIAN_POINT ( 'NONE',  ( 0.3996062992125985480, -0.1070741851644052972, -0.5032808398950130435 ) ) ;
#44429 = CARTESIAN_POINT ( 'NONE',  ( -0.3996062992125986035, -0.1070741851644056997, -1.148293963254592986 ) ) ;
#44430 = CARTESIAN_POINT ( 'NONE',  ( 0.2891555358219910499, 0.2891555358219910499, -0.1377952755905512694 ) ) ;
#44431 = CARTESIAN_POINT ( 'NONE',  ( 0.3726288332213487653, 0.1208384647389236927, -1.220472440944882164 ) ) ;
#44432 = CARTESIAN_POINT ( 'NONE',  ( 1.187664041994751285, -0.08942795157527998196, 0.3641732283464567121 ) ) ;
#44433 = CARTESIAN_POINT ( 'NONE',  ( 0.9383202099737536495, -0.2845877964562159024, 0.3641732283464567677 ) ) ;
#44434 = VECTOR ( 'NONE', #69354, 39.37007874015748143 ) ;
#44435 = CARTESIAN_POINT ( 'NONE',  ( 0.4133858267716541968, -0.5400638737290845981, -0.3530559997133363437 ) ) ;
#44436 = CARTESIAN_POINT ( 'NONE',  ( 0.3149606299212482918, 2.165354330708661568, 1.076935383196061080 ) ) ;
#44437 = CARTESIAN_POINT ( 'NONE',  ( -0.2891555358219911054, 0.2891555358219909388, -1.513779527559055094 ) ) ;
#44438 = CARTESIAN_POINT ( 'NONE',  ( 0.7152230971128616943, -0.08942795157527998196, 0.3641732283464567121 ) ) ;
#44439 = CARTESIAN_POINT ( 'NONE',  ( -0.4330708661417315697, -0.6692913385826771977, 8.415575281601705876E-17 ) ) ;
#44440 = CARTESIAN_POINT ( 'NONE',  ( -1.115485564304461219, 0.05413385826771626580, -0.4176697321401330321 ) ) ;
#44441 = CARTESIAN_POINT ( 'NONE',  ( 0.9448818897637802916, -0.1870078740157480879, -0.4822834645669291653 ) ) ;
#44442 = CARTESIAN_POINT ( 'NONE',  ( -0.4091458600556405756, 0.2362204724409446288, -1.601049868766404094 ) ) ;
#44443 = CARTESIAN_POINT ( 'NONE',  ( -0.2925321140481930704, -0.2925321140481933480, -2.736220472440943574 ) ) ;
#44444 = ADVANCED_FACE ( 'NONE', ( #17932 ), #55439, .F. ) ;
#44445 = VERTEX_POINT ( 'NONE', #70489 ) ;
#44446 = ORIENTED_EDGE ( 'NONE', *, *, #60654, .F. ) ;
#44447 = CARTESIAN_POINT ( 'NONE',  ( -1.128608923884513837, -0.6046776061558807314, 0.2411417322834647770 ) ) ;
#44448 = CARTESIAN_POINT ( 'NONE',  ( -0.4133858267716528645, -0.5400638737290844871, 0.3530559997133364547 ) ) ;
#44450 = CARTESIAN_POINT ( 'NONE',  ( -0.8989501312335946848, -0.6692913385826771977, 0.1292274648535927661 ) ) ;
#44449 = CARTESIAN_POINT ( 'NONE',  ( -0.8005249343832011588, -0.004921259842519870586, -0.3153832671262229437 ) ) ;
#44451 = CARTESIAN_POINT ( 'NONE',  ( 4.797336870675655290E-17, -0.3917322834645669549, -2.048537114664355396 ) ) ;
#44452 = CARTESIAN_POINT ( 'NONE',  ( 0.4527559055118117182, 0.1660481256975883668, -0.3530559997133364547 ) ) ;
#44453 = EDGE_CURVE ( 'NONE', #40881, #19658, #41992, .T. ) ;
#44454 = CARTESIAN_POINT ( 'NONE',  ( -0.2427821522309703550, -0.3162353388693405765, 0.4822834645669290543 ) ) ;
#44455 = CARTESIAN_POINT ( 'NONE',  ( 1.384514435695538337, -0.6692913385826771977, 0.1292274648535927661 ) ) ;
#44456 = VECTOR ( 'NONE', #65290, 39.37007874015748143 ) ;
#44457 = CARTESIAN_POINT ( 'NONE',  ( -0.7545931758530177724, 0.2952755905511811885, 0.1292274648535926551 ) ) ;
#44458 = CARTESIAN_POINT ( 'NONE',  ( 0.6430446194225728496, 0.05413385826771666132, 0.4176697321401328100 ) ) ;
#44459 = CARTESIAN_POINT ( 'NONE',  ( -9.594673741351313045E-17, 0.3917322834645670104, -1.409448818897637734 ) ) ;
#44460 = CARTESIAN_POINT ( 'NONE',  ( -0.8267716535433065062, 0.1771653543307087630, 0.000000000000000000 ) ) ;
#44461 = ORIENTED_EDGE ( 'NONE', *, *, #21276, .F. ) ;
#44462 = CARTESIAN_POINT ( 'NONE',  ( 0.2891555358219910499, 0.2891555358219910499, -1.870078740157480324 ) ) ;
#44463 = EDGE_LOOP ( 'NONE', ( #13326, #22333 ) ) ;
#44464 = CARTESIAN_POINT ( 'NONE',  ( -1.430446194225721390, -0.3690944881889763329, 0.3153832671262228327 ) ) ;
#44465 = CARTESIAN_POINT ( 'NONE',  ( -1.194225721784776262, -0.4281496062992124485, 0.4176697321401328655 ) ) ;
#44466 = CARTESIAN_POINT ( 'NONE',  ( -0.8005249343832011588, 0.05413385826771626580, -0.4176697321401330321 ) ) ;
#44467 = CARTESIAN_POINT ( 'NONE',  ( -9.787531504996567848E-17, 0.3996062992125986035, -0.3149606299212598381 ) ) ;
#44468 = CARTESIAN_POINT ( 'NONE',  ( -1.023622047244094002, -0.1870078740157480879, -0.4822834645669291653 ) ) ;
#44469 = CARTESIAN_POINT ( 'NONE',  ( -1.450131233595799651, -0.6692913385826771977, 0.1292274648535927661 ) ) ;
#44470 = CARTESIAN_POINT ( 'NONE',  ( -1.948818897637795367, 0.000000000000000000, 5.879133660591329580 ) ) ;
#44471 = DIRECTION ( 'NONE',  ( 0.000000000000000000, 0.000000000000000000, -1.000000000000000000 ) ) ;
#44472 = CARTESIAN_POINT ( 'NONE',  ( 0.3346456692913393205, -0.4536011799217368745, -0.2665933059059886201 ) ) ;
#44473 = DIRECTION ( 'NONE',  ( -1.000000000000000000, -1.734723475976808080E-16, -3.491481338843132961E-15 ) ) ;
#44474 = CARTESIAN_POINT ( 'NONE',  ( -0.2867679344610365999, 0.2867679344610364889, 0.05314960629921249707 ) ) ;
#44475 = CARTESIAN_POINT ( 'NONE',  ( -0.5511811023622041894, -0.1870078740157480601, -0.3641732283464567677 ) ) ;
#44476 = CARTESIAN_POINT ( 'NONE',  ( -0.2230971128608915943, 0.05413385826771666132, 0.4176697321401328100 ) ) ;
#44477 = CARTESIAN_POINT ( 'NONE',  ( 1.397637795275591177, -0.5400638737290844871, 0.3530559997133364547 ) ) ;
#44478 = CARTESIAN_POINT ( 'NONE',  ( -0.4790026246719152336, -0.05778040916215560624, -0.4822834645669293319 ) ) ;
#44479 = ORIENTED_EDGE ( 'NONE', *, *, #2516, .T. ) ;
#44480 = ORIENTED_EDGE ( 'NONE', *, *, #68203, .F. ) ;
#44481 = CARTESIAN_POINT ( 'NONE',  ( 0.3460692066303959202, -0.1998031496062991630, -1.599081364829396223 ) ) ;
#44482 = CARTESIAN_POINT ( 'NONE',  ( -0.3674540682414689785, 0.2306618581243848609, 0.2411417322834645549 ) ) ;
#44483 = CARTESIAN_POINT ( 'NONE',  ( 1.102362204724410155, -0.1870078740157479769, 0.4822834645669291653 ) ) ;
#44484 = CARTESIAN_POINT ( 'NONE',  ( -1.062992125984250968, 0.1771653543307087630, 0.000000000000000000 ) ) ;
#44485 = CARTESIAN_POINT ( 'NONE',  ( -1.515748031496062076, 0.1660481256975883668, -0.3530559997133364547 ) ) ;
#44486 = CARTESIAN_POINT ( 'NONE',  ( 0.2362204724409449064, 0.4091458600556404646, -0.7742782152230971437 ) ) ;
#44487 = EDGE_CURVE ( 'NONE', #7970, #56774, #76940, .T. ) ;
#44488 = LINE ( 'NONE', #17217, #68074 ) ;
#44489 = CARTESIAN_POINT ( 'NONE',  ( 0.2867679344610365999, 0.2867679344610365999, 0.02755905511811028441 ) ) ;
#44490 = CARTESIAN_POINT ( 'NONE',  ( 1.515748031496063408, 0.1660481256975885056, 0.3530559997133364547 ) ) ;
#44491 = DIRECTION ( 'NONE',  ( 0.7071067811865462405, -0.000000000000000000, 0.7071067811865486830 ) ) ;
#44492 = CARTESIAN_POINT ( 'NONE',  ( 0.07874015748031558404, -0.1870078740157479769, 0.4822834645669291653 ) ) ;
#44493 = CARTESIAN_POINT ( 'NONE',  ( -0.9842519685039360366, 0.1771653543307087630, 0.000000000000000000 ) ) ;
#44494 = CARTESIAN_POINT ( 'NONE',  ( -0.3805774278215216522, -0.4281496062992127816, -0.4176697321401328100 ) ) ;
#44495 = CARTESIAN_POINT ( 'NONE',  ( 0.1265901696524989462, 0.4724409448818897572, -2.747375328083988766 ) ) ;
#44496 = CARTESIAN_POINT ( 'NONE',  ( -0.7349081364829390672, 0.2306618581243847221, -0.2411417322834647770 ) ) ;
#44497 = CARTESIAN_POINT ( 'NONE',  ( -1.082677165354329896, 0.1660481256975885056, 0.3530559997133364547 ) ) ;
#44498 = EDGE_CURVE ( 'NONE', #58545, #16126, #56519, .T. ) ;
#44499 = CARTESIAN_POINT ( 'NONE',  ( 0.3420746716998660508, -0.1974969037888704149, -2.071522309711286258 ) ) ;
#44500 = CARTESIAN_POINT ( 'NONE',  ( 0.8727034120734912248, -0.2845877964562161244, -0.3641732283464567121 ) ) ;
#44501 = CARTESIAN_POINT ( 'NONE',  ( -0.3477690288713905509, -0.5511811023622046335, 0.09757992244046803654 ) ) ;
#44502 = CARTESIAN_POINT ( 'NONE',  ( 0.8923884514435703741, 0.1283753931104748280, 0.1820866141732283561 ) ) ;
#44503 = CARTESIAN_POINT ( 'NONE',  ( -1.633858267716534529, -0.5400638737290845981, -0.3530559997133363437 ) ) ;
#44504 = VECTOR ( 'NONE', #70226, 39.37007874015748854 ) ;
#44505 = CARTESIAN_POINT ( 'NONE',  ( 1.312335958005249825, 0.2306618581243847221, -0.2411417322834647770 ) ) ;
#44506 = CARTESIAN_POINT ( 'NONE',  ( 0.6561679790026253567, -0.5023911411419708095, -0.1820866141732282451 ) ) ;
#44507 = CARTESIAN_POINT ( 'NONE',  ( -0.6561679790026240244, 0.2306618581243847221, -0.2411417322834647770 ) ) ;
#44508 = CARTESIAN_POINT ( 'NONE',  ( 1.181102362204724976, -0.1870078740157480879, -0.4822834645669291653 ) ) ;
#44509 = EDGE_CURVE ( 'NONE', #62598, #4531, #30229, .T. ) ;
#44510 = CARTESIAN_POINT ( 'NONE',  ( -0.2362204724409451284, 0.4091458600556402425, 0.2250656167979002698 ) ) ;
#44511 = CARTESIAN_POINT ( 'NONE',  ( -0.1968503937007867743, 0.1771653543307087630, 0.000000000000000000 ) ) ;
#44512 = DIRECTION ( 'NONE',  ( -1.000000000000000000, -0.000000000000000000, -0.000000000000000000 ) ) ;
#44513 = CARTESIAN_POINT ( 'NONE',  ( 0.4593175853018380828, 0.05413385826771626580, -0.4176697321401330321 ) ) ;
#44514 = CARTESIAN_POINT ( 'NONE',  ( 0.6415071261929219393, 0.02791078216816263863, 0.4328096321851903627 ) ) ;
#44515 = CARTESIAN_POINT ( 'NONE',  ( 0.9842519685039375910, 0.1771653543307087630, 0.000000000000000000 ) ) ;
#44516 = CARTESIAN_POINT ( 'NONE',  ( 0.08530183727034192087, -0.2845877964562161244, -0.3641732283464567121 ) ) ;
#44517 = CARTESIAN_POINT ( 'NONE',  ( -1.528871391076114250, 0.2952755905511810774, -0.1292274648535930714 ) ) ;
#44518 = CARTESIAN_POINT ( 'NONE',  ( -0.5774278215223089816, -0.5023911411419708095, 0.1820866141732285504 ) ) ;
#44519 = DIRECTION ( 'NONE',  ( 0.8479387356305982948, 2.625811289636359704E-16, -0.5300942374872437135 ) ) ;
#44520 = CARTESIAN_POINT ( 'NONE',  ( -1.010498687664041384, -0.4281496062992127816, -0.4176697321401328100 ) ) ;
#44521 = CARTESIAN_POINT ( 'NONE',  ( -0.6299212598425188991, -0.1870078740157480879, -0.4822834645669291653 ) ) ;
#44522 = CARTESIAN_POINT ( 'NONE',  ( 0.3996062992125986035, -0.1070741851644052972, -1.133202099737532720 ) ) ;
#44523 = CARTESIAN_POINT ( 'NONE',  ( 0.3917322834645670104, -0.1049643490035303411, -2.243438320209974357 ) ) ;
#44524 = CARTESIAN_POINT ( 'NONE',  ( 0.5643044619422579178, -0.3690944881889765550, -0.3153832671262227771 ) ) ;
#44525 = CARTESIAN_POINT ( 'NONE',  ( -0.4265091863517051496, -0.6692913385826771977, 0.1292274648535927661 ) ) ;
#44526 = CARTESIAN_POINT ( 'NONE',  ( -0.7611548556430438595, -0.6046776061558809534, -0.2411417322834644161 ) ) ;
#44527 = CARTESIAN_POINT ( 'NONE',  ( -0.8858267716535425107, -0.4536011799217367080, 0.2665933059059888421 ) ) ;
#44528 = CYLINDRICAL_SURFACE ( 'NONE', #27964, 3.543307086614173151 ) ;
#44529 = CARTESIAN_POINT ( 'NONE',  ( -0.05905511811023545637, 0.1660481256975885056, 0.3530559997133364547 ) ) ;
#44530 = CARTESIAN_POINT ( 'NONE',  ( -1.587926509186350810, -0.3690944881889763329, 0.3153832671262228327 ) ) ;
#44531 = CARTESIAN_POINT ( 'NONE',  ( 1.213910761154856299, -0.6692913385826773087, -0.1292274648535924053 ) ) ;
#44532 = DIRECTION ( 'NONE',  ( 0.000000000000000000, 0.000000000000000000, -1.000000000000000000 ) ) ;
#44533 = CARTESIAN_POINT ( 'NONE',  ( 0.1958661417322836718, -0.3392501089628017219, -2.293326402396012487 ) ) ;
#44534 = VERTEX_POINT ( 'NONE', #43981 ) ;
#44535 = CARTESIAN_POINT ( 'NONE',  ( -1.089942661822471459, 0.000000000000000000, 0.3464511005275205946 ) ) ;
#44536 = CARTESIAN_POINT ( 'NONE',  ( -1.469816272965878357, -0.6046776061558809534, -0.2411417322834644161 ) ) ;
#44537 = CARTESIAN_POINT ( 'NONE',  ( -0.9842519685039365918, -0.6692913385826771977, 8.415575281601705876E-17 ) ) ;
#44538 = CARTESIAN_POINT ( 'NONE',  ( -1.410761154855641575, -0.3162353388693409650, -0.4822834645669289433 ) ) ;
#44539 = CARTESIAN_POINT ( 'NONE',  ( 0.3392501089628018884, -0.1958661417322834220, -1.921916010498687877 ) ) ;
#44540 = LINE ( 'NONE', #10934, #57867 ) ;
#44541 = CARTESIAN_POINT ( 'NONE',  ( 1.128608923884515169, -0.6046776061558809534, -0.2411417322834644161 ) ) ;
#44542 = CARTESIAN_POINT ( 'NONE',  ( -0.02624671916010428221, 0.2306618581243847221, -0.2411417322834647770 ) ) ;
#44543 = CARTESIAN_POINT ( 'NONE',  ( -0.3268936723430463931, 1.297973861003007810E-15, -0.3627985898453513491 ) ) ;
#44544 = CARTESIAN_POINT ( 'NONE',  ( -0.6970755509724322341, 0.02791078216816064370, 0.4328096321851915285 ) ) ;
#44545 = CARTESIAN_POINT ( 'NONE',  ( 1.207349081364829990, -0.5023911411419708095, -0.1820866141732282451 ) ) ;
#44546 = ADVANCED_FACE ( 'NONE', ( #69678 ), #31357, .F. ) ;
#44547 = CARTESIAN_POINT ( 'NONE',  ( -0.3996062992125987146, 0.1070741851644051862, -1.135170603674540590 ) ) ;
#44548 = VERTEX_POINT ( 'NONE', #43157 ) ;
#44549 = CARTESIAN_POINT ( 'NONE',  ( 0.2867679344610366554, 0.2867679344610366554, 0.02294656348325270490 ) ) ;
#44550 = VERTEX_POINT ( 'NONE', #5688 ) ;
#44551 = CARTESIAN_POINT ( 'NONE',  ( 0.4133858267716541968, -0.5400638737290845981, -0.3530559997133363437 ) ) ;
#44552 = CARTESIAN_POINT ( 'NONE',  ( -0.6955380577427815458, -0.4281496062992127816, -0.4176697321401328100 ) ) ;
#44553 = CARTESIAN_POINT ( 'NONE',  ( -1.358267716535432434, -0.5400638737290844871, 0.3530559997133364547 ) ) ;
#44554 = CARTESIAN_POINT ( 'NONE',  ( 0.5839895013123367340, 0.2952755905511811885, 0.1292274648535926551 ) ) ;
#44555 = CARTESIAN_POINT ( 'NONE',  ( -1.515748031496062076, -0.4536011799217367080, 0.2665933059059888421 ) ) ;
#44556 = CARTESIAN_POINT ( 'NONE',  ( 1.496062992125984703, -0.1870078740157480879, -0.4822834645669291653 ) ) ;
#44557 = CARTESIAN_POINT ( 'NONE',  ( -0.02624671916010428221, 0.2306618581243847221, -0.2411417322834647770 ) ) ;
#44558 = CIRCLE ( 'NONE', #67258, 1.122047244094488194 ) ;
#44559 = CARTESIAN_POINT ( 'NONE',  ( -1.338582677165353729, -0.1870078740157479769, 0.4822834645669291653 ) ) ;
#44560 = CARTESIAN_POINT ( 'NONE',  ( 1.148293963254593653, 0.2952755905511810774, -0.1292274648535930714 ) ) ;
#44561 = CARTESIAN_POINT ( 'NONE',  ( 1.574803149606299746, -0.1870078740157480879, -0.4822834645669291653 ) ) ;
#44562 = CARTESIAN_POINT ( 'NONE',  ( 0.3392501089628018329, 0.1958661417322835607, -0.1233595800524933811 ) ) ;
#44563 = CARTESIAN_POINT ( 'NONE',  ( 0.3280839895013130669, -0.3690944881889765550, -0.3153832671262227771 ) ) ;
#44564 = ORIENTED_EDGE ( 'NONE', *, *, #31972, .F. ) ;
#44565 = CARTESIAN_POINT ( 'NONE',  ( 0.2891555358219910499, -0.2891555358219909944, -0.09842519685039378963 ) ) ;
#44566 = VERTEX_POINT ( 'NONE', #57023 ) ;
#44567 = CARTESIAN_POINT ( 'NONE',  ( 0.07874015748031558404, -0.1870078740157480601, -0.3641732283464567677 ) ) ;
#44568 = CARTESIAN_POINT ( 'NONE',  ( 2.666386537446502558, 1.301102360844750727, -0.4123394245947693548 ) ) ;
#44569 = CARTESIAN_POINT ( 'NONE',  ( 0.2099737532808405305, 0.2306618581243847221, -0.2411417322834647770 ) ) ;
#44570 = CARTESIAN_POINT ( 'NONE',  ( -0.006561679790025524116, -0.3162353388693405765, 0.4822834645669290543 ) ) ;
#44571 = CARTESIAN_POINT ( 'NONE',  ( -0.4461942257217840213, 0.2306618581243848609, 0.2411417322834645549 ) ) ;
#44572 = CARTESIAN_POINT ( 'NONE',  ( -0.1049643490035302301, -0.3917322834645671770, -1.486239788222784020 ) ) ;
#44573 = CARTESIAN_POINT ( 'NONE',  ( -1.272965879265091305, 0.05413385826771626580, -0.4176697321401330321 ) ) ;
#44574 = CARTESIAN_POINT ( 'NONE',  ( -0.3917322834645670104, -7.196005306013484475E-17, -2.801181102362204633 ) ) ;
#44575 = CARTESIAN_POINT ( 'NONE',  ( 1.443569553805774897, 0.1283753931104748280, 0.1820866141732283561 ) ) ;
#44576 = CARTESIAN_POINT ( 'NONE',  ( 0.9383202099737538715, -0.05778040916215560624, -0.4822834645669293319 ) ) ;
#44577 = CARTESIAN_POINT ( 'NONE',  ( 0.8005249343832028242, -0.4281496062992127816, -0.4176697321401328100 ) ) ;
#44578 = CARTESIAN_POINT ( 'NONE',  ( -9.787531504996567848E-17, 0.3996062992125986035, -0.9448818897637796255 ) ) ;
#44579 = CARTESIAN_POINT ( 'NONE',  ( -1.187664041994750175, -0.05778040916215560624, -0.4822834645669293319 ) ) ;
#44580 = CARTESIAN_POINT ( 'NONE',  ( 0.1070741851644053388, 0.3996062992125986035, -0.2276902887139107545 ) ) ;
#44581 = CARTESIAN_POINT ( 'NONE',  ( 0.3460692066303958092, 0.1998031496062993018, -0.2080052493438320771 ) ) ;
#44582 = CARTESIAN_POINT ( 'NONE',  ( -0.09842519685039295696, 0.1660481256975883668, -0.3530559997133364547 ) ) ;
#44583 = CARTESIAN_POINT ( 'NONE',  ( -0.3996062992125987146, 0.1070741851644051862, -2.552493438320210029 ) ) ;
#44584 = CARTESIAN_POINT ( 'NONE',  ( 0.3917322834645669549, 0.1049643490035304660, -1.626640419947506411 ) ) ;
#44585 = CARTESIAN_POINT ( 'NONE',  ( 1.253280839895013710, -0.3162353388693405765, 0.4822834645669290543 ) ) ;
#44586 = CARTESIAN_POINT ( 'NONE',  ( 1.476377952755906442, -0.5400638737290844871, 0.3530559997133364547 ) ) ;
#44587 = CARTESIAN_POINT ( 'NONE',  ( 0.03280839895013198948, -0.5511811023622048555, -0.09757992244046775898 ) ) ;
#44588 = CARTESIAN_POINT ( 'NONE',  ( 0.8595800524934390507, -0.05778040916215560624, -0.4822834645669293319 ) ) ;
#44589 = CARTESIAN_POINT ( 'NONE',  ( -0.4724409448818899238, 0.1265901696524986686, -1.526902887139107490 ) ) ;
#44590 = CARTESIAN_POINT ( 'NONE',  ( 0.4133858267716541968, 0.07958543189024085140, 0.2665933059059887866 ) ) ;
#44591 = CARTESIAN_POINT ( 'NONE',  ( 0.3674540682414705883, 0.2306618581243847221, -0.2411417322834647770 ) ) ;
#44592 = CARTESIAN_POINT ( 'NONE',  ( -0.3949938075777411073, 0.1058382717557497660, -1.054461942257217899 ) ) ;
#44593 = CARTESIAN_POINT ( 'NONE',  ( -1.253280839895012377, -0.05778040916215522460, 0.4822834645669289988 ) ) ;
#44594 = CARTESIAN_POINT ( 'NONE',  ( 1.082677165354331228, -0.4536011799217367080, 0.2665933059059888421 ) ) ;
#44595 = CARTESIAN_POINT ( 'NONE',  ( 0.3674540682414705883, 0.1539470093639521697, -0.1968503937007875793 ) ) ;
#44596 = CARTESIAN_POINT ( 'NONE',  ( -0.4068241469816267775, 0.05413385826771626580, -0.4176697321401330321 ) ) ;
#44597 = CARTESIAN_POINT ( 'NONE',  ( -0.3740157480314953431, 0.07958543189024085140, 0.2665933059059887866 ) ) ;
#44598 = CARTESIAN_POINT ( 'NONE',  ( 0.4359958488159859091, 1.724409448818897905, -3.912791665790197992 ) ) ;
#44599 = CARTESIAN_POINT ( 'NONE',  ( -0.3937007874015740483, -0.1870078740157480879, -0.4822834645669291653 ) ) ;
#44600 = CARTESIAN_POINT ( 'NONE',  ( 0.1574803149606306130, -0.1870078740157479769, 0.3641732283464567677 ) ) ;
#44601 = CARTESIAN_POINT ( 'NONE',  ( 0.3996062992125985480, 2.446882876249141654E-17, -2.084645669291338876 ) ) ;
#44602 = CARTESIAN_POINT ( 'NONE',  ( 0.1049868766404206816, 0.2306618581243848609, 0.2411417322834645549 ) ) ;
#44603 = CARTESIAN_POINT ( 'NONE',  ( -0.3917322834645670659, 0.1049643490035301607, -1.687644726212911506 ) ) ;
#44604 = CARTESIAN_POINT ( 'NONE',  ( 0.9973753280839902091, -0.5023911411419708095, 0.1820866141732285504 ) ) ;
#44605 = LINE ( 'NONE', #43783, #20444 ) ;
#44606 = CARTESIAN_POINT ( 'NONE',  ( -0.7480314960629914633, 0.1771653543307087630, 0.000000000000000000 ) ) ;
#44607 = CARTESIAN_POINT ( 'NONE',  ( -0.6496062992125976043, -0.4536011799217367080, 0.2665933059059888421 ) ) ;
#44608 = CARTESIAN_POINT ( 'NONE',  ( -0.1115485564304453947, -0.6692913385826771977, 0.1292274648535927661 ) ) ;
#44609 = CARTESIAN_POINT ( 'NONE',  ( -0.07874015748031421014, -0.1870078740157480879, -0.4822834645669291653 ) ) ;
#44610 = CARTESIAN_POINT ( 'NONE',  ( 0.7545931758530189937, 0.1771653543307087075, -0.09757992244046823083 ) ) ;
#44611 = CARTESIAN_POINT ( 'NONE',  ( 0.1239563933494705478, 1.079204589967275085, -1.115281408855063550 ) ) ;
#44612 = CARTESIAN_POINT ( 'NONE',  ( 1.463254593175853824, 0.1771653543307087075, -0.09757992244046823083 ) ) ;
#44613 = AXIS2_PLACEMENT_3D ( 'NONE', #7703, #27041, #21562 ) ;
#44614 = CARTESIAN_POINT ( 'NONE',  ( 0.7414698162729663755, 0.2952755905511811885, 0.1292274648535926551 ) ) ;
#44615 = CARTESIAN_POINT ( 'NONE',  ( 0.4477123500622125496, 1.379796003448449326, -2.114018334261799303 ) ) ;
#44616 = CARTESIAN_POINT ( 'NONE',  ( -0.4724409448818890911, -0.1870078740157479769, 0.4822834645669291653 ) ) ;
#44617 = CARTESIAN_POINT ( 'NONE',  ( 4.797336870675656522E-17, -0.3917322834645670104, -1.108267716535433101 ) ) ;
#44618 = CARTESIAN_POINT ( 'NONE',  ( -1.463254593175852492, -0.6692913385826773087, -0.1292274648535924053 ) ) ;
#44619 = CARTESIAN_POINT ( 'NONE',  ( 0.9448818897637802916, -0.1870078740157480879, -0.4822834645669291653 ) ) ;
#44620 = CARTESIAN_POINT ( 'NONE',  ( 0.3937007874015754361, -0.1870078740157479769, 0.4822834645669291653 ) ) ;
#44621 = DIRECTION ( 'NONE',  ( -0.000000000000000000, -1.000000000000000000, -0.000000000000000000 ) ) ;
#44622 = CARTESIAN_POINT ( 'NONE',  ( 0.2559055118110243332, 0.07958543189024085140, 0.2665933059059887866 ) ) ;
#44623 = CARTESIAN_POINT ( 'NONE',  ( 1.207349081364829990, 0.2306618581243848609, 0.2411417322834645549 ) ) ;
#44624 = CARTESIAN_POINT ( 'NONE',  ( -0.4986876640419942164, -0.5023911411419708095, 0.1820866141732285504 ) ) ;
#44625 = CARTESIAN_POINT ( 'NONE',  ( -0.7480314960629914633, -0.6692913385826771977, 8.415575281601705876E-17 ) ) ;
#44626 = CARTESIAN_POINT ( 'NONE',  ( 0.8202099737532814183, 0.2952755905511811885, 0.1292274648535926551 ) ) ;
#44627 = CARTESIAN_POINT ( 'NONE',  ( 0.2952755905511816326, -0.5400638737290844871, 0.3530559997133364547 ) ) ;
#44628 = CARTESIAN_POINT ( 'NONE',  ( -0.8136482939632537770, 0.2306618581243847221, -0.2411417322834647770 ) ) ;
#44629 = CARTESIAN_POINT ( 'NONE',  ( -0.6364829396325453192, -0.2845877964562159024, 0.3641732283464567677 ) ) ;
#44630 = CARTESIAN_POINT ( 'NONE',  ( 0.5774278215223103139, -0.6046776061558809534, -0.2411417322834644161 ) ) ;
#44631 = CARTESIAN_POINT ( 'NONE',  ( -1.279527559055116948, -0.5400638737290844871, 0.3530559997133364547 ) ) ;
#44632 = CARTESIAN_POINT ( 'NONE',  ( -0.4855643044619415427, 0.05413385826771626580, -0.4176697321401330321 ) ) ;
#44634 = CARTESIAN_POINT ( 'NONE',  ( 1.345144356955381593, -0.3162353388693409650, -0.4822834645669289433 ) ) ;
#44633 = CARTESIAN_POINT ( 'NONE',  ( 0.3503937007874015630, 0.3733313776025731778, -0.01968503937007957602 ) ) ;
#44635 = CARTESIAN_POINT ( 'NONE',  ( 1.141732283464567788, -0.6692913385826771977, 8.415575281601705876E-17 ) ) ;
#44636 = CARTESIAN_POINT ( 'NONE',  ( 0.1049643490035304799, -0.3917322834645669549, -2.124671916010498762 ) ) ;
#44637 = B_SPLINE_CURVE_WITH_KNOTS ( 'NONE', 3,
 ( #969, #45544, #39241, #39667, #26623, #32511, #64088, #33362, #52694, #20733, #59435, #71242, #8107, #78819, #70827, #27449, #57755, #64925, #117, #7263, #21148, #65357, #46803, #59025, #72494, #33773, #27032, #46384 ),
 .UNSPECIFIED., .F., .F.,
 ( 4, 2, 2, 2, 2, 2, 2, 2, 2, 2, 2, 2, 2, 4 ),
 ( 0.06078874980787866283, 0.06175978776771125223, 0.06273082572754384856, 0.06370186368737643101, 0.06467290164720902734, 0.06564393960704162367, 0.06661497756687420613, 0.06855705348653938491, 0.06952809144637198124, 0.07049912940620456370, 0.07244120532586975636, 0.07341224328570235269, 0.07438328124553496290, 0.07632535716520016944 ),
 .UNSPECIFIED. ) ;
#44638 = DIRECTION ( 'NONE',  ( 1.000000000000000000, 0.000000000000000000, -0.000000000000000000 ) ) ;
#44639 = CARTESIAN_POINT ( 'NONE',  ( -0.9448818897637790704, -0.1870078740157479769, 0.4822834645669291653 ) ) ;
#44640 = CARTESIAN_POINT ( 'NONE',  ( 0.1265901696524990294, -0.4724409448818896462, -0.4002624671916010235 ) ) ;
#44641 = EDGE_CURVE ( 'NONE', #7205, #9834, #82717, .T. ) ;
#44642 = CARTESIAN_POINT ( 'NONE',  ( 0.2925321140481932369, -0.2925321140481932369, -0.2559055118110236116 ) ) ;
#44643 = ORIENTED_EDGE ( 'NONE', *, *, #63199, .F. ) ;
#44644 = CARTESIAN_POINT ( 'NONE',  ( -0.03280839895013062252, 0.1771653543307087075, -0.09757992244046823083 ) ) ;
#44645 = CARTESIAN_POINT ( 'NONE',  ( 4.797336870675656522E-17, -0.3917322834645670104, -1.960629921259842368 ) ) ;
#44646 = CARTESIAN_POINT ( 'NONE',  ( 0.8727034120734912248, -0.3162353388693409650, -0.4822834645669289433 ) ) ;
#44647 = CARTESIAN_POINT ( 'NONE',  ( -0.4091458600556405756, 0.2362204724409446288, -2.703412073490813583 ) ) ;
#44648 = CARTESIAN_POINT ( 'NONE',  ( -0.03443470937339725840, 0.000000000000000000, -1.320480459168889897 ) ) ;
#44649 = CARTESIAN_POINT ( 'NONE',  ( -0.4986876640419939388, 0.1283753931104746893, -0.1820866141732285504 ) ) ;
#44650 = DIRECTION ( 'NONE',  ( 0.000000000000000000, 0.8660254037844387076, -0.4999999999999998890 ) ) ;
#44651 = CARTESIAN_POINT ( 'NONE',  ( 0.9842519685039378130, -0.6692913385826771977, 8.415575281601705876E-17 ) ) ;
#44652 = CARTESIAN_POINT ( 'NONE',  ( 0.8333333333333340365, 0.1771653543307087075, -0.09757992244046823083 ) ) ;
#44653 = CARTESIAN_POINT ( 'NONE',  ( 0.09842519685039434474, 0.1660481256975885056, 0.3530559997133364547 ) ) ;
#44654 = CARTESIAN_POINT ( 'NONE',  ( 0.3917322834645669549, 2.398668435337827645E-17, -0.8280646737194732321 ) ) ;
#44655 = CARTESIAN_POINT ( 'NONE',  ( -0.3346456692913377662, 0.1660481256975883668, -0.3530559997133364547 ) ) ;
#44656 = CARTESIAN_POINT ( 'NONE',  ( -1.167979002624671470, -0.3690944881889765550, -0.3153832671262227771 ) ) ;
#44657 = CARTESIAN_POINT ( 'NONE',  ( -0.3477690288713905509, -0.6692913385826771977, 0.1292274648535927661 ) ) ;
#44658 = CARTESIAN_POINT ( 'NONE',  ( 1.561679790026247350, 0.05413385826771626580, -0.4176697321401330321 ) ) ;
#44659 = PLANE ( 'NONE',  #42287 ) ;
#44660 = ORIENTED_EDGE ( 'NONE', *, *, #24957, .T. ) ;
#44661 = CARTESIAN_POINT ( 'NONE',  ( -0.3917322834645671770, 0.1049643490035302024, -2.076790969325146730 ) ) ;
#44662 = CARTESIAN_POINT ( 'NONE',  ( 0.6233595800524942554, -0.05778040916215560624, -0.4822834645669293319 ) ) ;
#44663 = EDGE_LOOP ( 'NONE', ( #66979, #17991, #31393, #8677 ) ) ;
#44664 = CARTESIAN_POINT ( 'NONE',  ( -0.6889763779527552368, -0.5400638737290845981, -0.3530559997133363437 ) ) ;
#44665 = CARTESIAN_POINT ( 'NONE',  ( 1.469816272965879911, 0.2306618581243847221, -0.2411417322834647770 ) ) ;
#44666 = CARTESIAN_POINT ( 'NONE',  ( 0.7152230971128614723, -0.3162353388693409650, -0.4822834645669289433 ) ) ;
#44667 = VECTOR ( 'NONE', #11542, 39.37007874015748143 ) ;
#44668 = CARTESIAN_POINT ( 'NONE',  ( 0.05905511811023709395, -0.5400638737290844871, 0.3530559997133364547 ) ) ;
#44669 = CARTESIAN_POINT ( 'NONE',  ( -0.3917322834645669549, -0.1049643490035306603, -1.232939632545931863 ) ) ;
#44670 = CARTESIAN_POINT ( 'NONE',  ( -0.7086614173228339419, -0.1870078740157480879, -0.4822834645669291653 ) ) ;
#44671 = CARTESIAN_POINT ( 'NONE',  ( -0.2493438320209966919, -0.4281496062992124485, 0.4176697321401328655 ) ) ;
#44672 = CARTESIAN_POINT ( 'NONE',  ( -0.6627296587926501115, 0.2952755905511810774, -0.1292274648535930714 ) ) ;
#44673 = CARTESIAN_POINT ( 'NONE',  ( -0.01968503937007793844, 0.07958543189024071263, -0.2665933059059888421 ) ) ;
#44674 = CARTESIAN_POINT ( 'NONE',  ( -0.5944687039322197331, 1.968503937007873850, 0.4915354330708656128 ) ) ;
#44675 = CARTESIAN_POINT ( 'NONE',  ( -0.2362204724409442680, -0.1870078740157480879, -0.4822834645669291653 ) ) ;
#44676 = CARTESIAN_POINT ( 'NONE',  ( 3.908813327757459266, 1.601535082192234727, -0.4703318888109126461 ) ) ;
#44677 = CARTESIAN_POINT ( 'NONE',  ( 1.266404199475066328, -0.05778040916215522460, 0.4822834645669289988 ) ) ;
#44678 = ORIENTED_EDGE ( 'NONE', *, *, #14066, .F. ) ;
#44679 = ORIENTED_EDGE ( 'NONE', *, *, #41491, .F. ) ;
#44680 = CARTESIAN_POINT ( 'NONE',  ( 0.4396325459317593221, 0.2952755905511810774, -0.1292274648535930714 ) ) ;
#44681 = CARTESIAN_POINT ( 'NONE',  ( -0.4396325459317579898, 0.1771653543307087630, 0.09757992244046791164 ) ) ;
#44683 = CARTESIAN_POINT ( 'NONE',  ( -0.4724409448818898682, -8.678599364036362592E-17, -0.3543307086614173040 ) ) ;
#44682 = CARTESIAN_POINT ( 'NONE',  ( 1.561679790026247350, -0.004921259842519870586, -0.3153832671262229437 ) ) ;
#44684 = CARTESIAN_POINT ( 'NONE',  ( 0.3917322834645670104, -0.1049643490035303411, -1.298556430446194510 ) ) ;
#44685 = CARTESIAN_POINT ( 'NONE',  ( -1.157146581871515012E-16, 0.4724409448818898682, -0.3917322834645669549 ) ) ;
#44686 = FACE_OUTER_BOUND ( 'NONE', #2064, .T. ) ;
#44687 = CARTESIAN_POINT ( 'NONE',  ( 1.541994750656168645, -0.6692913385826771977, 0.1292274648535927661 ) ) ;
#44688 = CARTESIAN_POINT ( 'NONE',  ( -0.1974969037888704149, -0.3420746716998661063, 0.1725721784776902690 ) ) ;
#44689 = CARTESIAN_POINT ( 'NONE',  ( -0.04593175853018302557, -0.6692913385826773087, -0.1292274648535924053 ) ) ;
#44690 = CARTESIAN_POINT ( 'NONE',  ( -1.115485564304461219, 0.05413385826771626580, -0.4176697321401330321 ) ) ;
#44691 = CARTESIAN_POINT ( 'NONE',  ( -1.312335958005248715, -0.6046776061558809534, -0.2411417322834644161 ) ) ;
#44692 = CARTESIAN_POINT ( 'NONE',  ( 0.4593175853018379162, -0.4281496062992124485, 0.4176697321401328655 ) ) ;
#44693 = CARTESIAN_POINT ( 'NONE',  ( 0.3949938075777408852, 0.1058382717557500435, -0.2014435695538058235 ) ) ;
#44694 = CARTESIAN_POINT ( 'NONE',  ( 1.692913385826772421, 0.2952755905511811885, 0.000000000000000000 ) ) ;
#44695 = CARTESIAN_POINT ( 'NONE',  ( 1.095800524934383846, -0.3162353388693405765, 0.4822834645669290543 ) ) ;
#44696 = CARTESIAN_POINT ( 'NONE',  ( 1.272965879265092637, -0.3690944881889765550, -0.3153832671262227771 ) ) ;
#44697 = CARTESIAN_POINT ( 'NONE',  ( -0.1265901696524993347, 0.4724409448818896462, -0.9514435695538056015 ) ) ;
#44698 = CARTESIAN_POINT ( 'NONE',  ( 0.8858267716535438430, 0.07958543189024085140, 0.2665933059059887866 ) ) ;
#44699 = CARTESIAN_POINT ( 'NONE',  ( -1.272965879265091305, 0.05413385826771626580, -0.4176697321401330321 ) ) ;
#44700 = CARTESIAN_POINT ( 'NONE',  ( 0.1998031496062994128, -0.3460692066303957537, -1.113517060367454015 ) ) ;
#44701 = CARTESIAN_POINT ( 'NONE',  ( 1.095800524934383846, -0.05778040916215560624, -0.4822834645669293319 ) ) ;
#44702 =( BOUNDED_CURVE ( )  B_SPLINE_CURVE ( 2, ( #33293, #893, #32436, #6764, #82552, #26550, #52203, #24870, #50538, #38336, #45, #77062, #34537 ),
 .UNSPECIFIED., .F., .F. ) 
 B_SPLINE_CURVE_WITH_KNOTS ( ( 3, 2, 2, 2, 2, 2, 3 ),
 ( 0.8625000000000000444, 0.8666666666666666963, 0.8708333333333333481, 0.8750000000000001110, 0.8791666666666667629, 0.8833333333333334147, 0.8875000000000000666 ),
 .UNSPECIFIED. ) 
 CURVE ( )  GEOMETRIC_REPRESENTATION_ITEM ( )  RATIONAL_B_SPLINE_CURVE ( ( 1.000000000000000000, 0.9659258262890683122, 1.000000000000000000, 0.9659258262890683122, 1.000000000000000000, 0.9659258262890683122, 1.000000000000000000, 0.9659258262890683122, 1.000000000000000000, 0.9659258262890683122, 1.000000000000000000, 0.9659258262890674240, 1.000000000000000888 ) ) 
 REPRESENTATION_ITEM ( '' )  );
#44703 = CARTESIAN_POINT ( 'NONE',  ( -0.3917322834645670104, -7.196005306013484475E-17, -0.1889763779527558474 ) ) ;
#44705 = CYLINDRICAL_SURFACE ( 'NONE', #82878, 0.4724409448818898682 ) ;
#44704 = CARTESIAN_POINT ( 'NONE',  ( 0.7874015748031503170, -0.1870078740157480879, -0.4822834645669291653 ) ) ;
#44706 = CARTESIAN_POINT ( 'NONE',  ( -1.502624671916009680, -0.08942795157528024563, -0.3641732283464568787 ) ) ;
#44707 = CARTESIAN_POINT ( 'NONE',  ( -0.1115485564304453947, -0.6692913385826771977, 0.1292274648535927661 ) ) ;
#44708 = CARTESIAN_POINT ( 'NONE',  ( 0.9973753280839902091, 0.1283753931104746893, -0.1820866141732285504 ) ) ;
#44709 = CARTESIAN_POINT ( 'NONE',  ( 1.082677165354331228, 0.1660481256975883668, -0.3530559997133364547 ) ) ;
#44710 = FACE_OUTER_BOUND ( 'NONE', #22336, .T. ) ;
#44711 = CARTESIAN_POINT ( 'NONE',  ( -0.7152230971128602510, -0.08942795157528024563, -0.3641732283464568787 ) ) ;
#44712 = CARTESIAN_POINT ( 'NONE',  ( -0.7480314960629914633, 0.2952755905511811885, 0.000000000000000000 ) ) ;
#44713 = CARTESIAN_POINT ( 'NONE',  ( -1.574803149606298192, -0.1870078740157480601, -0.3641732283464567677 ) ) ;
#44714 = CARTESIAN_POINT ( 'NONE',  ( -1.122047244094487306, -0.5400638737290844871, 0.3530559997133364547 ) ) ;
#44715 = CARTESIAN_POINT ( 'NONE',  ( 0.9317585301837276734, 0.05413385826771626580, -0.4176697321401330321 ) ) ;
#44716 = CARTESIAN_POINT ( 'NONE',  ( -0.1958661417322833942, -0.3392501089628018884, -0.8497568485902381452 ) ) ;
#44717 = CARTESIAN_POINT ( 'NONE',  ( -1.338582677165353729, -0.1870078740157479769, 0.3641732283464567677 ) ) ;
#44718 = CARTESIAN_POINT ( 'NONE',  ( 2.554262525012302110, 1.537401574803149984, 0.4744094488188975722 ) ) ;
#44719 = CARTESIAN_POINT ( 'NONE',  ( 1.049868766404200127, -0.6046776061558809534, -0.2411417322834644161 ) ) ;
#44720 = CARTESIAN_POINT ( 'NONE',  ( -0.4091458600556405756, 0.2362204724409446288, -2.622703412073490892 ) ) ;
#44721 = CARTESIAN_POINT ( 'NONE',  ( -1.496062992125983815, -0.1870078740157480879, -0.4822834645669291653 ) ) ;
#44722 = CARTESIAN_POINT ( 'NONE',  ( -1.476377952755905110, 0.07958543189024085140, 0.2665933059059887866 ) ) ;
#44723 = CARTESIAN_POINT ( 'NONE',  ( -1.207349081364828880, 0.1283753931104746893, -0.1820866141732285504 ) ) ;
#44724 = CARTESIAN_POINT ( 'NONE',  ( 1.170004705068746986, -4.479759449472349425E-16, -0.3954985857520055825 ) ) ;
#44725 = CARTESIAN_POINT ( 'NONE',  ( -0.4986876640419939388, 0.2306618581243847221, -0.2411417322834647770 ) ) ;
#44726 = CARTESIAN_POINT ( 'NONE',  ( -0.2559055118110227234, -0.4536011799217367080, 0.2665933059059888421 ) ) ;
#44727 = CARTESIAN_POINT ( 'NONE',  ( -1.515748031496062076, 0.07958543189024071263, -0.2665933059059888421 ) ) ;
#44728 = CARTESIAN_POINT ( 'NONE',  ( 1.010498687664042716, -0.004921259842519870586, -0.3153832671262229437 ) ) ;
#44729 = VECTOR ( 'NONE', #57683, 39.37007874015748143 ) ;
#44730 = CARTESIAN_POINT ( 'NONE',  ( 0.4002624671916016896, -0.05778040916215522460, 0.4822834645669289988 ) ) ;
#44731 = CARTESIAN_POINT ( 'NONE',  ( 1.364829396325459854, -0.6046776061558809534, -0.2411417322834644161 ) ) ;
#44732 = CARTESIAN_POINT ( 'NONE',  ( -0.1312335958005241554, -0.5023911411419708095, -0.1820866141732282451 ) ) ;
#44733 = CARTESIAN_POINT ( 'NONE',  ( 0.5052493438320218022, -0.6692913385826773087, -0.1292274648535924053 ) ) ;
#44734 = CARTESIAN_POINT ( 'NONE',  ( 0.4330708661417329575, -0.5511811023622047445, 6.969142054262312111E-17 ) ) ;
#44735 = CARTESIAN_POINT ( 'NONE',  ( -1.581364829396324945, -0.05778040916215560624, -0.4822834645669293319 ) ) ;
#44736 = ADVANCED_FACE ( 'NONE', ( #76409 ), #5287, .T. ) ;
#44737 = CARTESIAN_POINT ( 'NONE',  ( -1.502624671916009680, -0.3162353388693405765, 0.4822834645669290543 ) ) ;
#44738 = CARTESIAN_POINT ( 'NONE',  ( -0.6036745406824141069, 0.2306618581243848609, 0.2411417322834645549 ) ) ;
#44739 = CARTESIAN_POINT ( 'NONE',  ( -0.2925321140481930704, -0.2925321140481933480, -0.3740157480314960092 ) ) ;
#44740 = CARTESIAN_POINT ( 'NONE',  ( -0.2925321140481932369, 0.2925321140481931259, -2.773622047244094002 ) ) ;
#44741 = CARTESIAN_POINT ( 'NONE',  ( 0.2755905511811031494, -0.6692913385826771977, 8.415575281601705876E-17 ) ) ;
#44742 = CARTESIAN_POINT ( 'NONE',  ( 1.220472440944882386, -0.5511811023622047445, 6.969142054262312111E-17 ) ) ;
#44743 = CARTESIAN_POINT ( 'NONE',  ( -0.5708661417322825615, -0.5400638737290844871, 0.3530559997133364547 ) ) ;
#44744 = CARTESIAN_POINT ( 'NONE',  ( 0.3674540682414705883, 0.2306618581243847221, -0.2411417322834647770 ) ) ;
#44745 = CARTESIAN_POINT ( 'NONE',  ( -0.1070741851644051862, -0.3996062992125987146, -2.119422572178477626 ) ) ;
#44746 = CARTESIAN_POINT ( 'NONE',  ( -0.3420746716998659953, -0.1974969037888706647, -1.627296587926509330 ) ) ;
#44747 = CARTESIAN_POINT ( 'NONE',  ( -0.3996062992125987146, 0.1070741851644051862, -2.709973753280840114 ) ) ;
#44748 = DIRECTION ( 'NONE',  ( 0.000000000000000000, 1.000000000000000000, 0.000000000000000000 ) ) ;
#44749 = CARTESIAN_POINT ( 'NONE',  ( -0.3917322834645669549, -0.1049643490035306603, -1.140419947506561504 ) ) ;
#44750 = CARTESIAN_POINT ( 'NONE',  ( -1.062992125984250968, 0.1771653543307087630, 0.000000000000000000 ) ) ;
#44751 = CARTESIAN_POINT ( 'NONE',  ( -1.200787401574802349, 0.1660481256975883668, -0.3530559997133364547 ) ) ;
#44752 = CARTESIAN_POINT ( 'NONE',  ( -0.1974969037888704149, -0.3420746716998661063, -2.504593175853018661 ) ) ;
#44753 = CARTESIAN_POINT ( 'NONE',  ( 0.8398950131233602345, -0.6046776061558807314, 0.2411417322834647770 ) ) ;
#44754 = CARTESIAN_POINT ( 'NONE',  ( 1.450131233595801428, 0.2952755905511811885, 0.1292274648535926551 ) ) ;
#44755 = CARTESIAN_POINT ( 'NONE',  ( 0.6430446194225728496, 0.05413385826771666132, 0.4176697321401328100 ) ) ;
#44756 = CARTESIAN_POINT ( 'NONE',  ( 0.4724409448818897572, -0.1265901696524988906, -2.946194225721785465 ) ) ;
#44757 = CARTESIAN_POINT ( 'NONE',  ( 0.3996062992125986590, -0.1070741851644053111, -2.158792650918635037 ) ) ;
#44758 = CARTESIAN_POINT ( 'NONE',  ( 0.2867679344610366554, -0.2867679344610365999, -0.7250849325797394940 ) ) ;
#44759 = CYLINDRICAL_SURFACE ( 'NONE', #33144, 0.1181102362204724116 ) ;
#44760 = CARTESIAN_POINT ( 'NONE',  ( 0.5643044619422579178, -0.4281496062992127816, -0.4176697321401328100 ) ) ;
#44761 = CARTESIAN_POINT ( 'NONE',  ( 0.6102362204724416372, -0.5400638737290844871, 0.3530559997133364547 ) ) ;
#44762 = CARTESIAN_POINT ( 'NONE',  ( 0.6692913385826777528, 0.1771653543307087630, 0.000000000000000000 ) ) ;
#44763 = CARTESIAN_POINT ( 'NONE',  ( 1.128608923884515169, -0.6046776061558809534, -0.2411417322834644161 ) ) ;
#44764 = CARTESIAN_POINT ( 'NONE',  ( 0.1049643490035303689, 0.3917322834645670104, -0.2355643044619422921 ) ) ;
#44765 = CARTESIAN_POINT ( 'NONE',  ( 0.5380577427821529035, 0.05413385826771626580, -0.4176697321401330321 ) ) ;
#44766 = CARTESIAN_POINT ( 'NONE',  ( 0.9842519685039378130, -0.6692913385826771977, 8.415575281601705876E-17 ) ) ;
#44767 = CARTESIAN_POINT ( 'NONE',  ( 0.4133858267716541968, 0.1660481256975885056, 0.3530559997133364547 ) ) ;
#44768 = CARTESIAN_POINT ( 'NONE',  ( 1.161417322834646493, -0.4536011799217367080, 0.2665933059059888421 ) ) ;
#44769 = CARTESIAN_POINT ( 'NONE',  ( -0.9711286089238838626, -0.6046776061558807314, 0.2411417322834647770 ) ) ;
#44770 = CARTESIAN_POINT ( 'NONE',  ( -1.200787401574802349, 0.1660481256975883668, -0.3530559997133364547 ) ) ;
#44771 = CARTESIAN_POINT ( 'NONE',  ( 1.122047244094488860, 0.1660481256975885056, 0.3530559997133364547 ) ) ;
#44772 = CARTESIAN_POINT ( 'NONE',  ( 0.3917322834645669549, 0.1049643490035304660, -0.6817585301837268963 ) ) ;
#44773 = CARTESIAN_POINT ( 'NONE',  ( -0.1958661417322834220, -0.3392501089628018884, -1.475065616797900381 ) ) ;
#44774 = CARTESIAN_POINT ( 'NONE',  ( 0.1958661417322836440, -0.3392501089628017219, -2.761154855643044304 ) ) ;
#44775 = ORIENTED_EDGE ( 'NONE', *, *, #17090, .T. ) ;
#44776 = CARTESIAN_POINT ( 'NONE',  ( 0.1998031496062994405, -0.3460692066303958092, -0.09186351706036746667 ) ) ;
#44777 = ORIENTED_EDGE ( 'NONE', *, *, #11980, .T. ) ;
#44778 = CARTESIAN_POINT ( 'NONE',  ( 1.482939632545932307, -0.4281496062992124485, 0.4176697321401328655 ) ) ;
#44779 = CARTESIAN_POINT ( 'NONE',  ( 1.213910761154856299, -0.5511811023622048555, -0.09757992244046775898 ) ) ;
#44780 = CARTESIAN_POINT ( 'NONE',  ( -0.1070741851644056997, 0.3996062992125986035, -1.423884514435695525 ) ) ;
#44781 = CARTESIAN_POINT ( 'NONE',  ( 1.437007874015748810, -0.4536011799217368745, -0.2665933059059886201 ) ) ;
#44782 = CARTESIAN_POINT ( 'NONE',  ( -0.2462293917967295909, -2.567464376874931580E-15, -0.4445507791589072832 ) ) ;
#44783 = CARTESIAN_POINT ( 'NONE',  ( -0.4606976121171968419, 1.423084236280317993, 2.585293067984823612 ) ) ;
#44784 = CARTESIAN_POINT ( 'NONE',  ( 0.3928700489057012635, -0.01966910102760525275, -1.929133858267715329 ) ) ;
#44785 = CARTESIAN_POINT ( 'NONE',  ( -0.3917322834645669549, -0.1049643490035306603, -0.9179790026246721357 ) ) ;
#44786 = CIRCLE ( 'NONE', #34077, 3.267716535433071279 ) ;
#44787 = CARTESIAN_POINT ( 'NONE',  ( -0.5577427821522301654, -0.2845877964562159024, 0.3641732283464567677 ) ) ;
#44788 = CARTESIAN_POINT ( 'NONE',  ( -1.417322834645668772, -0.1870078740157479769, 0.3641732283464567677 ) ) ;
#44789 = CARTESIAN_POINT ( 'NONE',  ( -1.076115485564303809, -0.6046776061558809534, -0.2411417322834644161 ) ) ;
#44790 = CARTESIAN_POINT ( 'NONE',  ( 0.09842519685039434474, -0.5400638737290845981, -0.3530559997133363437 ) ) ;
#44791 = CARTESIAN_POINT ( 'NONE',  ( -1.555118110236219930, -0.5400638737290845981, -0.3530559997133363437 ) ) ;
#44792 = VERTEX_POINT ( 'NONE', #56615 ) ;
#44793 = DIRECTION ( 'NONE',  ( 0.000000000000000000, 0.000000000000000000, 1.000000000000000000 ) ) ;
#44794 = LENGTH_MEASURE_WITH_UNIT ( LENGTH_MEASURE( 0.02539999999999999897 ), #70076 );
#44795 = CARTESIAN_POINT ( 'NONE',  ( 0.4724409448818897572, -0.1265901696524988906, -2.158792650918635037 ) ) ;
#44796 = DIRECTION ( 'NONE',  ( 1.000000000000000000, 0.000000000000000000, -0.000000000000000000 ) ) ;
#44797 = CARTESIAN_POINT ( 'NONE',  ( -0.6627296587926501115, 0.1771653543307087075, -0.09757992244046823083 ) ) ;
#44798 = B_SPLINE_CURVE_WITH_KNOTS ( 'NONE', 3,
 ( #42551, #67419, #68254, #72899 ),
 .UNSPECIFIED., .F., .F.,
 ( 4, 4 ),
 ( 0.07610408314619493408, 0.07753336624204351657 ),
 .UNSPECIFIED. ) ;
#44799 = CARTESIAN_POINT ( 'NONE',  ( -1.207349081364828436, -0.6046776061558807314, 0.2411417322834647770 ) ) ;
#44800 = CARTESIAN_POINT ( 'NONE',  ( 1.128608923884515169, -0.6046776061558809534, -0.2411417322834644161 ) ) ;
#44801 = ORIENTED_EDGE ( 'NONE', *, *, #70218, .F. ) ;
#44803 = CARTESIAN_POINT ( 'NONE',  ( 0.1265901696524990572, -0.4724409448818897017, -2.681758530183727451 ) ) ;
#44802 = CARTESIAN_POINT ( 'NONE',  ( 5.785732909357575061E-17, -0.4724409448818898682, -2.517716535433071279 ) ) ;
#44804 = CARTESIAN_POINT ( 'NONE',  ( 1.128608923884515169, -0.6046776061558809534, -0.2411417322834644161 ) ) ;
#44805 = CARTESIAN_POINT ( 'NONE',  ( -1.332020997375327642, -0.3162353388693409650, -0.4822834645669289433 ) ) ;
#44806 = CARTESIAN_POINT ( 'NONE',  ( 0.3917322834645669549, 2.398668435337827645E-17, -0.6705843587588433685 ) ) ;
#44807 = CARTESIAN_POINT ( 'NONE',  ( -0.2034120734908131112, -0.5511811023622048555, -0.09757992244046775898 ) ) ;
#44808 = CARTESIAN_POINT ( 'NONE',  ( 0.3392501089628018884, -0.1958661417322834220, -0.8195538057742782767 ) ) ;
#44809 = CARTESIAN_POINT ( 'NONE',  ( -0.4986876640419939388, 0.1283753931104746893, -0.1820866141732285504 ) ) ;
#44810 = CARTESIAN_POINT ( 'NONE',  ( -0.01968503937007793844, -0.4536011799217367080, 0.2665933059059888421 ) ) ;
#44811 = CARTESIAN_POINT ( 'NONE',  ( -0.07217847769028813698, -0.3162353388693409650, -0.4822834645669289433 ) ) ;
#44812 = CARTESIAN_POINT ( 'NONE',  ( -1.325459317585300889, -0.004921259842519576551, 0.3153832671262227771 ) ) ;
#44813 = CARTESIAN_POINT ( 'NONE',  ( -0.3917322834645670104, -7.196005306013484475E-17, -2.708661417322834275 ) ) ;
#44814 = CARTESIAN_POINT ( 'NONE',  ( 1.082677165354331228, -0.5400638737290844871, 0.3530559997133364547 ) ) ;
#44815 = CARTESIAN_POINT ( 'NONE',  ( -1.299212598425196097, 0.2952755905511811885, 0.000000000000000000 ) ) ;
#44816 = CARTESIAN_POINT ( 'NONE',  ( -1.157146581871515012E-16, 0.4724409448818898682, -1.179133858267716661 ) ) ;
#44817 = CARTESIAN_POINT ( 'NONE',  ( -0.5052493438320203589, -0.6692913385826771977, 0.1292274648535927661 ) ) ;
#44818 = CARTESIAN_POINT ( 'NONE',  ( -0.7808398950131222316, -0.3162353388693409650, -0.4822834645669289433 ) ) ;
#44819 = CARTESIAN_POINT ( 'NONE',  ( 1.003937007874016407, -0.4536011799217367080, 0.2665933059059888421 ) ) ;
#44820 = CARTESIAN_POINT ( 'NONE',  ( -0.3871391076115479057, -0.2845877964562161244, -0.3641732283464567121 ) ) ;
#44821 = CARTESIAN_POINT ( 'NONE',  ( -0.5118110236220466680, -0.6692913385826771977, 8.415575281601705876E-17 ) ) ;
#44822 = CARTESIAN_POINT ( 'NONE',  ( -1.207349081364828436, -0.6046776061558807314, 0.2411417322834647770 ) ) ;
#44823 = DIRECTION ( 'NONE',  ( 1.000000000000000000, -0.000000000000000000, -0.000000000000000000 ) ) ;
#44824 = CARTESIAN_POINT ( 'NONE',  ( 1.318897637795276356, -0.4536011799217367080, 0.2665933059059888421 ) ) ;
#44825 = AXIS2_PLACEMENT_3D ( 'NONE', #18990, #50960, #44638 ) ;
#44826 = CARTESIAN_POINT ( 'NONE',  ( -0.1509186351706028884, -0.3162353388693409650, -0.4822834645669289433 ) ) ;
#44827 = CARTESIAN_POINT ( 'NONE',  ( -1.456692913385826182, -0.6692913385826771977, 8.415575281601705876E-17 ) ) ;
#44828 = VERTEX_POINT ( 'NONE', #38087 ) ;
#44829 = CARTESIAN_POINT ( 'NONE',  ( -9.787531504996566615E-17, 0.3996062992125985480, -2.438976377952756014 ) ) ;
#44830 = CARTESIAN_POINT ( 'NONE',  ( -0.7808398950131222316, -0.2845877964562161244, -0.3641732283464567121 ) ) ;
#44831 = CARTESIAN_POINT ( 'NONE',  ( 0.6233595800524939223, -0.3162353388693405765, 0.4822834645669290543 ) ) ;
#44832 = CARTESIAN_POINT ( 'NONE',  ( -0.9908136482939626788, -0.5511811023622048555, -0.09757992244046775898 ) ) ;
#44833 = CARTESIAN_POINT ( 'NONE',  ( 0.1070741851644053388, 0.3996062992125986035, -1.172572178477690352 ) ) ;
#44834 = CARTESIAN_POINT ( 'NONE',  ( -1.154855643044618851, -0.6046776061558809534, -0.2411417322834644161 ) ) ;
#44835 = CARTESIAN_POINT ( 'NONE',  ( 0.7480314960629927956, 0.2952755905511811885, 0.000000000000000000 ) ) ;
#44836 = CARTESIAN_POINT ( 'NONE',  ( 0.3346456692913393205, -0.5400638737290845981, -0.3530559997133363437 ) ) ;
#44837 = CARTESIAN_POINT ( 'NONE',  ( 1.437007874015748810, 0.1660481256975885056, 0.3530559997133364547 ) ) ;
#44838 = CARTESIAN_POINT ( 'NONE',  ( -1.561679790026246017, -0.004921259842519576551, 0.3153832671262227771 ) ) ;
#44839 = CARTESIAN_POINT ( 'NONE',  ( -9.787531504996566615E-17, 0.3996062992125985480, -0.7066929133858268486 ) ) ;
#44840 = CARTESIAN_POINT ( 'NONE',  ( -0.3996062992125986035, -0.1070741851644056997, -0.9908136482939633449 ) ) ;
#44841 = AXIS2_PLACEMENT_3D ( 'NONE', #16443, #40852, #66537 ) ;
#44842 = CARTESIAN_POINT ( 'NONE',  ( -0.3949938075777411628, 0.1058382717557497937, -0.3477690288713912170 ) ) ;
#44843 = CARTESIAN_POINT ( 'NONE',  ( 0.4741686481756308691, 1.554815631980118740, 2.554860351194805368 ) ) ;
#44844 = CARTESIAN_POINT ( 'NONE',  ( 1.102362204724410155, -0.1870078740157480601, -0.3641732283464567677 ) ) ;
#44845 = CARTESIAN_POINT ( 'NONE',  ( 0.8792650918635177559, -0.3690944881889765550, -0.3153832671262227771 ) ) ;
#44846 = CARTESIAN_POINT ( 'NONE',  ( 0.2427821522309716595, -0.3162353388693409650, -0.4822834645669289433 ) ) ;
#44847 = LINE ( 'NONE', #76050, #5129 ) ;
#44848 = CARTESIAN_POINT ( 'NONE',  ( 0.2891555358219910499, -0.2891555358219909944, -1.120078740157480324 ) ) ;
#44849 = CARTESIAN_POINT ( 'NONE',  ( 0.3018372703412079971, -0.004921259842519870586, -0.3153832671262229437 ) ) ;
#44850 = CARTESIAN_POINT ( 'NONE',  ( -0.8792650918635160906, -0.4281496062992124485, 0.4176697321401328655 ) ) ;
#44851 = CARTESIAN_POINT ( 'NONE',  ( -1.351706036745406347, -0.4281496062992124485, 0.4176697321401328655 ) ) ;
#44852 = CARTESIAN_POINT ( 'NONE',  ( 0.6889763779527566800, -0.5400638737290844871, 0.3530559997133364547 ) ) ;
#44853 = CARTESIAN_POINT ( 'NONE',  ( 5.785732909357575061E-17, -0.4724409448818898682, -1.653543307086614123 ) ) ;
#44854 = DIRECTION ( 'NONE',  ( -0.000000000000000000, -1.000000000000000000, -0.000000000000000000 ) ) ;
#44855 = ORIENTED_EDGE ( 'NONE', *, *, #35758, .F. ) ;
#44856 = ORIENTED_EDGE ( 'NONE', *, *, #17268, .F. ) ;
#44857 = CARTESIAN_POINT ( 'NONE',  ( -1.476377952755905110, -0.5400638737290845981, -0.3530559997133363437 ) ) ;
#44858 = CARTESIAN_POINT ( 'NONE',  ( -0.5643044619422565855, -0.4281496062992124485, 0.4176697321401328655 ) ) ;
#44860 = CARTESIAN_POINT ( 'NONE',  ( -0.8595800524934373854, -0.05778040916215522460, 0.4822834645669289988 ) ) ;
#44859 = CARTESIAN_POINT ( 'NONE',  ( -0.8530183727034112984, -0.004921259842519576551, 0.3153832671262227771 ) ) ;
#44861 = CARTESIAN_POINT ( 'NONE',  ( -0.2867679344610366554, 0.2867679344610365444, -2.146962311514748478 ) ) ;
#44862 = CARTESIAN_POINT ( 'NONE',  ( 0.000000000000000000, 2.755905511811024056, 0.000000000000000000 ) ) ;
#44863 = CARTESIAN_POINT ( 'NONE',  ( -1.515748031496062076, -0.4536011799217367080, 0.2665933059059888421 ) ) ;
#44864 = CARTESIAN_POINT ( 'NONE',  ( -0.8792650918635160906, 0.05413385826771626580, -0.4176697321401330321 ) ) ;
#44865 = CARTESIAN_POINT ( 'NONE',  ( 0.3083989501312343062, -0.3162353388693405765, 0.4822834645669290543 ) ) ;
#44866 = ADVANCED_FACE ( 'NONE', ( #50710 ), #31776, .T. ) ;
#44867 = CARTESIAN_POINT ( 'NONE',  ( -0.8464566929133852113, 0.1660481256975885056, 0.3530559997133364547 ) ) ;
#44868 = ADVANCED_FACE ( 'NONE', ( #36860 ), #6102, .T. ) ;
#44869 = CARTESIAN_POINT ( 'NONE',  ( -9.594673741351313045E-17, 0.3917322834645670104, -1.566929133858267820 ) ) ;
#44870 = CARTESIAN_POINT ( 'NONE',  ( -1.003937007874014853, 0.07958543189024085140, 0.2665933059059887866 ) ) ;
#44871 = VERTEX_POINT ( 'NONE', #40176 ) ;
#44872 = CARTESIAN_POINT ( 'NONE',  ( 0.1974969037888704704, 0.3420746716998660508, -1.719160104986876769 ) ) ;
#44873 = ORIENTED_EDGE ( 'NONE', *, *, #24294, .T. ) ;
#44874 = CARTESIAN_POINT ( 'NONE',  ( -1.574803149606298636, -0.1870078740157479769, 0.3641732283464567677 ) ) ;
#44875 = CARTESIAN_POINT ( 'NONE',  ( -1.200787401574802349, -0.5400638737290844871, 0.3530559997133364547 ) ) ;
#44876 = CARTESIAN_POINT ( 'NONE',  ( -1.089238845144356427, -0.4281496062992127816, -0.4176697321401328100 ) ) ;
#44877 = CARTESIAN_POINT ( 'NONE',  ( -0.3996062992125987146, 0.1070741851644051862, -0.3477690288713909950 ) ) ;
#44878 = CARTESIAN_POINT ( 'NONE',  ( -1.233595800524933894, 0.2306618581243848609, 0.2411417322834645549 ) ) ;
#44879 = CARTESIAN_POINT ( 'NONE',  ( -1.200787401574802349, 0.1660481256975883668, -0.3530559997133364547 ) ) ;
#44880 = CYLINDRICAL_SURFACE ( 'NONE', #49868, 0.5118110236220472231 ) ;
#44881 = DIRECTION ( 'NONE',  ( 0.000000000000000000, 0.000000000000000000, 1.000000000000000000 ) ) ;
#44882 = CARTESIAN_POINT ( 'NONE',  ( 0.5905511811023629321, 0.1771653543307087630, 0.000000000000000000 ) ) ;
#44883 = CARTESIAN_POINT ( 'NONE',  ( -0.4824498642376744417, -2.567464376874931580E-15, -0.4445507791589072832 ) ) ;
#44884 = CARTESIAN_POINT ( 'NONE',  ( -0.1958661417322836718, 0.3392501089628017219, -0.4127296587926510552 ) ) ;
#44885 = CARTESIAN_POINT ( 'NONE',  ( -0.2165354330708654795, -0.4536011799217368745, -0.2665933059059886201 ) ) ;
#44886 = AXIS2_PLACEMENT_3D ( 'NONE', #25294, #38764, #31202 ) ;
#44887 = CARTESIAN_POINT ( 'NONE',  ( -0.6430446194225712953, 0.05413385826771626580, -0.4176697321401330321 ) ) ;
#44888 = CARTESIAN_POINT ( 'NONE',  ( 1.358267716535433323, -0.5400638737290845981, -0.3530559997133363437 ) ) ;
#44889 = CARTESIAN_POINT ( 'NONE',  ( -0.5708661417322825615, -0.5400638737290844871, 0.3530559997133364547 ) ) ;
#44890 = VERTEX_POINT ( 'NONE', #20404 ) ;
#44891 = VERTEX_POINT ( 'NONE', #33860 ) ;
#44892 = CARTESIAN_POINT ( 'NONE',  ( -0.1070741851644056997, 0.3996062992125984925, -1.815616797900262425 ) ) ;
#44893 = CARTESIAN_POINT ( 'NONE',  ( -0.9580052493438311334, 0.05413385826771626580, -0.4176697321401330321 ) ) ;
#44894 = CARTESIAN_POINT ( 'NONE',  ( 1.154855643044620184, 0.2306618581243847221, -0.2411417322834647770 ) ) ;
#44895 = CARTESIAN_POINT ( 'NONE',  ( -1.194225721784776262, -0.004921259842519870586, -0.3153832671262229437 ) ) ;
#44896 = CARTESIAN_POINT ( 'NONE',  ( -1.404199475065615932, 0.05413385826771666132, 0.4176697321401328100 ) ) ;
#44897 = CARTESIAN_POINT ( 'NONE',  ( 5.785732909357575061E-17, -0.4724409448818898682, -1.023622047244094446 ) ) ;
#44898 = CARTESIAN_POINT ( 'NONE',  ( -2.112686649479645684, 1.697109554835842804, 0.4469779880792058568 ) ) ;
#44899 = EDGE_CURVE ( 'NONE', #79813, #82661, #1700, .T. ) ;
#44900 = CARTESIAN_POINT ( 'NONE',  ( -0.3917322834645669549, -0.1049643490035306603, -0.03805774278215218187 ) ) ;
#44901 = LINE ( 'NONE', #37785, #41250 ) ;
#44902 = CARTESIAN_POINT ( 'NONE',  ( 0.07217847769028949700, -0.3162353388693405765, 0.4822834645669290543 ) ) ;
#44903 = CARTESIAN_POINT ( 'NONE',  ( -0.9251968503937002541, -0.4536011799217368745, -0.2665933059059886201 ) ) ;
#44904 = CARTESIAN_POINT ( 'NONE',  ( -0.7086614173228339419, -0.1870078740157480879, -0.4822834645669291653 ) ) ;
#44905 = CARTESIAN_POINT ( 'NONE',  ( 5.785732909357575061E-17, -0.4724409448818898682, -2.675196850393700920 ) ) ;
#44906 = CARTESIAN_POINT ( 'NONE',  ( -1.305774278215222184, -0.6692913385826773087, -0.1292274648535924053 ) ) ;
#44907 = CARTESIAN_POINT ( 'NONE',  ( -1.174540682414697335, -0.3162353388693409650, -0.4822834645669289433 ) ) ;
#44908 = CARTESIAN_POINT ( 'NONE',  ( -0.1181102362204717315, 0.2952755905511811885, 0.000000000000000000 ) ) ;
#44909 = VECTOR ( 'NONE', #26716, 39.37007874015748143 ) ;
#44910 = CARTESIAN_POINT ( 'NONE',  ( 4.837279021331061486E-17, -0.3949938075777409963, -2.517716535433071279 ) ) ;
#44911 = CARTESIAN_POINT ( 'NONE',  ( 0.9186351706036751663, -0.5023911411419708095, 0.1820866141732285504 ) ) ;
#44912 = CARTESIAN_POINT ( 'NONE',  ( -0.7152230971128602510, -0.08942795157528024563, -0.3641732283464568787 ) ) ;
#44913 = CARTESIAN_POINT ( 'NONE',  ( -1.113459889019125182, -4.850200619981615293E-15, -0.3954974714151464621 ) ) ;
#44914 = CARTESIAN_POINT ( 'NONE',  ( 0.9317585301837276734, -0.004921259842519870586, -0.3153832671262229437 ) ) ;
#44915 = CARTESIAN_POINT ( 'NONE',  ( 1.200787401574803681, -0.4536011799217368745, -0.2665933059059886201 ) ) ;
#44916 = CARTESIAN_POINT ( 'NONE',  ( 1.253280839895013710, -0.3162353388693405765, 0.4822834645669290543 ) ) ;
#44917 = CARTESIAN_POINT ( 'NONE',  ( 0.5183727034120741983, -0.5511811023622046335, 0.09757992244046803654 ) ) ;
#44918 = CARTESIAN_POINT ( 'NONE',  ( 0.2867679344610365999, -0.2867679344610365444, -1.665354330708661124 ) ) ;
#44919 = CARTESIAN_POINT ( 'NONE',  ( -0.8923884514435688198, -0.6046776061558807314, 0.2411417322834647770 ) ) ;
#44920 = CARTESIAN_POINT ( 'NONE',  ( 1.167979002624672580, 0.05413385826771626580, -0.4176697321401330321 ) ) ;
#44921 = CARTESIAN_POINT ( 'NONE',  ( -0.4724409448818899238, 0.1265901696524986686, 0.04790026246719158304 ) ) ;
#44922 = CARTESIAN_POINT ( 'NONE',  ( -0.3346456692913377662, 0.07958543189024071263, -0.2665933059059888421 ) ) ;
#44923 = CARTESIAN_POINT ( 'NONE',  ( 0.7186703366786207914, -1.374501131054255944E-15, 0.4445507791589066726 ) ) ;
#44924 = CARTESIAN_POINT ( 'NONE',  ( 0.3215223097112867578, -0.3162353388693409650, -0.4822834645669289433 ) ) ;
#44925 = CARTESIAN_POINT ( 'NONE',  ( -1.614173228346456712, 2.401574803149606474, -0.1372047244094478091 ) ) ;
#44926 = CARTESIAN_POINT ( 'NONE',  ( 0.8727034120734912248, -0.2845877964562161244, -0.3641732283464567121 ) ) ;
#44927 = CARTESIAN_POINT ( 'NONE',  ( 0.2887139107611556010, -0.5023911411419708095, 0.1820866141732285504 ) ) ;
#44928 = CARTESIAN_POINT ( 'NONE',  ( 0.1574803149606306130, -0.1870078740157480879, -0.4822834645669291653 ) ) ;
#44929 = CARTESIAN_POINT ( 'NONE',  ( -1.154855643044618851, -0.6046776061558809534, -0.2411417322834644161 ) ) ;
#44930 = CARTESIAN_POINT ( 'NONE',  ( -0.5052493438320203589, 0.1771653543307087075, -0.09757992244046823083 ) ) ;
#44931 = DIRECTION ( 'NONE',  ( -1.000000000000000000, 0.000000000000000000, 0.000000000000000000 ) ) ;
#44932 = CARTESIAN_POINT ( 'NONE',  ( -0.4790026246719152336, -0.05778040916215560624, -0.4822834645669293319 ) ) ;
#44933 = CARTESIAN_POINT ( 'NONE',  ( -0.3996062992125986590, 0.1070741851644051723, -1.211942257217847541 ) ) ;
#44934 = CARTESIAN_POINT ( 'NONE',  ( -0.1049643490035302024, -0.3917322834645671215, -2.676509186351705871 ) ) ;
#44935 = CARTESIAN_POINT ( 'NONE',  ( 0.03280839895013198948, 0.1771653543307087630, 0.09757992244046791164 ) ) ;
#44936 = CARTESIAN_POINT ( 'NONE',  ( -0.6561679790026240244, 0.2306618581243847221, -0.2411417322834647770 ) ) ;
#44937 = CARTESIAN_POINT ( 'NONE',  ( -1.318897637795274802, 0.1660481256975885056, 0.3530559997133364547 ) ) ;
#44938 = CARTESIAN_POINT ( 'NONE',  ( -1.213910761154854745, -0.5511811023622046335, 0.09757992244046803654 ) ) ;
#44939 = CARTESIAN_POINT ( 'NONE',  ( -1.559171609364246924, 0.3937007874015748254, 0.4177787735906735578 ) ) ;
#44940 = EDGE_CURVE ( 'NONE', #15637, #43552, #22617, .T. ) ;
#44941 = CARTESIAN_POINT ( 'NONE',  ( -0.5577427821522301654, -0.3162353388693405765, 0.4822834645669290543 ) ) ;
#44942 = CARTESIAN_POINT ( 'NONE',  ( -0.8661417322834640276, -0.1870078740157479769, 0.3641732283464567677 ) ) ;
#44943 = CARTESIAN_POINT ( 'NONE',  ( -1.633858267716534529, -0.4536011799217368745, -0.2665933059059886201 ) ) ;
#44944 = CARTESIAN_POINT ( 'NONE',  ( 1.358267716535433323, -0.5400638737290845981, -0.3530559997133363437 ) ) ;
#44945 = CARTESIAN_POINT ( 'NONE',  ( -0.3458507752293906723, -0.3458507752293910609, -0.6889763779527556808 ) ) ;
#44946 = CARTESIAN_POINT ( 'NONE',  ( -0.3392501089628019995, 0.1958661417322831999, -2.070229289535120198 ) ) ;
#44947 = ORIENTED_EDGE ( 'NONE', *, *, #53708, .F. ) ;
#44948 = AXIS2_PLACEMENT_3D ( 'NONE', #33032, #45645, #46481 ) ;
#44949 = DIRECTION ( 'NONE',  ( 0.000000000000000000, 0.000000000000000000, -1.000000000000000000 ) ) ;
#44950 = CARTESIAN_POINT ( 'NONE',  ( -1.279527559055116948, -0.5400638737290844871, 0.3530559997133364547 ) ) ;
#44951 = CARTESIAN_POINT ( 'NONE',  ( -0.8333333333333323711, -0.6692913385826773087, -0.1292274648535924053 ) ) ;
#44952 = ADVANCED_FACE ( 'NONE', ( #8194 ), #76965, .F. ) ;
#44953 = CARTESIAN_POINT ( 'NONE',  ( -1.522309711286088607, -0.6046776061558807314, 0.2411417322834647770 ) ) ;
#44954 = CARTESIAN_POINT ( 'NONE',  ( 0.1049643490035304938, -0.3917322834645669549, -2.059711286089238591 ) ) ;
#44955 = CARTESIAN_POINT ( 'NONE',  ( 1.482939632545932307, -0.3690944881889763329, 0.3153832671262228327 ) ) ;
#44956 = CARTESIAN_POINT ( 'NONE',  ( 0.4790026246719168435, -0.3162353388693409650, -0.4822834645669289433 ) ) ;
#44957 = CARTESIAN_POINT ( 'NONE',  ( 0.1706036745406830368, -0.4281496062992127816, -0.4176697321401328100 ) ) ;
#44958 = CARTESIAN_POINT ( 'NONE',  ( -0.3256598226813641195, -3.773335473449285555E-15, -0.4118477457933000796 ) ) ;
#44959 = CARTESIAN_POINT ( 'NONE',  ( 0.1998031496062992463, 0.3460692066303959202, -2.740813648293963567 ) ) ;
#44960 = CARTESIAN_POINT ( 'NONE',  ( 0.8727034120734912248, -0.2845877964562161244, -0.3641732283464567121 ) ) ;
#44961 = CARTESIAN_POINT ( 'NONE',  ( -0.3996062992125986035, -0.1070741851644056997, -1.148293963254592986 ) ) ;
#44962 = EDGE_LOOP ( 'NONE', ( #80346, #63110, #35394, #2167 ) ) ;
#44964 = CARTESIAN_POINT ( 'NONE',  ( -0.2867679344610367109, 0.2867679344610365444, -0.01642351525690478181 ) ) ;
#44963 = CIRCLE ( 'NONE', #69216, 0.1574803149606299746 ) ;
#44965 = ORIENTED_EDGE ( 'NONE', *, *, #17897, .F. ) ;
#44966 = CARTESIAN_POINT ( 'NONE',  ( -0.2034120734908131112, -0.6692913385826773087, -0.1292274648535924053 ) ) ;
#44967 = CARTESIAN_POINT ( 'NONE',  ( -0.8202099737532801971, -0.6692913385826771977, 0.1292274648535927661 ) ) ;
#44968 = CARTESIAN_POINT ( 'NONE',  ( -1.325459317585300889, 0.05413385826771666132, 0.4176697321401328100 ) ) ;
#44969 = CARTESIAN_POINT ( 'NONE',  ( 0.6299212598425204535, -0.1870078740157480879, -0.4822834645669291653 ) ) ;
#44970 = CARTESIAN_POINT ( 'NONE',  ( -1.581364829396324945, -0.08942795157528024563, -0.3641732283464568787 ) ) ;
#44971 = CARTESIAN_POINT ( 'NONE',  ( 1.568241469816273437, -0.3162353388693405765, 0.4822834645669290543 ) ) ;
#44972 = CARTESIAN_POINT ( 'NONE',  ( -0.3740157480314953431, 0.1660481256975885056, 0.3530559997133364547 ) ) ;
#44973 = CARTESIAN_POINT ( 'NONE',  ( 0.4855643044619428750, 0.05413385826771666132, 0.4176697321401328100 ) ) ;
#44974 = CARTESIAN_POINT ( 'NONE',  ( -1.574803149606298192, -0.1870078740157480879, -0.4822834645669291653 ) ) ;
#44975 = CARTESIAN_POINT ( 'NONE',  ( 1.141732283464567566, 0.2952755905511811885, 0.000000000000000000 ) ) ;
#44976 = B_SPLINE_CURVE_WITH_KNOTS ( 'NONE', 3,
 ( #49040, #25010, #76381, #18715 ),
 .UNSPECIFIED., .F., .F.,
 ( 4, 4 ),
 ( 3.593986969187450165E-07, 0.001287825409103291428 ),
 .UNSPECIFIED. ) ;
#44977 = CARTESIAN_POINT ( 'NONE',  ( 1.627296587926509996, -0.6046776061558807314, 0.2411417322834647770 ) ) ;
#44978 = CARTESIAN_POINT ( 'NONE',  ( 0.04593175853018440641, 0.2952755905511810774, -0.1292274648535930714 ) ) ;
#44979 = CARTESIAN_POINT ( 'NONE',  ( -0.2867679344610365999, 0.2867679344610364889, -0.3267716535433070613 ) ) ;
#44980 = CARTESIAN_POINT ( 'NONE',  ( 0.4724409448818904789, -0.1870078740157480601, -0.3641732283464567677 ) ) ;
#44981 = ORIENTED_EDGE ( 'NONE', *, *, #60079, .F. ) ;
#44982 = CARTESIAN_POINT ( 'NONE',  ( -0.1058382717557497937, -0.3949938075777411628, -0.7020997375328085210 ) ) ;
#44983 = ORIENTED_EDGE ( 'NONE', *, *, #69760, .F. ) ;
#44984 = CARTESIAN_POINT ( 'NONE',  ( -0.2427821522309703550, -0.08942795157528024563, -0.3641732283464568787 ) ) ;
#44985 = CARTESIAN_POINT ( 'NONE',  ( -0.5314960629921395840, 2.677165354330708791, 3.900966923095588346 ) ) ;
#44986 = CARTESIAN_POINT ( 'NONE',  ( 0.2821522309711292364, -0.6692913385826771977, 0.1292274648535927661 ) ) ;
#44987 = CARTESIAN_POINT ( 'NONE',  ( 0.07874015748031558404, -0.1870078740157480879, -0.4822834645669291653 ) ) ;
#44988 = CARTESIAN_POINT ( 'NONE',  ( -0.8661417322834640276, -0.1870078740157480879, -0.4822834645669291653 ) ) ;
#44989 = CARTESIAN_POINT ( 'NONE',  ( 4.797336870675656522E-17, -0.3917322834645670659, -1.807762097934070278 ) ) ;
#44990 = CARTESIAN_POINT ( 'NONE',  ( -1.266404199475064773, -0.05778040916215560624, -0.4822834645669293319 ) ) ;
#44991 = CARTESIAN_POINT ( 'NONE',  ( 0.5314960629921348101, 2.729661042438510599, -2.530077748780001023 ) ) ;
#44992 = CARTESIAN_POINT ( 'NONE',  ( 0.8989501312335963501, -0.5511811023622048555, -0.09757992244046775898 ) ) ;
#44993 = CARTESIAN_POINT ( 'NONE',  ( 0.4527559055118117182, 0.1660481256975883668, -0.3530559997133364547 ) ) ;
#44994 = CARTESIAN_POINT ( 'NONE',  ( 0.8792650918635177559, 0.05413385826771666132, 0.4176697321401328100 ) ) ;
#44995 = CARTESIAN_POINT ( 'NONE',  ( 0.3460692066303959757, -0.1998031496062991907, -1.207349081364829324 ) ) ;
#44996 = CARTESIAN_POINT ( 'NONE',  ( -1.561679790026246017, 0.05413385826771666132, 0.4176697321401328100 ) ) ;
#44997 = CARTESIAN_POINT ( 'NONE',  ( 0.1070741851644054776, -0.3996062992125984925, -0.7919947506561679784 ) ) ;
#44998 = CARTESIAN_POINT ( 'NONE',  ( -0.3460692066303960313, 0.1998031496062989965, -0.2604986876640419946 ) ) ;
#44999 = CARTESIAN_POINT ( 'NONE',  ( -0.1377952755905504645, 0.1660481256975885056, 0.3530559997133364547 ) ) ;
#45000 = CARTESIAN_POINT ( 'NONE',  ( 0.3996062992125986590, -0.1070741851644053111, -2.631233595800525293 ) ) ;
#45001 = CARTESIAN_POINT ( 'NONE',  ( -0.1049643490035307020, 0.3917322834645669549, -1.508530183727033736 ) ) ;
#45002 = CARTESIAN_POINT ( 'NONE',  ( -1.227034120734907141, -0.5511811023622048555, -0.09757992244046775898 ) ) ;
#45003 = CARTESIAN_POINT ( 'NONE',  ( 1.220472440944882386, -0.6692913385826771977, 8.415575281601705876E-17 ) ) ;
#45004 = CARTESIAN_POINT ( 'NONE',  ( 1.227034120734908917, 0.2952755905511810774, -0.1292274648535930714 ) ) ;
#45005 = CARTESIAN_POINT ( 'NONE',  ( 0.006561679790026889343, -0.2845877964562161244, -0.3641732283464567121 ) ) ;
#45006 = CARTESIAN_POINT ( 'NONE',  ( 0.4921259842519691285, 0.1660481256975885056, 0.3530559997133364547 ) ) ;
#45007 = CARTESIAN_POINT ( 'NONE',  ( 0.1265901696524990294, -0.4724409448818896462, -1.421916010498687877 ) ) ;
#45008 = CARTESIAN_POINT ( 'NONE',  ( 0.4986876640419954376, -0.5023911411419708095, -0.1820866141732282451 ) ) ;
#45009 = CARTESIAN_POINT ( 'NONE',  ( 0.2427821522309716595, -0.3162353388693409650, -0.4822834645669289433 ) ) ;
#45010 = CARTESIAN_POINT ( 'NONE',  ( 0.1974969037888704704, 0.3420746716998660508, -1.166010498687664265 ) ) ;
#45011 = CARTESIAN_POINT ( 'NONE',  ( -1.351706036745406347, 0.05413385826771626580, -0.4176697321401330321 ) ) ;
#45012 = CARTESIAN_POINT ( 'NONE',  ( -1.128608923884513837, 0.2306618581243847221, -0.2411417322834647770 ) ) ;
#45013 = CARTESIAN_POINT ( 'NONE',  ( 0.7217847769028878924, -0.3690944881889765550, -0.3153832671262227771 ) ) ;
#45014 = DIRECTION ( 'NONE',  ( -1.000000000000000000, -0.000000000000000000, -0.000000000000000000 ) ) ;
#45015 = CARTESIAN_POINT ( 'NONE',  ( -0.2099737532808391705, -0.6046776061558809534, -0.2411417322834644161 ) ) ;
#45016 = CARTESIAN_POINT ( 'NONE',  ( -0.1377952755905504645, -0.4536011799217368745, -0.2665933059059886201 ) ) ;
#45017 = LINE ( 'NONE', #77035, #23821 ) ;
#45018 = CARTESIAN_POINT ( 'NONE',  ( -0.2755905511811018171, 0.2952755905511811885, 0.000000000000000000 ) ) ;
#45019 = CARTESIAN_POINT ( 'NONE',  ( 0.1312335958005255154, -0.5023911411419708095, 0.1820866141732285504 ) ) ;
#45020 = CARTESIAN_POINT ( 'NONE',  ( 4.893765752498283308E-17, -0.3996062992125985480, -2.045275590551181466 ) ) ;
#45021 = CARTESIAN_POINT ( 'NONE',  ( 0.1181102362204730916, 0.2952755905511811885, 0.000000000000000000 ) ) ;
#45022 = CARTESIAN_POINT ( 'NONE',  ( 0.1049643490035303689, 0.3917322834645668994, -1.490794332512124010 ) ) ;
#45023 = CARTESIAN_POINT ( 'NONE',  ( 1.141732283464567788, -0.5511811023622047445, 6.969142054262312111E-17 ) ) ;
#45024 = CARTESIAN_POINT ( 'NONE',  ( 0.4843739873036773669, 1.677687439461655404E-16, 0.3627985898453510716 ) ) ;
#45025 = CARTESIAN_POINT ( 'NONE',  ( -0.9645669291338575535, -0.4536011799217367080, 0.2665933059059888421 ) ) ;
#45026 = EDGE_CURVE ( 'NONE', #69303, #49578, #26288, .T. ) ;
#45027 = CIRCLE ( 'NONE', #30269, 2.637795275590551380 ) ;
#45028 = CARTESIAN_POINT ( 'NONE',  ( -0.6824146981627291497, -0.5023911411419708095, -0.1820866141732282451 ) ) ;
#45029 = CARTESIAN_POINT ( 'NONE',  ( -0.5380577427821514602, 0.05413385826771666132, 0.4176697321401328100 ) ) ;
#45030 = CARTESIAN_POINT ( 'NONE',  ( -0.1706036745406816491, -0.4281496062992124485, 0.4176697321401328655 ) ) ;
#45031 = CARTESIAN_POINT ( 'NONE',  ( 0.6496062992125991586, -0.4536011799217368745, -0.2665933059059886201 ) ) ;
#45032 = CARTESIAN_POINT ( 'NONE',  ( 0.000000000000000000, 2.755905511811024056, 0.000000000000000000 ) ) ;
#45033 = CARTESIAN_POINT ( 'NONE',  ( 0.9645669291338588858, 0.07958543189024085140, 0.2665933059059887866 ) ) ;
#45034 = EDGE_CURVE ( 'NONE', #76998, #43965, #25879, .T. ) ;
#45035 = CARTESIAN_POINT ( 'NONE',  ( 0.8464566929133866546, -0.5400638737290844871, 0.3530559997133364547 ) ) ;
#45036 = CARTESIAN_POINT ( 'NONE',  ( 0.1070741851644053388, 0.3996062992125986035, -0.07020997375328083545 ) ) ;
#45037 = CARTESIAN_POINT ( 'NONE',  ( -0.3083989501312330295, -0.05778040916215522460, 0.4822834645669289988 ) ) ;
#45038 = CARTESIAN_POINT ( 'NONE',  ( -0.3392501089628017219, -0.1958661417322836718, -1.082020997375328086 ) ) ;
#45039 = CARTESIAN_POINT ( 'NONE',  ( 1.555118110236221041, -0.4536011799217367080, 0.2665933059059888421 ) ) ;
#45040 = CARTESIAN_POINT ( 'NONE',  ( 1.017060367454068803, -0.3162353388693405765, 0.4822834645669290543 ) ) ;
#45041 = CARTESIAN_POINT ( 'NONE',  ( -0.05905511811023545637, 0.1660481256975885056, 0.3530559997133364547 ) ) ;
#45042 = CARTESIAN_POINT ( 'NONE',  ( -1.586688153636163001, 2.388437996263389707, -0.1275903502784763444 ) ) ;
#45043 = CARTESIAN_POINT ( 'NONE',  ( 0.3543307086614181922, -0.5511811023622047445, 6.969142054262312111E-17 ) ) ;
#45044 = CARTESIAN_POINT ( 'NONE',  ( 0.9120734908136490793, 0.2952755905511810774, -0.1292274648535930714 ) ) ;
#45045 = CARTESIAN_POINT ( 'NONE',  ( -0.3477690288713905509, -0.5511811023622046335, 0.09757992244046803654 ) ) ;
#45046 = CARTESIAN_POINT ( 'NONE',  ( -0.9120734908136475250, -0.6692913385826773087, -0.1292274648535924053 ) ) ;
#45047 = CARTESIAN_POINT ( 'NONE',  ( -3.937007874015748143, 2.755905511811024056, -0.5314960629921260393 ) ) ;
#45048 = CARTESIAN_POINT ( 'NONE',  ( 0.4527559055118117182, -0.5400638737290844871, 0.3530559997133364547 ) ) ;
#45049 = CARTESIAN_POINT ( 'NONE',  ( -1.082677165354329896, -0.5400638737290845981, -0.3530559997133363437 ) ) ;
#45050 = CARTESIAN_POINT ( 'NONE',  ( -0.6430446194225716283, -0.3690944881889763329, 0.3153832671262228327 ) ) ;
#45051 = CARTESIAN_POINT ( 'NONE',  ( 0.4921259842519691285, 0.1660481256975885056, 0.3530559997133364547 ) ) ;
#45052 = CARTESIAN_POINT ( 'NONE',  ( -1.272965879265091305, -0.4281496062992124485, 0.4176697321401328655 ) ) ;
#45053 = CARTESIAN_POINT ( 'NONE',  ( -0.3280839895013117347, 0.05413385826771626580, -0.4176697321401330321 ) ) ;
#45054 = CARTESIAN_POINT ( 'NONE',  ( 1.135170603674541256, 0.2066929133858267931, 0.1054918080437490802 ) ) ;
#45056 = CARTESIAN_POINT ( 'NONE',  ( 1.358267716535433323, -0.5400638737290845981, -0.3530559997133363437 ) ) ;
#45055 = DIRECTION ( 'NONE',  ( 0.000000000000000000, -0.000000000000000000, 1.000000000000000000 ) ) ;
#45057 = CARTESIAN_POINT ( 'NONE',  ( 1.227034120734908917, 0.2952755905511810774, -0.1292274648535930714 ) ) ;
#45058 = CARTESIAN_POINT ( 'NONE',  ( 0.3917322834645670104, -0.1049643490035303273, -2.308398950131233640 ) ) ;
#45059 = CARTESIAN_POINT ( 'NONE',  ( -1.456692913385826182, 0.2952755905511811885, 0.000000000000000000 ) ) ;
#45060 = CARTESIAN_POINT ( 'NONE',  ( -1.030183727034119867, -0.05778040916215560624, -0.4822834645669293319 ) ) ;
#45061 = CARTESIAN_POINT ( 'NONE',  ( 0.1265901696524989462, 0.4724409448818897572, -0.6233595800524933672 ) ) ;
#45062 = CARTESIAN_POINT ( 'NONE',  ( 4.893765752498283924E-17, -0.3996062992125986035, 0.07874015748031494566 ) ) ;
#45063 = ORIENTED_EDGE ( 'NONE', *, *, #40694, .T. ) ;
#45064 = CARTESIAN_POINT ( 'NONE',  ( 0.1115485564304470323, 0.1771653543307087630, 0.09757992244046791164 ) ) ;
#45065 = CARTESIAN_POINT ( 'NONE',  ( 0.1049643490035304938, -0.3917322834645669549, -1.652230971128608505 ) ) ;
#45066 = ORIENTED_EDGE ( 'NONE', *, *, #27285, .F. ) ;
#45067 = CARTESIAN_POINT ( 'NONE',  ( 0.4265091863517067039, -0.6692913385826773087, -0.1292274648535924053 ) ) ;
#45068 = CARTESIAN_POINT ( 'NONE',  ( 0.4921259842519691285, 0.1660481256975885056, 0.3530559997133364547 ) ) ;
#45069 = CARTESIAN_POINT ( 'NONE',  ( 0.3458507752293908943, -0.3458507752293908943, -2.775590551181101429 ) ) ;
#45070 = LINE ( 'NONE', #33316, #41313 ) ;
#45071 = CARTESIAN_POINT ( 'NONE',  ( -0.4658792650918627265, -0.2845877964562161244, -0.3641732283464567121 ) ) ;
#45072 = CARTESIAN_POINT ( 'NONE',  ( -0.2379288306351265425, -0.1751536117528151026, 0.1496817530000226215 ) ) ;
#45073 = CARTESIAN_POINT ( 'NONE',  ( 0.8792650918635177559, 0.05413385826771666132, 0.4176697321401328100 ) ) ;
#45074 = CARTESIAN_POINT ( 'NONE',  ( 1.003937007874016185, 0.07958543189024071263, -0.2665933059059888421 ) ) ;
#45075 = CARTESIAN_POINT ( 'NONE',  ( -0.5774278215223089816, -0.6046776061558807314, 0.2411417322834647770 ) ) ;
#45076 = CARTESIAN_POINT ( 'NONE',  ( -0.3392501089628018329, -0.1958661417322836440, -1.077408505740470535 ) ) ;
#45077 = CARTESIAN_POINT ( 'NONE',  ( -0.6758530183727028406, 0.2952755905511811885, 0.1292274648535926551 ) ) ;
#45078 = CARTESIAN_POINT ( 'NONE',  ( -1.181102362204723644, -0.1870078740157480601, -0.3641732283464567677 ) ) ;
#45079 = CARTESIAN_POINT ( 'NONE',  ( -0.6496062992125976043, -0.5400638737290844871, 0.3530559997133364547 ) ) ;
#45080 = CARTESIAN_POINT ( 'NONE',  ( -0.4744094488188891900, 1.520194873416442993, -2.170146923806593797 ) ) ;
#45081 = ORIENTED_EDGE ( 'NONE', *, *, #17343, .F. ) ;
#45082 = CARTESIAN_POINT ( 'NONE',  ( -9.594673741351313045E-17, 0.3917322834645670659, -2.516423515256904331 ) ) ;
#45083 = CARTESIAN_POINT ( 'NONE',  ( -0.1640419947506553400, -0.05778040916215560624, -0.4822834645669293319 ) ) ;
#45084 = EDGE_LOOP ( 'NONE', ( #32706, #20699 ) ) ;
#45085 = CARTESIAN_POINT ( 'NONE',  ( -0.7086614173228339419, -0.1870078740157480879, -0.4822834645669291653 ) ) ;
#45086 = CARTESIAN_POINT ( 'NONE',  ( 1.345144356955381593, -0.3162353388693409650, -0.4822834645669289433 ) ) ;
#45087 = CARTESIAN_POINT ( 'NONE',  ( 1.338582677165355062, -0.1870078740157480879, -0.4822834645669291653 ) ) ;
#45088 = CARTESIAN_POINT ( 'NONE',  ( 0.6561679790026253567, 0.2306618581243848609, 0.2411417322834645549 ) ) ;
#45089 = CARTESIAN_POINT ( 'NONE',  ( 0.1246719160104994284, 0.2952755905511810774, -0.1292274648535930714 ) ) ;
#45090 = CARTESIAN_POINT ( 'NONE',  ( 0.1958661417322834775, 0.3392501089628018884, -1.488845144356955252 ) ) ;
#45091 = CARTESIAN_POINT ( 'NONE',  ( -1.404199475065615932, 0.05413385826771666132, 0.4176697321401328100 ) ) ;
#45092 = CARTESIAN_POINT ( 'NONE',  ( 0.01968503937007957949, -0.5400638737290845981, -0.3530559997133363437 ) ) ;
#45093 = CARTESIAN_POINT ( 'NONE',  ( 0.05249343832021075018, -0.5023911411419708095, 0.1820866141732285504 ) ) ;
#45094 = CARTESIAN_POINT ( 'NONE',  ( -0.2364516566766633465, -0.1768582946180018434, 5.689955017551601379 ) ) ;
#45095 = CARTESIAN_POINT ( 'NONE',  ( -0.2165354330708654795, -0.5400638737290845981, -0.3530559997133363437 ) ) ;
#45096 = CARTESIAN_POINT ( 'NONE',  ( 0.2887139107611556010, 0.1539470093639521697, -0.1968503937007875793 ) ) ;
#45097 = B_SPLINE_CURVE_WITH_KNOTS ( 'NONE', 3,
 ( #68476, #17960, #49924, #29745, #81528, #41961, #49097, #10814, #74801, #11230, #54589, #62149, #17552, #11648 ),
 .UNSPECIFIED., .F., .F.,
 ( 4, 2, 2, 2, 2, 2, 4 ),
 ( 0.000000000000000000, 0.0003923887041693346835, 0.0007847774083386693670, 0.001177166112508004105, 0.001569554816677338734, 0.002354332225016037266, 0.003139109633354736015 ),
 .UNSPECIFIED. ) ;
#45098 = CARTESIAN_POINT ( 'NONE',  ( 0.9317585301837276734, -0.4281496062992124485, 0.4176697321401328655 ) ) ;
#45099 = FACE_BOUND ( 'NONE', #54099, .T. ) ;
#45100 = VERTEX_POINT ( 'NONE', #59524 ) ;
#45101 = ORIENTED_EDGE ( 'NONE', *, *, #72340, .F. ) ;
#45102 = CARTESIAN_POINT ( 'NONE',  ( 0.2559055118110243332, 0.1660481256975885056, 0.3530559997133364547 ) ) ;
#45103 = CARTESIAN_POINT ( 'NONE',  ( -0.4724409448818890911, -0.1870078740157479769, 0.3641732283464567677 ) ) ;
#45105 = CARTESIAN_POINT ( 'NONE',  ( -0.1265901696524986964, -0.4724409448818899238, -0.3871391076115485719 ) ) ;
#45104 = CARTESIAN_POINT ( 'NONE',  ( 1.312335958005250269, -0.5023911411419708095, 0.1820866141732285504 ) ) ;
#45106 = CARTESIAN_POINT ( 'NONE',  ( -0.3917322834645671215, 0.1049643490035301469, -1.062335958005249603 ) ) ;
#45107 = CARTESIAN_POINT ( 'NONE',  ( -0.4724409448818899238, 0.1265901696524986686, -0.1095800524934383152 ) ) ;
#45108 = CARTESIAN_POINT ( 'NONE',  ( 1.397637795275591177, 0.07958543189024071263, -0.2665933059059888421 ) ) ;
#45109 = CARTESIAN_POINT ( 'NONE',  ( -1.489501312335957062, -0.05778040916215522460, 0.4822834645669289988 ) ) ;
#45110 = CARTESIAN_POINT ( 'NONE',  ( 0.3996062992125985480, 2.446882876249141654E-17, -2.714566929133858331 ) ) ;
#45111 = CARTESIAN_POINT ( 'NONE',  ( 0.1640419947506569498, -0.05778040916215522460, 0.4822834645669289988 ) ) ;
#45112 = CARTESIAN_POINT ( 'NONE',  ( -1.194225721784776262, -0.4281496062992124485, 0.4176697321401328655 ) ) ;
#45113 = CARTESIAN_POINT ( 'NONE',  ( 1.601049868766404982, 0.1283753931104748280, 0.1820866141732283561 ) ) ;
#45114 = CARTESIAN_POINT ( 'NONE',  ( 0.2624671916010504757, -0.6046776061558809534, -0.2411417322834644161 ) ) ;
#45115 = CARTESIAN_POINT ( 'NONE',  ( 4.837279021331061486E-17, -0.3949938075777409963, 0.001968503937007861845 ) ) ;
#45116 = CARTESIAN_POINT ( 'NONE',  ( 1.587926509186352586, -0.4281496062992127816, -0.4176697321401328100 ) ) ;
#45117 = CARTESIAN_POINT ( 'NONE',  ( 1.010498687664042716, 0.05413385826771626580, -0.4176697321401330321 ) ) ;
#45118 = CARTESIAN_POINT ( 'NONE',  ( 0.9448818897637802916, -0.1870078740157480601, -0.3641732283464567677 ) ) ;
#45119 = CARTESIAN_POINT ( 'NONE',  ( 0.8398950131233602345, 0.1539470093639521697, -0.1968503937007875793 ) ) ;
#45120 = CARTESIAN_POINT ( 'NONE',  ( 0.9317585301837276734, -0.004921259842519870586, -0.3153832671262229437 ) ) ;
#45121 = CARTESIAN_POINT ( 'NONE',  ( -1.161417322834644716, 0.1660481256975885056, 0.3530559997133364547 ) ) ;
#45122 = CARTESIAN_POINT ( 'NONE',  ( -0.3996062992125985480, -7.340648628747423112E-17, -0.7460629921259841479 ) ) ;
#45123 = CARTESIAN_POINT ( 'NONE',  ( 1.023622047244095334, -0.1870078740157479769, 0.4822834645669291653 ) ) ;
#45124 = CARTESIAN_POINT ( 'NONE',  ( -0.1958661417322836718, 0.3392501089628017219, -0.6351706036745405903 ) ) ;
#45125 = AXIS2_PLACEMENT_3D ( 'NONE', #18056, #25168, #62664 ) ;
#45126 = CIRCLE ( 'NONE', #78762, 1.889763779527559251 ) ;
#45128 = DIRECTION ( 'NONE',  ( 0.000000000000000000, 0.000000000000000000, 1.000000000000000000 ) ) ;
#45127 = CARTESIAN_POINT ( 'NONE',  ( 0.7677165354330716118, 0.1660481256975883668, -0.3530559997133364547 ) ) ;
#45129 = CARTESIAN_POINT ( 'NONE',  ( -1.614173228346457378, 1.055049524192299693, -0.1372047244094477536 ) ) ;
#45130 = CARTESIAN_POINT ( 'NONE',  ( -0.06561679790026180015, 0.05413385826771666132, 0.4176697321401328100 ) ) ;
#45131 = CARTESIAN_POINT ( 'NONE',  ( 0.6299212598425204535, -0.1870078740157479769, 0.3641732283464567677 ) ) ;
#45132 = EDGE_CURVE ( 'NONE', #73526, #81026, #53357, .T. ) ;
#45133 = CARTESIAN_POINT ( 'NONE',  ( 0.3543307086614181922, -0.6692913385826771977, 8.415575281601705876E-17 ) ) ;
#45134 = CARTESIAN_POINT ( 'NONE',  ( -0.4725026149319510593, 1.580736828574223596, 2.165487897237754034 ) ) ;
#45135 = CARTESIAN_POINT ( 'NONE',  ( -0.8202099737532801971, -0.5511811023622046335, 0.09757992244046803654 ) ) ;
#45136 = CARTESIAN_POINT ( 'NONE',  ( -0.6955380577427815458, -0.4281496062992127816, -0.4176697321401328100 ) ) ;
#45137 = CARTESIAN_POINT ( 'NONE',  ( 1.679790026246720025, 0.2306618581243848609, 0.2411417322834645549 ) ) ;
#45138 = CARTESIAN_POINT ( 'NONE',  ( -1.213910761154854745, 0.2952755905511810774, -0.1292274648535930714 ) ) ;
#45139 = CARTESIAN_POINT ( 'NONE',  ( 0.8727034120734913358, -0.05778040916215522460, 0.4822834645669289988 ) ) ;
#45140 = CARTESIAN_POINT ( 'NONE',  ( -1.391076115485563314, -0.5023911411419708095, -0.1820866141732282451 ) ) ;
#45141 = CARTESIAN_POINT ( 'NONE',  ( 1.102250182176885085, 1.111780926165008898, -0.2118791181513735022 ) ) ;
#45142 = CARTESIAN_POINT ( 'NONE',  ( 0.9711286089238851948, 0.2306618581243848609, 0.2411417322834645549 ) ) ;
#45143 = CARTESIAN_POINT ( 'NONE',  ( 0.4724409448818897572, -0.1265901696524988906, -2.550524934383202158 ) ) ;
#45144 = CIRCLE ( 'NONE', #16957, 0.2165354330708659791 ) ;
#45145 = CARTESIAN_POINT ( 'NONE',  ( -1.666666666666665853, 0.05413385826771626580, -0.4176697321401330321 ) ) ;
#45146 = CARTESIAN_POINT ( 'NONE',  ( -1.620734908136482577, 0.1771653543307087630, 0.09757992244046791164 ) ) ;
#45147 = CARTESIAN_POINT ( 'NONE',  ( -1.076115485564303809, 0.1283753931104748280, 0.1820866141732283561 ) ) ;
#45148 = CARTESIAN_POINT ( 'NONE',  ( 0.000000000000000000, 0.000000000000000000, -2.755905511811024056 ) ) ;
#45149 = CARTESIAN_POINT ( 'NONE',  ( -0.2624671916010490880, -0.6046776061558807314, 0.2411417322834647770 ) ) ;
#45150 = CARTESIAN_POINT ( 'NONE',  ( -0.2887139107611542133, -0.5023911411419708095, -0.1820866141732282451 ) ) ;
#45151 = CARTESIAN_POINT ( 'NONE',  ( -1.646981627296586703, -0.2845877964562161244, -0.3641732283464567121 ) ) ;
#45152 = CARTESIAN_POINT ( 'NONE',  ( 0.7939632545931766261, -0.08942795157527998196, 0.3641732283464567121 ) ) ;
#45153 = CARTESIAN_POINT ( 'NONE',  ( 0.5577427821522316087, -0.05778040916215522460, 0.4822834645669289988 ) ) ;
#45154 = CARTESIAN_POINT ( 'NONE',  ( 1.325459317585302665, 0.05413385826771626580, -0.4176697321401330321 ) ) ;
#45155 = CARTESIAN_POINT ( 'NONE',  ( 0.5577427821522316087, -0.05778040916215522460, 0.4822834645669289988 ) ) ;
#45156 = CARTESIAN_POINT ( 'NONE',  ( 0.7086614173228352742, -0.1870078740157480601, -0.3641732283464567677 ) ) ;
#45157 = CARTESIAN_POINT ( 'NONE',  ( -1.587926509186350810, 0.05413385826771626580, -0.4176697321401330321 ) ) ;
#45158 = CARTESIAN_POINT ( 'NONE',  ( -1.161417322834644716, 0.1660481256975885056, 0.3530559997133364547 ) ) ;
#45159 = CARTESIAN_POINT ( 'NONE',  ( -0.5511811023622041894, -0.1870078740157480879, -0.4822834645669291653 ) ) ;
#45160 = CARTESIAN_POINT ( 'NONE',  ( 0.2925321140481932369, -0.2925321140481931814, -0.2559055118110236116 ) ) ;
#45161 = CARTESIAN_POINT ( 'NONE',  ( 0.2362204724409449064, 0.4091458600556404646, -1.166010498687663821 ) ) ;
#45162 = CARTESIAN_POINT ( 'NONE',  ( -0.06561679790026180015, -0.4281496062992127816, -0.4176697321401328100 ) ) ;
#45163 = CARTESIAN_POINT ( 'NONE',  ( 1.148293963254593653, 0.1771653543307087075, -0.09757992244046823083 ) ) ;
#45164 = CARTESIAN_POINT ( 'NONE',  ( -0.2099737532808391705, 0.2306618581243848609, 0.2411417322834645549 ) ) ;
#45165 = CARTESIAN_POINT ( 'NONE',  ( 0.5643044619422579178, -0.4281496062992127816, -0.4176697321401328100 ) ) ;
#45166 = CARTESIAN_POINT ( 'NONE',  ( -0.1070741851644056997, 0.3996062992125986035, -2.368766404199475151 ) ) ;
#45167 = CARTESIAN_POINT ( 'NONE',  ( 0.1058382717557500713, -0.3949938075777409408, -1.817585301837270739 ) ) ;
#45168 = CARTESIAN_POINT ( 'NONE',  ( -0.1958661417322834220, -0.3392501089628018884, -0.3727034120734908362 ) ) ;
#45169 = CARTESIAN_POINT ( 'NONE',  ( -1.614173228346457378, 0.7794589730111968207, -0.1372047244094477536 ) ) ;
#45170 = CARTESIAN_POINT ( 'NONE',  ( -0.3917322834645669549, -0.1049643490035306603, -0.8254593175853016662 ) ) ;
#45171 = CARTESIAN_POINT ( 'NONE',  ( -0.9186351706036736120, 0.1283753931104748280, 0.1820866141732283561 ) ) ;
#45172 = CARTESIAN_POINT ( 'NONE',  ( -1.338582677165353729, -0.1870078740157480879, -0.4822834645669291653 ) ) ;
#45173 = CARTESIAN_POINT ( 'NONE',  ( -0.2891555358219909388, -0.2891555358219912164, -2.498031496062992574 ) ) ;
#45174 = CARTESIAN_POINT ( 'NONE',  ( 0.2755905511811031494, 0.2952755905511811885, 0.000000000000000000 ) ) ;
#45175 = CARTESIAN_POINT ( 'NONE',  ( 1.364829396325459854, -0.6046776061558809534, -0.2411417322834644161 ) ) ;
#45176 = CARTESIAN_POINT ( 'NONE',  ( 0.9186351706036751663, -0.6046776061558807314, 0.2411417322834647770 ) ) ;
#45177 = CARTESIAN_POINT ( 'NONE',  ( -0.3458507752293906723, -0.3458507752293910609, -2.893700787401574992 ) ) ;
#45178 = AXIS2_PLACEMENT_3D ( 'NONE', #46897, #59533, #47729 ) ;
#45179 = CARTESIAN_POINT ( 'NONE',  ( 4.893765752498283924E-17, -0.3996062992125986035, -2.440944881889763884 ) ) ;
#45180 = CARTESIAN_POINT ( 'NONE',  ( -0.1958661417322836995, 0.3392501089628017219, -0.7972634102700281167 ) ) ;
#45181 = DIRECTION ( 'NONE',  ( 1.000000000000000000, 0.000000000000000000, 0.000000000000000000 ) ) ;
#45182 = AXIS2_PLACEMENT_3D ( 'NONE', #49244, #55549, #36212 ) ;
#45183 = AXIS2_PLACEMENT_3D ( 'NONE', #62497, #4832, #31322 ) ;
#45184 = CARTESIAN_POINT ( 'NONE',  ( 0.5577427821522314977, -0.3162353388693409650, -0.4822834645669289433 ) ) ;
#45185 = CARTESIAN_POINT ( 'NONE',  ( 0.3346456692913390985, 0.1660481256975885056, 0.3530559997133364547 ) ) ;
#45186 = CARTESIAN_POINT ( 'NONE',  ( 0.6955380577427828781, -0.004921259842519870586, -0.3153832671262229437 ) ) ;
#45187 = CARTESIAN_POINT ( 'NONE',  ( 1.476377952755906442, -0.5400638737290844871, 0.3530559997133364547 ) ) ;
#45188 = CARTESIAN_POINT ( 'NONE',  ( 0.1958661417322834775, 0.3392501089628018884, -0.07152230971128617498 ) ) ;
#45189 = CARTESIAN_POINT ( 'NONE',  ( 0.3871391076115492380, -0.05778040916215560624, -0.4822834645669293319 ) ) ;
#45190 = CARTESIAN_POINT ( 'NONE',  ( 1.049868766404200349, 0.2306618581243848609, 0.2411417322834645549 ) ) ;
#45191 = CARTESIAN_POINT ( 'NONE',  ( 0.4527559055118117182, 0.1660481256975883668, -0.3530559997133364547 ) ) ;
#45192 = CARTESIAN_POINT ( 'NONE',  ( 1.043307086614173818, 0.07958543189024085140, 0.2665933059059887866 ) ) ;
#45193 = CARTESIAN_POINT ( 'NONE',  ( -0.8595800524934373854, -0.3162353388693409650, -0.4822834645669289433 ) ) ;
#45194 = CARTESIAN_POINT ( 'NONE',  ( -0.8989501312335946848, 0.2952755905511810774, -0.1292274648535930714 ) ) ;
#45195 = CARTESIAN_POINT ( 'NONE',  ( 1.161417322834646271, 0.1660481256975883668, -0.3530559997133364547 ) ) ;
#45196 = CARTESIAN_POINT ( 'NONE',  ( 0.3917322834645670104, 2.398668435337828261E-17, -0.6751968503937009203 ) ) ;
#45197 = CARTESIAN_POINT ( 'NONE',  ( -0.3917322834645670104, -7.196005306013484475E-17, -1.763779527559055094 ) ) ;
#45198 =( BOUNDED_SURFACE ( )  B_SPLINE_SURFACE ( 1, 2, ( 
 ( #54605, #10427, #36085, #3689, #29354, #55836, #75223, #30173, #74818, #81132, #15922, #80722, #41976, #42796, #61756, #17163, #4093, #36907, #79897, #68896, #62583, #22216, #67670, #67259, #29762, #60925, #36490, #47872, #23863, #73576, #48290, #68491, #9592, #55424, #10830, #55013, #10006, #62166, #3275, #81545, #80314, #22629, #16333, #35671, #61335, #49530, #23036, #48702, #70970, #76047, #50761, #69725, #5736, #31826, #76462, #25088, #6152, #24268, #83180, #63813, #18788, #31408, #69316, #12897, #24682, #63401, #57072, #12477, #50349, #75639, #17978, #45275, #57901, #18391, #82766, #64651, #57487, #44432, #11667, #70126, #43615, #25501, #37325, #44033, #38140, #77282, #19195, #51166, #6571, #76863, #44844, #5336, #70541, #19612, #62997, #37727, #38556, #64236, #32242, #267, #49941, #82363, #51580, #12070, #25922, #13315, #30994, #38968, #30593, #56259, #81955, #56662, #33083, #52418, #54402, #78127, #3488, #58750, #22015, #77708, #39815, #6989, #58324, #32657, #67466, #65075, #42190, #29154, #2666, #28741, #686, #66643, #26342, #79698, #47675, #73370, #61136, #1112, #41773, #26763, #60725, #28325, #41375, #80114, #9800, #71386, #53986, #54823, #7413, #8980, #80527, #52003, #34653, #67056, #60317, #20461, #20038, #71808, #73791, #46114, #13735, #3075, #22839, #48091, #9389, #15719, #35472, #48498, #74199, #35059, #22432, #14159, #16127, #16545, #45689, #39391, #82568, #81344, #24483, #11875, #69111, #23247, #18594, #18188, #81761, #75031, #49740, #37527, #24071, #11459, #56052, #29970, #10639, #43821, #75440, #62801, #68303, #10223, #74618, #55635, #50149, #75846, #31207, #29563, #23659, #43006, #48917, #69525, #5135, #16962, #4307, #42601, #36294, #17779, #63202, #5542, #61560, #43412, #3903, #37117, #61968, #56874, #49329, #17376, #68700, #30800, #56465, #11041, #36699, #62374, #24887, #50556, #55225, #4712, #76259, #30386, #67885, #35890, #82167, #80932, #482, #45064, #70767, #57283, #57700, #912, #71602, #45488, #82980, #78346, #77925, #58116, #51376, #26138, #13954, #51799, #71185, #32454, #6369, #70340, #20256, #77504, #39183, #44644, #69926, #50965, #32041, #26569, #52222, #7640, #5952, #62, #19413, #25299, #45905, #64867, #76662, #64029, #18995, #12695, #19839, #39612, #65301, #37938, #13527, #63615, #7206, #38354, #33310, #25716, #77080, #13117, #32877, #58546, #38769, #64446, #6782, #58972, #1328, #31621, #26977, #52642, #44237, #12282, #67373, #27816, #54304, #60218, #21502, #47160, #33717, #16034, #72442, #34552, #8056, #53476, #20677, #72023, #46330, #80016, #78766, #54727, #41680, #15200, #41277, #14379, #79186, #40037, #8876, #2568, #28227, #73694, #46749, #22334, #14791, #73271, #40859, #53886, #66963, #47995, #1737, #66543, #9707, #21090, #72852, #35378, #65723, #79600, #21916, #47577, #40448, #59379, #2149, #2980, #66127, #27393, #15620, #61042, #60629, #9296, #34966, #3393, #29056, #53054, #28645, #8464, #34133, #59795, #23560, #36198, #42093, #5039, #68204, #74934, #69010, #49231, #10942, #17279, #48818, #55126, #75335, #42907, #62277, #29468, #22742, #35791, #74517, #23975, #49643, #62700, #16448, #16865, #61868, #68602, #3806, #30286, #37019, #36599, #56371, #4614, #55952, #4209, #42502, #81665, #30708, #17682, #24383, #67789, #74102, #10126, #10541, #43312, #80836, #55535, #82070, #29873, #81244, #11361, #80432, #48402, #61458, #23149, #47848, #65986, #41546, #22192, #34830, #47434, #27670, #54579, #66399, #21772, #15478, #54160, #8737, #33990, #59652, #3667, #16308, #60075, #73127, #23012, #73554, #41134, #53337, #60489, #2008, #67235, #79046, #34407, #79874, #35649, #60900, #2839, #48265, #66825, #9157, #47018, #28502, #61311, #21364, #79453, #80291, #22605, #15898, #9566, #8324, #40714, #9981, #2430, #35236, #3252, #72711, #73962, #28914, #41952, #67646, #15058, #28087, #53744, #29330, #54991, #80699, #72303, #14649, #40306, #57922, #39835, #32677, #44863, #72247, #70990, #14177, #1541, #58768, #12918, #8269, #7855, #71406, #32261, #38575, #45710, #33102, #286, #77303, #25942, #46549, #27196, #70563, #19633, #14596 ),
 ( #64256, #40249, #52860, #45294, #58344, #57508, #7432, #26362, #6590, #20057, #51600, #52437, #13334, #38987, #65094, #20896, #46133, #13754, #33521, #705, #52022, #64670, #77728, #65932, #7009, #39411, #65524, #59184, #1131, #78147, #51186, #26781, #78570, #20479, #71827, #83199, #25521, #76885, #19215, #80239, #60846, #40661, #60020, #79398, #22555, #21717, #41082, #61259, #42309, #15421, #2787, #34777, #3198, #16253, #29279, #59599, #41900, #47796, #8684, #79822, #73500, #66771, #9104, #35596, #54943, #9925, #28862, #54524, #78989, #60436, #47381, #48217, #54106, #73913, #22138, #74323, #33934, #80649, #22962, #16670, #73072, #21309, #41497, #15004, #67594, #67182, #34354, #3613, #48628, #68007, #1954, #9512, #35185, #28447, #15848, #27616, #53279, #46962, #72654, #66346, #2375, #28032, #53690, #55762, #36419, #43954, #75564, #5257, #10759, #36012, #17086, #81469, #75972, #18312, #56995, #55351, #23786, #68825, #17904, #49864, #23373, #81883, #30100, #42723, #74738, #24194, #69650, #63325, #4024, #43541, #29688, #69240, #62092, #11994, #75152, #68419, #49041, #11588, #37248, #4433, #49457, #17497, #82692, #5663, #81057, #43127, #50684, #11171, #37648, #25011, #36832, #31330, #62923, #62505, #4843, #30518, #76382, #56180, #30921, #56587, #82288, #10352, #61683, #24606, #18716, #50274, #44357, #65429, #64572, #7331, #20796, #19534, #6076, #58243, #26265, #609, #39733, #12821, #20379, #38478, #39308, #6909, #19963, #32999, #46031, #51089, #32581, #33428, #70464, #45191, #7762, #70048, #70894, #45614, #13244, #44767, #12403, #51500, #52343, #6495, #76786, #64995, #59089, #26688, #71308, #51926, #71725, #14081, #1444, #38893, #27101, #78050, #64162, #52763, #77631, #57412, #78471, #188, #38060, #63737, #13655, #25424, #31750, #83105, #58669, #77205, #1034, #19118, #32165, #57821, #25841, #22459, #21621, #40987, #21210, #47281, #35497, #27518, #53594, #54428, #28765, #73394, #67081, #40154, #14906, #67491, #66247, #79722, #60749, #53174, #80138, #9006, #9413, #15745, #78889, #72559, #8585, #35083, #34257, #79303, #73816, #54849, #27936, #15322, #72971, #41399, #48118, #41800, #72145, #16153, #60341, #46865, #34678, #2689, #66667, #28349, #9827, #61162, #3513, #3101, #29182, #8171, #54010, #59918, #80553, #22039, #46452, #47699, #14501, #65838, #33836, #59503, #1856, #2273, #40566, #30414, #3930, #5163, #56082, #80959, #69137, #43851, #49767, #63230, #81787, #24098, #81371, #61995, #62402, #11902, #56492, #56902, #67912, #42216, #61585, #29998, #24511, #23274, #17402, #5570, #68327, #43032, #4332, #23684, #75467, #68727, #11068, #17806, #16571, #43440, #11489, #36726, #49358, #29589, #30827, #16987, #55661, #75055, #4741, #42630, #10248, #35919, #37556, #50178, #10665, #37143, #22865, #62828, #82194, #55252, #75873, #48943, #18216, #74645, #36320, #69554, #31235, #48526, #74226, #44672, #7558, #27736, #8798, #65219, #52559, #1252, #27316, #66050, #79108, #24915, #8387, #14299, #57309, #46251, #39960, #33229, #58892, #2070, #21427, #59715, #52975, #78689, #44264, #26900, #70367, #72366, #20599, #21012, #71947, #40777, #82596, #47081, #72772, #66462, #13872, #69955, #7976, #63642, #34052, #33640, #83007, #46672, #15123, #14714, #34474, #59302, #1659, #78268, #39531, #65646, #50583, #53401, #76290, #12309, #18621, #37966, #40369, #5980, #25328, #31651, #50992, #76690, #19024, #15958, #35298, #61377, #80352, #54642, #35707, #53806, #29390, #10043, #22665, #60960, #15540, #42421, #54222, #9627, #3310, #42013, #79938, #21834, #47497, #74857, #4132, #47911, #28975, #10866, #3726, #48324, #41199, #74021, #73189, #55050, #66887, #22253, #67707, #23483, #48739, #16367, #36119, #80757, #23071, #34890, #74436, #49150, #9217, #67294, #68121, #10466, #16783, #61792, #79519, #28566, #81167, #73616, #29797, #55458, #60551, #17199, #42832, #68525, #60140, #2902, #41605, #2491, #28150, #62202, #18823, #50384, #11283, #82398, #76082, #69351, #11705, #38175, #57525, #12514, #5774, #63438, #81584, #63032, #24306, #25125, #56699, #31443, #24716, #76900, #36527, #83216, #25537 ) ),
 .UNSPECIFIED., .F., .F., .F. ) 
 B_SPLINE_SURFACE_WITH_KNOTS ( ( 2, 2 ),
 ( 3, 2, 2, 2, 2, 2, 2, 2, 2, 2, 2, 2, 2, 2, 2, 2, 2, 2, 2, 2, 2, 2, 2, 2, 2, 2, 2, 2, 2, 2, 2, 2, 2, 2, 2, 2, 2, 2, 2, 2, 2, 2, 2, 2, 2, 2, 2, 2, 2, 2, 2, 2, 2, 2, 2, 2, 2, 2, 2, 2, 2, 2, 2, 2, 2, 2, 2, 2, 2, 2, 2, 2, 2, 2, 2, 2, 2, 2, 2, 2, 2, 2, 2, 2, 2, 2, 2, 2, 2, 2, 2, 2, 2, 2, 2, 2, 2, 2, 2, 2, 2, 2, 2, 2, 2, 2, 2, 2, 2, 2, 2, 2, 2, 2, 2, 2, 2, 2, 2, 2, 2, 2, 2, 2, 2, 2, 2, 2, 2, 2, 2, 2, 2, 2, 2, 2, 2, 2, 2, 2, 2, 2, 2, 2, 2, 2, 2, 2, 2, 2, 2, 2, 2, 2, 2, 2, 2, 2, 2, 2, 2, 2, 2, 2, 2, 2, 2, 2, 2, 2, 2, 2, 2, 2, 2, 2, 2, 2, 2, 2, 2, 2, 2, 2, 2, 2, 2, 2, 2, 2, 2, 2, 2, 2, 2, 2, 2, 2, 2, 2, 2, 2, 2, 2, 2, 2, 2, 2, 2, 2, 2, 2, 2, 2, 2, 2, 2, 2, 2, 2, 2, 2, 2, 2, 2, 2, 2, 2, 2, 2, 2, 2, 2, 2, 2, 2, 2, 2, 2, 2, 2, 2, 2, 2, 2, 2, 2, 2, 2, 2, 2, 2, 2, 2, 2, 3 ),
 ( 0.000000000000000000, 1.000000000000000000 ),
 ( 0.000000000000000000, 0.003787878787878787984, 0.007575757575757575968, 0.01136363636363636395, 0.01515151515151515194, 0.01893939393939393992, 0.02272727272727272790, 0.02651515151515151589, 0.03030303030303030387, 0.03409090909090908839, 0.03787878787878787984, 0.04166666666666666435, 0.04545454545454545581, 0.04924242424242424032, 0.05303030303030303177, 0.05681818181818181629, 0.06060606060606060774, 0.06439393939393939226, 0.06818181818181817677, 0.07196969696969697516, 0.07575757575757575968, 0.07954545454545454419, 0.08333333333333332871, 0.08712121212121212710, 0.09090909090909091161, 0.09469696969696969613, 0.09848484848484848064, 0.1022727272727272790, 0.1060606060606060635, 0.1098484848484848481, 0.1136363636363636326, 0.1174242424242424310, 0.1212121212121212155, 0.1250000000000000000, 0.1287878787878787845, 0.1325757575757575690, 0.1363636363636363535, 0.1401515151515151381, 0.1439393939393939503, 0.1477272727272727348, 0.1515151515151515194, 0.1553030303030303039, 0.1590909090909090884, 0.1628787878787878729, 0.1666666666666666574, 0.1704545454545454419, 0.1742424242424242542, 0.1780303030303030387, 0.1818181818181818232, 0.1856060606060606077, 0.1893939393939393923, 0.1931818181818181768, 0.1969696969696969613, 0.2007575757575757458, 0.2045454545454545581, 0.2083333333333333426, 0.2121212121212121271, 0.2159090909090909116, 0.2196969696969696961, 0.2234848484848484806, 0.2272727272727272652, 0.2310606060606060497, 0.2348484848484848619, 0.2386363636363636465, 0.2424242424242424310, 0.2462121212121212155, 0.2500000000000000000, 0.2537878787878787845, 0.2575757575757575690, 0.2613636363636363535, 0.2651515151515151381, 0.2689393939393939226, 0.2727272727272727071, 0.2765151515151514916, 0.2803030303030302761, 0.2840909090909091161, 0.2878787878787879007, 0.2916666666666666852, 0.2954545454545454697, 0.2992424242424242542, 0.3030303030303030387, 0.3068181818181818232, 0.3106060606060606077, 0.3143939393939393923, 0.3181818181818181768, 0.3219696969696969613, 0.3257575757575757458, 0.3295454545454545303, 0.3333333333333333148, 0.3371212121212120993, 0.3409090909090908839, 0.3446969696969697239, 0.3484848484848485084, 0.3522727272727272929, 0.3560606060606060774, 0.3598484848484848619, 0.3636363636363636465, 0.3674242424242424310, 0.3712121212121212155, 0.3750000000000000000, 0.3787878787878787845, 0.3825757575757575690, 0.3863636363636363535, 0.3901515151515151381, 0.3939393939393939226, 0.3977272727272727071, 0.4015151515151514916, 0.4053030303030302761, 0.4090909090909091161, 0.4128787878787879007, 0.4166666666666666852, 0.4204545454545454697, 0.4242424242424242542, 0.4280303030303030387, 0.4318181818181818232, 0.4356060606060606077, 0.4393939393939393923, 0.4431818181818181768, 0.4469696969696969613, 0.4507575757575757458, 0.4545454545454545303, 0.4583333333333333148, 0.4621212121212120993, 0.4659090909090908839, 0.4696969696969697239, 0.4734848484848485084, 0.4772727272727272929, 0.4810606060606060774, 0.4848484848484848619, 0.4886363636363636465, 0.4924242424242424310, 0.4962121212121212155, 0.5000000000000000000, 0.5037878787878787845, 0.5075757575757575690, 0.5113636363636363535, 0.5151515151515151381, 0.5189393939393939226, 0.5227272727272727071, 0.5265151515151514916, 0.5303030303030302761, 0.5340909090909090606, 0.5378787878787878451, 0.5416666666666666297, 0.5454545454545454142, 0.5492424242424241987, 0.5530303030303029832, 0.5568181818181817677, 0.5606060606060605522, 0.5643939393939394478, 0.5681818181818182323, 0.5719696969696970168, 0.5757575757575758013, 0.5795454545454545858, 0.5833333333333333703, 0.5871212121212121549, 0.5909090909090909394, 0.5946969696969697239, 0.5984848484848485084, 0.6022727272727272929, 0.6060606060606060774, 0.6098484848484848619, 0.6136363636363636465, 0.6174242424242424310, 0.6212121212121212155, 0.6250000000000000000, 0.6287878787878787845, 0.6325757575757575690, 0.6363636363636363535, 0.6401515151515151381, 0.6439393939393939226, 0.6477272727272727071, 0.6515151515151514916, 0.6553030303030302761, 0.6590909090909090606, 0.6628787878787878451, 0.6666666666666666297, 0.6704545454545454142, 0.6742424242424241987, 0.6780303030303029832, 0.6818181818181817677, 0.6856060606060605522, 0.6893939393939394478, 0.6931818181818182323, 0.6969696969696970168, 0.7007575757575758013, 0.7045454545454545858, 0.7083333333333333703, 0.7121212121212121549, 0.7159090909090909394, 0.7196969696969697239, 0.7234848484848485084, 0.7272727272727272929, 0.7310606060606060774, 0.7348484848484848619, 0.7386363636363636465, 0.7424242424242424310, 0.7462121212121212155, 0.7500000000000000000, 0.7537878787878787845, 0.7575757575757575690, 0.7613636363636363535, 0.7651515151515151381, 0.7689393939393939226, 0.7727272727272727071, 0.7765151515151514916, 0.7803030303030302761, 0.7840909090909090606, 0.7878787878787878451, 0.7916666666666666297, 0.7954545454545454142, 0.7992424242424241987, 0.8030303030303029832, 0.8068181818181817677, 0.8106060606060605522, 0.8143939393939394478, 0.8181818181818182323, 0.8219696969696970168, 0.8257575757575758013, 0.8295454545454545858, 0.8333333333333333703, 0.8371212121212121549, 0.8409090909090909394, 0.8446969696969697239, 0.8484848484848485084, 0.8522727272727272929, 0.8560606060606060774, 0.8598484848484848619, 0.8636363636363636465, 0.8674242424242424310, 0.8712121212121212155, 0.8750000000000000000, 0.8787878787878787845, 0.8825757575757575690, 0.8863636363636363535, 0.8901515151515151381, 0.8939393939393939226, 0.8977272727272727071, 0.9015151515151514916, 0.9053030303030302761, 0.9090909090909090606, 0.9128787878787878451, 0.9166666666666666297, 0.9204545454545454142, 0.9242424242424241987, 0.9280303030303029832, 0.9318181818181817677, 0.9356060606060605522, 0.9393939393939394478, 0.9431818181818182323, 0.9469696969696970168, 0.9507575757575758013, 0.9545454545454545858, 0.9583333333333333703, 0.9621212121212121549, 0.9659090909090909394 ),
 .UNSPECIFIED. ) 
 GEOMETRIC_REPRESENTATION_ITEM ( )  RATIONAL_B_SPLINE_SURFACE ( (
 ( 1.000000000000000000, 0.9659258262890683122, 1.000000000000000000, 0.9659258262890683122, 1.000000000000000000, 0.9659258262890683122, 1.000000000000000000, 0.9659258262890683122, 1.000000000000000000, 0.9659258262890683122, 1.000000000000000000, 0.9659258262890683122, 1.000000000000000000, 0.9659258262890683122, 1.000000000000000000, 0.9659258262890683122, 1.000000000000000000, 0.9659258262890683122, 1.000000000000000000, 0.9659258262890683122, 1.000000000000000000, 0.9659258262890683122, 1.000000000000000000, 0.9659258262890683122, 1.000000000000000000, 0.9659258262890683122, 1.000000000000000000, 0.9659258262890683122, 1.000000000000000000, 0.9659258262890683122, 1.000000000000000000, 0.9659258262890683122, 1.000000000000000000, 0.9659258262890683122, 1.000000000000000000, 0.9659258262890683122, 1.000000000000000000, 0.9659258262890683122, 1.000000000000000000, 0.9659258262890683122, 1.000000000000000000, 0.9659258262890683122, 1.000000000000000000, 0.9659258262890683122, 1.000000000000000000, 0.9659258262890683122, 1.000000000000000000, 0.9659258262890683122, 1.000000000000000000, 0.9659258262890683122, 1.000000000000000000, 0.9659258262890683122, 1.000000000000000000, 0.9659258262890683122, 1.000000000000000000, 0.9659258262890683122, 1.000000000000000000, 0.9659258262890683122, 1.000000000000000000, 0.9659258262890683122, 1.000000000000000000, 0.9659258262890683122, 1.000000000000000000, 0.9659258262890683122, 1.000000000000000000, 0.9659258262890683122, 1.000000000000000000, 0.9659258262890683122, 1.000000000000000000, 0.9659258262890683122, 1.000000000000000000, 0.9659258262890683122, 1.000000000000000000, 0.9659258262890683122, 1.000000000000000000, 0.9659258262890683122, 1.000000000000000000, 0.9659258262890683122, 1.000000000000000000, 0.9659258262890683122, 1.000000000000000000, 0.9659258262890683122, 1.000000000000000000, 0.9659258262890683122, 1.000000000000000000, 0.9659258262890683122, 1.000000000000000000, 0.9659258262890683122, 1.000000000000000000, 0.9659258262890683122, 1.000000000000000000, 0.9659258262890683122, 1.000000000000000000, 0.9659258262890683122, 1.000000000000000000, 0.9659258262890683122, 1.000000000000000000, 0.9659258262890683122, 1.000000000000000000, 0.9659258262890683122, 1.000000000000000000, 0.9659258262890683122, 1.000000000000000000, 0.9659258262890683122, 1.000000000000000000, 0.9659258262890683122, 1.000000000000000000, 0.9659258262890683122, 1.000000000000000000, 0.9659258262890683122, 1.000000000000000000, 0.9659258262890683122, 1.000000000000000000, 0.9659258262890683122, 1.000000000000000000, 0.9659258262890683122, 1.000000000000000000, 0.9659258262890683122, 1.000000000000000000, 0.9659258262890683122, 1.000000000000000000, 0.9659258262890683122, 1.000000000000000000, 0.9659258262890683122, 1.000000000000000000, 0.9659258262890683122, 1.000000000000000000, 0.9659258262890683122, 1.000000000000000000, 0.9659258262890683122, 1.000000000000000000, 0.9659258262890683122, 1.000000000000000000, 0.9659258262890683122, 1.000000000000000000, 0.9659258262890683122, 1.000000000000000000, 0.9659258262890683122, 1.000000000000000000, 0.9659258262890683122, 1.000000000000000000, 0.9659258262890683122, 1.000000000000000000, 0.9659258262890683122, 1.000000000000000000, 0.9659258262890683122, 1.000000000000000000, 0.9659258262890683122, 1.000000000000000000, 0.9659258262890683122, 1.000000000000000000, 0.9659258262890683122, 1.000000000000000000, 0.9659258262890683122, 1.000000000000000000, 0.9659258262890683122, 1.000000000000000000, 0.9659258262890683122, 1.000000000000000000, 0.9659258262890683122, 1.000000000000000000, 0.9659258262890683122, 1.000000000000000000, 0.9659258262890683122, 1.000000000000000000, 0.9659258262890683122, 1.000000000000000000, 0.9659258262890683122, 1.000000000000000000, 0.9659258262890683122, 1.000000000000000000, 0.9659258262890683122, 1.000000000000000000, 0.9659258262890683122, 1.000000000000000000, 0.9659258262890683122, 1.000000000000000000, 0.9659258262890683122, 1.000000000000000000, 0.9659258262890683122, 1.000000000000000000, 0.9659258262890683122, 1.000000000000000000, 0.9659258262890683122, 1.000000000000000000, 0.9659258262890683122, 1.000000000000000000, 0.9659258262890683122, 1.000000000000000000, 0.9659258262890683122, 1.000000000000000000, 0.9659258262890683122, 1.000000000000000000, 0.9659258262890683122, 1.000000000000000000, 0.9659258262890683122, 1.000000000000000000, 0.9659258262890683122, 1.000000000000000000, 0.9659258262890683122, 1.000000000000000000, 0.9659258262890683122, 1.000000000000000000, 0.9659258262890683122, 1.000000000000000000, 0.9659258262890683122, 1.000000000000000000, 0.9659258262890683122, 1.000000000000000000, 0.9659258262890683122, 1.000000000000000000, 0.9659258262890683122, 1.000000000000000000, 0.9659258262890683122, 1.000000000000000000, 0.9659258262890683122, 1.000000000000000000, 0.9659258262890683122, 1.000000000000000000, 0.9659258262890683122, 1.000000000000000000, 0.9659258262890683122, 1.000000000000000000, 0.9659258262890683122, 1.000000000000000000, 0.9659258262890683122, 1.000000000000000000, 0.9659258262890683122, 1.000000000000000000, 0.9659258262890683122, 1.000000000000000000, 0.9659258262890683122, 1.000000000000000000, 0.9659258262890683122, 1.000000000000000000, 0.9659258262890683122, 1.000000000000000000, 0.9659258262890683122, 1.000000000000000000, 0.9659258262890683122, 1.000000000000000000, 0.9659258262890683122, 1.000000000000000000, 0.9659258262890683122, 1.000000000000000000, 0.9659258262890683122, 1.000000000000000000, 0.9659258262890683122, 1.000000000000000000, 0.9659258262890683122, 1.000000000000000000, 0.9659258262890683122, 1.000000000000000000, 0.9659258262890683122, 1.000000000000000000, 0.9659258262890683122, 1.000000000000000000, 0.9659258262890683122, 1.000000000000000000, 0.9659258262890683122, 1.000000000000000000, 0.9659258262890683122, 1.000000000000000000, 0.9659258262890683122, 1.000000000000000000, 0.9659258262890683122, 1.000000000000000000, 0.9659258262890683122, 1.000000000000000000, 0.9659258262890683122, 1.000000000000000000, 0.9659258262890683122, 1.000000000000000000, 0.9659258262890683122, 1.000000000000000000, 0.9659258262890683122, 1.000000000000000000, 0.9659258262890683122, 1.000000000000000000, 0.9659258262890683122, 1.000000000000000000, 0.9659258262890683122, 1.000000000000000000, 0.9659258262890683122, 1.000000000000000000, 0.9659258262890683122, 1.000000000000000000, 0.9659258262890683122, 1.000000000000000000, 0.9659258262890683122, 1.000000000000000000, 0.9659258262890683122, 1.000000000000000000, 0.9659258262890683122, 1.000000000000000000, 0.9659258262890683122, 1.000000000000000000, 0.9659258262890683122, 1.000000000000000000, 0.9659258262890683122, 1.000000000000000000, 0.9659258262890683122, 1.000000000000000000, 0.9659258262890683122, 1.000000000000000000, 0.9659258262890683122, 1.000000000000000000, 0.9659258262890683122, 1.000000000000000000, 0.9659258262890683122, 1.000000000000000000, 0.9659258262890683122, 1.000000000000000000, 0.9659258262890683122, 1.000000000000000000, 0.9659258262890683122, 1.000000000000000000, 0.9659258262890683122, 1.000000000000000000, 0.9659258262890683122, 1.000000000000000000, 0.9659258262890683122, 1.000000000000000000, 0.9659258262890683122, 1.000000000000000000, 0.9659258262890683122, 1.000000000000000000, 0.9659258262890683122, 1.000000000000000000, 0.9659258262890683122, 1.000000000000000000, 0.9659258262890683122, 1.000000000000000000, 0.9659258262890683122, 1.000000000000000000, 0.9659258262890683122, 1.000000000000000000, 0.9659258262890683122, 1.000000000000000000, 0.9659258262890683122, 1.000000000000000000, 0.9659258262890683122, 1.000000000000000000, 0.9659258262890683122, 1.000000000000000000, 0.9659258262890683122, 1.000000000000000000, 0.9659258262890683122, 1.000000000000000000, 0.9659258262890683122, 1.000000000000000000, 0.9659258262890683122, 1.000000000000000000, 0.9659258262890683122, 1.000000000000000000, 0.9659258262890683122, 1.000000000000000000, 0.9659258262890683122, 1.000000000000000000, 0.9659258262890683122, 1.000000000000000000, 0.9659258262890683122, 1.000000000000000000, 0.9659258262890683122, 1.000000000000000000, 0.9659258262890683122, 1.000000000000000000, 0.9659258262890683122, 1.000000000000000000, 0.9659258262890683122, 1.000000000000000000, 0.9659258262890683122, 1.000000000000000000, 0.9659258262890683122, 1.000000000000000000, 0.9659258262890683122, 1.000000000000000000, 0.9659258262890683122, 1.000000000000000000, 0.9659258262890683122, 1.000000000000000000, 0.9659258262890683122, 1.000000000000000000, 0.9659258262890683122, 1.000000000000000000, 0.9659258262890683122, 1.000000000000000000, 0.9659258262890683122, 1.000000000000000000, 0.9659258262890683122, 1.000000000000000000, 0.9659258262890683122, 1.000000000000000000, 0.9659258262890683122, 1.000000000000000000, 0.9659258262890683122, 1.000000000000000000, 0.9659258262890683122, 1.000000000000000000, 0.9659258262890683122, 1.000000000000000000, 0.9659258262890683122, 1.000000000000000000, 0.9659258262890683122, 1.000000000000000000, 0.9659258262890683122, 1.000000000000000000, 0.9659258262890683122, 1.000000000000000000, 0.9659258262890683122, 1.000000000000000000, 0.9659258262890683122, 1.000000000000000000, 0.9659258262890683122, 1.000000000000000000, 0.9659258262890683122, 1.000000000000000000, 0.9659258262890683122, 1.000000000000000000, 0.9659258262890683122, 1.000000000000000000, 0.9659258262890683122, 1.000000000000000000, 0.9659258262890683122, 1.000000000000000000, 0.9659258262890683122, 1.000000000000000000, 0.9659258262890683122, 1.000000000000000000, 0.9659258262890683122, 1.000000000000000000, 0.9659258262890683122, 1.000000000000000000, 0.9659258262890683122, 1.000000000000000000, 0.9659258262890683122, 1.000000000000000000, 0.9659258262890683122, 1.000000000000000000, 0.9659258262890683122, 1.000000000000000000, 0.9659258262890683122, 1.000000000000000000, 0.9659258262890683122, 1.000000000000000000, 0.9659258262890683122, 1.000000000000000000, 0.9659258262890683122, 1.000000000000000000, 0.9659258262890683122, 1.000000000000000000, 0.9659258262890683122, 1.000000000000000000, 0.9659258262890683122, 1.000000000000000000, 0.9659258262890683122, 1.000000000000000000, 0.9659258262890683122, 1.000000000000000000, 0.9659258262890683122, 1.000000000000000000, 0.9659258262890683122, 1.000000000000000000, 0.9659258262890683122, 1.000000000000000000, 0.9659258262890683122, 1.000000000000000000, 0.9659258262890683122, 1.000000000000000000, 0.9659258262890683122, 1.000000000000000000, 0.9659258262890683122, 1.000000000000000000, 0.9659258262890683122, 1.000000000000000000, 0.9659258262890683122, 1.000000000000000000, 0.9659258262890683122, 1.000000000000000000, 0.9659258262890683122, 1.000000000000000000, 0.9659258262890683122, 1.000000000000000000, 0.9659258262890683122, 1.000000000000000000, 0.9659258262890683122, 1.000000000000000000, 0.9659258262890683122, 1.000000000000000000, 0.9659258262890683122, 1.000000000000000000, 0.9659258262890683122, 1.000000000000000000, 0.9659258262890683122, 1.000000000000000000, 0.9659258262890683122, 1.000000000000000000, 0.9659258262890683122, 1.000000000000000000, 0.9659258262890683122, 1.000000000000000000, 0.9659258262890683122, 1.000000000000000000, 0.9659258262890683122, 1.000000000000000000, 0.9659258262890683122, 1.000000000000000000, 0.9659258262890683122, 1.000000000000000000, 0.9659258262890683122, 1.000000000000000000),
 ( 1.000000000000000000, 0.9659258262890683122, 1.000000000000000000, 0.9659258262890683122, 1.000000000000000000, 0.9659258262890683122, 1.000000000000000000, 0.9659258262890683122, 1.000000000000000000, 0.9659258262890683122, 1.000000000000000000, 0.9659258262890683122, 1.000000000000000000, 0.9659258262890683122, 1.000000000000000000, 0.9659258262890683122, 1.000000000000000000, 0.9659258262890683122, 1.000000000000000000, 0.9659258262890683122, 1.000000000000000000, 0.9659258262890683122, 1.000000000000000000, 0.9659258262890683122, 1.000000000000000000, 0.9659258262890683122, 1.000000000000000000, 0.9659258262890683122, 1.000000000000000000, 0.9659258262890683122, 1.000000000000000000, 0.9659258262890683122, 1.000000000000000000, 0.9659258262890683122, 1.000000000000000000, 0.9659258262890683122, 1.000000000000000000, 0.9659258262890683122, 1.000000000000000000, 0.9659258262890683122, 1.000000000000000000, 0.9659258262890683122, 1.000000000000000000, 0.9659258262890683122, 1.000000000000000000, 0.9659258262890683122, 1.000000000000000000, 0.9659258262890683122, 1.000000000000000000, 0.9659258262890683122, 1.000000000000000000, 0.9659258262890683122, 1.000000000000000000, 0.9659258262890683122, 1.000000000000000000, 0.9659258262890683122, 1.000000000000000000, 0.9659258262890683122, 1.000000000000000000, 0.9659258262890683122, 1.000000000000000000, 0.9659258262890683122, 1.000000000000000000, 0.9659258262890683122, 1.000000000000000000, 0.9659258262890683122, 1.000000000000000000, 0.9659258262890683122, 1.000000000000000000, 0.9659258262890683122, 1.000000000000000000, 0.9659258262890683122, 1.000000000000000000, 0.9659258262890683122, 1.000000000000000000, 0.9659258262890683122, 1.000000000000000000, 0.9659258262890683122, 1.000000000000000000, 0.9659258262890683122, 1.000000000000000000, 0.9659258262890683122, 1.000000000000000000, 0.9659258262890683122, 1.000000000000000000, 0.9659258262890683122, 1.000000000000000000, 0.9659258262890683122, 1.000000000000000000, 0.9659258262890683122, 1.000000000000000000, 0.9659258262890683122, 1.000000000000000000, 0.9659258262890683122, 1.000000000000000000, 0.9659258262890683122, 1.000000000000000000, 0.9659258262890683122, 1.000000000000000000, 0.9659258262890683122, 1.000000000000000000, 0.9659258262890683122, 1.000000000000000000, 0.9659258262890683122, 1.000000000000000000, 0.9659258262890683122, 1.000000000000000000, 0.9659258262890683122, 1.000000000000000000, 0.9659258262890683122, 1.000000000000000000, 0.9659258262890683122, 1.000000000000000000, 0.9659258262890683122, 1.000000000000000000, 0.9659258262890683122, 1.000000000000000000, 0.9659258262890683122, 1.000000000000000000, 0.9659258262890683122, 1.000000000000000000, 0.9659258262890683122, 1.000000000000000000, 0.9659258262890683122, 1.000000000000000000, 0.9659258262890683122, 1.000000000000000000, 0.9659258262890683122, 1.000000000000000000, 0.9659258262890683122, 1.000000000000000000, 0.9659258262890683122, 1.000000000000000000, 0.9659258262890683122, 1.000000000000000000, 0.9659258262890683122, 1.000000000000000000, 0.9659258262890683122, 1.000000000000000000, 0.9659258262890683122, 1.000000000000000000, 0.9659258262890683122, 1.000000000000000000, 0.9659258262890683122, 1.000000000000000000, 0.9659258262890683122, 1.000000000000000000, 0.9659258262890683122, 1.000000000000000000, 0.9659258262890683122, 1.000000000000000000, 0.9659258262890683122, 1.000000000000000000, 0.9659258262890683122, 1.000000000000000000, 0.9659258262890683122, 1.000000000000000000, 0.9659258262890683122, 1.000000000000000000, 0.9659258262890683122, 1.000000000000000000, 0.9659258262890683122, 1.000000000000000000, 0.9659258262890683122, 1.000000000000000000, 0.9659258262890683122, 1.000000000000000000, 0.9659258262890683122, 1.000000000000000000, 0.9659258262890683122, 1.000000000000000000, 0.9659258262890683122, 1.000000000000000000, 0.9659258262890683122, 1.000000000000000000, 0.9659258262890683122, 1.000000000000000000, 0.9659258262890683122, 1.000000000000000000, 0.9659258262890683122, 1.000000000000000000, 0.9659258262890683122, 1.000000000000000000, 0.9659258262890683122, 1.000000000000000000, 0.9659258262890683122, 1.000000000000000000, 0.9659258262890683122, 1.000000000000000000, 0.9659258262890683122, 1.000000000000000000, 0.9659258262890683122, 1.000000000000000000, 0.9659258262890683122, 1.000000000000000000, 0.9659258262890683122, 1.000000000000000000, 0.9659258262890683122, 1.000000000000000000, 0.9659258262890683122, 1.000000000000000000, 0.9659258262890683122, 1.000000000000000000, 0.9659258262890683122, 1.000000000000000000, 0.9659258262890683122, 1.000000000000000000, 0.9659258262890683122, 1.000000000000000000, 0.9659258262890683122, 1.000000000000000000, 0.9659258262890683122, 1.000000000000000000, 0.9659258262890683122, 1.000000000000000000, 0.9659258262890683122, 1.000000000000000000, 0.9659258262890683122, 1.000000000000000000, 0.9659258262890683122, 1.000000000000000000, 0.9659258262890683122, 1.000000000000000000, 0.9659258262890683122, 1.000000000000000000, 0.9659258262890683122, 1.000000000000000000, 0.9659258262890683122, 1.000000000000000000, 0.9659258262890683122, 1.000000000000000000, 0.9659258262890683122, 1.000000000000000000, 0.9659258262890683122, 1.000000000000000000, 0.9659258262890683122, 1.000000000000000000, 0.9659258262890683122, 1.000000000000000000, 0.9659258262890683122, 1.000000000000000000, 0.9659258262890683122, 1.000000000000000000, 0.9659258262890683122, 1.000000000000000000, 0.9659258262890683122, 1.000000000000000000, 0.9659258262890683122, 1.000000000000000000, 0.9659258262890683122, 1.000000000000000000, 0.9659258262890683122, 1.000000000000000000, 0.9659258262890683122, 1.000000000000000000, 0.9659258262890683122, 1.000000000000000000, 0.9659258262890683122, 1.000000000000000000, 0.9659258262890683122, 1.000000000000000000, 0.9659258262890683122, 1.000000000000000000, 0.9659258262890683122, 1.000000000000000000, 0.9659258262890683122, 1.000000000000000000, 0.9659258262890683122, 1.000000000000000000, 0.9659258262890683122, 1.000000000000000000, 0.9659258262890683122, 1.000000000000000000, 0.9659258262890683122, 1.000000000000000000, 0.9659258262890683122, 1.000000000000000000, 0.9659258262890683122, 1.000000000000000000, 0.9659258262890683122, 1.000000000000000000, 0.9659258262890683122, 1.000000000000000000, 0.9659258262890683122, 1.000000000000000000, 0.9659258262890683122, 1.000000000000000000, 0.9659258262890683122, 1.000000000000000000, 0.9659258262890683122, 1.000000000000000000, 0.9659258262890683122, 1.000000000000000000, 0.9659258262890683122, 1.000000000000000000, 0.9659258262890683122, 1.000000000000000000, 0.9659258262890683122, 1.000000000000000000, 0.9659258262890683122, 1.000000000000000000, 0.9659258262890683122, 1.000000000000000000, 0.9659258262890683122, 1.000000000000000000, 0.9659258262890683122, 1.000000000000000000, 0.9659258262890683122, 1.000000000000000000, 0.9659258262890683122, 1.000000000000000000, 0.9659258262890683122, 1.000000000000000000, 0.9659258262890683122, 1.000000000000000000, 0.9659258262890683122, 1.000000000000000000, 0.9659258262890683122, 1.000000000000000000, 0.9659258262890683122, 1.000000000000000000, 0.9659258262890683122, 1.000000000000000000, 0.9659258262890683122, 1.000000000000000000, 0.9659258262890683122, 1.000000000000000000, 0.9659258262890683122, 1.000000000000000000, 0.9659258262890683122, 1.000000000000000000, 0.9659258262890683122, 1.000000000000000000, 0.9659258262890683122, 1.000000000000000000, 0.9659258262890683122, 1.000000000000000000, 0.9659258262890683122, 1.000000000000000000, 0.9659258262890683122, 1.000000000000000000, 0.9659258262890683122, 1.000000000000000000, 0.9659258262890683122, 1.000000000000000000, 0.9659258262890683122, 1.000000000000000000, 0.9659258262890683122, 1.000000000000000000, 0.9659258262890683122, 1.000000000000000000, 0.9659258262890683122, 1.000000000000000000, 0.9659258262890683122, 1.000000000000000000, 0.9659258262890683122, 1.000000000000000000, 0.9659258262890683122, 1.000000000000000000, 0.9659258262890683122, 1.000000000000000000, 0.9659258262890683122, 1.000000000000000000, 0.9659258262890683122, 1.000000000000000000, 0.9659258262890683122, 1.000000000000000000, 0.9659258262890683122, 1.000000000000000000, 0.9659258262890683122, 1.000000000000000000, 0.9659258262890683122, 1.000000000000000000, 0.9659258262890683122, 1.000000000000000000, 0.9659258262890683122, 1.000000000000000000, 0.9659258262890683122, 1.000000000000000000, 0.9659258262890683122, 1.000000000000000000, 0.9659258262890683122, 1.000000000000000000, 0.9659258262890683122, 1.000000000000000000, 0.9659258262890683122, 1.000000000000000000, 0.9659258262890683122, 1.000000000000000000, 0.9659258262890683122, 1.000000000000000000, 0.9659258262890683122, 1.000000000000000000, 0.9659258262890683122, 1.000000000000000000, 0.9659258262890683122, 1.000000000000000000, 0.9659258262890683122, 1.000000000000000000, 0.9659258262890683122, 1.000000000000000000, 0.9659258262890683122, 1.000000000000000000, 0.9659258262890683122, 1.000000000000000000, 0.9659258262890683122, 1.000000000000000000, 0.9659258262890683122, 1.000000000000000000, 0.9659258262890683122, 1.000000000000000000, 0.9659258262890683122, 1.000000000000000000, 0.9659258262890683122, 1.000000000000000000, 0.9659258262890683122, 1.000000000000000000, 0.9659258262890683122, 1.000000000000000000, 0.9659258262890683122, 1.000000000000000000, 0.9659258262890683122, 1.000000000000000000, 0.9659258262890683122, 1.000000000000000000, 0.9659258262890683122, 1.000000000000000000, 0.9659258262890683122, 1.000000000000000000, 0.9659258262890683122, 1.000000000000000000, 0.9659258262890683122, 1.000000000000000000, 0.9659258262890683122, 1.000000000000000000, 0.9659258262890683122, 1.000000000000000000, 0.9659258262890683122, 1.000000000000000000, 0.9659258262890683122, 1.000000000000000000, 0.9659258262890683122, 1.000000000000000000, 0.9659258262890683122, 1.000000000000000000, 0.9659258262890683122, 1.000000000000000000, 0.9659258262890683122, 1.000000000000000000, 0.9659258262890683122, 1.000000000000000000, 0.9659258262890683122, 1.000000000000000000, 0.9659258262890683122, 1.000000000000000000, 0.9659258262890683122, 1.000000000000000000, 0.9659258262890683122, 1.000000000000000000, 0.9659258262890683122, 1.000000000000000000, 0.9659258262890683122, 1.000000000000000000, 0.9659258262890683122, 1.000000000000000000, 0.9659258262890683122, 1.000000000000000000, 0.9659258262890683122, 1.000000000000000000, 0.9659258262890683122, 1.000000000000000000, 0.9659258262890683122, 1.000000000000000000, 0.9659258262890683122, 1.000000000000000000, 0.9659258262890683122, 1.000000000000000000, 0.9659258262890683122, 1.000000000000000000, 0.9659258262890683122, 1.000000000000000000, 0.9659258262890683122, 1.000000000000000000, 0.9659258262890683122, 1.000000000000000000, 0.9659258262890683122, 1.000000000000000000, 0.9659258262890683122, 1.000000000000000000, 0.9659258262890683122, 1.000000000000000000, 0.9659258262890683122, 1.000000000000000000, 0.9659258262890683122, 1.000000000000000000, 0.9659258262890683122, 1.000000000000000000, 0.9659258262890683122, 1.000000000000000000, 0.9659258262890683122, 1.000000000000000000, 0.9659258262890683122, 1.000000000000000000, 0.9659258262890683122, 1.000000000000000000, 0.9659258262890683122, 1.000000000000000000, 0.9659258262890683122, 1.000000000000000000, 0.9659258262890683122, 1.000000000000000000) ) ) 
 REPRESENTATION_ITEM ( '' )  SURFACE ( )  );
#45199 = CARTESIAN_POINT ( 'NONE',  ( -0.3917322834645669549, -0.1049643490035306603, -2.557742782152230721 ) ) ;
#45200 = ORIENTED_EDGE ( 'NONE', *, *, #61964, .T. ) ;
#45201 = CARTESIAN_POINT ( 'NONE',  ( 0.3996062992125986035, 2.446882876249141962E-17, 0.03937007874015746589 ) ) ;
#45202 = ORIENTED_EDGE ( 'NONE', *, *, #77795, .F. ) ;
#45203 = CARTESIAN_POINT ( 'NONE',  ( 1.364829396325460076, 0.2306618581243848609, 0.2411417322834645549 ) ) ;
#45204 = VECTOR ( 'NONE', #11204, 39.37007874015748143 ) ;
#45205 = CARTESIAN_POINT ( 'NONE',  ( 1.036745406824147508, -0.3690944881889765550, -0.3153832671262227771 ) ) ;
#45206 = CARTESIAN_POINT ( 'NONE',  ( -0.3996062992125986035, -7.340648628747425578E-17, -1.456692913385826849 ) ) ;
#45207 = CARTESIAN_POINT ( 'NONE',  ( 1.502624671916010790, -0.08942795157527998196, 0.3641732283464567121 ) ) ;
#45208 = CARTESIAN_POINT ( 'NONE',  ( -0.1265901696524993347, 0.4724409448818896462, -2.445538057742782101 ) ) ;
#45209 = CARTESIAN_POINT ( 'NONE',  ( -0.4744094488189058989, 1.537401574803149984, 2.554262525012261253 ) ) ;
#45210 = CARTESIAN_POINT ( 'NONE',  ( 0.3948371832379764523, 0.006307039255732700168, -1.929133858267718882 ) ) ;
#45211 = CARTESIAN_POINT ( 'NONE',  ( 0.3917322834645670104, -0.1049643490035303411, -0.8261154855643043637 ) ) ;
#45212 = CARTESIAN_POINT ( 'NONE',  ( -1.174540682414697335, -0.08942795157527998196, 0.3641732283464567121 ) ) ;
#45213 = CARTESIAN_POINT ( 'NONE',  ( -1.594488188976377563, -0.4536011799217367080, 0.2665933059059888421 ) ) ;
#45214 = CARTESIAN_POINT ( 'NONE',  ( -1.141732283464566011, 0.2952755905511811885, 0.000000000000000000 ) ) ;
#45215 = CARTESIAN_POINT ( 'NONE',  ( 0.1902887139107617975, 0.2952755905511811885, 0.1292274648535926551 ) ) ;
#45216 = CARTESIAN_POINT ( 'NONE',  ( 1.417322834645670104, -0.1870078740157479769, 0.4822834645669291653 ) ) ;
#45217 = ORIENTED_EDGE ( 'NONE', *, *, #19165, .F. ) ;
#45218 = CARTESIAN_POINT ( 'NONE',  ( -1.030590969126516265, 1.368909816122638512, -0.4437501211348749419 ) ) ;
#45219 = CARTESIAN_POINT ( 'NONE',  ( 3.523619145740923830, 2.378928776101099540, 5.973313079581529017 ) ) ;
#45220 = CARTESIAN_POINT ( 'NONE',  ( 0.2362204724409451007, -0.4091458600556402980, -2.139107611548556331 ) ) ;
#45221 = CARTESIAN_POINT ( 'NONE',  ( -0.4724409448818917001, 0.1265901696524956710, -2.709973753280840558 ) ) ;
#45222 = DIRECTION ( 'NONE',  ( 0.000000000000000000, 0.000000000000000000, -1.000000000000000000 ) ) ;
#45223 = CARTESIAN_POINT ( 'NONE',  ( -0.7545931758530176614, -0.5511811023622048555, -0.09757992244046775898 ) ) ;
#45224 = EDGE_CURVE ( 'NONE', #35196, #35306, #42516, .T. ) ;
#45225 = CARTESIAN_POINT ( 'NONE',  ( -0.9908136482939626788, 0.2952755905511811885, 0.1292274648535926551 ) ) ;
#45226 = CARTESIAN_POINT ( 'NONE',  ( 0.6955380577427828781, -0.4281496062992124485, 0.4176697321401328655 ) ) ;
#45227 = EDGE_LOOP ( 'NONE', ( #71520, #42504, #59925, #70997 ) ) ;
#45229 = CARTESIAN_POINT ( 'NONE',  ( -0.2362204724409447953, -0.4091458600556404646, -2.662073490813648746 ) ) ;
#45228 = DIRECTION ( 'NONE',  ( 0.000000000000000000, -1.000000000000000000, 0.000000000000000000 ) ) ;
#45230 = CARTESIAN_POINT ( 'NONE',  ( 1.062992125984252745, 0.2952755905511811885, 0.000000000000000000 ) ) ;
#45231 = CARTESIAN_POINT ( 'NONE',  ( 1.541994750656168645, -0.5511811023622046335, 0.09757992244046803654 ) ) ;
#45232 = CARTESIAN_POINT ( 'NONE',  ( 0.3917322834645668994, 0.1049643490035304522, -0.6771460385488696776 ) ) ;
#45233 = EDGE_CURVE ( 'NONE', #80562, #79831, #57364, .T. ) ;
#45234 = CARTESIAN_POINT ( 'NONE',  ( -0.3412073490813641308, -0.5023911411419708095, 0.1820866141732285504 ) ) ;
#45235 = CARTESIAN_POINT ( 'NONE',  ( -1.279527559055116948, 0.07958543189024071263, -0.2665933059059888421 ) ) ;
#45236 = LINE ( 'NONE', #38933, #46522 ) ;
#45237 = CARTESIAN_POINT ( 'NONE',  ( -0.4068241469816264999, -0.3690944881889763329, 0.3153832671262228327 ) ) ;
#45238 = CARTESIAN_POINT ( 'NONE',  ( 0.3018372703412079971, -0.3690944881889763329, 0.3153832671262228327 ) ) ;
#45239 = CARTESIAN_POINT ( 'NONE',  ( 0.006561679790026889343, -0.05778040916215522460, 0.4822834645669289988 ) ) ;
#45240 = CARTESIAN_POINT ( 'NONE',  ( -1.102362204724408601, -0.1870078740157480601, -0.3641732283464567677 ) ) ;
#45241 = CARTESIAN_POINT ( 'NONE',  ( 0.1958661417322836440, -0.3392501089628017219, -2.761154855643044304 ) ) ;
#45242 = CARTESIAN_POINT ( 'NONE',  ( 1.102362204724410155, -0.1870078740157479769, 0.4822834645669291653 ) ) ;
#45243 = VECTOR ( 'NONE', #61618, 39.37007874015748143 ) ;
#45244 = CARTESIAN_POINT ( 'NONE',  ( -1.568241469816272105, -0.3162353388693409650, -0.4822834645669289433 ) ) ;
#45245 = PRESENTATION_LAYER_ASSIGNMENT (  '', '', ( #72196 ) ) ;
#45246 = CARTESIAN_POINT ( 'NONE',  ( 0.4091458600556404646, -0.2362204724409448231, -1.284120734908136496 ) ) ;
#45247 = AXIS2_PLACEMENT_3D ( 'NONE', #47508, #28985, #53816 ) ;
#45248 = CARTESIAN_POINT ( 'NONE',  ( -0.4133858267716528645, 0.1660481256975883668, -0.3530559997133364547 ) ) ;
#45249 = CARTESIAN_POINT ( 'NONE',  ( -1.076115485564303809, -0.6046776061558809534, -0.2411417322834644161 ) ) ;
#45250 = CARTESIAN_POINT ( 'NONE',  ( 0.9383202099737538715, -0.08942795157528024563, -0.3641732283464568787 ) ) ;
#45251 = CARTESIAN_POINT ( 'NONE',  ( -0.3346456692913377662, -0.4536011799217367080, 0.2665933059059888421 ) ) ;
#45252 = CARTESIAN_POINT ( 'NONE',  ( -0.7020997375328076329, -0.3162353388693409650, -0.4822834645669289433 ) ) ;
#45253 = CARTESIAN_POINT ( 'NONE',  ( -1.633858267716534529, 0.1660481256975885056, 0.3530559997133364547 ) ) ;
#45254 = PLANE ( 'NONE',  #53318 ) ;
#45255 = CARTESIAN_POINT ( 'NONE',  ( 1.391076115485564868, 0.1283753931104746893, -0.1820866141732285504 ) ) ;
#45256 = PRODUCT_DEFINITION_SHAPE ( 'NONE', 'NONE',  #83310 ) ;
#45257 = CARTESIAN_POINT ( 'NONE',  ( -1.541994750656167090, -0.6692913385826773087, -0.1292274648535924053 ) ) ;
#45258 = CARTESIAN_POINT ( 'NONE',  ( -1.423884514435694859, -0.3162353388693405765, 0.4822834645669290543 ) ) ;
#45259 = VERTEX_POINT ( 'NONE', #78496 ) ;
#45260 = CARTESIAN_POINT ( 'NONE',  ( -0.1998031496062994405, 0.3460692066303957537, -2.294619422572178102 ) ) ;
#45261 = CARTESIAN_POINT ( 'NONE',  ( -1.010498687664041384, -0.004921259842519576551, 0.3153832671262227771 ) ) ;
#45262 = CARTESIAN_POINT ( 'NONE',  ( 0.6824146981627303710, 0.2306618581243847221, -0.2411417322834647770 ) ) ;
#45263 = CARTESIAN_POINT ( 'NONE',  ( -1.062992125984250968, 0.1771653543307087630, 0.000000000000000000 ) ) ;
#45264 = CARTESIAN_POINT ( 'NONE',  ( 0.1998031496062994128, -0.3460692066303957537, -1.270997375328084100 ) ) ;
#45265 = CARTESIAN_POINT ( 'NONE',  ( -1.082677165354329896, 0.1660481256975885056, 0.3530559997133364547 ) ) ;
#45266 = CARTESIAN_POINT ( 'NONE',  ( 0.7086614173228353852, -0.1870078740157479769, 0.4822834645669291653 ) ) ;
#45267 = CARTESIAN_POINT ( 'NONE',  ( 0.4986876640419954376, -0.6046776061558809534, -0.2411417322834644161 ) ) ;
#45268 = CARTESIAN_POINT ( 'NONE',  ( 1.410761154855643795, -0.3162353388693405765, 0.4822834645669290543 ) ) ;
#45269 = CARTESIAN_POINT ( 'NONE',  ( -1.417322834645668772, -0.1870078740157479769, 0.3641732283464567677 ) ) ;
#45270 = CARTESIAN_POINT ( 'NONE',  ( 0.3460692066303958092, 0.1998031496062993018, -0.8379265091863516979 ) ) ;
#45271 = CARTESIAN_POINT ( 'NONE',  ( -0.1998031496062991907, -0.3460692066303959757, -0.8530183727034120755 ) ) ;
#45272 = CARTESIAN_POINT ( 'NONE',  ( -0.3420746716998661618, 0.1974969037888702206, -0.4986876640419948270 ) ) ;
#45273 = B_SPLINE_CURVE_WITH_KNOTS ( 'NONE', 3,
 ( #15511, #9191, #33202, #27708, #58867, #53374, #7950 ),
 .UNSPECIFIED., .F., .F.,
 ( 4, 3, 4 ),
 ( 3.643951726750583631E-17, 0.001246232571205267009, 0.002492492258783277591 ),
 .UNSPECIFIED. ) ;
#45274 = CARTESIAN_POINT ( 'NONE',  ( 0.3961547706187970030, 1.274880491790000292, -1.735579852066672979 ) ) ;
#45275 = CARTESIAN_POINT ( 'NONE',  ( 1.227034120734908917, 0.1771653543307087075, -0.09757992244046823083 ) ) ;
#45276 = CARTESIAN_POINT ( 'NONE',  ( 0.5052493438320215802, 0.1771653543307087630, 0.09757992244046791164 ) ) ;
#45277 = CARTESIAN_POINT ( 'NONE',  ( 0.2952755905511816326, -0.5400638737290844871, 0.3530559997133364547 ) ) ;
#45278 = CARTESIAN_POINT ( 'NONE',  ( 1.384514435695538337, -0.6692913385826771977, 0.1292274648535927661 ) ) ;
#45279 = CARTESIAN_POINT ( 'NONE',  ( 0.3949938075777409963, 2.418639510665530743E-17, -1.297244094488188892 ) ) ;
#45280 = CARTESIAN_POINT ( 'NONE',  ( 0.5708661417322842269, 0.07958543189024085140, 0.2665933059059887866 ) ) ;
#45281 = CARTESIAN_POINT ( 'NONE',  ( -0.5971128608923877978, -0.6692913385826773087, -0.1292274648535924053 ) ) ;
#45282 = CARTESIAN_POINT ( 'NONE',  ( -1.227034120734907141, -0.6692913385826773087, -0.1292274648535924053 ) ) ;
#45283 = CARTESIAN_POINT ( 'NONE',  ( 0.9514435695538062676, -0.3162353388693409650, -0.4822834645669289433 ) ) ;
#45284 = CARTESIAN_POINT ( 'NONE',  ( -0.4724409448818898682, -8.678599364036362592E-17, -1.456692913385826849 ) ) ;
#45285 = CARTESIAN_POINT ( 'NONE',  ( -0.1070741851644051862, -0.3996062992125986590, -2.749343832020996636 ) ) ;
#45286 = EDGE_LOOP ( 'NONE', ( #68113, #61059, #14144, #43858 ) ) ;
#45287 = VERTEX_POINT ( 'NONE', #39755 ) ;
#45288 = CARTESIAN_POINT ( 'NONE',  ( -1.167979002624671470, -0.4281496062992127816, -0.4176697321401328100 ) ) ;
#45289 = CARTESIAN_POINT ( 'NONE',  ( -0.8136482939632537770, 0.2306618581243847221, -0.2411417322834647770 ) ) ;
#45291 = CARTESIAN_POINT ( 'NONE',  ( -0.8202099737532799750, 0.2952755905511810774, -0.1292274648535930714 ) ) ;
#45290 = CARTESIAN_POINT ( 'NONE',  ( -0.6692913385826764205, 0.1771653543307087630, 0.000000000000000000 ) ) ;
#45292 = CARTESIAN_POINT ( 'NONE',  ( -0.3392501089628018329, -0.1958661417322836440, -1.864810080543620074 ) ) ;
#45293 = CARTESIAN_POINT ( 'NONE',  ( -0.4600214019799515053, 0.000000000000000000, 0.3464511005275205946 ) ) ;
#45294 = CARTESIAN_POINT ( 'NONE',  ( 1.673228346456693494, 0.1660481256975885056, 0.3530559997133364547 ) ) ;
#45295 = CARTESIAN_POINT ( 'NONE',  ( -1.410761154855642463, -0.05778040916215522460, 0.4822834645669289988 ) ) ;
#45296 = CARTESIAN_POINT ( 'NONE',  ( 0.5183727034120741983, 0.2952755905511810774, -0.1292274648535930714 ) ) ;
#45297 = CARTESIAN_POINT ( 'NONE',  ( -0.6824146981627288167, 0.2306618581243848609, 0.2411417322834645549 ) ) ;
#45298 = CIRCLE ( 'NONE', #6321, 2.362204724409449064 ) ;
#45299 = CARTESIAN_POINT ( 'NONE',  ( -0.1958661417322836718, 0.3392501089628017219, -1.265091863517060489 ) ) ;
#45300 = CARTESIAN_POINT ( 'NONE',  ( -0.9120734908136475250, -0.5511811023622048555, -0.09757992244046775898 ) ) ;
#45301 = ORIENTED_EDGE ( 'NONE', *, *, #22330, .T. ) ;
#45302 = CARTESIAN_POINT ( 'NONE',  ( -9.674558042662121740E-17, 0.3949938075777409963, -2.047244094488188892 ) ) ;
#45303 = VECTOR ( 'NONE', #23517, 39.37007874015748143 ) ;
#45304 = ORIENTED_EDGE ( 'NONE', *, *, #78629, .T. ) ;
#45305 = CARTESIAN_POINT ( 'NONE',  ( -1.732283464566928277, -0.1870078740157479769, 0.3641732283464567677 ) ) ;
#45306 = CARTESIAN_POINT ( 'NONE',  ( -1.292650918635170010, -0.6692913385826771977, 0.1292274648535927661 ) ) ;
#45307 = CARTESIAN_POINT ( 'NONE',  ( -1.233595800524933894, -0.6046776061558809534, -0.2411417322834644161 ) ) ;
#45308 = CARTESIAN_POINT ( 'NONE',  ( -0.2925321140481932924, 0.2925321140481931814, -0.01968503937007875029 ) ) ;
#45309 = CARTESIAN_POINT ( 'NONE',  ( -1.076115485564303809, 0.2306618581243848609, 0.2411417322834645549 ) ) ;
#45310 = CARTESIAN_POINT ( 'NONE',  ( -1.062992125984250968, 0.2952755905511811885, 0.000000000000000000 ) ) ;
#45311 = SURFACE_SIDE_STYLE ('',( #27215 ) ) ;
#45312 = CARTESIAN_POINT ( 'NONE',  ( -0.8530183727034112984, 0.05413385826771666132, 0.4176697321401328100 ) ) ;
#45313 = CARTESIAN_POINT ( 'NONE',  ( -0.03280839895013062252, 0.1771653543307087075, -0.09757992244046823083 ) ) ;
#45314 = CARTESIAN_POINT ( 'NONE',  ( 0.4677827689124922084, 0.03937007874015747977, 2.154527559055118946 ) ) ;
#45315 = CARTESIAN_POINT ( 'NONE',  ( 0.1049643490035303689, 0.3917322834645670104, -0.2355643044619422921 ) ) ;
#45316 = CARTESIAN_POINT ( 'NONE',  ( -0.4724409448818890911, -0.1870078740157479769, 0.3641732283464567677 ) ) ;
#45317 = CARTESIAN_POINT ( 'NONE',  ( -0.7480314960629914633, -0.6692913385826771977, 8.415575281601705876E-17 ) ) ;
#45318 = CARTESIAN_POINT ( 'NONE',  ( 1.266404199475066328, -0.05778040916215522460, 0.4822834645669289988 ) ) ;
#45319 = CARTESIAN_POINT ( 'NONE',  ( -0.6824146981627288167, 0.2306618581243848609, 0.2411417322834645549 ) ) ;
#45320 = ORIENTED_EDGE ( 'NONE', *, *, #10592, .T. ) ;
#45321 = ORIENTED_EDGE ( 'NONE', *, *, #21258, .F. ) ;
#45322 = CARTESIAN_POINT ( 'NONE',  ( 0.3996062992125985480, 2.446882876249141654E-17, -2.084645669291338432 ) ) ;
#45323 = CARTESIAN_POINT ( 'NONE',  ( -1.154855643044618851, 0.2306618581243848609, 0.2411417322834645549 ) ) ;
#45324 = CARTESIAN_POINT ( 'NONE',  ( 1.279527559055118724, 0.1660481256975885056, 0.3530559997133364547 ) ) ;
#45325 = CARTESIAN_POINT ( 'NONE',  ( -1.220472440944881054, 0.1771653543307087630, 0.000000000000000000 ) ) ;
#45326 = CARTESIAN_POINT ( 'NONE',  ( -1.181102362204723644, -0.1870078740157480879, -0.4822834645669291653 ) ) ;
#45327 = CARTESIAN_POINT ( 'NONE',  ( -0.4724409448818895907, -0.1265901696524993070, -0.9908136482939633449 ) ) ;
#45328 = CARTESIAN_POINT ( 'NONE',  ( -2.138346301250427572, 1.653225543546886778, 0.4603267246303517357 ) ) ;
#45329 = CARTESIAN_POINT ( 'NONE',  ( 0.1049643490035303689, 0.3917322834645670104, -0.3005249343832020470 ) ) ;
#45330 = CARTESIAN_POINT ( 'NONE',  ( 0.3917322834645669549, 0.1049643490035304660, -2.099081364829396446 ) ) ;
#45331 = CARTESIAN_POINT ( 'NONE',  ( -0.05905511811023545637, 0.1660481256975885056, 0.3530559997133364547 ) ) ;
#45332 = CARTESIAN_POINT ( 'NONE',  ( -1.417322834645668772, -0.1870078740157480601, -0.3641732283464567677 ) ) ;
#45333 = CARTESIAN_POINT ( 'NONE',  ( -0.6496062992125976043, -0.5400638737290844871, 0.3530559997133364547 ) ) ;
#45334 = CARTESIAN_POINT ( 'NONE',  ( 0.4724409448818897572, -0.1265901696524988906, -2.708005249343832688 ) ) ;
#45335 = CARTESIAN_POINT ( 'NONE',  ( -1.181102362204723644, -0.1870078740157480879, -0.4822834645669291653 ) ) ;
#45336 = CARTESIAN_POINT ( 'NONE',  ( -1.187664041994750175, -0.05778040916215560624, -0.4822834645669293319 ) ) ;
#45337 = CARTESIAN_POINT ( 'NONE',  ( -0.1771653543307080136, -0.5400638737290844871, 0.3530559997133364547 ) ) ;
#45338 = CARTESIAN_POINT ( 'NONE',  ( 0.3949938075777409963, 2.418639510665530743E-17, -2.714566929133857887 ) ) ;
#45339 = CARTESIAN_POINT ( 'NONE',  ( 0.7742782152230978099, -0.3690944881889763329, 0.3153832671262228327 ) ) ;
#45340 = CARTESIAN_POINT ( 'NONE',  ( -0.9251968503937002541, 0.07958543189024085140, 0.2665933059059887866 ) ) ;
#45341 = CARTESIAN_POINT ( 'NONE',  ( -0.1091324866932888854, 1.075701271242782919, -1.559683122296843250 ) ) ;
#45342 = CARTESIAN_POINT ( 'NONE',  ( 0.9120734908136490793, 0.1771653543307087075, -0.09757992244046823083 ) ) ;
#45343 = CARTESIAN_POINT ( 'NONE',  ( 1.568241469816273437, -0.2845877964562159024, 0.3641732283464567677 ) ) ;
#45344 = CARTESIAN_POINT ( 'NONE',  ( 1.181102362204724976, -0.1870078740157480879, -0.4822834645669291653 ) ) ;
#45345 = CARTESIAN_POINT ( 'NONE',  ( 0.06561679790026316017, -0.3690944881889763329, 0.3153832671262228327 ) ) ;
#45346 = CARTESIAN_POINT ( 'NONE',  ( -0.1049643490035302024, -0.3917322834645671215, -1.481627296587926690 ) ) ;
#45347 = CARTESIAN_POINT ( 'NONE',  ( -0.7217847769028863381, -0.4281496062992124485, 0.4176697321401328655 ) ) ;
#45348 = CARTESIAN_POINT ( 'NONE',  ( 1.187664041994751285, -0.3162353388693409650, -0.4822834645669289433 ) ) ;
#45349 = CARTESIAN_POINT ( 'NONE',  ( 0.4724409448818898682, 2.892866454678787531E-17, 0.1200787401574803098 ) ) ;
#45350 = CARTESIAN_POINT ( 'NONE',  ( -0.4790026246719152336, -0.08942795157528024563, -0.3641732283464568787 ) ) ;
#45351 = CARTESIAN_POINT ( 'NONE',  ( 1.854472803289052507, 2.716535433070866645, 0.5314960629921260393 ) ) ;
#45352 = CARTESIAN_POINT ( 'NONE',  ( 0.4330708661417329575, 0.2952755905511811885, 0.000000000000000000 ) ) ;
#45353 = DIRECTION ( 'NONE',  ( -3.096699300667737957E-16, 1.000000000000000000, -0.000000000000000000 ) ) ;
#45354 = CARTESIAN_POINT ( 'NONE',  ( 0.7808398950131240079, -0.2845877964562159024, 0.3641732283464567677 ) ) ;
#45355 = CARTESIAN_POINT ( 'NONE',  ( 0.3412073490813655186, 0.1283753931104748280, 0.1820866141732283561 ) ) ;
#45356 = CARTESIAN_POINT ( 'NONE',  ( -0.5118110236220466680, 0.2952755905511811885, 0.000000000000000000 ) ) ;
#45357 = CARTESIAN_POINT ( 'NONE',  ( -1.266404199475064773, -0.3162353388693405765, 0.4822834645669290543 ) ) ;
#45358 = CARTESIAN_POINT ( 'NONE',  ( -0.7086614173228339419, -0.1870078740157479769, 0.3641732283464567677 ) ) ;
#45359 = CARTESIAN_POINT ( 'NONE',  ( 0.000000000000000000, 2.755905511811024056, 0.000000000000000000 ) ) ;
#45360 = EDGE_CURVE ( 'NONE', #43601, #49366, #54398, .T. ) ;
#45361 = CARTESIAN_POINT ( 'NONE',  ( -0.7283464566929126471, -0.5400638737290844871, 0.3530559997133364547 ) ) ;
#45362 = CARTESIAN_POINT ( 'NONE',  ( -0.1070741851644051862, -0.3996062992125986590, -1.093832020997375087 ) ) ;
#45363 = CARTESIAN_POINT ( 'NONE',  ( 4.797336870675656522E-17, -0.3917322834645670104, -2.683070866141731958 ) ) ;
#45364 = CARTESIAN_POINT ( 'NONE',  ( 0.01968503937007930540, 0.07958543189024085140, 0.2665933059059887866 ) ) ;
#45366 = AXIS2_PLACEMENT_3D ( 'NONE', #18194, #56881, #17784 ) ;
#45365 = CARTESIAN_POINT ( 'NONE',  ( -0.8070866141732276899, 0.1660481256975883668, -0.3530559997133364547 ) ) ;
#45367 = CARTESIAN_POINT ( 'NONE',  ( -0.9383202099737524282, -0.3162353388693409650, -0.4822834645669289433 ) ) ;
#45368 = CARTESIAN_POINT ( 'NONE',  ( -1.417322834645668772, -0.1870078740157480601, -0.3641732283464567677 ) ) ;
#45369 = CARTESIAN_POINT ( 'NONE',  ( 1.666666666666667185, 0.05413385826771666132, 0.4176697321401328100 ) ) ;
#45370 = CARTESIAN_POINT ( 'NONE',  ( -0.8267716535433065062, 0.1771653543307087630, 0.000000000000000000 ) ) ;
#45371 = LINE ( 'NONE', #71066, #69663 ) ;
#45372 = CARTESIAN_POINT ( 'NONE',  ( 1.246719160104987623, -0.4281496062992124485, 0.4176697321401328655 ) ) ;
#45373 = CARTESIAN_POINT ( 'NONE',  ( 0.01149616601327405584, 2.739544932778246860E-15, 0.3791475997938225095 ) ) ;
#45374 = CARTESIAN_POINT ( 'NONE',  ( -0.1049643490035307158, 0.3917322834645670104, -1.893063935204411186 ) ) ;
#45375 = VERTEX_POINT ( 'NONE', #47722 ) ;
#45376 = CARTESIAN_POINT ( 'NONE',  ( -0.2242874410717133060, -4.005968212718139582E-15, 0.3627989612356165572 ) ) ;
#45377 = CARTESIAN_POINT ( 'NONE',  ( 1.397637795275591177, -0.4536011799217367080, 0.2665933059059888421 ) ) ;
#45378 = CARTESIAN_POINT ( 'NONE',  ( -1.430446194225721390, -0.4281496062992124485, 0.4176697321401328655 ) ) ;
#45379 = CARTESIAN_POINT ( 'NONE',  ( 1.240157480314961314, -0.5400638737290844871, 0.3530559997133364547 ) ) ;
#45380 = CARTESIAN_POINT ( 'NONE',  ( 0.3917322834645670104, 2.398668435337828261E-17, -1.935039370078740273 ) ) ;
#45381 = CARTESIAN_POINT ( 'NONE',  ( -1.614173228346456712, 0.8346805926620878280, -0.1372047244094478091 ) ) ;
#45382 = EDGE_CURVE ( 'NONE', #4617, #27226, #61939, .T. ) ;
#45383 = CARTESIAN_POINT ( 'NONE',  ( 0.5905511811023629321, 0.2952755905511811885, 0.000000000000000000 ) ) ;
#45384 = CARTESIAN_POINT ( 'NONE',  ( -0.1509186351706028884, -0.3162353388693409650, -0.4822834645669289433 ) ) ;
#45385 = CARTESIAN_POINT ( 'NONE',  ( -0.6758530183727027296, 0.2952755905511811885, 0.1292274648535926551 ) ) ;
#45386 = CARTESIAN_POINT ( 'NONE',  ( 0.6561679790026253567, 0.1283753931104748280, 0.1820866141732283561 ) ) ;
#45387 = CARTESIAN_POINT ( 'NONE',  ( -0.3996062992125986035, -7.340648628747425578E-17, -1.141732283464566899 ) ) ;
#45388 = VERTEX_POINT ( 'NONE', #23298 ) ;
#45389 = CARTESIAN_POINT ( 'NONE',  ( -0.3917322834645670104, -0.1049643490035307020, -0.04267023441700976139 ) ) ;
#45390 = ORIENTED_EDGE ( 'NONE', *, *, #79506, .F. ) ;
#45391 = CARTESIAN_POINT ( 'NONE',  ( -0.1509186351706028884, -0.05778040916215522460, 0.4822834645669289988 ) ) ;
#45392 = CARTESIAN_POINT ( 'NONE',  ( -1.587926509186350810, 0.05413385826771626580, -0.4176697321401330321 ) ) ;
#45393 = CARTESIAN_POINT ( 'NONE',  ( 0.7086614173228353852, -0.1870078740157479769, 0.4822834645669291653 ) ) ;
#45394 = CARTESIAN_POINT ( 'NONE',  ( 1.023622047244095334, -0.1870078740157479769, 0.4822834645669291653 ) ) ;
#45395 = FACE_OUTER_BOUND ( 'NONE', #33529, .T. ) ;
#45396 = CARTESIAN_POINT ( 'NONE',  ( -0.5249343832020990641, 0.2306618581243848609, 0.2411417322834645549 ) ) ;
#45397 = CARTESIAN_POINT ( 'NONE',  ( 0.2165354330708668673, 0.1660481256975883668, -0.3530559997133364547 ) ) ;
#45398 = CARTESIAN_POINT ( 'NONE',  ( 1.489501312335958172, -0.05778040916215560624, -0.4822834645669293319 ) ) ;
#45400 = EDGE_CURVE ( 'NONE', #36200, #16126, #31130, .T. ) ;
#45399 = CARTESIAN_POINT ( 'NONE',  ( 1.292650918635171564, 0.2952755905511811885, 0.1292274648535926551 ) ) ;
#45401 = CARTESIAN_POINT ( 'NONE',  ( 1.030183727034121421, -0.05778040916215522460, 0.4822834645669289988 ) ) ;
#45402 = CARTESIAN_POINT ( 'NONE',  ( -0.1312335958005241554, 0.2306618581243848609, 0.2411417322834645549 ) ) ;
#45403 = CARTESIAN_POINT ( 'NONE',  ( -0.2867679344610365999, 0.2867679344610364889, -0.1692913385826771144 ) ) ;
#45404 = CARTESIAN_POINT ( 'NONE',  ( 0.4658792650918641698, -0.08942795157528024563, -0.3641732283464568787 ) ) ;
#45405 = ORIENTED_EDGE ( 'NONE', *, *, #37854, .T. ) ;
#45406 = CARTESIAN_POINT ( 'NONE',  ( 0.2891555358219910499, -0.2891555358219909944, -0.7283464566929134243 ) ) ;
#45407 = ORIENTED_EDGE ( 'NONE', *, *, #6791, .F. ) ;
#45408 = CARTESIAN_POINT ( 'NONE',  ( -0.3871391076115479057, -0.2845877964562161244, -0.3641732283464567121 ) ) ;
#45409 = CARTESIAN_POINT ( 'NONE',  ( 2.558820304884363406, 1.494558157769223961, -0.4725443725032419939 ) ) ;
#45410 = CARTESIAN_POINT ( 'NONE',  ( 0.2690288713910767848, -0.6692913385826773087, -0.1292274648535924053 ) ) ;
#45411 = CARTESIAN_POINT ( 'NONE',  ( -0.1902887139107604098, -0.6692913385826771977, 0.1292274648535927661 ) ) ;
#45412 = CARTESIAN_POINT ( 'NONE',  ( -0.8530183727034112984, -0.4281496062992127816, -0.4176697321401328100 ) ) ;
#45413 = CARTESIAN_POINT ( 'NONE',  ( -0.1049643490035302301, -0.3917322834645671770, -1.801200418144043969 ) ) ;
#45414 = CARTESIAN_POINT ( 'NONE',  ( -1.581364829396324945, -0.05778040916215560624, -0.4822834645669293319 ) ) ;
#45415 = CARTESIAN_POINT ( 'NONE',  ( -0.1455472725388424760, -1.150887559458346504E-15, 0.3627985898453522928 ) ) ;
#45416 = CARTESIAN_POINT ( 'NONE',  ( 1.062992125984252745, -0.5511811023622047445, 6.969142054262312111E-17 ) ) ;
#45417 = CARTESIAN_POINT ( 'NONE',  ( 0.3149606299212606708, -0.1870078740157480879, -0.4822834645669291653 ) ) ;
#45418 = CARTESIAN_POINT ( 'NONE',  ( 0.7808398950131241190, -0.05778040916215560624, -0.4822834645669293319 ) ) ;
#45419 = CARTESIAN_POINT ( 'NONE',  ( 0.3996062992125986590, -0.1070741851644053111, -1.371391076115485053 ) ) ;
#45420 = CARTESIAN_POINT ( 'NONE',  ( -2.571698080334722025, 1.622209144264171066, 0.4670403427556019671 ) ) ;
#45421 = CARTESIAN_POINT ( 'NONE',  ( -0.3996062992125985480, -7.340648628747423112E-17, -0.9035433070866141225 ) ) ;
#45422 = CARTESIAN_POINT ( 'NONE',  ( -0.1070741851644051862, -0.3996062992125986590, -0.3064304461942257141 ) ) ;
#45423 = CARTESIAN_POINT ( 'NONE',  ( -0.1509186351706028884, -0.05778040916215522460, 0.4822834645669289988 ) ) ;
#45424 = CARTESIAN_POINT ( 'NONE',  ( -0.1070741851644056997, 0.3996062992125986035, -2.526246719160104792 ) ) ;
#45425 = CARTESIAN_POINT ( 'NONE',  ( -0.1049643490035307020, 0.3917322834645669549, -2.138451443569553412 ) ) ;
#45426 = CARTESIAN_POINT ( 'NONE',  ( -1.410761154855641575, -0.2845877964562161244, -0.3641732283464567121 ) ) ;
#45427 = CARTESIAN_POINT ( 'NONE',  ( 1.135170603674541256, 0.2952755905511811885, 0.1292274648535926551 ) ) ;
#45428 = VECTOR ( 'NONE', #38649, 39.37007874015748143 ) ;
#45429 = CARTESIAN_POINT ( 'NONE',  ( 1.450131233595801428, -0.6692913385826773087, -0.1292274648535924053 ) ) ;
#45430 = CARTESIAN_POINT ( 'NONE',  ( 0.2362204724409456558, -0.1870078740157479769, 0.3641732283464567677 ) ) ;
#45431 = CARTESIAN_POINT ( 'NONE',  ( 0.3937007874015754361, -0.1870078740157480879, -0.4822834645669291653 ) ) ;
#45432 = CARTESIAN_POINT ( 'NONE',  ( -0.4724409448818899238, 0.1265901696524986686, -1.369422572178477404 ) ) ;
#45433 = CARTESIAN_POINT ( 'NONE',  ( 0.3608923884514443348, -0.5511811023622046335, 0.09757992244046803654 ) ) ;
#45434 = CARTESIAN_POINT ( 'NONE',  ( 0.09842519685039434474, -0.5400638737290845981, -0.3530559997133363437 ) ) ;
#45435 = CARTESIAN_POINT ( 'NONE',  ( 0.3420746716998660508, 0.1974969037888705814, -1.467847769028871374 ) ) ;
#45436 = CARTESIAN_POINT ( 'NONE',  ( -1.397637795275589623, 0.1660481256975885056, 0.3530559997133364547 ) ) ;
#45437 = CARTESIAN_POINT ( 'NONE',  ( 0.5708661417322841158, -0.4536011799217368745, -0.2665933059059886201 ) ) ;
#45438 = CARTESIAN_POINT ( 'NONE',  ( -1.076935383196057305, 5.463695987328539379E-17, -0.3149606299212603933 ) ) ;
#45439 = CARTESIAN_POINT ( 'NONE',  ( -0.6627296587926503335, -0.6692913385826771977, 0.1292274648535927661 ) ) ;
#45440 = CARTESIAN_POINT ( 'NONE',  ( -0.3412073490813641308, 0.1283753931104746893, -0.1820866141732285504 ) ) ;
#45441 = CARTESIAN_POINT ( 'NONE',  ( -0.7345763329969765554, 1.945772889739036060, -0.5309055118110235227 ) ) ;
#45442 = CARTESIAN_POINT ( 'NONE',  ( -0.9055118110236215490, 0.2952755905511811885, 0.000000000000000000 ) ) ;
#45443 = CARTESIAN_POINT ( 'NONE',  ( -0.08530183727034056085, -0.3162353388693405765, 0.4822834645669290543 ) ) ;
#45444 = CARTESIAN_POINT ( 'NONE',  ( 0.2559055118110243332, -0.4536011799217368745, -0.2665933059059886201 ) ) ;
#45445 = CARTESIAN_POINT ( 'NONE',  ( -0.2925321140481932369, 0.2925321140481931259, -1.986220472440945128 ) ) ;
#45446 = CARTESIAN_POINT ( 'NONE',  ( 0.07874015748031558404, -0.1870078740157479769, 0.4822834645669291653 ) ) ;
#45447 = CARTESIAN_POINT ( 'NONE',  ( 0.3917322834645669549, 2.398668435337827645E-17, -2.245387508365142892 ) ) ;
#45448 = CARTESIAN_POINT ( 'NONE',  ( 0.7020997375328090762, -0.2845877964562159024, 0.3641732283464567677 ) ) ;
#45449 = CARTESIAN_POINT ( 'NONE',  ( 1.286089238845145033, 0.2306618581243848609, 0.2411417322834645549 ) ) ;
#45450 = CARTESIAN_POINT ( 'NONE',  ( -0.6430446194225716283, -0.3690944881889763329, 0.3153832671262228327 ) ) ;
#45451 = CARTESIAN_POINT ( 'NONE',  ( -1.325459317585300889, -0.3690944881889765550, -0.3153832671262227771 ) ) ;
#45452 = CARTESIAN_POINT ( 'NONE',  ( -0.5774278215223089816, -0.6046776061558807314, 0.2411417322834647770 ) ) ;
#45453 = CARTESIAN_POINT ( 'NONE',  ( 0.04593175853018440641, 0.2952755905511810774, -0.1292274648535930714 ) ) ;
#45454 = CARTESIAN_POINT ( 'NONE',  ( 0.4265091863517067594, 0.1771653543307087630, 0.09757992244046791164 ) ) ;
#45455 = CARTESIAN_POINT ( 'NONE',  ( 0.000000000000000000, 2.165354330708661568, 0.000000000000000000 ) ) ;
#45456 = CARTESIAN_POINT ( 'NONE',  ( 1.187664041994751285, -0.2845877964562161244, -0.3641732283464567121 ) ) ;
#45457 = ADVANCED_FACE ( 'NONE', ( #35106 ), #63563, .F. ) ;
#45458 = CARTESIAN_POINT ( 'NONE',  ( 0.2887139107611556010, 0.2306618581243847221, -0.2411417322834647770 ) ) ;
#45459 = CARTESIAN_POINT ( 'NONE',  ( 0.01707598052245543063, 1.062992125984252745, -1.850393700787402729 ) ) ;
#45460 = CARTESIAN_POINT ( 'NONE',  ( -0.2230971128608915943, -0.4281496062992127816, -0.4176697321401328100 ) ) ;
#45461 = CARTESIAN_POINT ( 'NONE',  ( -0.3917322834645670104, -7.196005306013484475E-17, -1.383858267716535417 ) ) ;
#45462 = CARTESIAN_POINT ( 'NONE',  ( 1.548556430446194954, -0.5023911411419708095, 0.1820866141732285504 ) ) ;
#45463 = CARTESIAN_POINT ( 'NONE',  ( 0.2690288713910767848, 0.2952755905511811885, 0.1292274648535926551 ) ) ;
#45464 = CARTESIAN_POINT ( 'NONE',  ( 0.2821522309711292364, 0.2952755905511810774, -0.1292274648535930714 ) ) ;
#45465 = CARTESIAN_POINT ( 'NONE',  ( 0.5774278215223104249, 0.1539470093639523085, 0.1968503937007873850 ) ) ;
#45466 = CARTESIAN_POINT ( 'NONE',  ( 0.07217847769028949700, -0.2845877964562159024, 0.3641732283464567677 ) ) ;
#45467 = CARTESIAN_POINT ( 'NONE',  ( 0.9776902887139113929, -0.6692913385826773087, -0.1292274648535924053 ) ) ;
#45468 = CARTESIAN_POINT ( 'NONE',  ( -0.1771653543307080136, -0.4536011799217367080, 0.2665933059059888421 ) ) ;
#45469 = CARTESIAN_POINT ( 'NONE',  ( -0.8136482939632537770, 0.2306618581243847221, -0.2411417322834647770 ) ) ;
#45470 = DIRECTION ( 'NONE',  ( 1.000000000000000000, -0.000000000000000000, -0.000000000000000000 ) ) ;
#45471 = CARTESIAN_POINT ( 'NONE',  ( -0.2493438320209966919, 0.05413385826771626580, -0.4176697321401330321 ) ) ;
#45472 = APPLICATION_CONTEXT ( 'automotive_design' ) ;
#45473 = CARTESIAN_POINT ( 'NONE',  ( -1.240157480314959759, -0.5400638737290845981, -0.3530559997133363437 ) ) ;
#45474 = CARTESIAN_POINT ( 'NONE',  ( -0.7874015748031489847, -0.1870078740157479769, 0.3641732283464567677 ) ) ;
#45475 = CARTESIAN_POINT ( 'NONE',  ( 0.3280839895013130669, 0.05413385826771666132, 0.4176697321401328100 ) ) ;
#45476 = CARTESIAN_POINT ( 'NONE',  ( -1.246719160104986512, 0.05413385826771666132, 0.4176697321401328100 ) ) ;
#45477 = CARTESIAN_POINT ( 'NONE',  ( -0.1574803149606292529, -0.1870078740157480879, -0.4822834645669291653 ) ) ;
#45478 = DIRECTION ( 'NONE',  ( -0.000000000000000000, -1.000000000000000000, -0.000000000000000000 ) ) ;
#45480 = CARTESIAN_POINT ( 'NONE',  ( 1.404199475065617264, -0.4281496062992124485, 0.4176697321401328655 ) ) ;
#45479 = DIRECTION ( 'NONE',  ( 0.000000000000000000, 0.000000000000000000, 1.000000000000000000 ) ) ;
#45481 = CARTESIAN_POINT ( 'NONE',  ( 1.305774278215223960, -0.6692913385826771977, 0.1292274648535927661 ) ) ;
#45482 = CARTESIAN_POINT ( 'NONE',  ( 0.3917322834645670104, 2.398668435337828261E-17, -2.629921259842519898 ) ) ;
#45483 = CARTESIAN_POINT ( 'NONE',  ( 0.2362204724409449064, 0.000000000000000000, 0.000000000000000000 ) ) ;
#45484 = CARTESIAN_POINT ( 'NONE',  ( -1.122047244094487306, -0.5400638737290844871, 0.3530559997133364547 ) ) ;
#45485 = CARTESIAN_POINT ( 'NONE',  ( -0.2362204724409451284, 0.4091458600556402425, -0.8005249343832020470 ) ) ;
#45486 = CARTESIAN_POINT ( 'NONE',  ( -0.3996062992125986035, -7.340648628747425578E-17, 0.1181102362204724254 ) ) ;
#45487 = ORIENTED_EDGE ( 'NONE', *, *, #55596, .T. ) ;
#45488 = CARTESIAN_POINT ( 'NONE',  ( 0.07217847769028949700, -0.2845877964562159024, 0.3641732283464567677 ) ) ;
#45489 = CARTESIAN_POINT ( 'NONE',  ( 0.1958661417322836440, -0.3392501089628017219, -1.658792650918635259 ) ) ;
#45490 = ORIENTED_EDGE ( 'NONE', *, *, #11466, .T. ) ;
#45491 = CARTESIAN_POINT ( 'NONE',  ( 0.2952755905511816326, -0.5400638737290844871, 0.3530559997133364547 ) ) ;
#45492 = CARTESIAN_POINT ( 'NONE',  ( 0.3543307086614179147, 0.2952755905511811885, 0.000000000000000000 ) ) ;
#45493 = CARTESIAN_POINT ( 'NONE',  ( 0.4091458600556404646, -0.2362204724409448231, -2.939632545931758489 ) ) ;
#45494 = FACE_OUTER_BOUND ( 'NONE', #54288, .T. ) ;
#45495 = CARTESIAN_POINT ( 'NONE',  ( -0.9251968503937002541, -0.4536011799217368745, -0.2665933059059886201 ) ) ;
#45496 =( NAMED_UNIT ( * ) PLANE_ANGLE_UNIT ( ) SI_UNIT ( $, .RADIAN. ) );
#45497 = CARTESIAN_POINT ( 'NONE',  ( 0.9251968503937015864, 0.1660481256975883668, -0.3530559997133364547 ) ) ;
#45498 = CARTESIAN_POINT ( 'NONE',  ( 1.089238845144357537, -0.3690944881889763329, 0.3153832671262228327 ) ) ;
#45499 = CARTESIAN_POINT ( 'NONE',  ( -0.2690288713910754526, -0.6692913385826771977, 0.1292274648535927661 ) ) ;
#45500 = CARTESIAN_POINT ( 'NONE',  ( 0.3917322834645669549, 2.398668435337827645E-17, -1.300505618601362601 ) ) ;
#45501 = CARTESIAN_POINT ( 'NONE',  ( -0.6824146981627288167, 0.2306618581243848609, 0.2411417322834645549 ) ) ;
#45502 = CARTESIAN_POINT ( 'NONE',  ( -1.207349081364828880, 0.1283753931104746893, -0.1820866141732285504 ) ) ;
#45503 = CARTESIAN_POINT ( 'NONE',  ( -0.8136482939632537770, -0.6046776061558807314, 0.2411417322834647770 ) ) ;
#45504 = CARTESIAN_POINT ( 'NONE',  ( 1.450131233595801428, -0.6692913385826773087, -0.1292274648535924053 ) ) ;
#45505 = CARTESIAN_POINT ( 'NONE',  ( 1.673228346456693494, 0.07958543189024085140, 0.2665933059059887866 ) ) ;
#45506 = ORIENTED_EDGE ( 'NONE', *, *, #19638, .F. ) ;
#45507 = CARTESIAN_POINT ( 'NONE',  ( -0.1049643490035307158, 0.3917322834645670104, -2.365504880086300776 ) ) ;
#45508 = CARTESIAN_POINT ( 'NONE',  ( 0.1049868766404206816, 0.2306618581243848609, 0.2411417322834645549 ) ) ;
#45509 = ORIENTED_EDGE ( 'NONE', *, *, #17090, .F. ) ;
#45510 = CARTESIAN_POINT ( 'NONE',  ( -0.6102362204724400829, 0.1660481256975885056, 0.3530559997133364547 ) ) ;
#45511 = CARTESIAN_POINT ( 'NONE',  ( 1.423884514435696191, -0.05778040916215522460, 0.4822834645669289988 ) ) ;
#45512 = CARTESIAN_POINT ( 'NONE',  ( 1.417322834645670104, -0.1870078740157479769, 0.4822834645669291653 ) ) ;
#45513 = ADVANCED_FACE ( 'NONE', ( #28789 ), #38829, .F. ) ;
#45514 = CARTESIAN_POINT ( 'NONE',  ( 0.1968503937007881344, 0.2952755905511811885, 0.000000000000000000 ) ) ;
#45515 = CARTESIAN_POINT ( 'NONE',  ( -0.02624671916010428221, 0.2306618581243847221, -0.2411417322834647770 ) ) ;
#45516 = CARTESIAN_POINT ( 'NONE',  ( 0.2867679344610365999, -0.2867679344610365444, -1.915354330708661124 ) ) ;
#45517 = CARTESIAN_POINT ( 'NONE',  ( -1.030183727034119867, -0.05778040916215560624, -0.4822834645669293319 ) ) ;
#45518 = CARTESIAN_POINT ( 'NONE',  ( -0.1837270341207340729, 0.2306618581243847221, -0.2411417322834647770 ) ) ;
#45519 = EDGE_CURVE ( 'NONE', #38656, #4617, #21170, .T. ) ;
#45520 = CARTESIAN_POINT ( 'NONE',  ( -0.03280839895013062252, 0.1771653543307087075, -0.09757992244046823083 ) ) ;
#45521 = CARTESIAN_POINT ( 'NONE',  ( 1.299212598425197429, -0.6692913385826771977, 8.415575281601705876E-17 ) ) ;
#45522 = CARTESIAN_POINT ( 'NONE',  ( -0.4068241469816267775, 0.05413385826771626580, -0.4176697321401330321 ) ) ;
#45523 = CARTESIAN_POINT ( 'NONE',  ( 1.141392835773559211, 0.4110443821404751730, 1.318558190104271333 ) ) ;
#45524 = CARTESIAN_POINT ( 'NONE',  ( 0.9973753280839902091, 0.2306618581243847221, -0.2411417322834647770 ) ) ;
#45525 = DIRECTION ( 'NONE',  ( -3.096699300667737957E-16, 1.000000000000000000, -0.000000000000000000 ) ) ;
#45526 = ORIENTED_EDGE ( 'NONE', *, *, #69939, .F. ) ;
#45527 = ORIENTED_EDGE ( 'NONE', *, *, #3893, .T. ) ;
#45528 = CARTESIAN_POINT ( 'NONE',  ( 0.3805774278215230400, -0.4281496062992124485, 0.4176697321401328655 ) ) ;
#45529 = CARTESIAN_POINT ( 'NONE',  ( -0.2559055118110230564, 0.07958543189024071263, -0.2665933059059888421 ) ) ;
#45531 = DIRECTION ( 'NONE',  ( 0.000000000000000000, 0.000000000000000000, -1.000000000000000000 ) ) ;
#45530 = CARTESIAN_POINT ( 'NONE',  ( 1.384514435695538559, 0.1771653543307087075, -0.09757992244046823083 ) ) ;
#45532 = CARTESIAN_POINT ( 'NONE',  ( 0.2362204724409451007, -0.4091458600556402980, -0.3261154855643044748 ) ) ;
#45533 = CARTESIAN_POINT ( 'NONE',  ( 1.614173228346457378, 1.330640075373405118, -0.1372047244094476148 ) ) ;
#45534 = CARTESIAN_POINT ( 'NONE',  ( 1.233595800524935227, -0.6046776061558807314, 0.2411417322834647770 ) ) ;
#45535 = CARTESIAN_POINT ( 'NONE',  ( 0.3420746716998660508, -0.1974969037888704149, -0.3392388451443569819 ) ) ;
#45536 = CARTESIAN_POINT ( 'NONE',  ( 0.02624671916010564918, 0.2306618581243848609, 0.2411417322834645549 ) ) ;
#45537 = CARTESIAN_POINT ( 'NONE',  ( -0.000000000000000000, 0.1742125984251973736, -0.3937007874015748254 ) ) ;
#45538 = CARTESIAN_POINT ( 'NONE',  ( -1.653543307086613234, -0.1870078740157480879, -0.4822834645669291653 ) ) ;
#45539 = CARTESIAN_POINT ( 'NONE',  ( -0.1049868766404193215, 0.2306618581243847221, -0.2411417322834647770 ) ) ;
#45540 = CARTESIAN_POINT ( 'NONE',  ( -0.3420746716998662729, 0.1974969037888702206, -0.1030183727034120894 ) ) ;
#45541 = CARTESIAN_POINT ( 'NONE',  ( 1.581364829396326277, -0.3162353388693409650, -0.4822834645669289433 ) ) ;
#45542 = CARTESIAN_POINT ( 'NONE',  ( 0.3346456692913390985, 0.1660481256975885056, 0.3530559997133364547 ) ) ;
#45543 = CARTESIAN_POINT ( 'NONE',  ( 1.049868766404200349, 0.1283753931104748280, 0.1820866141732283561 ) ) ;
#45544 = CARTESIAN_POINT ( 'NONE',  ( 0.1455242698426520154, 1.053217739199509007, 0.2773898834120265833 ) ) ;
#45545 = CARTESIAN_POINT ( 'NONE',  ( 0.9580052493438327987, -0.3690944881889765550, -0.3153832671262227771 ) ) ;
#45546 = CARTESIAN_POINT ( 'NONE',  ( -1.410761154855641575, -0.3162353388693409650, -0.4822834645669289433 ) ) ;
#45547 = ADVANCED_FACE ( 'NONE', ( #14563 ), #72620, .T. ) ;
#45548 = CARTESIAN_POINT ( 'NONE',  ( -0.2925321140481930149, -0.2925321140481933480, -0.7657480314960628531 ) ) ;
#45549 = CARTESIAN_POINT ( 'NONE',  ( 1.299212598425197429, -0.6692913385826771977, 8.415575281601705876E-17 ) ) ;
#45550 = CARTESIAN_POINT ( 'NONE',  ( 0.1958661417322834775, 0.3392501089628018884, -0.4514435695538057125 ) ) ;
#45552 = CARTESIAN_POINT ( 'NONE',  ( 0.5314960629920926216, 2.755905511811024056, 3.184294706754636106 ) ) ;
#45551 = CARTESIAN_POINT ( 'NONE',  ( 0.8530183727034128527, -0.4281496062992124485, 0.4176697321401328655 ) ) ;
#45553 = CARTESIAN_POINT ( 'NONE',  ( -0.4724409448818898682, -8.678599364036362592E-17, -2.559055118110236560 ) ) ;
#45554 = CARTESIAN_POINT ( 'NONE',  ( 0.2427821522309716595, -0.2845877964562161244, -0.3641732283464567121 ) ) ;
#45555 = EDGE_CURVE ( 'NONE', #28439, #42372, #43195, .T. ) ;
#45556 = CARTESIAN_POINT ( 'NONE',  ( 0.5774278215223104249, 0.2306618581243848609, 0.2411417322834645549 ) ) ;
#45557 = CARTESIAN_POINT ( 'NONE',  ( 1.614173228346457378, 0.5038684218300975015, 0.1372047244094478369 ) ) ;
#45558 = CARTESIAN_POINT ( 'NONE',  ( -0.9514435695538050464, -0.2845877964562159024, 0.3641732283464567677 ) ) ;
#45559 = CARTESIAN_POINT ( 'NONE',  ( -0.9055118110236215490, 0.2952755905511811885, 0.000000000000000000 ) ) ;
#45560 = CARTESIAN_POINT ( 'NONE',  ( 1.010498687664042716, -0.4281496062992124485, 0.4176697321401328655 ) ) ;
#45561 = CARTESIAN_POINT ( 'NONE',  ( -1.135170603674539924, -0.6692913385826771977, 0.1292274648535927661 ) ) ;
#45562 = CARTESIAN_POINT ( 'NONE',  ( 1.076115485564305141, 0.2306618581243847221, -0.2411417322834647770 ) ) ;
#45563 = CARTESIAN_POINT ( 'NONE',  ( -1.246719160104985846, -0.3690944881889765550, -0.3153832671262227771 ) ) ;
#45564 = EDGE_CURVE ( 'NONE', #37037, #36386, #40215, .T. ) ;
#45565 = CARTESIAN_POINT ( 'NONE',  ( -1.646051170424378096, 0.000000000000000000, 0.3464511005275205946 ) ) ;
#45566 = CARTESIAN_POINT ( 'NONE',  ( 1.115485564304462551, 0.05413385826771666132, 0.4176697321401328100 ) ) ;
#45567 = CARTESIAN_POINT ( 'NONE',  ( 0.1265901696524990294, -0.4724409448818896462, -2.366797900262467280 ) ) ;
#45568 = DIRECTION ( 'NONE',  ( -0.000000000000000000, -1.000000000000000000, -0.000000000000000000 ) ) ;
#45569 = CARTESIAN_POINT ( 'NONE',  ( 1.594488188976378673, -0.5400638737290845981, -0.3530559997133363437 ) ) ;
#45570 = CARTESIAN_POINT ( 'NONE',  ( -1.305774278215222184, -0.5511811023622048555, -0.09757992244046775898 ) ) ;
#45572 = CARTESIAN_POINT ( 'NONE',  ( 1.456692913385827515, -0.5511811023622047445, 6.969142054262312111E-17 ) ) ;
#45571 =( BOUNDED_SURFACE ( )  B_SPLINE_SURFACE ( 1, 2, ( 
 ( #23085, #48752, #74451, #16797, #43251, #42434, #80365, #48337, #36957, #4978, #68134, #10479, #74034, #16381, #42027, #10057, #37778, #57121, #76509, #77333, #70593, #76914, #82815, #7040, #12527, #83229, #31878, #57949, #38188, #25970, #69776, #25139, #317, #31459, #39016, #51629, #63863, #6200, #32709, #52053, #63454, #50808, #64700, #57538, #12947, #58375, #13785, #25550, #12120, #19662, #26395, #45324, #77758, #20091, #71437, #5789, #738, #45741, #71019, #56714, #13363, #39441, #51217, #65129, #38605, #19243, #64283, #18838, #82412, #50399, #44894, #18440, #6618, #31045, #32289, #24731, #76096, #44082, #44483, #70175, #58804, #1162, #42647, #40279, #26813, #79021, #67509, #74663, #52471, #20510, #29201, #74245, #21340, #14625, #41818, #54867, #67927, #71859, #65962, #9845, #27646, #7464, #35517, #8298, #72278, #61180, #39865, #10268, #46163, #52889, #16587, #27229, #14209, #3534, #3948, #48547, #80573, #72686, #80980, #22883, #53308, #61605, #35936, #42233, #7887, #29609, #55269, #46993, #15034, #65556, #48963, #59628, #78179, #1983, #33134, #23292, #17007, #33966, #78601, #33551, #59213, #1574, #20925, #46580, #43459, #51010, #4350, #31670, #25348, #63660, #75072, #30435, #50601, #76308, #36745, #55682, #76709, #36339, #6001, #17419, #62013, #4759, #30017, #57331, #82615, #5180, #44283, #37985, #81389, #56509, #23705, #82211, #62422, #18639, #19042, #43050, #75486, #68344, #83025, #49376, #10684, #11089, #30844, #43873, #68746, #56100, #81804, #5586, #69973, #24530, #17826, #18233, #31253, #12327, #24116, #69157, #69571, #50195, #49785, #11919, #11508, #37164, #37574, #62844, #75893, #63247, #56920, #24931, #64494, #51425, #39659, #40080, #1373, #77973, #26615, #33764, #33354, #7254, #14428, #72069, #52685, #45111, #27024, #20303, #961, #52268, #19461, #1781, #13578, #64080, #39232, #78811, #78393, #58592, #51848, #6832, #65767, #45953, #77555, #71234, #71650, #19888, #45536, #25764, #65349, #8099, #59017, #59426, #27440, #53102, #58165, #20724, #64917, #44689, #14001, #7687, #46376, #77127, #32086, #70385, #70818, #12741, #38400, #32927, #533, #6417, #57747, #109, #13166, #38816, #32502, #26187, #34602, #73743, #29513, #79232, #66590, #40908, #54352, #53935, #21964, #16496, #72486, #48042, #8925, #8513, #60267, #80064, #67008, #79647, #59844, #22789, #21547, #2617, #47208, #3025, #15249, #66175, #34179, #10174, #35423, #67418, #47624, #2196, #74149, #21140, #14835, #9341, #27864, #16079, #53524, #72898, #41724, #9751, #73320, #28273, #60676, #35839, #54773, #55174, #15666, #40495, #35012, #41328, #61088, #46795, #28691, #22382, #3439, #29102, #80477, #48449, #42140, #67835, #61507, #3853, #68253, #17325, #30752, #43357, #55999, #36245, #82518, #55582, #42954, #23608, #62748, #74980, #42550, #10588, #69879, #11826, #43769, #81710, #61914, #50503, #80883, #74566, #69057, #4256, #75793, #29919, #5899, #37479, #76207, #11407, #56820, #63151, #5083, #18544, #81293, #24020, #12232, #49277, #68648, #10986, #36647, #62322, #37063, #4659, #23196, #63565, #82114, #69473, #30333, #49688, #5492, #56415, #31153, #24428, #75381, #17729, #50097, #24834, #18135, #44188, #37889, #31571, #48867, #16912, #58064, #856, #38717, #52167, #12640, #12, #26513, #57650, #65245, #77871, #6731, #32401, #58917, #78293, #6312, #25665, #7583, #431, #31989, #20201, #19362, #64395, #38300, #45851, #52584, #71550, #20625, #46276, #14326, #70711, #33255, #26086, #26925, #32824, #7153, #39557, #63976, #44593, #1276, #77030, #71972, #58491, #51746, #13899, #39984, #65674, #76615, #18945, #8001, #57228, #82929, #51326, #45011, #25251, #50915, #13063, #70288, #77449, #19783, #45436, #71131, #13474, #39131, #64812, #80379, #47940, #53833, #9656, #3338, #27342, #21860, #53000, #47525, #2096, #41632, #16396, #40393, #40804, #42042, #29002, #14740, #74048, #59742, #79547, #66075, #67322, #22692, #54251, #59327, #22280, #54668, #66488, #35326, #73216, #34500, #41226, #27761, #1683, #78713, #15566, #21038, #8823, #33665, #60165, #2518, #28176, #73643, #66913, #67738, #46697, #72390 ),
 ( #48351, #8411, #34079, #53426, #79134, #21451, #9245, #47108, #72798, #15147, #34917, #15985, #60579, #2930, #60989, #28594, #79967, #36971, #16813, #36147, #55486, #56323, #49596, #55903, #61819, #69380, #74884, #62230, #10894, #62651, #17230, #4992, #48767, #4159, #30660, #10493, #18044, #82022, #42860, #68553, #11734, #75290, #29824, #55075, #80783, #82426, #24335, #50005, #36554, #74466, #63061, #10071, #3752, #81615, #23099, #75702, #42449, #18454, #43677, #5398, #23929, #37389, #31061, #17633, #56729, #68149, #4569, #24746, #81197, #23512, #49181, #30240, #43265, #68962, #11312, #35735, #76113, #50413, #44097, #61403, #29416, #52067, #32304, #32725, #13379, #76525, #12544, #31892, #58393, #25986, #57965, #38203, #45756, #51232, #38620, #70608, #39032, #76931, #64716, #25155, #63877, #7057, #70190, #77774, #753, #19258, #44911, #71452, #7482, #18853, #6216, #20107, #12963, #44500, #26414, #57553, #64298, #50823, #13800, #65146, #39458, #33152, #58821, #26829, #83244, #1178, #6632, #52487, #45339, #19680, #78195, #25566, #57136, #20526, #332, #69790, #12136, #51645, #77349, #71035, #37792, #63470, #5804, #31475, #82833, #34398, #59642, #15468, #54569, #20940, #8314, #65977, #79443, #79036, #47008, #41538, #14224, #73116, #33981, #33566, #1999, #21762, #8728, #21355, #1589, #47840, #46598, #27661, #72294, #60066, #40296, #71875, #28906, #47425, #34821, #52903, #14640, #28491, #2420, #9149, #41125, #78617, #53327, #72702, #60479, #28077, #53735, #15049, #22183, #40705, #66389, #66816, #2830, #54151, #79865, #27244, #73546, #15889, #67226, #9557, #35227, #60891, #3241, #80283, #46178, #39884, #65571, #7905, #59228, #80691, #17536, #68049, #29729, #3659, #43168, #17944, #11213, #69282, #11628, #62964, #36053, #30560, #55391, #75605, #81509, #55803, #4886, #29322, #9970, #56226, #48670, #75192, #49499, #81097, #61725, #62132, #37289, #81924, #56628, #67638, #41942, #10798, #4062, #68864, #30961, #23004, #10396, #42351, #23831, #23414, #49081, #43580, #73953, #36872, #74781, #35641, #17132, #62550, #68460, #42764, #61301, #24235, #74367, #36458, #16710, #4472, #30140, #54983, #49908, #5302, #22596, #48257, #16299, #37691, #51962, #82329, #76012, #44807, #69691, #77244, #63366, #7367, #38931, #77669, #12861, #58281, #13279, #6535, #19999, #57036, #57451, #71345, #5700, #82731, #25050, #50725, #31372, #64611, #45234, #83144, #76423, #45650, #24647, #18354, #70502, #12034, #19574, #18752, #33037, #6948, #13692, #38518, #646, #32619, #32205, #39347, #44396, #25463, #65032, #70088, #12442, #38101, #63776, #6116, #64201, #31788, #50314, #43997, #229, #70934, #51130, #76824, #26303, #57862, #19157, #25880, #51541, #1482, #20833, #21658, #14943, #21247, #27136, #34714, #40190, #27555, #59539, #2311, #65874, #53630, #14116, #52801, #27972, #59125, #66707, #79338, #8209, #33874, #60375, #79758, #7797, #78510, #9040, #1895, #33463, #47318, #46486, #53214, #39769, #73009, #54044, #15360, #22075, #47734, #15782, #72181, #2723, #78925, #28384, #34295, #8624, #41021, #65464, #46071, #73432, #14539, #41434, #67117, #46902, #72596, #40602, #9448, #58705, #1071, #20418, #78087, #66285, #59956, #26724, #52378, #71763, #80591, #54886, #68364, #67945, #35954, #30454, #3138, #62033, #22899, #22493, #48566, #10702, #80998, #10287, #73851, #36766, #9866, #74264, #61197, #17026, #29219, #80178, #48156, #24134, #16192, #30038, #56118, #23725, #81824, #49804, #75505, #16607, #43068, #42250, #4778, #36358, #4369, #17438, #41838, #67528, #68765, #3554, #55700, #81408, #61623, #3965, #74680, #17844, #11109, #69174, #35535, #54465, #23312, #29628, #49396, #43478, #55288, #48981, #42665, #75090, #62442, #35119, #60785, #28801, #39569, #31272, #82230, #56937, #45864, #58505, #69990, #50215, #14337, #69589, #82634, #37590, #77883, #5604, #56527, #24549, #1695, #26936, #58928, #12345, #75911, #65685, #11525, #5198, #868, #18250, #7595, #43892, #21050, #52598, #8012, #26526, #71984, #78304, #20215, #33676, #11935, #38001, #27353, #63263, #24947, #50620, #76325, #18655, #52180, #44299 ) ),
 .UNSPECIFIED., .F., .F., .F. ) 
 B_SPLINE_SURFACE_WITH_KNOTS ( ( 2, 2 ),
 ( 3, 2, 2, 2, 2, 2, 2, 2, 2, 2, 2, 2, 2, 2, 2, 2, 2, 2, 2, 2, 2, 2, 2, 2, 2, 2, 2, 2, 2, 2, 2, 2, 2, 2, 2, 2, 2, 2, 2, 2, 2, 2, 2, 2, 2, 2, 2, 2, 2, 2, 2, 2, 2, 2, 2, 2, 2, 2, 2, 2, 2, 2, 2, 2, 2, 2, 2, 2, 2, 2, 2, 2, 2, 2, 2, 2, 2, 2, 2, 2, 2, 2, 2, 2, 2, 2, 2, 2, 2, 2, 2, 2, 2, 2, 2, 2, 2, 2, 2, 2, 2, 2, 2, 2, 2, 2, 2, 2, 2, 2, 2, 2, 2, 2, 2, 2, 2, 2, 2, 2, 2, 2, 2, 2, 2, 2, 2, 2, 2, 2, 2, 2, 2, 2, 2, 2, 2, 2, 2, 2, 2, 2, 2, 2, 2, 2, 2, 2, 2, 2, 2, 2, 2, 2, 2, 2, 2, 2, 2, 2, 2, 2, 2, 2, 2, 2, 2, 2, 2, 2, 2, 2, 2, 2, 2, 2, 2, 2, 2, 2, 2, 2, 2, 2, 2, 2, 2, 2, 2, 2, 2, 2, 2, 2, 2, 2, 2, 2, 2, 2, 2, 2, 2, 2, 2, 2, 2, 2, 2, 2, 2, 2, 2, 2, 2, 2, 2, 2, 2, 2, 2, 2, 2, 2, 2, 2, 2, 2, 2, 2, 2, 2, 2, 2, 2, 2, 2, 2, 2, 2, 2, 2, 2, 2, 2, 2, 2, 2, 2, 2, 2, 2, 2, 2, 2, 3 ),
 ( 0.000000000000000000, 1.000000000000000000 ),
 ( 0.000000000000000000, 0.003787878787878787984, 0.007575757575757575968, 0.01136363636363636395, 0.01515151515151515194, 0.01893939393939393992, 0.02272727272727272790, 0.02651515151515151589, 0.03030303030303030387, 0.03409090909090908839, 0.03787878787878787984, 0.04166666666666666435, 0.04545454545454545581, 0.04924242424242424032, 0.05303030303030303177, 0.05681818181818181629, 0.06060606060606060774, 0.06439393939393939226, 0.06818181818181817677, 0.07196969696969697516, 0.07575757575757575968, 0.07954545454545454419, 0.08333333333333332871, 0.08712121212121212710, 0.09090909090909091161, 0.09469696969696969613, 0.09848484848484848064, 0.1022727272727272790, 0.1060606060606060635, 0.1098484848484848481, 0.1136363636363636326, 0.1174242424242424310, 0.1212121212121212155, 0.1250000000000000000, 0.1287878787878787845, 0.1325757575757575690, 0.1363636363636363535, 0.1401515151515151381, 0.1439393939393939503, 0.1477272727272727348, 0.1515151515151515194, 0.1553030303030303039, 0.1590909090909090884, 0.1628787878787878729, 0.1666666666666666574, 0.1704545454545454419, 0.1742424242424242542, 0.1780303030303030387, 0.1818181818181818232, 0.1856060606060606077, 0.1893939393939393923, 0.1931818181818181768, 0.1969696969696969613, 0.2007575757575757458, 0.2045454545454545581, 0.2083333333333333426, 0.2121212121212121271, 0.2159090909090909116, 0.2196969696969696961, 0.2234848484848484806, 0.2272727272727272652, 0.2310606060606060497, 0.2348484848484848619, 0.2386363636363636465, 0.2424242424242424310, 0.2462121212121212155, 0.2500000000000000000, 0.2537878787878787845, 0.2575757575757575690, 0.2613636363636363535, 0.2651515151515151381, 0.2689393939393939226, 0.2727272727272727071, 0.2765151515151514916, 0.2803030303030302761, 0.2840909090909091161, 0.2878787878787879007, 0.2916666666666666852, 0.2954545454545454697, 0.2992424242424242542, 0.3030303030303030387, 0.3068181818181818232, 0.3106060606060606077, 0.3143939393939393923, 0.3181818181818181768, 0.3219696969696969613, 0.3257575757575757458, 0.3295454545454545303, 0.3333333333333333148, 0.3371212121212120993, 0.3409090909090908839, 0.3446969696969697239, 0.3484848484848485084, 0.3522727272727272929, 0.3560606060606060774, 0.3598484848484848619, 0.3636363636363636465, 0.3674242424242424310, 0.3712121212121212155, 0.3750000000000000000, 0.3787878787878787845, 0.3825757575757575690, 0.3863636363636363535, 0.3901515151515151381, 0.3939393939393939226, 0.3977272727272727071, 0.4015151515151514916, 0.4053030303030302761, 0.4090909090909091161, 0.4128787878787879007, 0.4166666666666666852, 0.4204545454545454697, 0.4242424242424242542, 0.4280303030303030387, 0.4318181818181818232, 0.4356060606060606077, 0.4393939393939393923, 0.4431818181818181768, 0.4469696969696969613, 0.4507575757575757458, 0.4545454545454545303, 0.4583333333333333148, 0.4621212121212120993, 0.4659090909090908839, 0.4696969696969697239, 0.4734848484848485084, 0.4772727272727272929, 0.4810606060606060774, 0.4848484848484848619, 0.4886363636363636465, 0.4924242424242424310, 0.4962121212121212155, 0.5000000000000000000, 0.5037878787878787845, 0.5075757575757575690, 0.5113636363636363535, 0.5151515151515151381, 0.5189393939393939226, 0.5227272727272727071, 0.5265151515151514916, 0.5303030303030302761, 0.5340909090909090606, 0.5378787878787878451, 0.5416666666666666297, 0.5454545454545454142, 0.5492424242424241987, 0.5530303030303029832, 0.5568181818181817677, 0.5606060606060605522, 0.5643939393939394478, 0.5681818181818182323, 0.5719696969696970168, 0.5757575757575758013, 0.5795454545454545858, 0.5833333333333333703, 0.5871212121212121549, 0.5909090909090909394, 0.5946969696969697239, 0.5984848484848485084, 0.6022727272727272929, 0.6060606060606060774, 0.6098484848484848619, 0.6136363636363636465, 0.6174242424242424310, 0.6212121212121212155, 0.6250000000000000000, 0.6287878787878787845, 0.6325757575757575690, 0.6363636363636363535, 0.6401515151515151381, 0.6439393939393939226, 0.6477272727272727071, 0.6515151515151514916, 0.6553030303030302761, 0.6590909090909090606, 0.6628787878787878451, 0.6666666666666666297, 0.6704545454545454142, 0.6742424242424241987, 0.6780303030303029832, 0.6818181818181817677, 0.6856060606060605522, 0.6893939393939394478, 0.6931818181818182323, 0.6969696969696970168, 0.7007575757575758013, 0.7045454545454545858, 0.7083333333333333703, 0.7121212121212121549, 0.7159090909090909394, 0.7196969696969697239, 0.7234848484848485084, 0.7272727272727272929, 0.7310606060606060774, 0.7348484848484848619, 0.7386363636363636465, 0.7424242424242424310, 0.7462121212121212155, 0.7500000000000000000, 0.7537878787878787845, 0.7575757575757575690, 0.7613636363636363535, 0.7651515151515151381, 0.7689393939393939226, 0.7727272727272727071, 0.7765151515151514916, 0.7803030303030302761, 0.7840909090909090606, 0.7878787878787878451, 0.7916666666666666297, 0.7954545454545454142, 0.7992424242424241987, 0.8030303030303029832, 0.8068181818181817677, 0.8106060606060605522, 0.8143939393939394478, 0.8181818181818182323, 0.8219696969696970168, 0.8257575757575758013, 0.8295454545454545858, 0.8333333333333333703, 0.8371212121212121549, 0.8409090909090909394, 0.8446969696969697239, 0.8484848484848485084, 0.8522727272727272929, 0.8560606060606060774, 0.8598484848484848619, 0.8636363636363636465, 0.8674242424242424310, 0.8712121212121212155, 0.8750000000000000000, 0.8787878787878787845, 0.8825757575757575690, 0.8863636363636363535, 0.8901515151515151381, 0.8939393939393939226, 0.8977272727272727071, 0.9015151515151514916, 0.9053030303030302761, 0.9090909090909090606, 0.9128787878787878451, 0.9166666666666666297, 0.9204545454545454142, 0.9242424242424241987, 0.9280303030303029832, 0.9318181818181817677, 0.9356060606060605522, 0.9393939393939394478, 0.9431818181818182323, 0.9469696969696970168, 0.9507575757575758013, 0.9545454545454545858, 0.9583333333333333703, 0.9621212121212121549, 0.9659090909090909394 ),
 .UNSPECIFIED. ) 
 GEOMETRIC_REPRESENTATION_ITEM ( )  RATIONAL_B_SPLINE_SURFACE ( (
 ( 1.000000000000000000, 0.9659258262890683122, 1.000000000000000000, 0.9659258262890683122, 1.000000000000000000, 0.9659258262890683122, 1.000000000000000000, 0.9659258262890683122, 1.000000000000000000, 0.9659258262890683122, 1.000000000000000000, 0.9659258262890683122, 1.000000000000000000, 0.9659258262890683122, 1.000000000000000000, 0.9659258262890683122, 1.000000000000000000, 0.9659258262890683122, 1.000000000000000000, 0.9659258262890683122, 1.000000000000000000, 0.9659258262890683122, 1.000000000000000000, 0.9659258262890683122, 1.000000000000000000, 0.9659258262890683122, 1.000000000000000000, 0.9659258262890683122, 1.000000000000000000, 0.9659258262890683122, 1.000000000000000000, 0.9659258262890683122, 1.000000000000000000, 0.9659258262890683122, 1.000000000000000000, 0.9659258262890683122, 1.000000000000000000, 0.9659258262890683122, 1.000000000000000000, 0.9659258262890683122, 1.000000000000000000, 0.9659258262890683122, 1.000000000000000000, 0.9659258262890683122, 1.000000000000000000, 0.9659258262890683122, 1.000000000000000000, 0.9659258262890683122, 1.000000000000000000, 0.9659258262890683122, 1.000000000000000000, 0.9659258262890683122, 1.000000000000000000, 0.9659258262890683122, 1.000000000000000000, 0.9659258262890683122, 1.000000000000000000, 0.9659258262890683122, 1.000000000000000000, 0.9659258262890683122, 1.000000000000000000, 0.9659258262890683122, 1.000000000000000000, 0.9659258262890683122, 1.000000000000000000, 0.9659258262890683122, 1.000000000000000000, 0.9659258262890683122, 1.000000000000000000, 0.9659258262890683122, 1.000000000000000000, 0.9659258262890683122, 1.000000000000000000, 0.9659258262890683122, 1.000000000000000000, 0.9659258262890683122, 1.000000000000000000, 0.9659258262890683122, 1.000000000000000000, 0.9659258262890683122, 1.000000000000000000, 0.9659258262890683122, 1.000000000000000000, 0.9659258262890683122, 1.000000000000000000, 0.9659258262890683122, 1.000000000000000000, 0.9659258262890683122, 1.000000000000000000, 0.9659258262890683122, 1.000000000000000000, 0.9659258262890683122, 1.000000000000000000, 0.9659258262890683122, 1.000000000000000000, 0.9659258262890683122, 1.000000000000000000, 0.9659258262890683122, 1.000000000000000000, 0.9659258262890683122, 1.000000000000000000, 0.9659258262890683122, 1.000000000000000000, 0.9659258262890683122, 1.000000000000000000, 0.9659258262890683122, 1.000000000000000000, 0.9659258262890683122, 1.000000000000000000, 0.9659258262890683122, 1.000000000000000000, 0.9659258262890683122, 1.000000000000000000, 0.9659258262890683122, 1.000000000000000000, 0.9659258262890683122, 1.000000000000000000, 0.9659258262890683122, 1.000000000000000000, 0.9659258262890683122, 1.000000000000000000, 0.9659258262890683122, 1.000000000000000000, 0.9659258262890683122, 1.000000000000000000, 0.9659258262890683122, 1.000000000000000000, 0.9659258262890683122, 1.000000000000000000, 0.9659258262890683122, 1.000000000000000000, 0.9659258262890683122, 1.000000000000000000, 0.9659258262890683122, 1.000000000000000000, 0.9659258262890683122, 1.000000000000000000, 0.9659258262890683122, 1.000000000000000000, 0.9659258262890683122, 1.000000000000000000, 0.9659258262890683122, 1.000000000000000000, 0.9659258262890683122, 1.000000000000000000, 0.9659258262890683122, 1.000000000000000000, 0.9659258262890683122, 1.000000000000000000, 0.9659258262890683122, 1.000000000000000000, 0.9659258262890683122, 1.000000000000000000, 0.9659258262890683122, 1.000000000000000000, 0.9659258262890683122, 1.000000000000000000, 0.9659258262890683122, 1.000000000000000000, 0.9659258262890683122, 1.000000000000000000, 0.9659258262890683122, 1.000000000000000000, 0.9659258262890683122, 1.000000000000000000, 0.9659258262890683122, 1.000000000000000000, 0.9659258262890683122, 1.000000000000000000, 0.9659258262890683122, 1.000000000000000000, 0.9659258262890683122, 1.000000000000000000, 0.9659258262890683122, 1.000000000000000000, 0.9659258262890683122, 1.000000000000000000, 0.9659258262890683122, 1.000000000000000000, 0.9659258262890683122, 1.000000000000000000, 0.9659258262890683122, 1.000000000000000000, 0.9659258262890683122, 1.000000000000000000, 0.9659258262890683122, 1.000000000000000000, 0.9659258262890683122, 1.000000000000000000, 0.9659258262890683122, 1.000000000000000000, 0.9659258262890683122, 1.000000000000000000, 0.9659258262890683122, 1.000000000000000000, 0.9659258262890683122, 1.000000000000000000, 0.9659258262890683122, 1.000000000000000000, 0.9659258262890683122, 1.000000000000000000, 0.9659258262890683122, 1.000000000000000000, 0.9659258262890683122, 1.000000000000000000, 0.9659258262890683122, 1.000000000000000000, 0.9659258262890683122, 1.000000000000000000, 0.9659258262890683122, 1.000000000000000000, 0.9659258262890683122, 1.000000000000000000, 0.9659258262890683122, 1.000000000000000000, 0.9659258262890683122, 1.000000000000000000, 0.9659258262890683122, 1.000000000000000000, 0.9659258262890683122, 1.000000000000000000, 0.9659258262890683122, 1.000000000000000000, 0.9659258262890683122, 1.000000000000000000, 0.9659258262890683122, 1.000000000000000000, 0.9659258262890683122, 1.000000000000000000, 0.9659258262890683122, 1.000000000000000000, 0.9659258262890683122, 1.000000000000000000, 0.9659258262890683122, 1.000000000000000000, 0.9659258262890683122, 1.000000000000000000, 0.9659258262890683122, 1.000000000000000000, 0.9659258262890683122, 1.000000000000000000, 0.9659258262890683122, 1.000000000000000000, 0.9659258262890683122, 1.000000000000000000, 0.9659258262890683122, 1.000000000000000000, 0.9659258262890683122, 1.000000000000000000, 0.9659258262890683122, 1.000000000000000000, 0.9659258262890683122, 1.000000000000000000, 0.9659258262890683122, 1.000000000000000000, 0.9659258262890683122, 1.000000000000000000, 0.9659258262890683122, 1.000000000000000000, 0.9659258262890683122, 1.000000000000000000, 0.9659258262890683122, 1.000000000000000000, 0.9659258262890683122, 1.000000000000000000, 0.9659258262890683122, 1.000000000000000000, 0.9659258262890683122, 1.000000000000000000, 0.9659258262890683122, 1.000000000000000000, 0.9659258262890683122, 1.000000000000000000, 0.9659258262890683122, 1.000000000000000000, 0.9659258262890683122, 1.000000000000000000, 0.9659258262890683122, 1.000000000000000000, 0.9659258262890683122, 1.000000000000000000, 0.9659258262890683122, 1.000000000000000000, 0.9659258262890683122, 1.000000000000000000, 0.9659258262890683122, 1.000000000000000000, 0.9659258262890683122, 1.000000000000000000, 0.9659258262890683122, 1.000000000000000000, 0.9659258262890683122, 1.000000000000000000, 0.9659258262890683122, 1.000000000000000000, 0.9659258262890683122, 1.000000000000000000, 0.9659258262890683122, 1.000000000000000000, 0.9659258262890683122, 1.000000000000000000, 0.9659258262890683122, 1.000000000000000000, 0.9659258262890683122, 1.000000000000000000, 0.9659258262890683122, 1.000000000000000000, 0.9659258262890683122, 1.000000000000000000, 0.9659258262890683122, 1.000000000000000000, 0.9659258262890683122, 1.000000000000000000, 0.9659258262890683122, 1.000000000000000000, 0.9659258262890683122, 1.000000000000000000, 0.9659258262890683122, 1.000000000000000000, 0.9659258262890683122, 1.000000000000000000, 0.9659258262890683122, 1.000000000000000000, 0.9659258262890683122, 1.000000000000000000, 0.9659258262890683122, 1.000000000000000000, 0.9659258262890683122, 1.000000000000000000, 0.9659258262890683122, 1.000000000000000000, 0.9659258262890683122, 1.000000000000000000, 0.9659258262890683122, 1.000000000000000000, 0.9659258262890683122, 1.000000000000000000, 0.9659258262890683122, 1.000000000000000000, 0.9659258262890683122, 1.000000000000000000, 0.9659258262890683122, 1.000000000000000000, 0.9659258262890683122, 1.000000000000000000, 0.9659258262890683122, 1.000000000000000000, 0.9659258262890683122, 1.000000000000000000, 0.9659258262890683122, 1.000000000000000000, 0.9659258262890683122, 1.000000000000000000, 0.9659258262890683122, 1.000000000000000000, 0.9659258262890683122, 1.000000000000000000, 0.9659258262890683122, 1.000000000000000000, 0.9659258262890683122, 1.000000000000000000, 0.9659258262890683122, 1.000000000000000000, 0.9659258262890683122, 1.000000000000000000, 0.9659258262890683122, 1.000000000000000000, 0.9659258262890683122, 1.000000000000000000, 0.9659258262890683122, 1.000000000000000000, 0.9659258262890683122, 1.000000000000000000, 0.9659258262890683122, 1.000000000000000000, 0.9659258262890683122, 1.000000000000000000, 0.9659258262890683122, 1.000000000000000000, 0.9659258262890683122, 1.000000000000000000, 0.9659258262890683122, 1.000000000000000000, 0.9659258262890683122, 1.000000000000000000, 0.9659258262890683122, 1.000000000000000000, 0.9659258262890683122, 1.000000000000000000, 0.9659258262890683122, 1.000000000000000000, 0.9659258262890683122, 1.000000000000000000, 0.9659258262890683122, 1.000000000000000000, 0.9659258262890683122, 1.000000000000000000, 0.9659258262890683122, 1.000000000000000000, 0.9659258262890683122, 1.000000000000000000, 0.9659258262890683122, 1.000000000000000000, 0.9659258262890683122, 1.000000000000000000, 0.9659258262890683122, 1.000000000000000000, 0.9659258262890683122, 1.000000000000000000, 0.9659258262890683122, 1.000000000000000000, 0.9659258262890683122, 1.000000000000000000, 0.9659258262890683122, 1.000000000000000000, 0.9659258262890683122, 1.000000000000000000, 0.9659258262890683122, 1.000000000000000000, 0.9659258262890683122, 1.000000000000000000, 0.9659258262890683122, 1.000000000000000000, 0.9659258262890683122, 1.000000000000000000, 0.9659258262890683122, 1.000000000000000000, 0.9659258262890683122, 1.000000000000000000, 0.9659258262890683122, 1.000000000000000000, 0.9659258262890683122, 1.000000000000000000, 0.9659258262890683122, 1.000000000000000000, 0.9659258262890683122, 1.000000000000000000, 0.9659258262890683122, 1.000000000000000000, 0.9659258262890683122, 1.000000000000000000, 0.9659258262890683122, 1.000000000000000000, 0.9659258262890683122, 1.000000000000000000, 0.9659258262890683122, 1.000000000000000000, 0.9659258262890683122, 1.000000000000000000, 0.9659258262890683122, 1.000000000000000000, 0.9659258262890683122, 1.000000000000000000, 0.9659258262890683122, 1.000000000000000000, 0.9659258262890683122, 1.000000000000000000, 0.9659258262890683122, 1.000000000000000000, 0.9659258262890683122, 1.000000000000000000, 0.9659258262890683122, 1.000000000000000000, 0.9659258262890683122, 1.000000000000000000, 0.9659258262890683122, 1.000000000000000000, 0.9659258262890683122, 1.000000000000000000, 0.9659258262890683122, 1.000000000000000000, 0.9659258262890683122, 1.000000000000000000, 0.9659258262890683122, 1.000000000000000000, 0.9659258262890683122, 1.000000000000000000, 0.9659258262890683122, 1.000000000000000000, 0.9659258262890683122, 1.000000000000000000, 0.9659258262890683122, 1.000000000000000000, 0.9659258262890683122, 1.000000000000000000, 0.9659258262890683122, 1.000000000000000000, 0.9659258262890683122, 1.000000000000000000, 0.9659258262890683122, 1.000000000000000000, 0.9659258262890683122, 1.000000000000000000, 0.9659258262890683122, 1.000000000000000000, 0.9659258262890683122, 1.000000000000000000, 0.9659258262890683122, 1.000000000000000000, 0.9659258262890683122, 1.000000000000000000, 0.9659258262890683122, 1.000000000000000000, 0.9659258262890683122, 1.000000000000000000, 0.9659258262890683122, 1.000000000000000000, 0.9659258262890683122, 1.000000000000000000, 0.9659258262890683122, 1.000000000000000000),
 ( 1.000000000000000000, 0.9659258262890683122, 1.000000000000000000, 0.9659258262890683122, 1.000000000000000000, 0.9659258262890683122, 1.000000000000000000, 0.9659258262890683122, 1.000000000000000000, 0.9659258262890683122, 1.000000000000000000, 0.9659258262890683122, 1.000000000000000000, 0.9659258262890683122, 1.000000000000000000, 0.9659258262890683122, 1.000000000000000000, 0.9659258262890683122, 1.000000000000000000, 0.9659258262890683122, 1.000000000000000000, 0.9659258262890683122, 1.000000000000000000, 0.9659258262890683122, 1.000000000000000000, 0.9659258262890683122, 1.000000000000000000, 0.9659258262890683122, 1.000000000000000000, 0.9659258262890683122, 1.000000000000000000, 0.9659258262890683122, 1.000000000000000000, 0.9659258262890683122, 1.000000000000000000, 0.9659258262890683122, 1.000000000000000000, 0.9659258262890683122, 1.000000000000000000, 0.9659258262890683122, 1.000000000000000000, 0.9659258262890683122, 1.000000000000000000, 0.9659258262890683122, 1.000000000000000000, 0.9659258262890683122, 1.000000000000000000, 0.9659258262890683122, 1.000000000000000000, 0.9659258262890683122, 1.000000000000000000, 0.9659258262890683122, 1.000000000000000000, 0.9659258262890683122, 1.000000000000000000, 0.9659258262890683122, 1.000000000000000000, 0.9659258262890683122, 1.000000000000000000, 0.9659258262890683122, 1.000000000000000000, 0.9659258262890683122, 1.000000000000000000, 0.9659258262890683122, 1.000000000000000000, 0.9659258262890683122, 1.000000000000000000, 0.9659258262890683122, 1.000000000000000000, 0.9659258262890683122, 1.000000000000000000, 0.9659258262890683122, 1.000000000000000000, 0.9659258262890683122, 1.000000000000000000, 0.9659258262890683122, 1.000000000000000000, 0.9659258262890683122, 1.000000000000000000, 0.9659258262890683122, 1.000000000000000000, 0.9659258262890683122, 1.000000000000000000, 0.9659258262890683122, 1.000000000000000000, 0.9659258262890683122, 1.000000000000000000, 0.9659258262890683122, 1.000000000000000000, 0.9659258262890683122, 1.000000000000000000, 0.9659258262890683122, 1.000000000000000000, 0.9659258262890683122, 1.000000000000000000, 0.9659258262890683122, 1.000000000000000000, 0.9659258262890683122, 1.000000000000000000, 0.9659258262890683122, 1.000000000000000000, 0.9659258262890683122, 1.000000000000000000, 0.9659258262890683122, 1.000000000000000000, 0.9659258262890683122, 1.000000000000000000, 0.9659258262890683122, 1.000000000000000000, 0.9659258262890683122, 1.000000000000000000, 0.9659258262890683122, 1.000000000000000000, 0.9659258262890683122, 1.000000000000000000, 0.9659258262890683122, 1.000000000000000000, 0.9659258262890683122, 1.000000000000000000, 0.9659258262890683122, 1.000000000000000000, 0.9659258262890683122, 1.000000000000000000, 0.9659258262890683122, 1.000000000000000000, 0.9659258262890683122, 1.000000000000000000, 0.9659258262890683122, 1.000000000000000000, 0.9659258262890683122, 1.000000000000000000, 0.9659258262890683122, 1.000000000000000000, 0.9659258262890683122, 1.000000000000000000, 0.9659258262890683122, 1.000000000000000000, 0.9659258262890683122, 1.000000000000000000, 0.9659258262890683122, 1.000000000000000000, 0.9659258262890683122, 1.000000000000000000, 0.9659258262890683122, 1.000000000000000000, 0.9659258262890683122, 1.000000000000000000, 0.9659258262890683122, 1.000000000000000000, 0.9659258262890683122, 1.000000000000000000, 0.9659258262890683122, 1.000000000000000000, 0.9659258262890683122, 1.000000000000000000, 0.9659258262890683122, 1.000000000000000000, 0.9659258262890683122, 1.000000000000000000, 0.9659258262890683122, 1.000000000000000000, 0.9659258262890683122, 1.000000000000000000, 0.9659258262890683122, 1.000000000000000000, 0.9659258262890683122, 1.000000000000000000, 0.9659258262890683122, 1.000000000000000000, 0.9659258262890683122, 1.000000000000000000, 0.9659258262890683122, 1.000000000000000000, 0.9659258262890683122, 1.000000000000000000, 0.9659258262890683122, 1.000000000000000000, 0.9659258262890683122, 1.000000000000000000, 0.9659258262890683122, 1.000000000000000000, 0.9659258262890683122, 1.000000000000000000, 0.9659258262890683122, 1.000000000000000000, 0.9659258262890683122, 1.000000000000000000, 0.9659258262890683122, 1.000000000000000000, 0.9659258262890683122, 1.000000000000000000, 0.9659258262890683122, 1.000000000000000000, 0.9659258262890683122, 1.000000000000000000, 0.9659258262890683122, 1.000000000000000000, 0.9659258262890683122, 1.000000000000000000, 0.9659258262890683122, 1.000000000000000000, 0.9659258262890683122, 1.000000000000000000, 0.9659258262890683122, 1.000000000000000000, 0.9659258262890683122, 1.000000000000000000, 0.9659258262890683122, 1.000000000000000000, 0.9659258262890683122, 1.000000000000000000, 0.9659258262890683122, 1.000000000000000000, 0.9659258262890683122, 1.000000000000000000, 0.9659258262890683122, 1.000000000000000000, 0.9659258262890683122, 1.000000000000000000, 0.9659258262890683122, 1.000000000000000000, 0.9659258262890683122, 1.000000000000000000, 0.9659258262890683122, 1.000000000000000000, 0.9659258262890683122, 1.000000000000000000, 0.9659258262890683122, 1.000000000000000000, 0.9659258262890683122, 1.000000000000000000, 0.9659258262890683122, 1.000000000000000000, 0.9659258262890683122, 1.000000000000000000, 0.9659258262890683122, 1.000000000000000000, 0.9659258262890683122, 1.000000000000000000, 0.9659258262890683122, 1.000000000000000000, 0.9659258262890683122, 1.000000000000000000, 0.9659258262890683122, 1.000000000000000000, 0.9659258262890683122, 1.000000000000000000, 0.9659258262890683122, 1.000000000000000000, 0.9659258262890683122, 1.000000000000000000, 0.9659258262890683122, 1.000000000000000000, 0.9659258262890683122, 1.000000000000000000, 0.9659258262890683122, 1.000000000000000000, 0.9659258262890683122, 1.000000000000000000, 0.9659258262890683122, 1.000000000000000000, 0.9659258262890683122, 1.000000000000000000, 0.9659258262890683122, 1.000000000000000000, 0.9659258262890683122, 1.000000000000000000, 0.9659258262890683122, 1.000000000000000000, 0.9659258262890683122, 1.000000000000000000, 0.9659258262890683122, 1.000000000000000000, 0.9659258262890683122, 1.000000000000000000, 0.9659258262890683122, 1.000000000000000000, 0.9659258262890683122, 1.000000000000000000, 0.9659258262890683122, 1.000000000000000000, 0.9659258262890683122, 1.000000000000000000, 0.9659258262890683122, 1.000000000000000000, 0.9659258262890683122, 1.000000000000000000, 0.9659258262890683122, 1.000000000000000000, 0.9659258262890683122, 1.000000000000000000, 0.9659258262890683122, 1.000000000000000000, 0.9659258262890683122, 1.000000000000000000, 0.9659258262890683122, 1.000000000000000000, 0.9659258262890683122, 1.000000000000000000, 0.9659258262890683122, 1.000000000000000000, 0.9659258262890683122, 1.000000000000000000, 0.9659258262890683122, 1.000000000000000000, 0.9659258262890683122, 1.000000000000000000, 0.9659258262890683122, 1.000000000000000000, 0.9659258262890683122, 1.000000000000000000, 0.9659258262890683122, 1.000000000000000000, 0.9659258262890683122, 1.000000000000000000, 0.9659258262890683122, 1.000000000000000000, 0.9659258262890683122, 1.000000000000000000, 0.9659258262890683122, 1.000000000000000000, 0.9659258262890683122, 1.000000000000000000, 0.9659258262890683122, 1.000000000000000000, 0.9659258262890683122, 1.000000000000000000, 0.9659258262890683122, 1.000000000000000000, 0.9659258262890683122, 1.000000000000000000, 0.9659258262890683122, 1.000000000000000000, 0.9659258262890683122, 1.000000000000000000, 0.9659258262890683122, 1.000000000000000000, 0.9659258262890683122, 1.000000000000000000, 0.9659258262890683122, 1.000000000000000000, 0.9659258262890683122, 1.000000000000000000, 0.9659258262890683122, 1.000000000000000000, 0.9659258262890683122, 1.000000000000000000, 0.9659258262890683122, 1.000000000000000000, 0.9659258262890683122, 1.000000000000000000, 0.9659258262890683122, 1.000000000000000000, 0.9659258262890683122, 1.000000000000000000, 0.9659258262890683122, 1.000000000000000000, 0.9659258262890683122, 1.000000000000000000, 0.9659258262890683122, 1.000000000000000000, 0.9659258262890683122, 1.000000000000000000, 0.9659258262890683122, 1.000000000000000000, 0.9659258262890683122, 1.000000000000000000, 0.9659258262890683122, 1.000000000000000000, 0.9659258262890683122, 1.000000000000000000, 0.9659258262890683122, 1.000000000000000000, 0.9659258262890683122, 1.000000000000000000, 0.9659258262890683122, 1.000000000000000000, 0.9659258262890683122, 1.000000000000000000, 0.9659258262890683122, 1.000000000000000000, 0.9659258262890683122, 1.000000000000000000, 0.9659258262890683122, 1.000000000000000000, 0.9659258262890683122, 1.000000000000000000, 0.9659258262890683122, 1.000000000000000000, 0.9659258262890683122, 1.000000000000000000, 0.9659258262890683122, 1.000000000000000000, 0.9659258262890683122, 1.000000000000000000, 0.9659258262890683122, 1.000000000000000000, 0.9659258262890683122, 1.000000000000000000, 0.9659258262890683122, 1.000000000000000000, 0.9659258262890683122, 1.000000000000000000, 0.9659258262890683122, 1.000000000000000000, 0.9659258262890683122, 1.000000000000000000, 0.9659258262890683122, 1.000000000000000000, 0.9659258262890683122, 1.000000000000000000, 0.9659258262890683122, 1.000000000000000000, 0.9659258262890683122, 1.000000000000000000, 0.9659258262890683122, 1.000000000000000000, 0.9659258262890683122, 1.000000000000000000, 0.9659258262890683122, 1.000000000000000000, 0.9659258262890683122, 1.000000000000000000, 0.9659258262890683122, 1.000000000000000000, 0.9659258262890683122, 1.000000000000000000, 0.9659258262890683122, 1.000000000000000000, 0.9659258262890683122, 1.000000000000000000, 0.9659258262890683122, 1.000000000000000000, 0.9659258262890683122, 1.000000000000000000, 0.9659258262890683122, 1.000000000000000000, 0.9659258262890683122, 1.000000000000000000, 0.9659258262890683122, 1.000000000000000000, 0.9659258262890683122, 1.000000000000000000, 0.9659258262890683122, 1.000000000000000000, 0.9659258262890683122, 1.000000000000000000, 0.9659258262890683122, 1.000000000000000000, 0.9659258262890683122, 1.000000000000000000, 0.9659258262890683122, 1.000000000000000000, 0.9659258262890683122, 1.000000000000000000, 0.9659258262890683122, 1.000000000000000000, 0.9659258262890683122, 1.000000000000000000, 0.9659258262890683122, 1.000000000000000000, 0.9659258262890683122, 1.000000000000000000, 0.9659258262890683122, 1.000000000000000000, 0.9659258262890683122, 1.000000000000000000, 0.9659258262890683122, 1.000000000000000000, 0.9659258262890683122, 1.000000000000000000, 0.9659258262890683122, 1.000000000000000000, 0.9659258262890683122, 1.000000000000000000, 0.9659258262890683122, 1.000000000000000000, 0.9659258262890683122, 1.000000000000000000, 0.9659258262890683122, 1.000000000000000000, 0.9659258262890683122, 1.000000000000000000, 0.9659258262890683122, 1.000000000000000000, 0.9659258262890683122, 1.000000000000000000, 0.9659258262890683122, 1.000000000000000000, 0.9659258262890683122, 1.000000000000000000, 0.9659258262890683122, 1.000000000000000000, 0.9659258262890683122, 1.000000000000000000, 0.9659258262890683122, 1.000000000000000000, 0.9659258262890683122, 1.000000000000000000, 0.9659258262890683122, 1.000000000000000000, 0.9659258262890683122, 1.000000000000000000, 0.9659258262890683122, 1.000000000000000000, 0.9659258262890683122, 1.000000000000000000, 0.9659258262890683122, 1.000000000000000000, 0.9659258262890683122, 1.000000000000000000) ) ) 
 REPRESENTATION_ITEM ( '' )  SURFACE ( )  );
#45573 = CARTESIAN_POINT ( 'NONE',  ( -1.482939632545930975, -0.004921259842519576551, 0.3153832671262227771 ) ) ;
#45574 = CARTESIAN_POINT ( 'NONE',  ( -0.4002624671916004129, -0.2845877964562159024, 0.3641732283464567677 ) ) ;
#45575 = CARTESIAN_POINT ( 'NONE',  ( -1.528871391076114250, 0.1771653543307087075, -0.09757992244046823083 ) ) ;
#45576 = CARTESIAN_POINT ( 'NONE',  ( 0.9842519685039375910, 0.1771653543307087630, 0.000000000000000000 ) ) ;
#45577 = CARTESIAN_POINT ( 'NONE',  ( 0.6561679790026253567, -0.6046776061558809534, -0.2411417322834644161 ) ) ;
#45578 = CARTESIAN_POINT ( 'NONE',  ( 1.299212598425197429, 0.2952755905511811885, 0.000000000000000000 ) ) ;
#45579 = CARTESIAN_POINT ( 'NONE',  ( 0.05249343832021075018, -0.6046776061558807314, 0.2411417322834647770 ) ) ;
#45580 = CARTESIAN_POINT ( 'NONE',  ( 0.5446194225721792126, -0.08942795157528024563, -0.3641732283464568787 ) ) ;
#45581 = CARTESIAN_POINT ( 'NONE',  ( 1.509186351706037543, -0.4281496062992127816, -0.4176697321401328100 ) ) ;
#45582 = CARTESIAN_POINT ( 'NONE',  ( 1.586052503253845503, 1.023622047244095556, 0.1653254495020588799 ) ) ;
#45583 = CARTESIAN_POINT ( 'NONE',  ( -0.4593175853018366950, 0.05413385826771666132, 0.4176697321401328100 ) ) ;
#45584 = CARTESIAN_POINT ( 'NONE',  ( -0.3996062992125986035, -7.340648628747425578E-17, -0.5118110236220472231 ) ) ;
#45585 = CARTESIAN_POINT ( 'NONE',  ( -2.787279214012418738, 0.000000000000000000, 0.000000000000000000 ) ) ;
#45586 = CARTESIAN_POINT ( 'NONE',  ( 0.1640419947506569498, -0.05778040916215522460, 0.4822834645669289988 ) ) ;
#45587 = CARTESIAN_POINT ( 'NONE',  ( -0.4724409448818890911, -0.1870078740157480879, -0.4822834645669291653 ) ) ;
#45589 = AXIS2_PLACEMENT_3D ( 'NONE', #67472, #47680, #54829 ) ;
#45588 = CARTESIAN_POINT ( 'NONE',  ( 0.04593175853018440641, 0.2952755905511810774, -0.1292274648535930714 ) ) ;
#45590 = CARTESIAN_POINT ( 'NONE',  ( 0.3996062992125986035, 0.1070741851644054776, -2.801837270341207553 ) ) ;
#45591 = CARTESIAN_POINT ( 'NONE',  ( 0.3949938075777409963, 2.418639510665530435E-17, -2.007874015748031482 ) ) ;
#45592 = CARTESIAN_POINT ( 'NONE',  ( 0.2867679344610365999, -0.2867679344610365444, -0.5629921259842519676 ) ) ;
#45593 = CARTESIAN_POINT ( 'NONE',  ( 0.2596916824146294211, -0.1407161764240515978, 5.810203857714901332 ) ) ;
#45594 = CARTESIAN_POINT ( 'NONE',  ( 0.2867679344610366554, -0.2867679344610365444, -0.8779527559055116948 ) ) ;
#45595 = CARTESIAN_POINT ( 'NONE',  ( -1.030183727034119867, -0.08942795157528024563, -0.3641732283464568787 ) ) ;
#45596 = CARTESIAN_POINT ( 'NONE',  ( 0.3917322834645670104, 2.398668435337828261E-17, -0.8976377952755905110 ) ) ;
#45597 = CARTESIAN_POINT ( 'NONE',  ( -1.122047244094487306, -0.5400638737290844871, 0.3530559997133364547 ) ) ;
#45598 = CARTESIAN_POINT ( 'NONE',  ( -0.3949938075777408852, -0.1058382717557502933, -2.799868766404199683 ) ) ;
#45599 = CARTESIAN_POINT ( 'NONE',  ( 0.5511811023622055217, -0.1870078740157479769, 0.4822834645669291653 ) ) ;
#45600 = CARTESIAN_POINT ( 'NONE',  ( -0.1509186351706028884, -0.08942795157527998196, 0.3641732283464567121 ) ) ;
#45601 = CARTESIAN_POINT ( 'NONE',  ( 1.318897637795276356, 0.1660481256975883668, -0.3530559997133364547 ) ) ;
#45602 = CARTESIAN_POINT ( 'NONE',  ( 0.2755905511811031494, -0.6692913385826771977, 8.415575281601705876E-17 ) ) ;
#45603 = CARTESIAN_POINT ( 'NONE',  ( -0.4744094488188895231, 1.546135192374304745, -2.170146923806595574 ) ) ;
#45604 = CARTESIAN_POINT ( 'NONE',  ( -0.1070741851644056997, 0.3996062992125986035, -2.683727034120735322 ) ) ;
#45605 = CARTESIAN_POINT ( 'NONE',  ( 0.3917322834645670659, -0.1049643490035303273, -1.053168922081052283 ) ) ;
#45606 = CARTESIAN_POINT ( 'NONE',  ( 1.122047244094488860, -0.5400638737290845981, -0.3530559997133363437 ) ) ;
#45607 = CARTESIAN_POINT ( 'NONE',  ( 0.4396325459317590445, -0.6692913385826771977, 0.1292274648535927661 ) ) ;
#45608 = EDGE_CURVE ( 'NONE', #9070, #7002, #29244, .T. ) ;
#45609 = CARTESIAN_POINT ( 'NONE',  ( 0.2493438320209980519, -0.4281496062992127816, -0.4176697321401328100 ) ) ;
#45610 = CARTESIAN_POINT ( 'NONE',  ( 1.443569553805774897, -0.6046776061558809534, -0.2411417322834644161 ) ) ;
#45611 = CARTESIAN_POINT ( 'NONE',  ( -0.1958661417322836718, 0.3392501089628017219, -0.7276902887139108378 ) ) ;
#45612 = CARTESIAN_POINT ( 'NONE',  ( -0.09186351706036689768, 0.05413385826771626580, -0.4176697321401330321 ) ) ;
#45613 = CARTESIAN_POINT ( 'NONE',  ( 0.9580052493438327987, -0.4281496062992127816, -0.4176697321401328100 ) ) ;
#45614 = CARTESIAN_POINT ( 'NONE',  ( 0.4265091863517067594, 0.2952755905511811885, 0.1292274648535926551 ) ) ;
#45615 = CARTESIAN_POINT ( 'NONE',  ( 1.010498687664042716, -0.3690944881889763329, 0.3153832671262228327 ) ) ;
#45616 = CARTESIAN_POINT ( 'NONE',  ( -1.056430446194224881, 0.2952755905511810774, -0.1292274648535930714 ) ) ;
#45617 = CARTESIAN_POINT ( 'NONE',  ( -1.305774278215222184, -0.6692913385826773087, -0.1292274648535924053 ) ) ;
#45618 = CARTESIAN_POINT ( 'NONE',  ( 0.6889763779527563470, 0.1660481256975883668, -0.3530559997133364547 ) ) ;
#45619 = CARTESIAN_POINT ( 'NONE',  ( 0.02544847934575847695, -0.3910482532978202808, -1.929133858267716439 ) ) ;
#45620 = CARTESIAN_POINT ( 'NONE',  ( -0.1049643490035307020, 0.3917322834645669549, -1.730971128608923992 ) ) ;
#45621 = CARTESIAN_POINT ( 'NONE',  ( 1.535433070866142558, 0.2952755905511811885, 0.000000000000000000 ) ) ;
#45622 = ORIENTED_EDGE ( 'NONE', *, *, #48595, .T. ) ;
#45623 = CARTESIAN_POINT ( 'NONE',  ( -0.2925321140481930704, -0.2925321140481933480, 0.09842519685039367860 ) ) ;
#45624 = ORIENTED_EDGE ( 'NONE', *, *, #20141, .F. ) ;
#45625 = CARTESIAN_POINT ( 'NONE',  ( 1.358267716535433323, 0.1660481256975885056, 0.3530559997133364547 ) ) ;
#45626 = CARTESIAN_POINT ( 'NONE',  ( 0.9908136482939640111, 0.1771653543307087075, -0.09757992244046823083 ) ) ;
#45627 = FACE_OUTER_BOUND ( 'NONE', #28740, .T. ) ;
#45628 = CARTESIAN_POINT ( 'NONE',  ( -0.3013144171194466203, 1.169708940200700820, 2.776959576054383927 ) ) ;
#45629 = CARTESIAN_POINT ( 'NONE',  ( -1.614173228346457378, 0.2753471884572478157, -0.1372047244094478091 ) ) ;
#45630 = CARTESIAN_POINT ( 'NONE',  ( 0.1958661417322834775, 0.3392501089628018884, -0.8589238845144357981 ) ) ;
#45631 = CARTESIAN_POINT ( 'NONE',  ( -1.286089238845143479, 0.1283753931104746893, -0.1820866141732285504 ) ) ;
#45632 = CARTESIAN_POINT ( 'NONE',  ( -1.732283464566928277, -0.1870078740157479769, 0.3641732283464567677 ) ) ;
#45633 = CYLINDRICAL_SURFACE ( 'NONE', #4953, 0.3149606299212598381 ) ;
#45634 = CARTESIAN_POINT ( 'NONE',  ( -0.3215223097112853146, -0.3162353388693405765, 0.4822834645669290543 ) ) ;
#45635 = CARTESIAN_POINT ( 'NONE',  ( 1.463254593175853824, 0.2952755905511810774, -0.1292274648535930714 ) ) ;
#45636 = ORIENTED_EDGE ( 'NONE', *, *, #6668, .T. ) ;
#45637 = CARTESIAN_POINT ( 'NONE',  ( -0.7186703366786194591, -2.567464376874931580E-15, -0.4445507791589072832 ) ) ;
#45638 =( NAMED_UNIT ( * ) PLANE_ANGLE_UNIT ( ) SI_UNIT ( $, .RADIAN. ) );
#45639 = CARTESIAN_POINT ( 'NONE',  ( 0.1265901696524989184, 0.4724409448818898127, -2.670603674540682260 ) ) ;
#45640 = CARTESIAN_POINT ( 'NONE',  ( -1.603475055217291612, 1.881749232079046097, 0.04573490813648253134 ) ) ;
#45641 = CARTESIAN_POINT ( 'NONE',  ( -1.036745406824146176, -0.3690944881889763329, 0.3153832671262228327 ) ) ;
#45642 = CARTESIAN_POINT ( 'NONE',  ( -1.509186351706035767, -0.4281496062992124485, 0.4176697321401328655 ) ) ;
#45643 = CARTESIAN_POINT ( 'NONE',  ( 0.4527559055118117182, 0.1660481256975883668, -0.3530559997133364547 ) ) ;
#45644 = EDGE_LOOP ( 'NONE', ( #5461, #47919, #6555, #63634 ) ) ;
#45646 = DIRECTION ( 'NONE',  ( -8.673617379884022653E-16, 1.000000000000000000, -3.028377322213053966E-30 ) ) ;
#45645 = DIRECTION ( 'NONE',  ( 0.000000000000000000, -1.000000000000000000, -0.000000000000000000 ) ) ;
#45647 = CARTESIAN_POINT ( 'NONE',  ( 1.187664041994751285, -0.05778040916215522460, 0.4822834645669289988 ) ) ;
#45648 = CARTESIAN_POINT ( 'NONE',  ( 1.561679790026247350, -0.3690944881889763329, 0.3153832671262228327 ) ) ;
#45649 = CARTESIAN_POINT ( 'NONE',  ( -0.2867679344610366554, 0.2867679344610365444, -0.8871197918297093477 ) ) ;
#45650 = CARTESIAN_POINT ( 'NONE',  ( -0.3608923884514428360, -0.5511811023622048555, -0.09757992244046775898 ) ) ;
#45651 = CARTESIAN_POINT ( 'NONE',  ( -1.640419947506561060, -0.004921259842519576551, 0.3153832671262227771 ) ) ;
#45652 = FACE_OUTER_BOUND ( 'NONE', #67175, .T. ) ;
#45653 = CARTESIAN_POINT ( 'NONE',  ( 0.3149606299212603933, -0.1870078740157479769, 0.4822834645669291653 ) ) ;
#45654 = CARTESIAN_POINT ( 'NONE',  ( -0.4921259842519677963, 0.07958543189024071263, -0.2665933059059888421 ) ) ;
#45655 = CARTESIAN_POINT ( 'NONE',  ( 0.05249343832021075018, 0.1283753931104746893, -0.1820866141732285504 ) ) ;
#45656 = CARTESIAN_POINT ( 'NONE',  ( 0.2952755905511816326, -0.5400638737290844871, 0.3530559997133364547 ) ) ;
#45657 = CARTESIAN_POINT ( 'NONE',  ( -1.233595800524933894, -0.5023911411419708095, -0.1820866141732282451 ) ) ;
#45658 = CARTESIAN_POINT ( 'NONE',  ( -0.2867679344610365444, -0.2867679344610367664, 0.1016867209635676783 ) ) ;
#45659 = CARTESIAN_POINT ( 'NONE',  ( 0.8464566929133865436, 0.1660481256975883668, -0.3530559997133364547 ) ) ;
#45660 = CARTESIAN_POINT ( 'NONE',  ( -1.489501312335957062, -0.05778040916215522460, 0.4822834645669289988 ) ) ;
#45661 = CARTESIAN_POINT ( 'NONE',  ( -0.4724409448818898682, -8.678599364036362592E-17, -1.218503937007874072 ) ) ;
#45662 = CARTESIAN_POINT ( 'NONE',  ( -0.4593175853018366950, 0.05413385826771666132, 0.4176697321401328100 ) ) ;
#45663 = CARTESIAN_POINT ( 'NONE',  ( 0.2952755905511816326, -0.4536011799217367080, 0.2665933059059888421 ) ) ;
#45664 = CARTESIAN_POINT ( 'NONE',  ( -1.082677165354329896, -0.5400638737290845981, -0.3530559997133363437 ) ) ;
#45665 = CARTESIAN_POINT ( 'NONE',  ( 0.7874015748031503170, -0.1870078740157480601, -0.3641732283464567677 ) ) ;
#45666 = CARTESIAN_POINT ( 'NONE',  ( -0.1706036745406816491, -0.3690944881889763329, 0.3153832671262228327 ) ) ;
#45667 = CARTESIAN_POINT ( 'NONE',  ( -0.6627296587926503335, -0.6692913385826771977, 0.1292274648535927661 ) ) ;
#45668 = CARTESIAN_POINT ( 'NONE',  ( -1.568241469816272105, -0.3162353388693409650, -0.4822834645669289433 ) ) ;
#45669 = DIRECTION ( 'NONE',  ( 1.000000000000000000, 0.000000000000000000, 0.000000000000000000 ) ) ;
#45670 = CARTESIAN_POINT ( 'NONE',  ( 1.443569553805774897, -0.5023911411419708095, -0.1820866141732282451 ) ) ;
#45671 = CARTESIAN_POINT ( 'NONE',  ( 0.3740157480314966754, -0.5400638737290844871, 0.3530559997133364547 ) ) ;
#45672 = CARTESIAN_POINT ( 'NONE',  ( -1.614173228346455824, 0.2952755905511811885, 0.000000000000000000 ) ) ;
#45673 = CARTESIAN_POINT ( 'NONE',  ( -1.502624671916009680, -0.05778040916215560624, -0.4822834645669293319 ) ) ;
#45674 = ORIENTED_EDGE ( 'NONE', *, *, #83038, .T. ) ;
#45675 = CARTESIAN_POINT ( 'NONE',  ( -9.787531504996566615E-17, 0.3996062992125985480, -2.596456692913385655 ) ) ;
#45676 = CARTESIAN_POINT ( 'NONE',  ( -0.9645669291338575535, 0.07958543189024071263, -0.2665933059059888421 ) ) ;
#45677 = CARTESIAN_POINT ( 'NONE',  ( 0.8005249343832027131, 0.05413385826771666132, 0.4176697321401328100 ) ) ;
#45678 = CARTESIAN_POINT ( 'NONE',  ( -0.9448818897637790704, -0.1870078740157479769, 0.3641732283464567677 ) ) ;
#45679 = CARTESIAN_POINT ( 'NONE',  ( 0.3996062992125984925, 0.1070741851644054637, -1.933727034120735100 ) ) ;
#45680 = CARTESIAN_POINT ( 'NONE',  ( -1.049868766404198794, 0.2306618581243847221, -0.2411417322834647770 ) ) ;
#45681 = CARTESIAN_POINT ( 'NONE',  ( 1.043307086614173818, 0.1660481256975885056, 0.3530559997133364547 ) ) ;
#45682 = CARTESIAN_POINT ( 'NONE',  ( 0.4790026246719168435, -0.3162353388693409650, -0.4822834645669289433 ) ) ;
#45683 = CARTESIAN_POINT ( 'NONE',  ( 1.476377952755906220, 0.1660481256975883668, -0.3530559997133364547 ) ) ;
#45684 = CARTESIAN_POINT ( 'NONE',  ( -1.692913385826770645, 0.1771653543307087630, 0.000000000000000000 ) ) ;
#45685 = CARTESIAN_POINT ( 'NONE',  ( -0.1070741851644057135, 0.3996062992125984925, -1.028215223097112663 ) ) ;
#45686 = CARTESIAN_POINT ( 'NONE',  ( 0.1070741851644053527, 0.3996062992125986590, -1.253280839895013044 ) ) ;
#45687 = CARTESIAN_POINT ( 'NONE',  ( 0.1058382717557499880, 0.3949938075777411073, -0.6233595800524935893 ) ) ;
#45688 = DIRECTION ( 'NONE',  ( -0.000000000000000000, 1.000000000000000000, -0.000000000000000000 ) ) ;
#45689 = CARTESIAN_POINT ( 'NONE',  ( 0.5511811023622055217, -0.1870078740157479769, 0.3641732283464567677 ) ) ;
#45690 = CARTESIAN_POINT ( 'NONE',  ( 0.3280839895013130669, -0.004921259842519576551, 0.3153832671262227771 ) ) ;
#45691 = CARTESIAN_POINT ( 'NONE',  ( 0.1706036745406830368, 0.05413385826771666132, 0.4176697321401328100 ) ) ;
#45692 = CARTESIAN_POINT ( 'NONE',  ( 1.437007874015748810, 0.1660481256975885056, 0.3530559997133364547 ) ) ;
#45693 = CARTESIAN_POINT ( 'NONE',  ( -0.2891555358219911054, 0.2891555358219909388, -1.671259842519685179 ) ) ;
#45694 = CARTESIAN_POINT ( 'NONE',  ( 0.4199475065616805614, 0.1283753931104748280, 0.1820866141732283561 ) ) ;
#45695 =( BOUNDED_CURVE ( )  B_SPLINE_CURVE ( 2, ( #41534, #28073, #21758, #47421, #53322, #52899, #9553, #14636, #20522, #35223, #15045, #53731, #47836 ),
 .UNSPECIFIED., .F., .F. ) 
 B_SPLINE_CURVE_WITH_KNOTS ( ( 3, 2, 2, 2, 2, 2, 3 ),
 ( 0.6740332660251416863, 0.6742424242424241987, 0.6780303030303029832, 0.6818181818181817677, 0.6856060606060605522, 0.6893939393939394478, 0.6896030976112219602 ),
 .UNSPECIFIED. ) 
 CURVE ( )  GEOMETRIC_REPRESENTATION_ITEM ( )  RATIONAL_B_SPLINE_CURVE ( ( 0.9964447847208419695, 0.9981185001348091834, 1.000000000000000000, 0.9659258262890683122, 1.000000000000000000, 0.9659258262890683122, 1.000000000000000000, 0.9659258262890683122, 1.000000000000000000, 0.9659258262890683122, 1.000000000000000000, 0.9981185001348091834, 0.9964447847208420805 ) ) 
 REPRESENTATION_ITEM ( '' )  );
#45696 = CARTESIAN_POINT ( 'NONE',  ( -0.7677165354330699465, -0.5400638737290845981, -0.3530559997133363437 ) ) ;
#45697 = CARTESIAN_POINT ( 'NONE',  ( -1.450131233595799651, 0.2952755905511810774, -0.1292274648535930714 ) ) ;
#45698 = CARTESIAN_POINT ( 'NONE',  ( 0.7874015748031503170, -0.1870078740157480879, -0.4822834645669291653 ) ) ;
#45699 = CARTESIAN_POINT ( 'NONE',  ( -0.1265901696524986964, -0.4724409448818899238, -1.489501312335957950 ) ) ;
#45700 = CARTESIAN_POINT ( 'NONE',  ( 0.1123167701215799369, 0.3758920641862485423, -2.755905511811022279 ) ) ;
#45701 = ORIENTED_EDGE ( 'NONE', *, *, #24294, .F. ) ;
#45702 = EDGE_CURVE ( 'NONE', #74865, #41210, #61223, .T. ) ;
#45703 = ORIENTED_EDGE ( 'NONE', *, *, #26367, .T. ) ;
#45704 = CARTESIAN_POINT ( 'NONE',  ( -1.417322834645668772, -0.1870078740157479769, 0.4822834645669291653 ) ) ;
#45705 = CARTESIAN_POINT ( 'NONE',  ( -1.207349081364828436, -0.6046776061558807314, 0.2411417322834647770 ) ) ;
#45707 = CARTESIAN_POINT ( 'NONE',  ( -0.6233595800524928121, -0.3162353388693409650, -0.4822834645669289433 ) ) ;
#45706 = CARTESIAN_POINT ( 'NONE',  ( -0.7611548556430438595, -0.5023911411419708095, -0.1820866141732282451 ) ) ;
#45708 = CARTESIAN_POINT ( 'NONE',  ( -0.1049643490035306742, 0.3917322834645668994, -2.133838951934696304 ) ) ;
#45709 = CARTESIAN_POINT ( 'NONE',  ( -0.4624320255261038515, -2.191421614605370878E-15, 0.4445507791589071167 ) ) ;
#45710 = CARTESIAN_POINT ( 'NONE',  ( -1.594488188976377119, 0.07958543189024071263, -0.2665933059059888421 ) ) ;
#45711 = CARTESIAN_POINT ( 'NONE',  ( -1.417322834645668772, -0.1870078740157479769, 0.4822834645669291653 ) ) ;
#45712 = CARTESIAN_POINT ( 'NONE',  ( 0.2755905511811031494, -0.6692913385826771977, 8.415575281601705876E-17 ) ) ;
#45713 = CARTESIAN_POINT ( 'NONE',  ( -0.9383202099737524282, -0.3162353388693409650, -0.4822834645669289433 ) ) ;
#45714 = CARTESIAN_POINT ( 'NONE',  ( -0.3917322834645670104, -7.196005306013484475E-17, 0.1909448818897636901 ) ) ;
#45715 = CARTESIAN_POINT ( 'NONE',  ( 0.5971128608923890191, -0.6692913385826771977, 0.1292274648535927661 ) ) ;
#45716 = CARTESIAN_POINT ( 'NONE',  ( 4.797336870675656522E-17, -0.3917322834645670104, -1.330708661417322691 ) ) ;
#45717 = CARTESIAN_POINT ( 'NONE',  ( -0.7480314960629914633, -0.5511811023622047445, 6.969142054262312111E-17 ) ) ;
#45718 = EDGE_LOOP ( 'NONE', ( #12488, #33901, #37957, #72275, #63945 ) ) ;
#45719 = CARTESIAN_POINT ( 'NONE',  ( -0.3420746716998659953, -0.1974969037888706647, -1.784776902887138972 ) ) ;
#45720 = ORIENTED_EDGE ( 'NONE', *, *, #44425, .T. ) ;
#45721 = CARTESIAN_POINT ( 'NONE',  ( -1.673228346456691717, 0.07958543189024071263, -0.2665933059059888421 ) ) ;
#45722 = CARTESIAN_POINT ( 'NONE',  ( -0.9383202099737524282, -0.05778040916215522460, 0.4822834645669289988 ) ) ;
#45723 = CARTESIAN_POINT ( 'NONE',  ( -1.391076115485563314, -0.6046776061558809534, -0.2411417322834644161 ) ) ;
#45724 = CARTESIAN_POINT ( 'NONE',  ( -0.1070741851644056997, 0.3996062992125986035, -0.6364829396325458744 ) ) ;
#45725 = CARTESIAN_POINT ( 'NONE',  ( -1.299212598425196097, -0.6692913385826771977, 8.415575281601705876E-17 ) ) ;
#45726 = CARTESIAN_POINT ( 'NONE',  ( -1.463254593175852492, -0.6692913385826773087, -0.1292274648535924053 ) ) ;
#45727 = CARTESIAN_POINT ( 'NONE',  ( -1.391076115485563314, -0.6046776061558809534, -0.2411417322834644161 ) ) ;
#45728 =( NAMED_UNIT ( * ) PLANE_ANGLE_UNIT ( ) SI_UNIT ( $, .RADIAN. ) );
#45729 = CARTESIAN_POINT ( 'NONE',  ( -1.586052503253848389, 0.7480314960629931287, -0.1653254495020559933 ) ) ;
#45730 = CARTESIAN_POINT ( 'NONE',  ( 0.2821522309711292364, 0.1771653543307087075, -0.09757992244046823083 ) ) ;
#45731 = CARTESIAN_POINT ( 'NONE',  ( -0.02863813702883717324, 1.063821633877343631, -1.439971228356280220 ) ) ;
#45732 = CARTESIAN_POINT ( 'NONE',  ( 0.1958661417322836440, -0.3392501089628017219, -0.3339895013123360679 ) ) ;
#45733 = CARTESIAN_POINT ( 'NONE',  ( -0.3740157480314953431, -0.4536011799217368745, -0.2665933059059886201 ) ) ;
#45734 = CARTESIAN_POINT ( 'NONE',  ( -0.9645669291338575535, 0.1660481256975883668, -0.3530559997133364547 ) ) ;
#45735 = CARTESIAN_POINT ( 'NONE',  ( 1.141732283464567566, 0.2952755905511811885, 0.000000000000000000 ) ) ;
#45736 = CARTESIAN_POINT ( 'NONE',  ( -0.4133858267716528645, -0.5400638737290844871, 0.3530559997133364547 ) ) ;
#45737 = ORIENTED_EDGE ( 'NONE', *, *, #35750, .F. ) ;
#45738 = ORIENTED_EDGE ( 'NONE', *, *, #31645, .T. ) ;
#45739 = CARTESIAN_POINT ( 'NONE',  ( 0.1998031496062992463, 0.3460692066303959202, -1.795931758530183719 ) ) ;
#45740 = CARTESIAN_POINT ( 'NONE',  ( -0.8070866141732276899, 0.1660481256975883668, -0.3530559997133364547 ) ) ;
#45741 = CARTESIAN_POINT ( 'NONE',  ( 1.240157480314961314, -0.5400638737290844871, 0.3530559997133364547 ) ) ;
#45742 = CARTESIAN_POINT ( 'NONE',  ( -1.614173228346456268, -0.5511811023622047445, 6.969142054262312111E-17 ) ) ;
#45743 = CARTESIAN_POINT ( 'NONE',  ( -0.01219799715822228459, 1.075705580628688374, 0.2362204724409448509 ) ) ;
#45744 = CARTESIAN_POINT ( 'NONE',  ( 0.2362204724409451007, -0.4091458600556402980, -0.8792650918635170898 ) ) ;
#45745 = CARTESIAN_POINT ( 'NONE',  ( -0.4705803914132928312, 1.475246498736264344, 3.908783377261402681 ) ) ;
#45746 = CARTESIAN_POINT ( 'NONE',  ( -9.594673741351313045E-17, 0.3917322834645670104, -0.4645669291338582751 ) ) ;
#45747 = DIRECTION ( 'NONE',  ( 0.000000000000000000, 0.000000000000000000, 1.000000000000000000 ) ) ;
#45748 = CARTESIAN_POINT ( 'NONE',  ( -0.2493438320209966919, -0.4281496062992124485, 0.4176697321401328655 ) ) ;
#45749 = CARTESIAN_POINT ( 'NONE',  ( -1.607611548556429737, 0.1771653543307087075, -0.09757992244046823083 ) ) ;
#45750 = CARTESIAN_POINT ( 'NONE',  ( -0.6889763779527552368, -0.5400638737290845981, -0.3530559997133363437 ) ) ;
#45751 = CARTESIAN_POINT ( 'NONE',  ( -0.3996062992125985480, -7.340648628747423112E-17, 0.1988188976377952277 ) ) ;
#45752 = CARTESIAN_POINT ( 'NONE',  ( -1.450131233595799651, -0.6692913385826771977, 0.1292274648535927661 ) ) ;
#45753 = CARTESIAN_POINT ( 'NONE',  ( -1.141732283464566011, -0.6692913385826771977, 8.415575281601705876E-17 ) ) ;
#45754 = CARTESIAN_POINT ( 'NONE',  ( -0.4199475065616791736, 0.2306618581243847221, -0.2411417322834647770 ) ) ;
#45755 = CARTESIAN_POINT ( 'NONE',  ( 0.3420746716998660508, 0.1974969037888705814, -2.570209973753280863 ) ) ;
#45756 = CARTESIAN_POINT ( 'NONE',  ( 1.010498687664042716, -0.004921259842519870586, -0.3153832671262229437 ) ) ;
#45757 = CARTESIAN_POINT ( 'NONE',  ( 0.6233595800524942554, -0.08942795157528024563, -0.3641732283464568787 ) ) ;
#45758 = CARTESIAN_POINT ( 'NONE',  ( 1.391076115485564868, -0.5023911411419708095, 0.1820866141732285504 ) ) ;
#45759 = CARTESIAN_POINT ( 'NONE',  ( 1.227034120734908917, -0.6692913385826771977, 0.1292274648535927661 ) ) ;
#45760 = CARTESIAN_POINT ( 'NONE',  ( 0.04593175853018440641, -0.5511811023622046335, 0.09757992244046803654 ) ) ;
#45761 = CARTESIAN_POINT ( 'NONE',  ( -0.2867679344610364334, -0.2867679344610367109, -1.625984251968503491 ) ) ;
#45762 = CARTESIAN_POINT ( 'NONE',  ( -1.299212598425196097, 0.2952755905511811885, 0.000000000000000000 ) ) ;
#45763 = CARTESIAN_POINT ( 'NONE',  ( 1.082677165354331228, -0.5400638737290844871, 0.3530559997133364547 ) ) ;
#45764 = CARTESIAN_POINT ( 'NONE',  ( -0.4091458600556402980, -0.2362204724409451284, 0.1856955380577427484 ) ) ;
#45765 = CARTESIAN_POINT ( 'NONE',  ( -0.6824146981627288167, 0.1283753931104748280, 0.1820866141732283561 ) ) ;
#45766 = LINE ( 'NONE', #764, #42617 ) ;
#45767 = CARTESIAN_POINT ( 'NONE',  ( 0.4396325459317593221, 0.2952755905511810774, -0.1292274648535930714 ) ) ;
#45768 = LINE ( 'NONE', #58407, #16999 ) ;
#45769 = CARTESIAN_POINT ( 'NONE',  ( 0.8267716535433077274, 0.1771653543307087630, 0.000000000000000000 ) ) ;
#45770 = CARTESIAN_POINT ( 'NONE',  ( 0.05249343832021075018, 0.1283753931104746893, -0.1820866141732285504 ) ) ;
#45771 = CARTESIAN_POINT ( 'NONE',  ( -0.2821522309711278487, -0.6692913385826773087, -0.1292274648535924053 ) ) ;
#45772 = CARTESIAN_POINT ( 'NONE',  ( -1.338582677165353729, -0.1870078740157480879, -0.4822834645669291653 ) ) ;
#45773 = CARTESIAN_POINT ( 'NONE',  ( -0.5118110236220466680, 0.1771653543307087630, 0.000000000000000000 ) ) ;
#45774 = DIRECTION ( 'NONE',  ( 0.000000000000000000, 1.000000000000000000, -0.000000000000000000 ) ) ;
#45775 = CARTESIAN_POINT ( 'NONE',  ( 0.4855643044619430415, -0.4281496062992127816, -0.4176697321401328100 ) ) ;
#45776 = CIRCLE ( 'NONE', #57847, 0.1937007874015747588 ) ;
#45777 = CARTESIAN_POINT ( 'NONE',  ( -1.056430446194224881, -0.6692913385826771977, 0.1292274648535927661 ) ) ;
#45778 = CARTESIAN_POINT ( 'NONE',  ( -0.3996062992125984925, -0.1070741851644056858, -1.225065616797899937 ) ) ;
#45779 = CARTESIAN_POINT ( 'NONE',  ( -0.1958661417322834220, -0.3392501089628018884, -2.827427821522309426 ) ) ;
#45780 = CARTESIAN_POINT ( 'NONE',  ( 0.1706036745406830368, -0.004921259842519576551, 0.3153832671262227771 ) ) ;
#45781 = CARTESIAN_POINT ( 'NONE',  ( -0.9186351706036736120, -0.6046776061558809534, -0.2411417322834644161 ) ) ;
#45782 = CARTESIAN_POINT ( 'NONE',  ( -1.003937007874014853, 0.1660481256975885056, 0.3530559997133364547 ) ) ;
#45783 = CARTESIAN_POINT ( 'NONE',  ( -1.141732283464566011, 0.1771653543307087630, 0.000000000000000000 ) ) ;
#45784 = CARTESIAN_POINT ( 'NONE',  ( 1.614173228346457378, -0.6692913385826771977, 8.415575281601705876E-17 ) ) ;
#45785 = CARTESIAN_POINT ( 'NONE',  ( -1.095800524934382292, -0.2845877964562161244, -0.3641732283464567121 ) ) ;
#45786 = CARTESIAN_POINT ( 'NONE',  ( 0.4498537592782897998, 0.000000000000000000, 2.118110236220472675 ) ) ;
#45787 = CARTESIAN_POINT ( 'NONE',  ( 1.377952755905512472, -0.6692913385826771977, 8.415575281601705876E-17 ) ) ;
#45788 = CARTESIAN_POINT ( 'NONE',  ( 0.01109768429471727318, 2.739544932778246860E-15, 0.3954974714151458515 ) ) ;
#45789 = CARTESIAN_POINT ( 'NONE',  ( 4.797336870675656522E-17, -0.3917322834645670659, -2.595163672737219596 ) ) ;
#45790 = ORIENTED_EDGE ( 'NONE', *, *, #68162, .T. ) ;
#45791 = AXIS2_PLACEMENT_3D ( 'NONE', #74926, #34958, #74094 ) ;
#45792 = CARTESIAN_POINT ( 'NONE',  ( 0.01930322177395383046, -0.3957358693849765685, -5.613290098372282899E-13 ) ) ;
#45793 = CARTESIAN_POINT ( 'NONE',  ( 1.384514435695538337, -0.5511811023622046335, 0.09757992244046803654 ) ) ;
#45794 = CARTESIAN_POINT ( 'NONE',  ( -1.272965879265091305, -0.4281496062992124485, 0.4176697321401328655 ) ) ;
#45795 = CARTESIAN_POINT ( 'NONE',  ( 1.141732283464567566, 0.2952755905511811885, 0.000000000000000000 ) ) ;
#45796 = CARTESIAN_POINT ( 'NONE',  ( 4.797336870675656522E-17, -0.3917322834645670104, -2.210629921259842590 ) ) ;
#45797 = CARTESIAN_POINT ( 'NONE',  ( 1.679790026246720025, 0.1283753931104748280, 0.1820866141732283561 ) ) ;
#45798 = EDGE_CURVE ( 'NONE', #11714, #44018, #13113, .T. ) ;
#45799 = CARTESIAN_POINT ( 'NONE',  ( 0.5118110236220480003, -0.6692913385826771977, 8.415575281601705876E-17 ) ) ;
#45800 = CARTESIAN_POINT ( 'NONE',  ( 0.1115485564304470323, 0.2952755905511811885, 0.1292274648535926551 ) ) ;
#45801 = CARTESIAN_POINT ( 'NONE',  ( 5.818687728935708833E-24, 1.062992125984252745, -3.937007874015748143 ) ) ;
#45802 = CARTESIAN_POINT ( 'NONE',  ( -0.7330049731598978768, 2.188112158500873150, -0.5178675056768471396 ) ) ;
#45803 = CARTESIAN_POINT ( 'NONE',  ( 0.8070866141732288002, 0.07958543189024085140, 0.2665933059059887866 ) ) ;
#45804 = CARTESIAN_POINT ( 'NONE',  ( -0.2925321140481930704, -0.2925321140481933480, -1.161417322834645383 ) ) ;
#45805 = ORIENTED_EDGE ( 'NONE', *, *, #68362, .T. ) ;
#45806 = CARTESIAN_POINT ( 'NONE',  ( 0.1049643490035304799, -0.3917322834645670104, -0.08204031315716725503 ) ) ;
#45807 = VERTEX_POINT ( 'NONE', #15809 ) ;
#45808 = CARTESIAN_POINT ( 'NONE',  ( 0.1771653543307093182, 0.1660481256975885056, 0.3530559997133364547 ) ) ;
#45809 = CARTESIAN_POINT ( 'NONE',  ( 1.535433070866142335, -0.6692913385826771977, 8.415575281601705876E-17 ) ) ;
#45810 = CARTESIAN_POINT ( 'NONE',  ( 0.7152230971128616943, -0.05778040916215522460, 0.4822834645669289988 ) ) ;
#45811 = CARTESIAN_POINT ( 'NONE',  ( 1.049868766404200349, 0.2306618581243848609, 0.2411417322834645549 ) ) ;
#45812 = CARTESIAN_POINT ( 'NONE',  ( -0.4265091863517051496, -0.6692913385826771977, 0.1292274648535927661 ) ) ;
#45813 = CARTESIAN_POINT ( 'NONE',  ( -0.006561679790025524116, -0.3162353388693405765, 0.4822834645669290543 ) ) ;
#45814 = CARTESIAN_POINT ( 'NONE',  ( 1.614173228346457378, 0.2952755905511811885, 0.000000000000000000 ) ) ;
#45815 = CARTESIAN_POINT ( 'NONE',  ( 1.364829396325459854, -0.6046776061558809534, -0.2411417322834644161 ) ) ;
#45816 = CARTESIAN_POINT ( 'NONE',  ( 0.9973753280839902091, -0.6046776061558807314, 0.2411417322834647770 ) ) ;
#45817 = CARTESIAN_POINT ( 'NONE',  ( 0.1049643490035304938, -0.3917322834645669549, -0.3923884514435695414 ) ) ;
#45818 = CARTESIAN_POINT ( 'NONE',  ( 0.5511811023622055217, -0.1870078740157479769, 0.3641732283464567677 ) ) ;
#45819 = EDGE_LOOP ( 'NONE', ( #56207, #56051, #74520 ) ) ;
#45820 = CARTESIAN_POINT ( 'NONE',  ( 0.3420746716998659953, 0.1974969037888705536, -0.4461942257217848540 ) ) ;
#45821 = EDGE_LOOP ( 'NONE', ( #75983, #70955, #19412, #31243 ) ) ;
#45822 = CARTESIAN_POINT ( 'NONE',  ( -0.3937007874015740483, -0.1870078740157480601, -0.3641732283464567677 ) ) ;
#45823 = CARTESIAN_POINT ( 'NONE',  ( -0.01968503937007793844, 0.1660481256975883668, -0.3530559997133364547 ) ) ;
#45824 = CARTESIAN_POINT ( 'NONE',  ( 2.800715669567023003, 1.143166703770569281, -0.2643333500026459060 ) ) ;
#45825 = CARTESIAN_POINT ( 'NONE',  ( 0.3215223097112867578, -0.05778040916215522460, 0.4822834645669289988 ) ) ;
#45826 = CARTESIAN_POINT ( 'NONE',  ( 0.1706036745406830368, 0.05413385826771666132, 0.4176697321401328100 ) ) ;
#45827 = CARTESIAN_POINT ( 'NONE',  ( -0.9580052493438311334, -0.4281496062992124485, 0.4176697321401328655 ) ) ;
#45828 = CARTESIAN_POINT ( 'NONE',  ( 1.482939632545932307, -0.3690944881889763329, 0.3153832671262228327 ) ) ;
#45829 = CARTESIAN_POINT ( 'NONE',  ( -1.535433070866141225, -0.6692913385826771977, 8.415575281601705876E-17 ) ) ;
#45830 = LINE ( 'NONE', #71529, #41095 ) ;
#45831 = CARTESIAN_POINT ( 'NONE',  ( 1.010498687664042716, -0.004921259842519870586, -0.3153832671262229437 ) ) ;
#45832 = CARTESIAN_POINT ( 'NONE',  ( 0.4658792650918641698, -0.05778040916215560624, -0.4822834645669293319 ) ) ;
#45833 = CARTESIAN_POINT ( 'NONE',  ( 0.9186351706036752773, 0.2306618581243847221, -0.2411417322834647770 ) ) ;
#45834 = VECTOR ( 'NONE', #20497, 39.37007874015748143 ) ;
#45835 = CARTESIAN_POINT ( 'NONE',  ( 0.3460692066303959202, 0.1998031496062993295, -1.233595800524934338 ) ) ;
#45836 = CARTESIAN_POINT ( 'NONE',  ( -1.692913385826770645, 0.2952755905511811885, 0.000000000000000000 ) ) ;
#45837 = CARTESIAN_POINT ( 'NONE',  ( 0.3460692066303959202, -0.1998031496062991630, -0.8116797900262466836 ) ) ;
#45838 = CARTESIAN_POINT ( 'NONE',  ( 0.1998031496062994128, -0.3460692066303957537, -0.1686351706036745557 ) ) ;
#45839 = CARTESIAN_POINT ( 'NONE',  ( -0.1771653543307080136, -0.5400638737290844871, 0.3530559997133364547 ) ) ;
#45840 = CARTESIAN_POINT ( 'NONE',  ( 0.3996062992125986035, 0.1070741851644054776, -2.644356955380577912 ) ) ;
#45841 = CARTESIAN_POINT ( 'NONE',  ( -0.3917322834645671215, 0.1049643490035301469, -2.164698162729658648 ) ) ;
#45842 = CARTESIAN_POINT ( 'NONE',  ( -1.128608923884513837, 0.1283753931104746893, -0.1820866141732285504 ) ) ;
#45843 = CARTESIAN_POINT ( 'NONE',  ( 1.181102362204724976, -0.1870078740157480879, -0.4822834645669291653 ) ) ;
#45844 = CARTESIAN_POINT ( 'NONE',  ( 1.135170603674541256, -0.6692913385826773087, -0.1292274648535924053 ) ) ;
#45845 = CARTESIAN_POINT ( 'NONE',  ( -0.1640419947506553400, -0.08942795157528024563, -0.3641732283464568787 ) ) ;
#45846 = CARTESIAN_POINT ( 'NONE',  ( 0.3674540682414705883, 0.2306618581243847221, -0.2411417322834647770 ) ) ;
#45847 = CARTESIAN_POINT ( 'NONE',  ( -0.2362204724409451284, 0.4091458600556402425, -1.664698162729658426 ) ) ;
#45848 = CARTESIAN_POINT ( 'NONE',  ( 0.2296587926509192634, -0.2845877964562159024, 0.3641732283464567677 ) ) ;
#45849 = CARTESIAN_POINT ( 'NONE',  ( 0.09186351706036799403, -0.4281496062992127816, -0.4176697321401328100 ) ) ;
#45850 = CARTESIAN_POINT ( 'NONE',  ( 0.2891555358219910499, -0.2891555358219909944, -1.435039370078739829 ) ) ;
#45851 = CARTESIAN_POINT ( 'NONE',  ( -1.161417322834644716, -0.5400638737290845981, -0.3530559997133363437 ) ) ;
#45852 = CARTESIAN_POINT ( 'NONE',  ( 0.4790026246719167324, -0.08942795157527998196, 0.3641732283464567121 ) ) ;
#45853 = AXIS2_PLACEMENT_3D ( 'NONE', #59018, #10589, #3026 ) ;
#45854 = CARTESIAN_POINT ( 'NONE',  ( 0.4687358108553562053, 1.787282772535974340, 0.5180085934481408749 ) ) ;
#45855 = CARTESIAN_POINT ( 'NONE',  ( -0.5905511811023615998, 0.2952755905511811885, 0.000000000000000000 ) ) ;
#45856 = CARTESIAN_POINT ( 'NONE',  ( -0.4921259842519677963, 0.07958543189024071263, -0.2665933059059888421 ) ) ;
#45857 = CARTESIAN_POINT ( 'NONE',  ( -1.604771003085130543, 0.4514378173630710367, -0.1466069496707740061 ) ) ;
#45858 = CARTESIAN_POINT ( 'NONE',  ( -0.6299212598425188991, -0.1870078740157479769, 0.4822834645669291653 ) ) ;
#45859 = CARTESIAN_POINT ( 'NONE',  ( -0.1902887139107604098, 0.2952755905511810774, -0.1292274648535930714 ) ) ;
#45860 = CARTESIAN_POINT ( 'NONE',  ( 0.3018372703412079971, -0.3690944881889763329, 0.3153832671262228327 ) ) ;
#45861 = CARTESIAN_POINT ( 'NONE',  ( -0.1070741851644056997, 0.3996062992125984925, -2.130577427821522818 ) ) ;
#45862 = CARTESIAN_POINT ( 'NONE',  ( 0.05249343832021075018, -0.6046776061558807314, 0.2411417322834647770 ) ) ;
#45863 = CARTESIAN_POINT ( 'NONE',  ( -0.1049643490035306742, 0.3917322834645668994, -2.133838951934696304 ) ) ;
#45864 = CARTESIAN_POINT ( 'NONE',  ( -1.463254593175852492, -0.5511811023622048555, -0.09757992244046775898 ) ) ;
#45865 = CARTESIAN_POINT ( 'NONE',  ( 0.5905511811023629321, 0.1771653543307087630, 0.000000000000000000 ) ) ;
#45866 = CARTESIAN_POINT ( 'NONE',  ( 1.364829396325459854, -0.6046776061558809534, -0.2411417322834644161 ) ) ;
#45867 = CARTESIAN_POINT ( 'NONE',  ( -0.9251968503937002541, 0.07958543189024085140, 0.2665933059059887866 ) ) ;
#45868 = CARTESIAN_POINT ( 'NONE',  ( -1.181102362204723644, -0.1870078740157480601, -0.3641732283464567677 ) ) ;
#45869 = CARTESIAN_POINT ( 'NONE',  ( -0.7874015748031489847, -0.1870078740157480879, -0.4822834645669291653 ) ) ;
#45870 = CARTESIAN_POINT ( 'NONE',  ( -0.09842519685039295696, 0.1660481256975883668, -0.3530559997133364547 ) ) ;
#45871 = CARTESIAN_POINT ( 'NONE',  ( 0.5971128608923891301, 0.1771653543307087075, -0.09757992244046823083 ) ) ;
#45872 = CARTESIAN_POINT ( 'NONE',  ( -0.2747679750349199534, 0.1085817515558208796, 5.561517368279697671 ) ) ;
#45873 = CARTESIAN_POINT ( 'NONE',  ( 0.8858267716535438430, -0.4536011799217368745, -0.2665933059059886201 ) ) ;
#45874 = CARTESIAN_POINT ( 'NONE',  ( 0.1837270341207357105, -0.6046776061558809534, -0.2411417322834644161 ) ) ;
#45875 = CARTESIAN_POINT ( 'NONE',  ( -9.787531504996566615E-17, 0.3996062992125985480, -0.07677165354330710290 ) ) ;
#45876 = CARTESIAN_POINT ( 'NONE',  ( -0.5249343832020990641, -0.6046776061558809534, -0.2411417322834644161 ) ) ;
#45877 = CARTESIAN_POINT ( 'NONE',  ( -0.2867679344610364334, -0.2867679344610367109, -1.561023622047243986 ) ) ;
#45878 = CARTESIAN_POINT ( 'NONE',  ( 1.397637795275591177, -0.4536011799217367080, 0.2665933059059888421 ) ) ;
#45879 = CARTESIAN_POINT ( 'NONE',  ( 0.4199475065616805614, 0.2306618581243848609, 0.2411417322834645549 ) ) ;
#45880 = CARTESIAN_POINT ( 'NONE',  ( 0.2493438320209980519, 0.05413385826771666132, 0.4176697321401328100 ) ) ;
#45881 = FACE_OUTER_BOUND ( 'NONE', #31874, .T. ) ;
#45882 = CARTESIAN_POINT ( 'NONE',  ( -0.006561679790025524116, -0.08942795157528024563, -0.3641732283464568787 ) ) ;
#45883 = CARTESIAN_POINT ( 'NONE',  ( 0.8333333333333340365, -0.6692913385826771977, 0.1292274648535927661 ) ) ;
#45884 = CARTESIAN_POINT ( 'NONE',  ( -0.2690288713910754526, 0.1771653543307087075, -0.09757992244046823083 ) ) ;
#45885 = CARTESIAN_POINT ( 'NONE',  ( -0.8464566929133852113, 0.1660481256975885056, 0.3530559997133364547 ) ) ;
#45886 = DIRECTION ( 'NONE',  ( 0.000000000000000000, -1.000000000000000000, 1.408710688920637755E-15 ) ) ;
#45887 = CARTESIAN_POINT ( 'NONE',  ( -0.06561679790026180015, -0.4281496062992127816, -0.4176697321401328100 ) ) ;
#45888 = EDGE_LOOP ( 'NONE', ( #33631, #3622 ) ) ;
#45889 = CARTESIAN_POINT ( 'NONE',  ( -1.036745406824146176, -0.4281496062992124485, 0.4176697321401328655 ) ) ;
#45890 = CARTESIAN_POINT ( 'NONE',  ( -0.5380577427821514602, -0.3690944881889765550, -0.3153832671262227771 ) ) ;
#45891 = VECTOR ( 'NONE', #79735, 39.37007874015748143 ) ;
#45892 = CARTESIAN_POINT ( 'NONE',  ( 0.006561679790026889343, -0.05778040916215522460, 0.4822834645669289988 ) ) ;
#45893 = CARTESIAN_POINT ( 'NONE',  ( -1.161417322834644716, -0.5400638737290845981, -0.3530559997133363437 ) ) ;
#45894 = CARTESIAN_POINT ( 'NONE',  ( -0.9251968503937002541, -0.5400638737290845981, -0.3530559997133363437 ) ) ;
#45895 = CARTESIAN_POINT ( 'NONE',  ( 1.220472440944882386, 0.000000000000000000, 0.4445507791589061175 ) ) ;
#45897 = CARTESIAN_POINT ( 'NONE',  ( 1.017060367454068581, -0.05778040916215560624, -0.4822834645669293319 ) ) ;
#45896 = CARTESIAN_POINT ( 'NONE',  ( 0.4665770185116077107, 1.519790403714398108, -0.5309055118110237448 ) ) ;
#45898 = CARTESIAN_POINT ( 'NONE',  ( 1.089238845144357759, 0.05413385826771626580, -0.4176697321401330321 ) ) ;
#45899 = CARTESIAN_POINT ( 'NONE',  ( -0.1049643490035301885, -0.3917322834645671215, -2.426509186351705871 ) ) ;
#45900 = CARTESIAN_POINT ( 'NONE',  ( 1.541994750656168645, -0.6692913385826771977, 0.1292274648535927661 ) ) ;
#45901 = CARTESIAN_POINT ( 'NONE',  ( -1.522309711286088607, 0.2306618581243847221, -0.2411417322834647770 ) ) ;
#45902 = CARTESIAN_POINT ( 'NONE',  ( 0.1265901696524990294, -0.4724409448818896462, -0.7152230971128609172 ) ) ;
#45903 = CARTESIAN_POINT ( 'NONE',  ( -0.3996062992125986035, -0.1070741851644056997, -0.2034120734908136385 ) ) ;
#45904 = VERTEX_POINT ( 'NONE', #54490 ) ;
#45905 = CARTESIAN_POINT ( 'NONE',  ( -0.1049868766404193215, -0.5023911411419708095, 0.1820866141732285504 ) ) ;
#45906 = CARTESIAN_POINT ( 'NONE',  ( -0.3392501089628019995, 0.1958661417322832277, -1.908136482939632561 ) ) ;
#45907 = ORIENTED_EDGE ( 'NONE', *, *, #78379, .F. ) ;
#45908 = CARTESIAN_POINT ( 'NONE',  ( 0.08530183727034192087, -0.3162353388693409650, -0.4822834645669289433 ) ) ;
#45909 = CARTESIAN_POINT ( 'NONE',  ( 0.006561679790026889343, -0.05778040916215522460, 0.4822834645669289988 ) ) ;
#45910 = CARTESIAN_POINT ( 'NONE',  ( -0.3458507752293909498, 0.3458507752293907833, -2.696850393700787052 ) ) ;
#45911 = DIRECTION ( 'NONE',  ( -0.000000000000000000, 1.000000000000000000, -0.000000000000000000 ) ) ;
#45912 = CARTESIAN_POINT ( 'NONE',  ( -0.8989501312335946848, -0.5511811023622046335, 0.09757992244046803654 ) ) ;
#45913 = DIRECTION ( 'NONE',  ( 0.000000000000000000, 0.000000000000000000, 1.000000000000000000 ) ) ;
#45914 = CARTESIAN_POINT ( 'NONE',  ( 0.7677165354330716118, 0.1660481256975883668, -0.3530559997133364547 ) ) ;
#45915 = CARTESIAN_POINT ( 'NONE',  ( 0.9120734908136489683, -0.5511811023622046335, 0.09757992244046803654 ) ) ;
#45916 = CARTESIAN_POINT ( 'NONE',  ( -0.3740157480314953431, 0.1660481256975885056, 0.3530559997133364547 ) ) ;
#45917 = CARTESIAN_POINT ( 'NONE',  ( 0.1049643490035304522, -0.3917322834645668994, -1.110216904690602080 ) ) ;
#45918 = CARTESIAN_POINT ( 'NONE',  ( -0.9251968503937002541, -0.5400638737290845981, -0.3530559997133363437 ) ) ;
#45919 = DIRECTION ( 'NONE',  ( 0.000000000000000000, 0.000000000000000000, 1.000000000000000000 ) ) ;
#45920 = CARTESIAN_POINT ( 'NONE',  ( 1.345144356955381593, -0.05778040916215522460, 0.4822834645669289988 ) ) ;
#45921 = CARTESIAN_POINT ( 'NONE',  ( 1.561679790026247350, -0.004921259842519870586, -0.3153832671262229437 ) ) ;
#45922 = ORIENTED_EDGE ( 'NONE', *, *, #64052, .F. ) ;
#45923 = CARTESIAN_POINT ( 'NONE',  ( 0.1958661417322836718, -0.3392501089628017219, -2.608287032317271770 ) ) ;
#45924 = CARTESIAN_POINT ( 'NONE',  ( -0.006561679790025524116, -0.05778040916215560624, -0.4822834645669293319 ) ) ;
#45925 = ORIENTED_EDGE ( 'NONE', *, *, #25308, .F. ) ;
#45926 = CARTESIAN_POINT ( 'NONE',  ( -0.7480314960629914633, 0.2952755905511811885, 0.000000000000000000 ) ) ;
#45927 = CARTESIAN_POINT ( 'NONE',  ( 1.200787401574803681, -0.5400638737290845981, -0.3530559997133363437 ) ) ;
#45928 = CARTESIAN_POINT ( 'NONE',  ( 1.240157480314961314, -0.5400638737290844871, 0.3530559997133364547 ) ) ;
#45929 = CARTESIAN_POINT ( 'NONE',  ( 0.2099737532808405305, 0.2306618581243847221, -0.2411417322834647770 ) ) ;
#45930 = CARTESIAN_POINT ( 'NONE',  ( -0.3280839895013117347, 0.05413385826771626580, -0.4176697321401330321 ) ) ;
#45931 = CARTESIAN_POINT ( 'NONE',  ( 0.1049643490035304938, -0.3917322834645669549, -1.744750656167979308 ) ) ;
#45932 = CARTESIAN_POINT ( 'NONE',  ( -1.332020997375327642, -0.3162353388693409650, -0.4822834645669289433 ) ) ;
#45933 = CARTESIAN_POINT ( 'NONE',  ( -0.1574803149606292529, -0.1870078740157480879, -0.4822834645669291653 ) ) ;
#45934 = CARTESIAN_POINT ( 'NONE',  ( -0.01312335958005186876, -0.004921259842519870586, -0.3153832671262229437 ) ) ;
#45935 = CARTESIAN_POINT ( 'NONE',  ( 2.583694225513480713, 2.755905511811024056, -0.5314960629921260393 ) ) ;
#45936 = EDGE_CURVE ( 'NONE', #16761, #4749, #70336, .T. ) ;
#45937 = CARTESIAN_POINT ( 'NONE',  ( 1.404199475065617708, 0.05413385826771626580, -0.4176697321401330321 ) ) ;
#45938 = CARTESIAN_POINT ( 'NONE',  ( -0.5643044619422565855, 0.05413385826771626580, -0.4176697321401330321 ) ) ;
#45939 = LINE ( 'NONE', #39645, #74908 ) ;
#45940 = CARTESIAN_POINT ( 'NONE',  ( 1.141732283464567566, 0.2952755905511811885, 0.000000000000000000 ) ) ;
#45941 = CARTESIAN_POINT ( 'NONE',  ( 0.5314960629921265944, 0.1012011053420775880, -0.2882089793578257453 ) ) ;
#45942 = EDGE_CURVE ( 'NONE', #8792, #10560, #65155, .T. ) ;
#45943 = ORIENTED_EDGE ( 'NONE', *, *, #41383, .T. ) ;
#45944 = CARTESIAN_POINT ( 'NONE',  ( 0.4658792650918641698, -0.05778040916215560624, -0.4822834645669293319 ) ) ;
#45945 = CARTESIAN_POINT ( 'NONE',  ( -0.3871391076115479057, -0.2845877964562161244, -0.3641732283464567121 ) ) ;
#45947 = CARTESIAN_POINT ( 'NONE',  ( -0.4724409448818898682, -8.678599364036362592E-17, -2.478346456692913868 ) ) ;
#45946 = CARTESIAN_POINT ( 'NONE',  ( 1.095800524934383846, -0.08942795157528024563, -0.3641732283464568787 ) ) ;
#45948 = CARTESIAN_POINT ( 'NONE',  ( -1.157146581871515012E-16, 0.4724409448818898682, -0.07677165354330710290 ) ) ;
#45949 = CARTESIAN_POINT ( 'NONE',  ( 1.633858267716535639, -0.4536011799217367080, 0.2665933059059888421 ) ) ;
#45950 = CARTESIAN_POINT ( 'NONE',  ( 1.391076115485564868, -0.6046776061558807314, 0.2411417322834647770 ) ) ;
#45951 = CARTESIAN_POINT ( 'NONE',  ( 0.1974969037888704704, 0.3420746716998660508, -0.06364829396325460964 ) ) ;
#45952 = PRODUCT_DEFINITION_SHAPE ( 'NONE', 'NONE',  #83322 ) ;
#45953 = CARTESIAN_POINT ( 'NONE',  ( 0.05905511811023681640, 0.1660481256975883668, -0.3530559997133364547 ) ) ;
#45954 = CARTESIAN_POINT ( 'NONE',  ( -1.620734908136482577, 0.2952755905511811885, 0.1292274648535926551 ) ) ;
#45955 = CARTESIAN_POINT ( 'NONE',  ( -1.496062992125983815, -0.1870078740157480879, -0.4822834645669291653 ) ) ;
#45956 = CARTESIAN_POINT ( 'NONE',  ( -0.09842519685039295696, 0.1660481256975883668, -0.3530559997133364547 ) ) ;
#45957 = CARTESIAN_POINT ( 'NONE',  ( -0.3420746716998660508, -0.1974969037888706924, -0.1292650918635170898 ) ) ;
#45958 = CARTESIAN_POINT ( 'NONE',  ( 1.633858267716535639, -0.5400638737290844871, 0.3530559997133364547 ) ) ;
#45959 = CARTESIAN_POINT ( 'NONE',  ( 0.4921259842519691285, 0.1660481256975885056, 0.3530559997133364547 ) ) ;
#45960 = VECTOR ( 'NONE', #32032, 39.37007874015748143 ) ;
#45961 = CARTESIAN_POINT ( 'NONE',  ( 0.9842519685039378130, -0.5511811023622047445, 6.969142054262312111E-17 ) ) ;
#45962 = CARTESIAN_POINT ( 'NONE',  ( -0.05249343832020911260, 0.2306618581243848609, 0.2411417322834645549 ) ) ;
#45963 = CARTESIAN_POINT ( 'NONE',  ( 1.036745406824147731, -0.004921259842519576551, 0.3153832671262227771 ) ) ;
#45964 = CARTESIAN_POINT ( 'NONE',  ( -1.167979002624671470, 0.05413385826771666132, 0.4176697321401328100 ) ) ;
#45965 = CARTESIAN_POINT ( 'NONE',  ( -0.1070741851644051862, -0.3996062992125986590, -0.7788713910761155823 ) ) ;
#45966 = CARTESIAN_POINT ( 'NONE',  ( 1.017060367454068803, -0.3162353388693405765, 0.4822834645669290543 ) ) ;
#45967 = EDGE_CURVE ( 'NONE', #19542, #40260, #54908, .T. ) ;
#45968 = CARTESIAN_POINT ( 'NONE',  ( -0.3392501089628017219, -0.1958661417322836718, -0.8320209973753279753 ) ) ;
#45969 = EDGE_CURVE ( 'NONE', #48621, #69752, #28826, .T. ) ;
#45971 = DIRECTION ( 'NONE',  ( 0.000000000000000000, 1.000000000000000000, -0.000000000000000000 ) ) ;
#45970 = CARTESIAN_POINT ( 'NONE',  ( 0.5905511811023629321, 0.2952755905511811885, 0.000000000000000000 ) ) ;
#45972 = CARTESIAN_POINT ( 'NONE',  ( -3.886287458032462006, 2.165354330708661568, 0.6299212598425196763 ) ) ;
#45973 = CARTESIAN_POINT ( 'NONE',  ( 0.5708661417322841158, -0.4536011799217368745, -0.2665933059059886201 ) ) ;
#45974 = CARTESIAN_POINT ( 'NONE',  ( 0.6561679790026253567, -0.6046776061558809534, -0.2411417322834644161 ) ) ;
#45975 = CARTESIAN_POINT ( 'NONE',  ( 0.7214341416610914326, 0.004960608223780192325, 0.3437734562760181856 ) ) ;
#45976 = CARTESIAN_POINT ( 'NONE',  ( -0.9973753280839886548, -0.5023911411419708095, -0.1820866141732282451 ) ) ;
#45977 = CARTESIAN_POINT ( 'NONE',  ( -1.181102362204723644, -0.1870078740157480879, -0.4822834645669291653 ) ) ;
#45978 = CARTESIAN_POINT ( 'NONE',  ( -1.450131233595799651, -0.6692913385826771977, 0.1292274648535927661 ) ) ;
#45979 = CARTESIAN_POINT ( 'NONE',  ( 0.7677165354330716118, 0.1660481256975883668, -0.3530559997133364547 ) ) ;
#45980 = CARTESIAN_POINT ( 'NONE',  ( -1.607611548556429737, 0.1771653543307087075, -0.09757992244046823083 ) ) ;
#45981 = CARTESIAN_POINT ( 'NONE',  ( -0.3983403474834782965, -0.03178304480584832892, -1.220472440944881942 ) ) ;
#45982 = CARTESIAN_POINT ( 'NONE',  ( 0.8136482939632553313, 0.2306618581243848609, 0.2411417322834645549 ) ) ;
#45983 = CARTESIAN_POINT ( 'NONE',  ( 0.3996062992125986035, -0.1070741851644052972, 0.1266404199475064940 ) ) ;
#45984 = CARTESIAN_POINT ( 'NONE',  ( 2.503252890251015828, 2.755905511811024056, -0.5314960629921260393 ) ) ;
#45985 = CARTESIAN_POINT ( 'NONE',  ( 1.338582677165355062, -0.1870078740157479769, 0.4822834645669291653 ) ) ;
#45986 = CARTESIAN_POINT ( 'NONE',  ( -1.456692913385826182, -0.5511811023622047445, 6.969142054262312111E-17 ) ) ;
#45987 = CARTESIAN_POINT ( 'NONE',  ( 1.062992125984252745, 0.1771653543307087630, 0.000000000000000000 ) ) ;
#45988 = CARTESIAN_POINT ( 'NONE',  ( -1.213910761154854745, -0.5511811023622046335, 0.09757992244046803654 ) ) ;
#45989 = CARTESIAN_POINT ( 'NONE',  ( -0.5511811023622038563, -0.1870078740157479769, 0.3641732283464567677 ) ) ;
#45990 = CARTESIAN_POINT ( 'NONE',  ( 0.4724409448818898682, 2.892866454678787531E-17, -2.007874015748031482 ) ) ;
#45991 = CARTESIAN_POINT ( 'NONE',  ( 0.8530183727034126306, -0.004921259842519870586, -0.3153832671262229437 ) ) ;
#45992 = CARTESIAN_POINT ( 'NONE',  ( 0.4724409448818904789, -0.1870078740157480879, -0.4822834645669291653 ) ) ;
#45993 = CARTESIAN_POINT ( 'NONE',  ( 0.9776902887139113929, 0.2952755905511811885, 0.1292274648535926551 ) ) ;
#45994 = CARTESIAN_POINT ( 'NONE',  ( 0.2493438320209980519, 0.05413385826771666132, 0.4176697321401328100 ) ) ;
#45995 = CARTESIAN_POINT ( 'NONE',  ( 0.5905511811023629321, -0.5511811023622047445, 6.969142054262312111E-17 ) ) ;
#45996 = B_SPLINE_CURVE_WITH_KNOTS ( 'NONE', 3,
 ( #75921, #18260, #19070, #6445, #24958, #50630, #31699, #57358, #17854, #69599, #32116, #57774, #137, #63275, #25793, #17448, #51453, #68775, #11119, #30872, #30465, #5208, #5615, #24145, #36776, #56128, #69184, #11535, #37192, #56539, #82240, #24559, #59456, #45141, #6860, #1807, #32952, #40522, #27053, #58618, #51876, #78838, #77582, #71677, #34206, #39260, #14029, #986, #52295, #78423, #39685, #65377 ),
 .UNSPECIFIED., .F., .F.,
 ( 4, 2, 2, 2, 2, 2, 2, 2, 2, 2, 2, 2, 2, 2, 2, 2, 2, 2, 2, 2, 2, 2, 2, 2, 2, 4 ),
 ( 0.000000000000000000, 0.002382837996120773603, 0.003574256994181160187, 0.004765675992241547206, 0.007148513988362320375, 0.008339932986422706959, 0.009531351984483092676, 0.01072277098254347839, 0.01191418998060386758, 0.01429702797672463208, 0.01548844697478501606, 0.01667986597284539657, 0.01906270396896615066, 0.02025412296702652770, 0.02144554196508690821, 0.02263696096314728873, 0.02382837996120766577, 0.02621121795732841986, 0.02740263695538880037, 0.02859405595344917742, 0.03097689394956994538, 0.03216831294763032589, 0.03335973194569070988, 0.03574256994181145702, 0.03693398893987184101, 0.03812540793793221805 ),
 .UNSPECIFIED. ) ;
#45997 = CARTESIAN_POINT ( 'NONE',  ( 1.200787401574803681, -0.5400638737290845981, -0.3530559997133363437 ) ) ;
#45998 = CARTESIAN_POINT ( 'NONE',  ( -0.1837270341207340729, 0.1539470093639521697, -0.1968503937007875793 ) ) ;
#45999 = CARTESIAN_POINT ( 'NONE',  ( -0.5118110236220466680, -0.6692913385826771977, 8.415575281601705876E-17 ) ) ;
#46000 = CARTESIAN_POINT ( 'NONE',  ( -0.1998031496062994683, 0.3460692066303958092, -0.1706036745406824540 ) ) ;
#46001 = CARTESIAN_POINT ( 'NONE',  ( 0.9881811337016640495, 0.000000000000000000, -0.5314960629921260393 ) ) ;
#46002 = CARTESIAN_POINT ( 'NONE',  ( 5.463695987328526437E-16, -0.1870078740157479769, 0.4822834645669291653 ) ) ;
#46003 = CARTESIAN_POINT ( 'NONE',  ( -0.5511811023622038563, -0.1870078740157479769, 0.4822834645669291653 ) ) ;
#46004 = CARTESIAN_POINT ( 'NONE',  ( 0.1181102362204730916, -0.6692913385826771977, 8.415575281601705876E-17 ) ) ;
#46005 = CARTESIAN_POINT ( 'NONE',  ( -0.1998031496062991907, -0.3460692066303959757, -2.742782152230971437 ) ) ;
#46006 = CARTESIAN_POINT ( 'NONE',  ( -0.1058382717557497937, -0.3949938075777411628, -2.119422572178478070 ) ) ;
#46007 = CARTESIAN_POINT ( 'NONE',  ( -0.1049643490035302024, -0.3917322834645671215, -0.6942257217847765949 ) ) ;
#46008 = CARTESIAN_POINT ( 'NONE',  ( 3.924389226575468737, 2.559055118110236560, -0.3149606299212596716 ) ) ;
#46009 = CARTESIAN_POINT ( 'NONE',  ( 0.2867679344610366554, -0.2867679344610365444, -1.192913385826771533 ) ) ;
#46010 = CARTESIAN_POINT ( 'NONE',  ( -0.9514435695538050464, -0.2845877964562159024, 0.3641732283464567677 ) ) ;
#46011 = CARTESIAN_POINT ( 'NONE',  ( 0.2867679344610365999, -0.2867679344610365444, -1.035433070866141447 ) ) ;
#46012 = CARTESIAN_POINT ( 'NONE',  ( -1.371391076115484831, 0.2952755905511810774, -0.1292274648535930714 ) ) ;
#46013 = VECTOR ( 'NONE', #3064, 39.37007874015748143 ) ;
#46014 = CARTESIAN_POINT ( 'NONE',  ( -0.3917322834645670659, 0.1049643490035301607, 0.04463873835401757639 ) ) ;
#46015 = EDGE_CURVE ( 'NONE', #2910, #29808, #18171, .T. ) ;
#46016 = CARTESIAN_POINT ( 'NONE',  ( 0.6364829396325465405, -0.3162353388693409650, -0.4822834645669289433 ) ) ;
#46017 = CARTESIAN_POINT ( 'NONE',  ( -0.3805774278215216522, -0.3690944881889765550, -0.3153832671262227771 ) ) ;
#46018 = CARTESIAN_POINT ( 'NONE',  ( 1.095800524934383846, -0.3162353388693405765, 0.4822834645669290543 ) ) ;
#46019 = CARTESIAN_POINT ( 'NONE',  ( 0.5643044619422579178, -0.4281496062992127816, -0.4176697321401328100 ) ) ;
#46020 = CARTESIAN_POINT ( 'NONE',  ( 0.4713250013438510799, 1.474963701727497467, 1.018277200043820274 ) ) ;
#46021 = CARTESIAN_POINT ( 'NONE',  ( -0.3460692066303958092, -0.1998031496062994683, -2.729658792650918375 ) ) ;
#46022 = CARTESIAN_POINT ( 'NONE',  ( 0.1049643490035303967, 0.3917322834645670659, -1.407499630742469199 ) ) ;
#46023 = CARTESIAN_POINT ( 'NONE',  ( 1.194225721784777594, 0.05413385826771666132, 0.4176697321401328100 ) ) ;
#46024 = CARTESIAN_POINT ( 'NONE',  ( 0.5774278215223103139, -0.6046776061558809534, -0.2411417322834644161 ) ) ;
#46025 = CARTESIAN_POINT ( 'NONE',  ( 0.1902887139107617975, 0.2952755905511811885, 0.1292274648535926551 ) ) ;
#46026 = CARTESIAN_POINT ( 'NONE',  ( 1.548556430446194954, -0.6046776061558807314, 0.2411417322834647770 ) ) ;
#46027 = CARTESIAN_POINT ( 'NONE',  ( 0.7611548556430454138, 0.2306618581243847221, -0.2411417322834647770 ) ) ;
#46028 = CARTESIAN_POINT ( 'NONE',  ( -0.3917322834645671215, 0.1049643490035301469, -0.4324146981627298159 ) ) ;
#46029 = CARTESIAN_POINT ( 'NONE',  ( -0.1181102362204717315, 0.2952755905511811885, 0.000000000000000000 ) ) ;
#46030 = CARTESIAN_POINT ( 'NONE',  ( 1.082677165354331228, 0.1660481256975883668, -0.3530559997133364547 ) ) ;
#46031 = CARTESIAN_POINT ( 'NONE',  ( 0.4855643044619430415, -0.4281496062992127816, -0.4176697321401328100 ) ) ;
#46032 = CARTESIAN_POINT ( 'NONE',  ( 1.017060367454068803, -0.2845877964562159024, 0.3641732283464567677 ) ) ;
#46033 = CARTESIAN_POINT ( 'NONE',  ( -0.8267716535433065062, -0.6692913385826771977, 8.415575281601705876E-17 ) ) ;
#46034 = CARTESIAN_POINT ( 'NONE',  ( -1.430446194225721390, -0.4281496062992124485, 0.4176697321401328655 ) ) ;
#46035 = CARTESIAN_POINT ( 'NONE',  ( 0.6561679790026253567, 0.2306618581243848609, 0.2411417322834645549 ) ) ;
#46036 = CARTESIAN_POINT ( 'NONE',  ( 0.3204081651526057839, -0.2263583204863392762, -1.929133858267716883 ) ) ;
#46037 = CARTESIAN_POINT ( 'NONE',  ( -0.1049643490035302024, -0.3917322834645671215, -2.111548556430446144 ) ) ;
#46038 = EDGE_CURVE ( 'NONE', #24368, #21487, #35979, .T. ) ;
#46039 = ORIENTED_EDGE ( 'NONE', *, *, #24992, .T. ) ;
#46040 = CARTESIAN_POINT ( 'NONE',  ( -0.2925321140481932924, 0.2925321140481931814, 0.1377952755905511584 ) ) ;
#46041 = ORIENTED_EDGE ( 'NONE', *, *, #64831, .F. ) ;
#46042 = CARTESIAN_POINT ( 'NONE',  ( 1.515748031496063408, 0.1660481256975885056, 0.3530559997133364547 ) ) ;
#46043 = CARTESIAN_POINT ( 'NONE',  ( 0.8398950131233602345, 0.1283753931104746893, -0.1820866141732285504 ) ) ;
#46044 = DIRECTION ( 'NONE',  ( 0.000000000000000000, 0.000000000000000000, -1.000000000000000000 ) ) ;
#46045 = AXIS2_PLACEMENT_3D ( 'NONE', #63859, #57534, #83225 ) ;
#46046 = CARTESIAN_POINT ( 'NONE',  ( -0.4426149705447187110, 1.366040861858872635, 2.619418448465752558 ) ) ;
#46047 = CARTESIAN_POINT ( 'NONE',  ( 0.4177787735907000366, 0.3937007874015747699, -1.757006255033530806 ) ) ;
#46048 = CARTESIAN_POINT ( 'NONE',  ( 0.1049643490035304938, -0.3917322834645669549, -0.9573490813648293241 ) ) ;
#46049 = CARTESIAN_POINT ( 'NONE',  ( -1.049868766404198794, -0.5023911411419708095, 0.1820866141732285504 ) ) ;
#46050 = CARTESIAN_POINT ( 'NONE',  ( 1.541994750656168645, -0.6692913385826771977, 0.1292274648535927661 ) ) ;
#46051 = CARTESIAN_POINT ( 'NONE',  ( -0.3979867861067992729, -0.002674255378744507493, -1.929133858267716661 ) ) ;
#46052 = CARTESIAN_POINT ( 'NONE',  ( -0.3412073490813641308, -0.6046776061558807314, 0.2411417322834647770 ) ) ;
#46053 = CARTESIAN_POINT ( 'NONE',  ( 1.010498687664042716, 0.05413385826771626580, -0.4176697321401330321 ) ) ;
#46054 = ORIENTED_EDGE ( 'NONE', *, *, #25485, .T. ) ;
#46055 = CARTESIAN_POINT ( 'NONE',  ( -1.666666666666665853, 0.05413385826771626580, -0.4176697321401330321 ) ) ;
#46056 = CARTESIAN_POINT ( 'NONE',  ( -1.016821367227983552, 1.537401574803149984, -0.4744094488188975722 ) ) ;
#46057 = CARTESIAN_POINT ( 'NONE',  ( -0.4724409448818898682, -8.678599364036362592E-17, -2.716535433070865757 ) ) ;
#46058 = CARTESIAN_POINT ( 'NONE',  ( 1.614173228346457378, 1.267785121476991073, -0.1372047244094476148 ) ) ;
#46059 = CARTESIAN_POINT ( 'NONE',  ( -0.8792650918635160906, -0.3690944881889763329, 0.3153832671262228327 ) ) ;
#46060 = ADVANCED_FACE ( 'NONE', ( #35146, #35560 ), #43804, .F. ) ;
#46061 = CARTESIAN_POINT ( 'NONE',  ( -1.476377952755905110, 0.1660481256975885056, 0.3530559997133364547 ) ) ;
#46062 = CARTESIAN_POINT ( 'NONE',  ( 0.4921259842519691285, -0.5400638737290845981, -0.3530559997133363437 ) ) ;
#46063 = ORIENTED_EDGE ( 'NONE', *, *, #27570, .F. ) ;
#46065 = CARTESIAN_POINT ( 'NONE',  ( -0.4593175853018366950, 0.009842519685039463617, 0.3409548833797002576 ) ) ;
#46064 = CARTESIAN_POINT ( 'NONE',  ( -3.937007874015748143, 2.559055118110236560, 0.5314960629921260393 ) ) ;
#46066 =( BOUNDED_SURFACE ( )  B_SPLINE_SURFACE ( 1, 2, ( 
 ( #25163, #342, #44510, #13390, #762, #7914, #18861, #38212, #45764, #7493, #39043, #32314, #58403, #71463, #1188, #6226, #25999, #26424, #45349, #50832, #52076, #51656, #6642, #77784, #83253, #26838, #63887, #70618, #33162, #44921, #31901, #20117, #20536, #65156, #13810, #7066, #14234, #39469, #71046, #78205, #52496, #58830, #25576, #46187, #71884, #64727, #32735, #76942, #65580, #77360, #70198, #19692, #76533, #39893, #33575, #12553, #12974, #19268, #38630, #64308, #54161, #54581, #67236, #20950, #46608, #48266, #41953, #80292, #8325, #47019, #9567, #35237, #60490, #72304, #73963, #27253, #22606, #33991, #52912, #21365, #78626, #16309, #15899, #21773, #60901, #67647, #14650, #73128, #40307, #15479, #53338, #3253, #9982, #59653, #8738, #35650, #1598, #65987, #2009, #27671, #47435, #79047, #28915, #72712, #22193, #15059, #73555, #40715, #34408, #66400, #41136, #2431, #60076, #28088, #53745, #79454, #66826, #9158, #34831, #2840, #28503, #79875, #47850, #41547, #11640, #4071, #30570, #4898, #36467, #17141, #17545, #50324, #37299, #12044, #23013, #80700, #49508, #74792, #56236, #69701, #36062, #23425, #81108, #11222, #10807, #62142, #56637, #29331, #81933, #49090, #48681, #42773, #36882, #23841, #4481, #16720, #62973, #61734, #68469, #29738, #43177, #55401, #74377, #42361, #76022, #75615, #24244, #30151, #68060, #30970, #61312, #54992, #75201, #10405, #49917, #55813, #3668, #17953, #82338, #68874, #5312, #43590, #62560, #24656, #81521, #69291, #18365, #44007, #12451, #63786, #6125, #70099, #240, #31799, #63375, #20429, #38941, #26314, #44405, #38112, #20010, #25892, #658, #64622, #57460, #83153, #25473, #51974, #77255, #51552, #51140, #13704, #19168, #6544, #38529, #6959, #44816, #32630, #76433, #76834, #58293, #70513, #45661, #77680, #12870, #64210, #39359, #58719, #32214, #57873, #71357, #19585, #45246, #65044, #70944, #13289, #18762, #7381, #33049, #1083, #26735, #52389, #78098, #46082, #71775, #5711, #37702, #31381, #57046, #82740, #25060, #50734, #21670, #40202, #65477, #33475, #27983, #1495, #46914, #14129, #40613, #66296, #72608, #54055, #2326, #80189, #7809, #59137, #48167, #14956, #27147, #53643, #73021, #22506, #52811, #78521, #34727, #79770, #79351, #21260, #47331, #60386, #73445, #20845, #8635, #15371, #34306, #39782, #41032, #59967, #78941, #66718, #46498, #15795, #72197, #59551, #22086, #33885, #14551, #9054, #9459, #47745, #2737, #28397, #3149, #41445, #67129, #35133, #60795, #28813, #65886, #54476, #8221, #1906, #27567, #53226, #30874, #42677, #9877, #68375, #24561, #24147, #4382, #81009, #10299, #69187, #49410, #23323, #43080, #43491, #56131, #35546, #61208, #37194, #56541, #11537, #80601, #35965, #81836, #49817, #75103, #3564, #62875, #16203, #5210, #22910, #41850, #61635, #67542, #82242, #4790, #10714, #75517, #73862, #29231, #62045, #54895, #30050, #42261, #17856, #48578, #74275, #48993, #16619, #67956, #3976, #29640, #55301, #74691, #17037, #36371, #23737, #55712, #81421, #17450, #68777, #11121, #36778, #62454, #30467, #6030, #6448, #39262, #563, #988, #11948, #69602, #38430, #63691, #19490, #58620, #24960, #12357, #70002, #139, #83056, #51041, #45567, #18262, #77158, #38015, #37603, #31701, #25795, #12773, #25378, #5618, #51878, #50632, #57360, #76337, #32118, #44312, #63277, #31284, #64944, #64525, #13198, #76742, #56949, #19918, #50227, #43904, #64113, #82646, #45143, #18667, #75923, #6862, #71262, #57776, #26216, #32531, #51455, #13608, #19072, #44720, #7284, #70418, #70847, #38845, #58195, #77584, #32954, #27055, #26643, #53961, #66203, #2225, #7714, #59045, #21573, #53129, #27890, #8542, #33382, #52714, #20753, #53550, #46822, #78840, #78425, #72924, #14455, #59458, #33793, #34208, #40107, #59871, #65379, #46403, #79258, #1399, #47235, #15276 ),
 ( #28299, #66616, #72096, #65794, #40937, #8953, #40524, #14031, #34628, #21166, #60292, #2642, #52297, #8128, #78003, #20331, #14862, #45983, #1809, #71679, #72513, #27471, #39687, #52571, #52152, #32388, #25651, #38287, #13884, #77434, #51313, #71118, #71536, #842, #37877, #63551, #65232, #58903, #39543, #25237, #63963, #26500, #77858, #19769, #5885, #7569, #44175, #33241, #50902, #69868, #6300, #12220, #1263, #32811, #38703, #20187, #26911, #31558, #6718, #57215, #58051, #70274, #45838, #18532, #76602, #77016, #82917, #18933, #44581, #12628, #31976, #64382, #57636, #7370, #19348, #39118, #44998, #7138, #70697, #13050, #417, #26073, #51732, #45422, #13461, #64799, #58478, #8810, #65658, #27748, #78279, #21438, #47094, #53412, #34903, #66475, #60973, #46263, #71958, #28988, #79121, #14311, #34486, #53819, #3324, #39971, #7987, #15553, #60565, #60152, #2083, #28163, #41212, #54236, #59314, #72784, #79533, #15134, #20611, #21847, #40790, #59728, #47511, #27327, #79953, #33651, #40379, #2916, #14726, #1670, #73203, #73629, #28579, #66900, #2504, #67307, #21023, #9230, #22266, #47924, #34065, #15971, #9642, #41618, #52987, #78700, #46684, #35311, #8398, #72377, #66062, #60200, #80414, #34950, #47559, #59777, #35360, #16430, #47978, #53036, #16019, #22726, #34535, #61023, #66947, #28209, #60613, #53459, #78748, #46731, #41261, #14773, #2551, #27374, #53868, #79581, #21896, #67356, #15601, #10109, #21073, #72423, #61441, #73253, #40428, #9279, #2962, #35771, #66109, #8445, #73678, #9689, #28628, #54285, #80002, #41665, #3374, #34115, #22315, #29037, #54708, #2131, #48385, #74084, #8857, #42076, #27799, #67771, #79167, #72833, #21484, #47143, #15183, #40840, #66526, #44833, #38129, #70116, #77272, #76851, #50751, #57890, #32232, #12886, #4193, #70531, #63803, #44421, #12467, #61852, #45264, #57062, #23134, #82755, #38957, #38546, #18778, #10926, #23544, #257, #6141, #37717, #57476, #25909, #64226, #48802, #74500, #51569, #70960, #19601, #10525, #49212, #6560, #13305, #31816, #16848, #3788, #29452, #55110, #36180, #80819, #74917, #42482, #68186, #25490, #29856, #76451, #63391, #83170, #51156, #55519, #81227, #5726, #19184, #25077, #17262, #42891, #31397, #68585, #40223, #13725, #40635, #77698, #26753, #46936, #1102, #71375, #59571, #59990, #21281, #14571, #46519, #53664, #53248, #27169, #34327, #8656, #72628, #65064, #14976, #65905, #20868, #72220, #39379, #21690, #33495, #677, #59157, #15391, #66317, #78543, #71796, #52408, #2348, #8241, #14149, #33907, #28004, #79371, #26331, #51993, #47353, #73042, #64641, #7402, #78117, #6978, #32647, #1927, #20028, #58312, #45679, #33071, #58740, #20450, #46103, #39803, #65496, #78962, #1515, #7828, #52831, #27590, #29251, #60408, #54915, #9482, #49015, #23758, #47769, #48187, #49431, #60817, #73884, #10734, #48599, #61231, #73468, #74712, #30072, #61656, #66739, #29661, #36391, #16224, #17059, #80621, #41871, #74295, #67153, #9077, #2759, #22933, #28418, #67565, #41053, #9897, #35568, #3585, #81032, #16641, #75125, #34748, #54078, #79793, #42281, #22109, #67979, #10322, #15819, #41468, #22525, #35986, #35157, #3169, #3997, #28833, #42698, #55323, #23344, #68395, #62065, #4404, #54497, #80209, #55735, #81443, #75536, #12376, #62895, #24580, #81856, #38034, #12792, #6049, #64132, #6466, #57793, #30894, #49837, #56561, #68797, #17876, #50655, #83076, #24168, #4812, #51061, #43510, #70023, #44332, #75943, #82262, #56968, #32136, #76761, #51473, #62477, #36801, #5637, #50247, #63709, #25813, #160, #17470, #19091, #56153, #18284, #43927, #38448, #11142, #31721, #37216, #30488, #5230, #76357, #63299, #69623, #69210, #44740, #11559, #11968, #37623, #82666, #31304, #24981, #18689, #43101, #57382, #25397, #70435, #32550, #46839, #77176, #70866 ) ),
 .UNSPECIFIED., .F., .F., .F. ) 
 B_SPLINE_SURFACE_WITH_KNOTS ( ( 2, 2 ),
 ( 3, 2, 2, 2, 2, 2, 2, 2, 2, 2, 2, 2, 2, 2, 2, 2, 2, 2, 2, 2, 2, 2, 2, 2, 2, 2, 2, 2, 2, 2, 2, 2, 2, 2, 2, 2, 2, 2, 2, 2, 2, 2, 2, 2, 2, 2, 2, 2, 2, 2, 2, 2, 2, 2, 2, 2, 2, 2, 2, 2, 2, 2, 2, 2, 2, 2, 2, 2, 2, 2, 2, 2, 2, 2, 2, 2, 2, 2, 2, 2, 2, 2, 2, 2, 2, 2, 2, 2, 2, 2, 2, 2, 2, 2, 2, 2, 2, 2, 2, 2, 2, 2, 2, 2, 2, 2, 2, 2, 2, 2, 2, 2, 2, 2, 2, 2, 2, 2, 2, 2, 2, 2, 2, 2, 2, 2, 2, 2, 2, 2, 2, 2, 2, 2, 2, 2, 2, 2, 2, 2, 2, 2, 2, 2, 2, 2, 2, 2, 2, 2, 2, 2, 2, 2, 2, 2, 2, 2, 2, 2, 2, 2, 2, 2, 2, 2, 2, 2, 2, 2, 2, 2, 2, 2, 2, 2, 2, 2, 2, 2, 2, 2, 2, 2, 2, 2, 2, 2, 2, 2, 2, 2, 2, 2, 2, 2, 2, 2, 2, 2, 2, 2, 2, 2, 2, 2, 2, 2, 2, 2, 2, 2, 2, 2, 2, 2, 2, 2, 2, 2, 2, 2, 2, 2, 2, 2, 2, 2, 2, 2, 2, 2, 2, 2, 2, 2, 2, 3 ),
 ( 0.000000000000000000, 1.000000000000000000 ),
 ( 0.000000000000000000, 0.004166666666666666609, 0.008333333333333333218, 0.01250000000000000069, 0.01666666666666666644, 0.02083333333333333218, 0.02500000000000000139, 0.02916666666666666713, 0.03333333333333333287, 0.03749999999999999861, 0.04166666666666666435, 0.04583333333333333010, 0.05000000000000000278, 0.05416666666666666852, 0.05833333333333333426, 0.06250000000000000000, 0.06666666666666666574, 0.07083333333333333148, 0.07499999999999999722, 0.07916666666666666297, 0.08333333333333332871, 0.08749999999999999445, 0.09166666666666666019, 0.09583333333333333981, 0.1000000000000000056, 0.1041666666666666713, 0.1083333333333333370, 0.1125000000000000028, 0.1166666666666666685, 0.1208333333333333343, 0.1250000000000000000, 0.1291666666666666796, 0.1333333333333333315, 0.1375000000000000111, 0.1416666666666666630, 0.1458333333333333426, 0.1499999999999999944, 0.1541666666666666741, 0.1583333333333333259, 0.1625000000000000056, 0.1666666666666666574, 0.1708333333333333370, 0.1749999999999999889, 0.1791666666666666685, 0.1833333333333333204, 0.1875000000000000000, 0.1916666666666666796, 0.1958333333333333315, 0.2000000000000000111, 0.2041666666666666630, 0.2083333333333333426, 0.2124999999999999944, 0.2166666666666666741, 0.2208333333333333259, 0.2250000000000000056, 0.2291666666666666574, 0.2333333333333333370, 0.2374999999999999889, 0.2416666666666666685, 0.2458333333333333204, 0.2500000000000000000, 0.2541666666666666519, 0.2583333333333333592, 0.2625000000000000111, 0.2666666666666666630, 0.2708333333333333148, 0.2750000000000000222, 0.2791666666666666741, 0.2833333333333333259, 0.2874999999999999778, 0.2916666666666666852, 0.2958333333333333370, 0.2999999999999999889, 0.3041666666666666408, 0.3083333333333333481, 0.3125000000000000000, 0.3166666666666666519, 0.3208333333333333592, 0.3250000000000000111, 0.3291666666666666630, 0.3333333333333333148, 0.3375000000000000222, 0.3416666666666666741, 0.3458333333333333259, 0.3499999999999999778, 0.3541666666666666852, 0.3583333333333333370, 0.3624999999999999889, 0.3666666666666666408, 0.3708333333333333481, 0.3750000000000000000, 0.3791666666666666519, 0.3833333333333333592, 0.3875000000000000111, 0.3916666666666666630, 0.3958333333333333148, 0.4000000000000000222, 0.4041666666666666741, 0.4083333333333333259, 0.4124999999999999778, 0.4166666666666666852, 0.4208333333333333370, 0.4249999999999999889, 0.4291666666666666408, 0.4333333333333333481, 0.4375000000000000000, 0.4416666666666666519, 0.4458333333333333592, 0.4500000000000000111, 0.4541666666666666630, 0.4583333333333333148, 0.4625000000000000222, 0.4666666666666666741, 0.4708333333333333259, 0.4749999999999999778, 0.4791666666666666852, 0.4833333333333333370, 0.4874999999999999889, 0.4916666666666666408, 0.4958333333333333481, 0.5000000000000000000, 0.5041666666666666519, 0.5083333333333333037, 0.5124999999999999556, 0.5166666666666667185, 0.5208333333333333703, 0.5250000000000000222, 0.5291666666666666741, 0.5333333333333333259, 0.5374999999999999778, 0.5416666666666666297, 0.5458333333333332815, 0.5500000000000000444, 0.5541666666666666963, 0.5583333333333333481, 0.5625000000000000000, 0.5666666666666666519, 0.5708333333333333037, 0.5749999999999999556, 0.5791666666666667185, 0.5833333333333333703, 0.5875000000000000222, 0.5916666666666666741, 0.5958333333333333259, 0.5999999999999999778, 0.6041666666666666297, 0.6083333333333332815, 0.6125000000000000444, 0.6166666666666666963, 0.6208333333333333481, 0.6250000000000000000, 0.6291666666666666519, 0.6333333333333333037, 0.6374999999999999556, 0.6416666666666667185, 0.6458333333333333703, 0.6500000000000000222, 0.6541666666666666741, 0.6583333333333333259, 0.6624999999999999778, 0.6666666666666666297, 0.6708333333333332815, 0.6750000000000000444, 0.6791666666666666963, 0.6833333333333333481, 0.6875000000000000000, 0.6916666666666666519, 0.6958333333333333037, 0.6999999999999999556, 0.7041666666666667185, 0.7083333333333333703, 0.7125000000000000222, 0.7166666666666666741, 0.7208333333333333259, 0.7249999999999999778, 0.7291666666666666297, 0.7333333333333332815, 0.7375000000000000444, 0.7416666666666666963, 0.7458333333333333481, 0.7500000000000000000, 0.7541666666666666519, 0.7583333333333333037, 0.7624999999999999556, 0.7666666666666667185, 0.7708333333333333703, 0.7750000000000000222, 0.7791666666666666741, 0.7833333333333333259, 0.7874999999999999778, 0.7916666666666666297, 0.7958333333333332815, 0.8000000000000000444, 0.8041666666666666963, 0.8083333333333333481, 0.8125000000000000000, 0.8166666666666666519, 0.8208333333333333037, 0.8249999999999999556, 0.8291666666666667185, 0.8333333333333333703, 0.8375000000000000222, 0.8416666666666666741, 0.8458333333333333259, 0.8499999999999999778, 0.8541666666666666297, 0.8583333333333332815, 0.8625000000000000444, 0.8666666666666666963, 0.8708333333333333481, 0.8750000000000000000, 0.8791666666666666519, 0.8833333333333333037, 0.8874999999999999556, 0.8916666666666667185, 0.8958333333333333703, 0.9000000000000000222, 0.9041666666666666741, 0.9083333333333333259, 0.9124999999999999778, 0.9166666666666666297, 0.9208333333333332815, 0.9250000000000000444, 0.9291666666666666963, 0.9333333333333333481, 0.9375000000000000000, 0.9416666666666666519, 0.9458333333333333037, 0.9499999999999999556, 0.9541666666666667185, 0.9583333333333333703, 0.9625000000000000222, 0.9666666666666666741, 0.9708333333333333259, 0.9749999999999999778, 0.9791666666666666297, 0.9833333333333332815, 0.9875000000000000444 ),
 .UNSPECIFIED. ) 
 GEOMETRIC_REPRESENTATION_ITEM ( )  RATIONAL_B_SPLINE_SURFACE ( (
 ( 1.000000000000000000, 0.9659258262890683122, 1.000000000000000000, 0.9659258262890683122, 1.000000000000000000, 0.9659258262890683122, 1.000000000000000000, 0.9659258262890683122, 1.000000000000000000, 0.9659258262890683122, 1.000000000000000000, 0.9659258262890683122, 1.000000000000000000, 0.9659258262890683122, 1.000000000000000000, 0.9659258262890683122, 1.000000000000000000, 0.9659258262890683122, 1.000000000000000000, 0.9659258262890683122, 1.000000000000000000, 0.9659258262890683122, 1.000000000000000000, 0.9659258262890683122, 1.000000000000000000, 0.9659258262890683122, 1.000000000000000000, 0.9659258262890683122, 1.000000000000000000, 0.9659258262890683122, 1.000000000000000000, 0.9659258262890683122, 1.000000000000000000, 0.9659258262890683122, 1.000000000000000000, 0.9659258262890683122, 1.000000000000000000, 0.9659258262890683122, 1.000000000000000000, 0.9659258262890683122, 1.000000000000000000, 0.9659258262890683122, 1.000000000000000000, 0.9659258262890683122, 1.000000000000000000, 0.9659258262890683122, 1.000000000000000000, 0.9659258262890683122, 1.000000000000000000, 0.9659258262890683122, 1.000000000000000000, 0.9659258262890683122, 1.000000000000000000, 0.9659258262890683122, 1.000000000000000000, 0.9659258262890683122, 1.000000000000000000, 0.9659258262890683122, 1.000000000000000000, 0.9659258262890683122, 1.000000000000000000, 0.9659258262890683122, 1.000000000000000000, 0.9659258262890683122, 1.000000000000000000, 0.9659258262890683122, 1.000000000000000000, 0.9659258262890683122, 1.000000000000000000, 0.9659258262890683122, 1.000000000000000000, 0.9659258262890683122, 1.000000000000000000, 0.9659258262890683122, 1.000000000000000000, 0.9659258262890683122, 1.000000000000000000, 0.9659258262890683122, 1.000000000000000000, 0.9659258262890683122, 1.000000000000000000, 0.9659258262890683122, 1.000000000000000000, 0.9659258262890683122, 1.000000000000000000, 0.9659258262890683122, 1.000000000000000000, 0.9659258262890683122, 1.000000000000000000, 0.9659258262890683122, 1.000000000000000000, 0.9659258262890683122, 1.000000000000000000, 0.9659258262890683122, 1.000000000000000000, 0.9659258262890683122, 1.000000000000000000, 0.9659258262890683122, 1.000000000000000000, 0.9659258262890683122, 1.000000000000000000, 0.9659258262890683122, 1.000000000000000000, 0.9659258262890683122, 1.000000000000000000, 0.9659258262890683122, 1.000000000000000000, 0.9659258262890683122, 1.000000000000000000, 0.9659258262890683122, 1.000000000000000000, 0.9659258262890683122, 1.000000000000000000, 0.9659258262890683122, 1.000000000000000000, 0.9659258262890683122, 1.000000000000000000, 0.9659258262890683122, 1.000000000000000000, 0.9659258262890683122, 1.000000000000000000, 0.9659258262890683122, 1.000000000000000000, 0.9659258262890683122, 1.000000000000000000, 0.9659258262890683122, 1.000000000000000000, 0.9659258262890683122, 1.000000000000000000, 0.9659258262890683122, 1.000000000000000000, 0.9659258262890683122, 1.000000000000000000, 0.9659258262890683122, 1.000000000000000000, 0.9659258262890683122, 1.000000000000000000, 0.9659258262890683122, 1.000000000000000000, 0.9659258262890683122, 1.000000000000000000, 0.9659258262890683122, 1.000000000000000000, 0.9659258262890683122, 1.000000000000000000, 0.9659258262890683122, 1.000000000000000000, 0.9659258262890683122, 1.000000000000000000, 0.9659258262890683122, 1.000000000000000000, 0.9659258262890683122, 1.000000000000000000, 0.9659258262890683122, 1.000000000000000000, 0.9659258262890683122, 1.000000000000000000, 0.9659258262890683122, 1.000000000000000000, 0.9659258262890683122, 1.000000000000000000, 0.9659258262890683122, 1.000000000000000000, 0.9659258262890683122, 1.000000000000000000, 0.9659258262890683122, 1.000000000000000000, 0.9659258262890683122, 1.000000000000000000, 0.9659258262890683122, 1.000000000000000000, 0.9659258262890683122, 1.000000000000000000, 0.9659258262890683122, 1.000000000000000000, 0.9659258262890683122, 1.000000000000000000, 0.9659258262890683122, 1.000000000000000000, 0.9659258262890683122, 1.000000000000000000, 0.9659258262890683122, 1.000000000000000000, 0.9659258262890683122, 1.000000000000000000, 0.9659258262890683122, 1.000000000000000000, 0.9659258262890683122, 1.000000000000000000, 0.9659258262890683122, 1.000000000000000000, 0.9659258262890683122, 1.000000000000000000, 0.9659258262890683122, 1.000000000000000000, 0.9659258262890683122, 1.000000000000000000, 0.9659258262890683122, 1.000000000000000000, 0.9659258262890683122, 1.000000000000000000, 0.9659258262890683122, 1.000000000000000000, 0.9659258262890683122, 1.000000000000000000, 0.9659258262890683122, 1.000000000000000000, 0.9659258262890683122, 1.000000000000000000, 0.9659258262890683122, 1.000000000000000000, 0.9659258262890683122, 1.000000000000000000, 0.9659258262890683122, 1.000000000000000000, 0.9659258262890683122, 1.000000000000000000, 0.9659258262890683122, 1.000000000000000000, 0.9659258262890683122, 1.000000000000000000, 0.9659258262890683122, 1.000000000000000000, 0.9659258262890683122, 1.000000000000000000, 0.9659258262890683122, 1.000000000000000000, 0.9659258262890683122, 1.000000000000000000, 0.9659258262890683122, 1.000000000000000000, 0.9659258262890683122, 1.000000000000000000, 0.9659258262890683122, 1.000000000000000000, 0.9659258262890683122, 1.000000000000000000, 0.9659258262890683122, 1.000000000000000000, 0.9659258262890683122, 1.000000000000000000, 0.9659258262890683122, 1.000000000000000000, 0.9659258262890683122, 1.000000000000000000, 0.9659258262890683122, 1.000000000000000000, 0.9659258262890683122, 1.000000000000000000, 0.9659258262890683122, 1.000000000000000000, 0.9659258262890683122, 1.000000000000000000, 0.9659258262890683122, 1.000000000000000000, 0.9659258262890683122, 1.000000000000000000, 0.9659258262890683122, 1.000000000000000000, 0.9659258262890683122, 1.000000000000000000, 0.9659258262890683122, 1.000000000000000000, 0.9659258262890683122, 1.000000000000000000, 0.9659258262890683122, 1.000000000000000000, 0.9659258262890683122, 1.000000000000000000, 0.9659258262890683122, 1.000000000000000000, 0.9659258262890683122, 1.000000000000000000, 0.9659258262890683122, 1.000000000000000000, 0.9659258262890683122, 1.000000000000000000, 0.9659258262890683122, 1.000000000000000000, 0.9659258262890683122, 1.000000000000000000, 0.9659258262890683122, 1.000000000000000000, 0.9659258262890683122, 1.000000000000000000, 0.9659258262890683122, 1.000000000000000000, 0.9659258262890683122, 1.000000000000000000, 0.9659258262890683122, 1.000000000000000000, 0.9659258262890683122, 1.000000000000000000, 0.9659258262890683122, 1.000000000000000000, 0.9659258262890683122, 1.000000000000000000, 0.9659258262890683122, 1.000000000000000000, 0.9659258262890683122, 1.000000000000000000, 0.9659258262890683122, 1.000000000000000000, 0.9659258262890683122, 1.000000000000000000, 0.9659258262890683122, 1.000000000000000000, 0.9659258262890683122, 1.000000000000000000, 0.9659258262890683122, 1.000000000000000000, 0.9659258262890683122, 1.000000000000000000, 0.9659258262890683122, 1.000000000000000000, 0.9659258262890683122, 1.000000000000000000, 0.9659258262890683122, 1.000000000000000000, 0.9659258262890683122, 1.000000000000000000, 0.9659258262890683122, 1.000000000000000000, 0.9659258262890683122, 1.000000000000000000, 0.9659258262890683122, 1.000000000000000000, 0.9659258262890683122, 1.000000000000000000, 0.9659258262890683122, 1.000000000000000000, 0.9659258262890683122, 1.000000000000000000, 0.9659258262890683122, 1.000000000000000000, 0.9659258262890683122, 1.000000000000000000, 0.9659258262890683122, 1.000000000000000000, 0.9659258262890683122, 1.000000000000000000, 0.9659258262890683122, 1.000000000000000000, 0.9659258262890683122, 1.000000000000000000, 0.9659258262890683122, 1.000000000000000000, 0.9659258262890683122, 1.000000000000000000, 0.9659258262890683122, 1.000000000000000000, 0.9659258262890683122, 1.000000000000000000, 0.9659258262890683122, 1.000000000000000000, 0.9659258262890683122, 1.000000000000000000, 0.9659258262890683122, 1.000000000000000000, 0.9659258262890683122, 1.000000000000000000, 0.9659258262890683122, 1.000000000000000000, 0.9659258262890683122, 1.000000000000000000, 0.9659258262890683122, 1.000000000000000000, 0.9659258262890683122, 1.000000000000000000, 0.9659258262890683122, 1.000000000000000000, 0.9659258262890683122, 1.000000000000000000, 0.9659258262890683122, 1.000000000000000000, 0.9659258262890683122, 1.000000000000000000, 0.9659258262890683122, 1.000000000000000000, 0.9659258262890683122, 1.000000000000000000, 0.9659258262890683122, 1.000000000000000000, 0.9659258262890683122, 1.000000000000000000, 0.9659258262890683122, 1.000000000000000000, 0.9659258262890683122, 1.000000000000000000, 0.9659258262890683122, 1.000000000000000000, 0.9659258262890683122, 1.000000000000000000, 0.9659258262890683122, 1.000000000000000000, 0.9659258262890683122, 1.000000000000000000, 0.9659258262890683122, 1.000000000000000000, 0.9659258262890683122, 1.000000000000000000, 0.9659258262890683122, 1.000000000000000000, 0.9659258262890683122, 1.000000000000000000, 0.9659258262890683122, 1.000000000000000000, 0.9659258262890683122, 1.000000000000000000, 0.9659258262890683122, 1.000000000000000000, 0.9659258262890683122, 1.000000000000000000, 0.9659258262890683122, 1.000000000000000000, 0.9659258262890683122, 1.000000000000000000, 0.9659258262890683122, 1.000000000000000000, 0.9659258262890683122, 1.000000000000000000, 0.9659258262890683122, 1.000000000000000000, 0.9659258262890683122, 1.000000000000000000, 0.9659258262890683122, 1.000000000000000000, 0.9659258262890683122, 1.000000000000000000, 0.9659258262890683122, 1.000000000000000000, 0.9659258262890683122, 1.000000000000000000, 0.9659258262890683122, 1.000000000000000000, 0.9659258262890683122, 1.000000000000000000, 0.9659258262890683122, 1.000000000000000000, 0.9659258262890683122, 1.000000000000000000, 0.9659258262890683122, 1.000000000000000000, 0.9659258262890683122, 1.000000000000000000, 0.9659258262890683122, 1.000000000000000000, 0.9659258262890683122, 1.000000000000000000, 0.9659258262890683122, 1.000000000000000000, 0.9659258262890683122, 1.000000000000000000, 0.9659258262890683122, 1.000000000000000000, 0.9659258262890683122, 1.000000000000000000, 0.9659258262890683122, 1.000000000000000000, 0.9659258262890683122, 1.000000000000000000, 0.9659258262890683122, 1.000000000000000000, 0.9659258262890683122, 1.000000000000000000, 0.9659258262890683122, 1.000000000000000000, 0.9659258262890683122, 1.000000000000000000, 0.9659258262890683122, 1.000000000000000000, 0.9659258262890683122, 1.000000000000000000, 0.9659258262890683122, 1.000000000000000000),
 ( 1.000000000000000000, 0.9659258262890683122, 1.000000000000000000, 0.9659258262890683122, 1.000000000000000000, 0.9659258262890683122, 1.000000000000000000, 0.9659258262890683122, 1.000000000000000000, 0.9659258262890683122, 1.000000000000000000, 0.9659258262890683122, 1.000000000000000000, 0.9659258262890683122, 1.000000000000000000, 0.9659258262890683122, 1.000000000000000000, 0.9659258262890683122, 1.000000000000000000, 0.9659258262890683122, 1.000000000000000000, 0.9659258262890683122, 1.000000000000000000, 0.9659258262890683122, 1.000000000000000000, 0.9659258262890683122, 1.000000000000000000, 0.9659258262890683122, 1.000000000000000000, 0.9659258262890683122, 1.000000000000000000, 0.9659258262890683122, 1.000000000000000000, 0.9659258262890683122, 1.000000000000000000, 0.9659258262890683122, 1.000000000000000000, 0.9659258262890683122, 1.000000000000000000, 0.9659258262890683122, 1.000000000000000000, 0.9659258262890683122, 1.000000000000000000, 0.9659258262890683122, 1.000000000000000000, 0.9659258262890683122, 1.000000000000000000, 0.9659258262890683122, 1.000000000000000000, 0.9659258262890683122, 1.000000000000000000, 0.9659258262890683122, 1.000000000000000000, 0.9659258262890683122, 1.000000000000000000, 0.9659258262890683122, 1.000000000000000000, 0.9659258262890683122, 1.000000000000000000, 0.9659258262890683122, 1.000000000000000000, 0.9659258262890683122, 1.000000000000000000, 0.9659258262890683122, 1.000000000000000000, 0.9659258262890683122, 1.000000000000000000, 0.9659258262890683122, 1.000000000000000000, 0.9659258262890683122, 1.000000000000000000, 0.9659258262890683122, 1.000000000000000000, 0.9659258262890683122, 1.000000000000000000, 0.9659258262890683122, 1.000000000000000000, 0.9659258262890683122, 1.000000000000000000, 0.9659258262890683122, 1.000000000000000000, 0.9659258262890683122, 1.000000000000000000, 0.9659258262890683122, 1.000000000000000000, 0.9659258262890683122, 1.000000000000000000, 0.9659258262890683122, 1.000000000000000000, 0.9659258262890683122, 1.000000000000000000, 0.9659258262890683122, 1.000000000000000000, 0.9659258262890683122, 1.000000000000000000, 0.9659258262890683122, 1.000000000000000000, 0.9659258262890683122, 1.000000000000000000, 0.9659258262890683122, 1.000000000000000000, 0.9659258262890683122, 1.000000000000000000, 0.9659258262890683122, 1.000000000000000000, 0.9659258262890683122, 1.000000000000000000, 0.9659258262890683122, 1.000000000000000000, 0.9659258262890683122, 1.000000000000000000, 0.9659258262890683122, 1.000000000000000000, 0.9659258262890683122, 1.000000000000000000, 0.9659258262890683122, 1.000000000000000000, 0.9659258262890683122, 1.000000000000000000, 0.9659258262890683122, 1.000000000000000000, 0.9659258262890683122, 1.000000000000000000, 0.9659258262890683122, 1.000000000000000000, 0.9659258262890683122, 1.000000000000000000, 0.9659258262890683122, 1.000000000000000000, 0.9659258262890683122, 1.000000000000000000, 0.9659258262890683122, 1.000000000000000000, 0.9659258262890683122, 1.000000000000000000, 0.9659258262890683122, 1.000000000000000000, 0.9659258262890683122, 1.000000000000000000, 0.9659258262890683122, 1.000000000000000000, 0.9659258262890683122, 1.000000000000000000, 0.9659258262890683122, 1.000000000000000000, 0.9659258262890683122, 1.000000000000000000, 0.9659258262890683122, 1.000000000000000000, 0.9659258262890683122, 1.000000000000000000, 0.9659258262890683122, 1.000000000000000000, 0.9659258262890683122, 1.000000000000000000, 0.9659258262890683122, 1.000000000000000000, 0.9659258262890683122, 1.000000000000000000, 0.9659258262890683122, 1.000000000000000000, 0.9659258262890683122, 1.000000000000000000, 0.9659258262890683122, 1.000000000000000000, 0.9659258262890683122, 1.000000000000000000, 0.9659258262890683122, 1.000000000000000000, 0.9659258262890683122, 1.000000000000000000, 0.9659258262890683122, 1.000000000000000000, 0.9659258262890683122, 1.000000000000000000, 0.9659258262890683122, 1.000000000000000000, 0.9659258262890683122, 1.000000000000000000, 0.9659258262890683122, 1.000000000000000000, 0.9659258262890683122, 1.000000000000000000, 0.9659258262890683122, 1.000000000000000000, 0.9659258262890683122, 1.000000000000000000, 0.9659258262890683122, 1.000000000000000000, 0.9659258262890683122, 1.000000000000000000, 0.9659258262890683122, 1.000000000000000000, 0.9659258262890683122, 1.000000000000000000, 0.9659258262890683122, 1.000000000000000000, 0.9659258262890683122, 1.000000000000000000, 0.9659258262890683122, 1.000000000000000000, 0.9659258262890683122, 1.000000000000000000, 0.9659258262890683122, 1.000000000000000000, 0.9659258262890683122, 1.000000000000000000, 0.9659258262890683122, 1.000000000000000000, 0.9659258262890683122, 1.000000000000000000, 0.9659258262890683122, 1.000000000000000000, 0.9659258262890683122, 1.000000000000000000, 0.9659258262890683122, 1.000000000000000000, 0.9659258262890683122, 1.000000000000000000, 0.9659258262890683122, 1.000000000000000000, 0.9659258262890683122, 1.000000000000000000, 0.9659258262890683122, 1.000000000000000000, 0.9659258262890683122, 1.000000000000000000, 0.9659258262890683122, 1.000000000000000000, 0.9659258262890683122, 1.000000000000000000, 0.9659258262890683122, 1.000000000000000000, 0.9659258262890683122, 1.000000000000000000, 0.9659258262890683122, 1.000000000000000000, 0.9659258262890683122, 1.000000000000000000, 0.9659258262890683122, 1.000000000000000000, 0.9659258262890683122, 1.000000000000000000, 0.9659258262890683122, 1.000000000000000000, 0.9659258262890683122, 1.000000000000000000, 0.9659258262890683122, 1.000000000000000000, 0.9659258262890683122, 1.000000000000000000, 0.9659258262890683122, 1.000000000000000000, 0.9659258262890683122, 1.000000000000000000, 0.9659258262890683122, 1.000000000000000000, 0.9659258262890683122, 1.000000000000000000, 0.9659258262890683122, 1.000000000000000000, 0.9659258262890683122, 1.000000000000000000, 0.9659258262890683122, 1.000000000000000000, 0.9659258262890683122, 1.000000000000000000, 0.9659258262890683122, 1.000000000000000000, 0.9659258262890683122, 1.000000000000000000, 0.9659258262890683122, 1.000000000000000000, 0.9659258262890683122, 1.000000000000000000, 0.9659258262890683122, 1.000000000000000000, 0.9659258262890683122, 1.000000000000000000, 0.9659258262890683122, 1.000000000000000000, 0.9659258262890683122, 1.000000000000000000, 0.9659258262890683122, 1.000000000000000000, 0.9659258262890683122, 1.000000000000000000, 0.9659258262890683122, 1.000000000000000000, 0.9659258262890683122, 1.000000000000000000, 0.9659258262890683122, 1.000000000000000000, 0.9659258262890683122, 1.000000000000000000, 0.9659258262890683122, 1.000000000000000000, 0.9659258262890683122, 1.000000000000000000, 0.9659258262890683122, 1.000000000000000000, 0.9659258262890683122, 1.000000000000000000, 0.9659258262890683122, 1.000000000000000000, 0.9659258262890683122, 1.000000000000000000, 0.9659258262890683122, 1.000000000000000000, 0.9659258262890683122, 1.000000000000000000, 0.9659258262890683122, 1.000000000000000000, 0.9659258262890683122, 1.000000000000000000, 0.9659258262890683122, 1.000000000000000000, 0.9659258262890683122, 1.000000000000000000, 0.9659258262890683122, 1.000000000000000000, 0.9659258262890683122, 1.000000000000000000, 0.9659258262890683122, 1.000000000000000000, 0.9659258262890683122, 1.000000000000000000, 0.9659258262890683122, 1.000000000000000000, 0.9659258262890683122, 1.000000000000000000, 0.9659258262890683122, 1.000000000000000000, 0.9659258262890683122, 1.000000000000000000, 0.9659258262890683122, 1.000000000000000000, 0.9659258262890683122, 1.000000000000000000, 0.9659258262890683122, 1.000000000000000000, 0.9659258262890683122, 1.000000000000000000, 0.9659258262890683122, 1.000000000000000000, 0.9659258262890683122, 1.000000000000000000, 0.9659258262890683122, 1.000000000000000000, 0.9659258262890683122, 1.000000000000000000, 0.9659258262890683122, 1.000000000000000000, 0.9659258262890683122, 1.000000000000000000, 0.9659258262890683122, 1.000000000000000000, 0.9659258262890683122, 1.000000000000000000, 0.9659258262890683122, 1.000000000000000000, 0.9659258262890683122, 1.000000000000000000, 0.9659258262890683122, 1.000000000000000000, 0.9659258262890683122, 1.000000000000000000, 0.9659258262890683122, 1.000000000000000000, 0.9659258262890683122, 1.000000000000000000, 0.9659258262890683122, 1.000000000000000000, 0.9659258262890683122, 1.000000000000000000, 0.9659258262890683122, 1.000000000000000000, 0.9659258262890683122, 1.000000000000000000, 0.9659258262890683122, 1.000000000000000000, 0.9659258262890683122, 1.000000000000000000, 0.9659258262890683122, 1.000000000000000000, 0.9659258262890683122, 1.000000000000000000, 0.9659258262890683122, 1.000000000000000000, 0.9659258262890683122, 1.000000000000000000, 0.9659258262890683122, 1.000000000000000000, 0.9659258262890683122, 1.000000000000000000, 0.9659258262890683122, 1.000000000000000000, 0.9659258262890683122, 1.000000000000000000, 0.9659258262890683122, 1.000000000000000000, 0.9659258262890683122, 1.000000000000000000, 0.9659258262890683122, 1.000000000000000000, 0.9659258262890683122, 1.000000000000000000, 0.9659258262890683122, 1.000000000000000000, 0.9659258262890683122, 1.000000000000000000, 0.9659258262890683122, 1.000000000000000000, 0.9659258262890683122, 1.000000000000000000, 0.9659258262890683122, 1.000000000000000000, 0.9659258262890683122, 1.000000000000000000, 0.9659258262890683122, 1.000000000000000000, 0.9659258262890683122, 1.000000000000000000, 0.9659258262890683122, 1.000000000000000000, 0.9659258262890683122, 1.000000000000000000, 0.9659258262890683122, 1.000000000000000000, 0.9659258262890683122, 1.000000000000000000, 0.9659258262890683122, 1.000000000000000000, 0.9659258262890683122, 1.000000000000000000, 0.9659258262890683122, 1.000000000000000000, 0.9659258262890683122, 1.000000000000000000, 0.9659258262890683122, 1.000000000000000000, 0.9659258262890683122, 1.000000000000000000, 0.9659258262890683122, 1.000000000000000000, 0.9659258262890683122, 1.000000000000000000, 0.9659258262890683122, 1.000000000000000000, 0.9659258262890683122, 1.000000000000000000, 0.9659258262890683122, 1.000000000000000000, 0.9659258262890683122, 1.000000000000000000, 0.9659258262890683122, 1.000000000000000000, 0.9659258262890683122, 1.000000000000000000, 0.9659258262890683122, 1.000000000000000000, 0.9659258262890683122, 1.000000000000000000, 0.9659258262890683122, 1.000000000000000000, 0.9659258262890683122, 1.000000000000000000, 0.9659258262890683122, 1.000000000000000000, 0.9659258262890683122, 1.000000000000000000, 0.9659258262890683122, 1.000000000000000000, 0.9659258262890683122, 1.000000000000000000) ) ) 
 REPRESENTATION_ITEM ( '' )  SURFACE ( )  );
#46067 = CARTESIAN_POINT ( 'NONE',  ( 0.8923884514435703741, 0.2306618581243848609, 0.2411417322834645549 ) ) ;
#46068 = CARTESIAN_POINT ( 'NONE',  ( 1.509186351706037543, -0.3690944881889765550, -0.3153832671262227771 ) ) ;
#46069 = CARTESIAN_POINT ( 'NONE',  ( 0.3392501089628018329, -0.1958661417322834497, -0.6574609991787909724 ) ) ;
#46070 = VECTOR ( 'NONE', #23327, 39.37007874015748854 ) ;
#46071 = CARTESIAN_POINT ( 'NONE',  ( -0.8989501312335946848, 0.1771653543307087075, -0.09757992244046823083 ) ) ;
#46072 = CARTESIAN_POINT ( 'NONE',  ( -1.653543307086613234, -0.1870078740157479769, 0.3641732283464567677 ) ) ;
#46073 = CARTESIAN_POINT ( 'NONE',  ( -0.1958661417322834220, -0.3392501089628018884, -1.095144356955380704 ) ) ;
#46074 = CARTESIAN_POINT ( 'NONE',  ( 0.5643044619422579178, -0.4281496062992127816, -0.4176697321401328100 ) ) ;
#46075 = CARTESIAN_POINT ( 'NONE',  ( -0.7677165354330699465, -0.4536011799217368745, -0.2665933059059886201 ) ) ;
#46076 = CARTESIAN_POINT ( 'NONE',  ( 0.1640419947506569498, -0.08942795157527998196, 0.3641732283464567121 ) ) ;
#46077 = CARTESIAN_POINT ( 'NONE',  ( -0.2493438320209966919, 0.05413385826771626580, -0.4176697321401330321 ) ) ;
#46078 = CARTESIAN_POINT ( 'NONE',  ( -1.128608923884513837, 0.1283753931104746893, -0.1820866141732285504 ) ) ;
#46079 = CARTESIAN_POINT ( 'NONE',  ( 0.3917322834645670659, -0.1049643490035303273, 0.04919328264335768447 ) ) ;
#46080 = CARTESIAN_POINT ( 'NONE',  ( 0.7545931758530188826, -0.6692913385826771977, 0.1292274648535927661 ) ) ;
#46081 = CARTESIAN_POINT ( 'NONE',  ( -1.476377952755905110, 0.1660481256975885056, 0.3530559997133364547 ) ) ;
#46082 = CARTESIAN_POINT ( 'NONE',  ( -0.3458507752293909498, 0.3458507752293907833, -1.356299212598425230 ) ) ;
#46083 = CARTESIAN_POINT ( 'NONE',  ( -0.8792650918635160906, 0.05413385826771626580, -0.4176697321401330321 ) ) ;
#46084 = CARTESIAN_POINT ( 'NONE',  ( -0.2559055118110230564, 0.07958543189024071263, -0.2665933059059888421 ) ) ;
#46085 = EDGE_CURVE ( 'NONE', #38268, #43230, #66730, .T. ) ;
#46086 = CARTESIAN_POINT ( 'NONE',  ( -1.535433070866141225, -0.6692913385826771977, 8.415575281601705876E-17 ) ) ;
#46087 = CARTESIAN_POINT ( 'NONE',  ( 0.7742782152230979209, -0.004921259842519870586, -0.3153832671262229437 ) ) ;
#46088 = CARTESIAN_POINT ( 'NONE',  ( -0.3740157480314953431, -0.4536011799217368745, -0.2665933059059886201 ) ) ;
#46089 = CARTESIAN_POINT ( 'NONE',  ( -0.8661417322834640276, -0.1870078740157480879, -0.4822834645669291653 ) ) ;
#46090 = CARTESIAN_POINT ( 'NONE',  ( -1.246719160104986512, 0.05413385826771666132, 0.4176697321401328100 ) ) ;
#46091 = CARTESIAN_POINT ( 'NONE',  ( -1.397637795275589623, -0.5400638737290845981, -0.3530559997133363437 ) ) ;
#46092 = LINE ( 'NONE', #22096, #13878 ) ;
#46093 = CARTESIAN_POINT ( 'NONE',  ( 1.417322834645670104, -0.1870078740157480601, -0.3641732283464567677 ) ) ;
#46094 = CARTESIAN_POINT ( 'NONE',  ( 0.5708661417322842269, 0.1660481256975885056, 0.3530559997133364547 ) ) ;
#46095 = EDGE_CURVE ( 'NONE', #53271, #50299, #3137, .T. ) ;
#46096 = CARTESIAN_POINT ( 'NONE',  ( -1.489501312335957062, -0.05778040916215522460, 0.4822834645669289988 ) ) ;
#46097 = CARTESIAN_POINT ( 'NONE',  ( -1.732283464566928277, -0.1870078740157479769, 0.4822834645669291653 ) ) ;
#46098 = ORIENTED_EDGE ( 'NONE', *, *, #47242, .F. ) ;
#46099 = CARTESIAN_POINT ( 'NONE',  ( 0.1998031496062994128, -0.3460692066303957537, -2.530839895013123453 ) ) ;
#46100 = CARTESIAN_POINT ( 'NONE',  ( -0.9580052493438311334, -0.004921259842519870586, -0.3153832671262229437 ) ) ;
#46101 = CARTESIAN_POINT ( 'NONE',  ( 0.5708661417322841158, -0.5400638737290845981, -0.3530559997133363437 ) ) ;
#46102 = CARTESIAN_POINT ( 'NONE',  ( -1.220472440944881054, 0.1771653543307087630, 0.000000000000000000 ) ) ;
#46103 = CARTESIAN_POINT ( 'NONE',  ( 0.1070741851644053388, 0.3996062992125986035, -1.959973753280839892 ) ) ;
#46104 = CARTESIAN_POINT ( 'NONE',  ( -1.509186351706035767, 0.05413385826771626580, -0.4176697321401330321 ) ) ;
#46105 = CARTESIAN_POINT ( 'NONE',  ( 0.7808398950131241190, -0.05778040916215560624, -0.4822834645669293319 ) ) ;
#46106 = CARTESIAN_POINT ( 'NONE',  ( 0.4724409448818904789, -0.1870078740157480879, -0.4822834645669291653 ) ) ;
#46107 = CARTESIAN_POINT ( 'NONE',  ( 1.148293963254593653, 0.2952755905511810774, -0.1292274648535930714 ) ) ;
#46108 = CARTESIAN_POINT ( 'NONE',  ( -1.719160104986876103, -0.004921259842519576551, 0.3153832671262227771 ) ) ;
#46109 = CARTESIAN_POINT ( 'NONE',  ( 0.3460692066303959202, -0.1998031496062991630, -1.126640419947506633 ) ) ;
#46110 = CARTESIAN_POINT ( 'NONE',  ( -0.1998031496062994683, 0.3460692066303958092, -1.430446194225721834 ) ) ;
#46111 = CARTESIAN_POINT ( 'NONE',  ( -0.3949938075777409963, -7.255918531996591613E-17, -0.8267716535433070613 ) ) ;
#46112 = AXIS2_PLACEMENT_3D ( 'NONE', #72207, #2747, #20438 ) ;
#46113 = CARTESIAN_POINT ( 'NONE',  ( 0.2980541528757573722, 1.168268747105946970, -1.689904592075601952 ) ) ;
#46114 = CARTESIAN_POINT ( 'NONE',  ( 0.6496062992125991586, -0.4536011799217368745, -0.2665933059059886201 ) ) ;
#46115 = CARTESIAN_POINT ( 'NONE',  ( 0.4724409448818904789, -0.1870078740157479769, 0.3641732283464567677 ) ) ;
#46116 = CARTESIAN_POINT ( 'NONE',  ( -0.1049868766404193215, 0.2306618581243847221, -0.2411417322834647770 ) ) ;
#46117 = CARTESIAN_POINT ( 'NONE',  ( 1.476377952755906220, 0.1660481256975883668, -0.3530559997133364547 ) ) ;
#46118 = CARTESIAN_POINT ( 'NONE',  ( 0.1974969037888706092, -0.3420746716998660508, -1.743438320209973913 ) ) ;
#46119 = CARTESIAN_POINT ( 'NONE',  ( 0.3149606299212606708, -0.1870078740157480601, -0.3641732283464567677 ) ) ;
#46120 = CARTESIAN_POINT ( 'NONE',  ( -0.8202099737532799750, 0.2952755905511810774, -0.1292274648535930714 ) ) ;
#46121 = CARTESIAN_POINT ( 'NONE',  ( -1.502624671916009680, -0.3162353388693405765, 0.4822834645669290543 ) ) ;
#46122 = CARTESIAN_POINT ( 'NONE',  ( 0.9973753280839902091, -0.6046776061558807314, 0.2411417322834647770 ) ) ;
#46123 = CARTESIAN_POINT ( 'NONE',  ( -0.4091458600556405756, 0.2362204724409446288, -2.073490813648294129 ) ) ;
#46124 = CARTESIAN_POINT ( 'NONE',  ( 0.1208384647389237204, -0.3726288332213487653, -2.755905511811024056 ) ) ;
#46125 = VERTEX_POINT ( 'NONE', #22926 ) ;
#46126 = ORIENTED_EDGE ( 'NONE', *, *, #45224, .F. ) ;
#46127 = AXIS2_PLACEMENT_3D ( 'NONE', #29654, #69508, #11857 ) ;
#46128 = CARTESIAN_POINT ( 'NONE',  ( -1.272965879265091305, -0.4281496062992124485, 0.4176697321401328655 ) ) ;
#46130 = CARTESIAN_POINT ( 'NONE',  ( -1.279527559055116948, 0.1660481256975883668, -0.3530559997133364547 ) ) ;
#46129 = CARTESIAN_POINT ( 'NONE',  ( -0.9120734908136475250, -0.5511811023622048555, -0.09757992244046775898 ) ) ;
#46131 = CARTESIAN_POINT ( 'NONE',  ( -0.1049643490035301746, -0.3917322834645670659, -2.514416379756218678 ) ) ;
#46132 = DIRECTION ( 'NONE',  ( 0.000000000000000000, 1.000000000000000000, 0.000000000000000000 ) ) ;
#46133 = CARTESIAN_POINT ( 'NONE',  ( 1.587926509186352586, -0.4281496062992127816, -0.4176697321401328100 ) ) ;
#46134 = CARTESIAN_POINT ( 'NONE',  ( -1.299212598425196097, -0.6692913385826771977, 8.415575281601705876E-17 ) ) ;
#46135 = CARTESIAN_POINT ( 'NONE',  ( 0.3346456692913390985, 0.1660481256975885056, 0.3530559997133364547 ) ) ;
#46136 = CARTESIAN_POINT ( 'NONE',  ( -1.069553805774277722, -0.6692913385826773087, -0.1292274648535924053 ) ) ;
#46137 = CARTESIAN_POINT ( 'NONE',  ( 0.1958661417322836162, -0.3392501089628018329, -2.691581734086927469 ) ) ;
#46138 = CARTESIAN_POINT ( 'NONE',  ( 0.6364829396325465405, -0.05778040916215522460, 0.4822834645669289988 ) ) ;
#46139 = CARTESIAN_POINT ( 'NONE',  ( 0.3917322834645670104, 2.398668435337828261E-17, -1.842519685039370136 ) ) ;
#46140 = CARTESIAN_POINT ( 'NONE',  ( -0.8792650918635160906, -0.3690944881889763329, 0.3153832671262228327 ) ) ;
#46141 = ORIENTED_EDGE ( 'NONE', *, *, #21932, .F. ) ;
#46142 = CARTESIAN_POINT ( 'NONE',  ( 0.3420746716998659953, 0.1974969037888705536, -2.020997375328084100 ) ) ;
#46143 = EDGE_LOOP ( 'NONE', ( #76278, #69009, #5363, #26695 ) ) ;
#46144 = CARTESIAN_POINT ( 'NONE',  ( 3.937007874015748143, 2.755905511811024056, 0.5314960629921260393 ) ) ;
#46145 = CARTESIAN_POINT ( 'NONE',  ( -1.010498687664041384, -0.4281496062992127816, -0.4176697321401328100 ) ) ;
#46146 = CARTESIAN_POINT ( 'NONE',  ( -1.469816272965878357, 0.2306618581243848609, 0.2411417322834645549 ) ) ;
#46147 = CARTESIAN_POINT ( 'NONE',  ( 0.1070741851644054915, -0.3996062992125986035, -0.7152230971128609172 ) ) ;
#46148 = CARTESIAN_POINT ( 'NONE',  ( -1.660104986876639543, -0.05778040916215560624, -0.4822834645669293319 ) ) ;
#46149 = CARTESIAN_POINT ( 'NONE',  ( -1.286089238845143479, -0.6046776061558807314, 0.2411417322834647770 ) ) ;
#46150 = CARTESIAN_POINT ( 'NONE',  ( -1.646981627296586703, -0.05778040916215522460, 0.4822834645669289988 ) ) ;
#46151 = CARTESIAN_POINT ( 'NONE',  ( -1.595398199321655497, 1.839868176060737159, 0.1559797534342489411 ) ) ;
#46152 = CARTESIAN_POINT ( 'NONE',  ( -0.8333333333333323711, 0.2952755905511811885, 0.1292274648535926551 ) ) ;
#46153 = CARTESIAN_POINT ( 'NONE',  ( 0.01312335958005323398, -0.3690944881889765550, -0.3153832671262227771 ) ) ;
#46154 = CARTESIAN_POINT ( 'NONE',  ( 1.614173228346457378, 0.5038684218300975015, 0.1372047244094478369 ) ) ;
#46155 = CARTESIAN_POINT ( 'NONE',  ( 0.3392501089628018329, 0.1958661417322835607, -0.3733595800524935338 ) ) ;
#46156 = CARTESIAN_POINT ( 'NONE',  ( -0.4986876640419942164, -0.5023911411419708095, 0.1820866141732285504 ) ) ;
#46157 = CARTESIAN_POINT ( 'NONE',  ( -0.8070866141732276899, 0.1660481256975883668, -0.3530559997133364547 ) ) ;
#46158 = CARTESIAN_POINT ( 'NONE',  ( 0.9776902887139113929, 0.2952755905511811885, 0.1292274648535926551 ) ) ;
#46159 = CARTESIAN_POINT ( 'NONE',  ( -1.082677165354329896, -0.5400638737290845981, -0.3530559997133363437 ) ) ;
#46160 = VERTEX_POINT ( 'NONE', #80201 ) ;
#46161 = ORIENTED_EDGE ( 'NONE', *, *, #53975, .T. ) ;
#46162 = CARTESIAN_POINT ( 'NONE',  ( -0.8464566929133852113, 0.1660481256975885056, 0.3530559997133364547 ) ) ;
#46163 = CARTESIAN_POINT ( 'NONE',  ( 0.9055118110236227702, -0.6692913385826771977, 8.415575281601705876E-17 ) ) ;
#46164 = CARTESIAN_POINT ( 'NONE',  ( -1.351706036745406347, -0.004921259842519870586, -0.3153832671262229437 ) ) ;
#46165 = CARTESIAN_POINT ( 'NONE',  ( -0.3458507752293909498, 0.3458507752293907833, -1.122047244094488194 ) ) ;
#46166 = CARTESIAN_POINT ( 'NONE',  ( -2.149112266099376445, 1.629972608277048485, 0.4653577321740515194 ) ) ;
#46167 = CARTESIAN_POINT ( 'NONE',  ( 0.3917322834645670104, 2.398668435337828261E-17, -0.2677165354330708347 ) ) ;
#46168 = CARTESIAN_POINT ( 'NONE',  ( 0.3392501089628018884, -0.1958661417322834220, -2.551837270341207109 ) ) ;
#46169 = CARTESIAN_POINT ( 'NONE',  ( -0.4330708661417315697, -0.6692913385826771977, 8.415575281601705876E-17 ) ) ;
#46170 = CARTESIAN_POINT ( 'NONE',  ( -1.555118110236219930, -0.4536011799217368745, -0.2665933059059886201 ) ) ;
#46171 = CARTESIAN_POINT ( 'NONE',  ( -0.5971128608923877978, 0.2952755905511811885, 0.1292274648535926551 ) ) ;
#46172 = CARTESIAN_POINT ( 'NONE',  ( -9.787531504996566615E-17, 0.3996062992125985480, -0.2342519685039370358 ) ) ;
#46174 = DIRECTION ( 'NONE',  ( 0.000000000000000000, -1.000000000000000000, 0.000000000000000000 ) ) ;
#46173 = CARTESIAN_POINT ( 'NONE',  ( -1.404199475065615932, 0.05413385826771666132, 0.4176697321401328100 ) ) ;
#46175 = CARTESIAN_POINT ( 'NONE',  ( -0.9383202099737524282, -0.05778040916215522460, 0.4822834645669289988 ) ) ;
#46176 = CARTESIAN_POINT ( 'NONE',  ( -0.2755905511811018171, 0.2952755905511811885, 0.000000000000000000 ) ) ;
#46177 = CARTESIAN_POINT ( 'NONE',  ( 0.1974969037888706092, -0.3420746716998660508, -2.688320209973753094 ) ) ;
#46178 = CARTESIAN_POINT ( 'NONE',  ( 0.2755905511811031494, -0.5511811023622047445, 6.969142054262312111E-17 ) ) ;
#46179 = CARTESIAN_POINT ( 'NONE',  ( 1.220472440944879722, 2.401574803149606474, 0.5309055118110233007 ) ) ;
#46180 = CARTESIAN_POINT ( 'NONE',  ( 0.4199475065616805614, 0.1283753931104748280, 0.1820866141732283561 ) ) ;
#46181 = CARTESIAN_POINT ( 'NONE',  ( 1.377952755905512472, -0.5511811023622047445, 6.969142054262312111E-17 ) ) ;
#46182 = CARTESIAN_POINT ( 'NONE',  ( 1.305774278215223960, 0.2952755905511810774, -0.1292274648535930714 ) ) ;
#46183 = CARTESIAN_POINT ( 'NONE',  ( 0.1049868766404206816, 0.1283753931104748280, 0.1820866141732283561 ) ) ;
#46184 = CARTESIAN_POINT ( 'NONE',  ( -0.1958661417322836718, 0.3392501089628017219, -1.895013123359580165 ) ) ;
#46185 = CARTESIAN_POINT ( 'NONE',  ( -1.437007874015747477, 0.1660481256975883668, -0.3530559997133364547 ) ) ;
#46186 = CARTESIAN_POINT ( 'NONE',  ( 1.430446194225722500, 0.05413385826771666132, 0.4176697321401328100 ) ) ;
#46187 = CARTESIAN_POINT ( 'NONE',  ( 0.4724409448818896462, 0.1265901696524990294, -0.04396325459317586282 ) ) ;
#46188 = CARTESIAN_POINT ( 'NONE',  ( -0.4724409448818890911, -0.1870078740157480601, -0.3641732283464567677 ) ) ;
#46189 = LINE ( 'NONE', #70200, #21130 ) ;
#46190 = ADVANCED_FACE ( 'NONE', ( #63185 ), #48591, .T. ) ;
#46191 = CARTESIAN_POINT ( 'NONE',  ( 0.1968503937007881344, -0.6692913385826771977, 8.415575281601705876E-17 ) ) ;
#46192 = CARTESIAN_POINT ( 'NONE',  ( -0.4091458600556405756, 0.2362204724409446288, -0.7329396325459317518 ) ) ;
#46193 = AXIS2_PLACEMENT_3D ( 'NONE', #51299, #31545, #71105 ) ;
#46194 = CARTESIAN_POINT ( 'NONE',  ( 0.7677165354330716118, -0.4536011799217367080, 0.2665933059059888421 ) ) ;
#46195 = CARTESIAN_POINT ( 'NONE',  ( 0.2559055118110243332, -0.4536011799217368745, -0.2665933059059886201 ) ) ;
#46196 = CARTESIAN_POINT ( 'NONE',  ( -0.1640419947506553400, -0.05778040916215560624, -0.4822834645669293319 ) ) ;
#46197 = CARTESIAN_POINT ( 'NONE',  ( -1.712598425196849572, 0.1660481256975885056, 0.3530559997133364547 ) ) ;
#46198 = CARTESIAN_POINT ( 'NONE',  ( -0.5577427821522301654, -0.2845877964562159024, 0.3641732283464567677 ) ) ;
#46199 = CARTESIAN_POINT ( 'NONE',  ( -2.570293866835912766, 2.742779993824306484, -0.5314960629921260393 ) ) ;
#46200 = CARTESIAN_POINT ( 'NONE',  ( 0.4002624671916016896, -0.05778040916215522460, 0.4822834645669289988 ) ) ;
#46201 = CARTESIAN_POINT ( 'NONE',  ( -0.8923884514435688198, -0.6046776061558807314, 0.2411417322834647770 ) ) ;
#46202 = CARTESIAN_POINT ( 'NONE',  ( -0.3460692066303960313, 0.1998031496062989965, -1.205380577427821454 ) ) ;
#46203 =( BOUNDED_CURVE ( )  B_SPLINE_CURVE ( 2, ( #54645, #81170, #68528, #79942, #48742, #54225, #9220, #80355, #34893, #49154, #22256, #67710, #60555 ),
 .UNSPECIFIED., .F., .F. ) 
 B_SPLINE_CURVE_WITH_KNOTS ( ( 3, 2, 2, 2, 2, 2, 3 ),
 ( 0.1875000000000000000, 0.1916666666666666796, 0.1958333333333333315, 0.2000000000000000111, 0.2041666666666666907, 0.2083333333333333703, 0.2125000000000000222 ),
 .UNSPECIFIED. ) 
 CURVE ( )  GEOMETRIC_REPRESENTATION_ITEM ( )  RATIONAL_B_SPLINE_CURVE ( ( 1.000000000000000000, 0.9659258262890683122, 1.000000000000000000, 0.9659258262890683122, 1.000000000000000000, 0.9659258262890683122, 1.000000000000000000, 0.9659258262890683122, 1.000000000000000000, 0.9659258262890683122, 1.000000000000000000, 0.9659258262890680902, 1.000000000000000222 ) ) 
 REPRESENTATION_ITEM ( '' )  );
#46204 = CARTESIAN_POINT ( 'NONE',  ( 0.1958661417322836440, -0.3392501089628017219, -2.538713910761154491 ) ) ;
#46205 = CARTESIAN_POINT ( 'NONE',  ( 0.2034120734908142214, 0.1771653543307087075, -0.09757992244046823083 ) ) ;
#46206 = CARTESIAN_POINT ( 'NONE',  ( -0.6430446194225712953, 0.05413385826771626580, -0.4176697321401330321 ) ) ;
#46207 = CARTESIAN_POINT ( 'NONE',  ( -1.062992125984250968, -0.6692913385826771977, 8.415575281601705876E-17 ) ) ;
#46208 = CARTESIAN_POINT ( 'NONE',  ( -1.358267716535432434, -0.4536011799217367080, 0.2665933059059888421 ) ) ;
#46209 = LINE ( 'NONE', #7084, #45428 ) ;
#46210 = CARTESIAN_POINT ( 'NONE',  ( -0.9973753280839886548, 0.1283753931104748280, 0.1820866141732283561 ) ) ;
#46211 = DIRECTION ( 'NONE',  ( 1.000000000000000000, 0.000000000000000000, 0.000000000000000000 ) ) ;
#46212 = CARTESIAN_POINT ( 'NONE',  ( 0.8070866141732288002, 0.1660481256975885056, 0.3530559997133364547 ) ) ;
#46213 = CARTESIAN_POINT ( 'NONE',  ( -0.3996062992125986035, -7.340648628747425578E-17, -0.1968503937007874127 ) ) ;
#46214 = CARTESIAN_POINT ( 'NONE',  ( 0.3917322834645670104, 0.1049643490035304660, -2.641095431267403537 ) ) ;
#46215 = EDGE_LOOP ( 'NONE', ( #81667, #70111, #83129, #26774, #16759 ) ) ;
#46216 = CARTESIAN_POINT ( 'NONE',  ( 2.362204724409448620, 1.929133858267716661, -0.5118110236220390075 ) ) ;
#46217 = CARTESIAN_POINT ( 'NONE',  ( 1.377952755905512472, -0.5511811023622047445, 6.969142054262312111E-17 ) ) ;
#46218 = CARTESIAN_POINT ( 'NONE',  ( -1.154855643044618851, -0.6046776061558809534, -0.2411417322834644161 ) ) ;
#46219 = CARTESIAN_POINT ( 'NONE',  ( 1.187664041994751285, -0.3162353388693409650, -0.4822834645669289433 ) ) ;
#46220 = CARTESIAN_POINT ( 'NONE',  ( 0.2867679344610365999, -0.2867679344610365444, -2.387795275590551380 ) ) ;
#46221 = CARTESIAN_POINT ( 'NONE',  ( 1.548556430446194954, 0.1283753931104746893, -0.1820866141732285504 ) ) ;
#46222 = CARTESIAN_POINT ( 'NONE',  ( 0.5314960629921267055, -0.5400638737290844871, 0.3530559997133364547 ) ) ;
#46223 = CARTESIAN_POINT ( 'NONE',  ( -0.2559055118110227234, -0.5400638737290844871, 0.3530559997133364547 ) ) ;
#46224 = CARTESIAN_POINT ( 'NONE',  ( 0.4744094488189112835, 1.537401574803149984, -3.908320185825791881 ) ) ;
#46225 = CARTESIAN_POINT ( 'NONE',  ( -0.1070741851644051862, -0.3996062992125986590, -1.961942257217847763 ) ) ;
#46226 = CARTESIAN_POINT ( 'NONE',  ( 0.8136482939632553313, 0.1283753931104748280, 0.1820866141732283561 ) ) ;
#46227 = CARTESIAN_POINT ( 'NONE',  ( 4.893765752498283924E-17, -0.3996062992125986035, -1.496062992125984259 ) ) ;
#46228 = ORIENTED_EDGE ( 'NONE', *, *, #76419, .F. ) ;
#46229 = CARTESIAN_POINT ( 'NONE',  ( -0.3917322834645669549, -0.1049643490035306603, -2.872703412073490448 ) ) ;
#46230 = ORIENTED_EDGE ( 'NONE', *, *, #60899, .T. ) ;
#46231 = CARTESIAN_POINT ( 'NONE',  ( -0.1574803149606292529, -0.1870078740157479769, 0.4822834645669291653 ) ) ;
#46232 = CARTESIAN_POINT ( 'NONE',  ( 1.351706036745407458, -0.4281496062992127816, -0.4176697321401328100 ) ) ;
#46233 = CARTESIAN_POINT ( 'NONE',  ( 0.2362204724409456558, -0.1870078740157479769, 0.4822834645669291653 ) ) ;
#46234 = CIRCLE ( 'NONE', #11289, 0.3149606299212597826 ) ;
#46235 = CARTESIAN_POINT ( 'NONE',  ( 1.227034120734908917, 0.2952755905511810774, -0.1292274648535930714 ) ) ;
#46236 = CARTESIAN_POINT ( 'NONE',  ( -0.3805774278215216522, 0.05413385826771666132, 0.4176697321401328100 ) ) ;
#46237 = CARTESIAN_POINT ( 'NONE',  ( -0.1509186351706028884, -0.05778040916215522460, 0.4822834645669289988 ) ) ;
#46238 = CARTESIAN_POINT ( 'NONE',  ( -1.541994750656167090, -0.6692913385826773087, -0.1292274648535924053 ) ) ;
#46239 = CARTESIAN_POINT ( 'NONE',  ( 1.338582677165355062, -0.1870078740157480879, -0.4822834645669291653 ) ) ;
#46240 = CARTESIAN_POINT ( 'NONE',  ( 0.9842519685039378130, -0.6692913385826771977, 8.415575281601705876E-17 ) ) ;
#46241 = CARTESIAN_POINT ( 'NONE',  ( 0.3917322834645670104, 2.398668435337828261E-17, -0.7401574803149605364 ) ) ;
#46242 = CARTESIAN_POINT ( 'NONE',  ( 0.3805774278215230400, -0.3690944881889763329, 0.3153832671262228327 ) ) ;
#46243 = ORIENTED_EDGE ( 'NONE', *, *, #14549, .F. ) ;
#46244 = CARTESIAN_POINT ( 'NONE',  ( 0.2891555358219910499, 0.2891555358219910499, -0.6102362204724410821 ) ) ;
#46245 = VERTEX_POINT ( 'NONE', #47344 ) ;
#46246 = CARTESIAN_POINT ( 'NONE',  ( -0.5774278215223089816, 0.1283753931104746893, -0.1820866141732285504 ) ) ;
#46247 = CARTESIAN_POINT ( 'NONE',  ( -0.2165354330708654795, 0.1660481256975885056, 0.3530559997133364547 ) ) ;
#46248 = CARTESIAN_POINT ( 'NONE',  ( 1.604771003085129433, 0.4934440724007136403, -0.1466069496707749775 ) ) ;
#46249 = CARTESIAN_POINT ( 'NONE',  ( 0.3280839895013130669, 0.05413385826771666132, 0.4176697321401328100 ) ) ;
#46250 = CARTESIAN_POINT ( 'NONE',  ( 0.006561679790026889343, -0.05778040916215522460, 0.4822834645669289988 ) ) ;
#46251 = CARTESIAN_POINT ( 'NONE',  ( -0.7545931758530176614, -0.6692913385826773087, -0.1292274648535924053 ) ) ;
#46252 = CARTESIAN_POINT ( 'NONE',  ( -1.181102362204723644, -0.1870078740157480879, -0.4822834645669291653 ) ) ;
#46253 = AXIS2_PLACEMENT_3D ( 'NONE', #43274, #4577, #63070 ) ;
#46254 = CARTESIAN_POINT ( 'NONE',  ( 1.181102362204725198, -0.1870078740157479769, 0.3641732283464567677 ) ) ;
#46255 = LINE ( 'NONE', #46676, #69448 ) ;
#46256 = CARTESIAN_POINT ( 'NONE',  ( -1.586052503253847057, 1.574803149606300412, -0.1653254495020572423 ) ) ;
#46257 = CARTESIAN_POINT ( 'NONE',  ( 0.9645669291338588858, 0.07958543189024085140, 0.2665933059059887866 ) ) ;
#46258 = CARTESIAN_POINT ( 'NONE',  ( 0.2624671916010504757, 0.2306618581243848609, 0.2411417322834645549 ) ) ;
#46259 = CARTESIAN_POINT ( 'NONE',  ( 0.6627296587926517768, -0.6692913385826773087, -0.1292274648535924053 ) ) ;
#46260 = CARTESIAN_POINT ( 'NONE',  ( 0.3460692066303959202, 0.1998031496062993295, -1.391076115485564424 ) ) ;
#46261 = CARTESIAN_POINT ( 'NONE',  ( -1.574803149606298636, -0.1870078740157479769, 0.4822834645669291653 ) ) ;
#46262 = CARTESIAN_POINT ( 'NONE',  ( -0.1070741851644056997, 0.3996062992125984925, -0.5557742782152230721 ) ) ;
#46263 = CARTESIAN_POINT ( 'NONE',  ( -0.1070741851644056997, 0.3996062992125984925, -0.3982939632545932085 ) ) ;
#46264 = CARTESIAN_POINT ( 'NONE',  ( -0.6299212598425188991, -0.1870078740157479769, 0.4822834645669291653 ) ) ;
#46265 = CARTESIAN_POINT ( 'NONE',  ( 0.4091458600556404646, -0.2362204724409448231, -0.1049868766404199460 ) ) ;
#46266 = CARTESIAN_POINT ( 'NONE',  ( 0.3392501089628018329, 0.1958661417322835607, -2.263123359580052618 ) ) ;
#46267 = CARTESIAN_POINT ( 'NONE',  ( -1.062992125984250968, -0.5511811023622047445, 6.969142054262312111E-17 ) ) ;
#46268 = CARTESIAN_POINT ( 'NONE',  ( 1.489501312335958172, -0.05778040916215560624, -0.4822834645669293319 ) ) ;
#46269 = CARTESIAN_POINT ( 'NONE',  ( 1.082677165354331228, 0.1660481256975883668, -0.3530559997133364547 ) ) ;
#46270 = CARTESIAN_POINT ( 'NONE',  ( -0.3149606299212590610, -0.1870078740157480601, -0.3641732283464567677 ) ) ;
#46271 = CARTESIAN_POINT ( 'NONE',  ( 0.4527559055118117182, -0.5400638737290844871, 0.3530559997133364547 ) ) ;
#46272 = CARTESIAN_POINT ( 'NONE',  ( 0.4724409448818897572, -0.1265901696524988906, -1.920603674540682038 ) ) ;
#46273 = CARTESIAN_POINT ( 'NONE',  ( -0.2427821522309703550, -0.2845877964562159024, 0.3641732283464567677 ) ) ;
#46274 = CARTESIAN_POINT ( 'NONE',  ( 0.06561679790026316017, 0.05413385826771626580, -0.4176697321401330321 ) ) ;
#46275 = CARTESIAN_POINT ( 'NONE',  ( -0.3949938075777408852, -0.1058382717557502933, -1.540026246719160108 ) ) ;
#46276 = CARTESIAN_POINT ( 'NONE',  ( -1.187664041994750175, -0.05778040916215560624, -0.4822834645669293319 ) ) ;
#46277 = CARTESIAN_POINT ( 'NONE',  ( 0.5314960629921264834, 0.07958543189024071263, -0.2665933059059888421 ) ) ;
#46278 = CARTESIAN_POINT ( 'NONE',  ( 1.220472440944882386, -0.1870078740157480046, 1.254653134982923898E-17 ) ) ;
#46279 = CARTESIAN_POINT ( 'NONE',  ( -0.5643044619422565855, 0.05413385826771626580, -0.4176697321401330321 ) ) ;
#46280 = CARTESIAN_POINT ( 'NONE',  ( -0.1049868766404193215, -0.5023911411419708095, 0.1820866141732285504 ) ) ;
#46281 = CARTESIAN_POINT ( 'NONE',  ( -1.614173228346457378, 0.2753471884572480932, 0.1372047244094471985 ) ) ;
#46282 = CARTESIAN_POINT ( 'NONE',  ( -0.5314960629921254842, -0.5400638737290845981, -0.3530559997133363437 ) ) ;
#46283 = CARTESIAN_POINT ( 'NONE',  ( -0.4658792650918627265, -0.3162353388693409650, -0.4822834645669289433 ) ) ;
#46284 = CARTESIAN_POINT ( 'NONE',  ( -0.01968503937007793844, 0.1660481256975883668, -0.3530559997133364547 ) ) ;
#46285 = CARTESIAN_POINT ( 'NONE',  ( -0.3460692066303960313, 0.1998031496062989965, -2.150262467191601079 ) ) ;
#46286 = EDGE_CURVE ( 'NONE', #38370, #82979, #73767, .T. ) ;
#46287 = CARTESIAN_POINT ( 'NONE',  ( 0.1049643490035304522, -0.3917322834645668994, -2.212579109415011569 ) ) ;
#46288 = CARTESIAN_POINT ( 'NONE',  ( -0.5314960629921123836, 2.677165354330708791, -3.900966923095591454 ) ) ;
#46289 = CARTESIAN_POINT ( 'NONE',  ( 0.7808398950131241190, -0.08942795157528024563, -0.3641732283464568787 ) ) ;
#46290 = CARTESIAN_POINT ( 'NONE',  ( 1.299212598425197429, 0.2952755905511811885, 0.000000000000000000 ) ) ;
#46291 = CARTESIAN_POINT ( 'NONE',  ( -0.8989501312335946848, 0.1771653543307087075, -0.09757992244046823083 ) ) ;
#46292 = CARTESIAN_POINT ( 'NONE',  ( -1.089238845144356427, -0.004921259842519576551, 0.3153832671262227771 ) ) ;
#46293 = ADVANCED_FACE ( 'NONE', ( #73877 ), #16216, .F. ) ;
#46294 = CARTESIAN_POINT ( 'NONE',  ( -0.8136482939632537770, 0.2306618581243847221, -0.2411417322834647770 ) ) ;
#46295 = CARTESIAN_POINT ( 'NONE',  ( 0.1049868766404206816, -0.6046776061558809534, -0.2411417322834644161 ) ) ;
#46296 = CARTESIAN_POINT ( 'NONE',  ( 0.5774278215223104249, 0.1283753931104748280, 0.1820866141732283561 ) ) ;
#46297 = CARTESIAN_POINT ( 'NONE',  ( -0.2710655044954047299, 0.1174279065223611113, 5.568826803765084321 ) ) ;
#46298 = CARTESIAN_POINT ( 'NONE',  ( 1.174540682414699111, -0.08942795157528024563, -0.3641732283464568787 ) ) ;
#46299 = AXIS2_PLACEMENT_3D ( 'NONE', #24642, #62127, #55797 ) ;
#46300 = CARTESIAN_POINT ( 'NONE',  ( 0.4658792650918641698, -0.05778040916215560624, -0.4822834645669293319 ) ) ;
#46301 = CARTESIAN_POINT ( 'NONE',  ( -0.2925321140481932369, 0.2925321140481931259, 0.06102362204724409017 ) ) ;
#46302 = CARTESIAN_POINT ( 'NONE',  ( -0.6955380577427815458, -0.4281496062992127816, -0.4176697321401328100 ) ) ;
#46303 = CARTESIAN_POINT ( 'NONE',  ( -0.3917322834645670104, -7.196005306013484475E-17, -1.541338582677165503 ) ) ;
#46304 = CARTESIAN_POINT ( 'NONE',  ( 1.286089238845145033, 0.1283753931104748280, 0.1820866141732283561 ) ) ;
#46305 = CARTESIAN_POINT ( 'NONE',  ( 0.5446194225721792126, -0.3162353388693405765, 0.4822834645669290543 ) ) ;
#46306 = CARTESIAN_POINT ( 'NONE',  ( 0.2427821522309719648, -0.05778040916215522460, 0.4822834645669289988 ) ) ;
#46307 = CARTESIAN_POINT ( 'NONE',  ( -0.09842519685039295696, -0.4536011799217367080, 0.2665933059059888421 ) ) ;
#46308 = DIRECTION ( 'NONE',  ( -1.000000000000000000, 0.000000000000000000, 0.000000000000000000 ) ) ;
#46309 = CARTESIAN_POINT ( 'NONE',  ( -0.1706036745406816491, -0.004921259842519870586, -0.3153832671262229437 ) ) ;
#46310 = CARTESIAN_POINT ( 'NONE',  ( 0.8792650918635177559, 0.05413385826771666132, 0.4176697321401328100 ) ) ;
#46311 = CARTESIAN_POINT ( 'NONE',  ( -0.7874015748031489847, -0.1870078740157479769, 0.3641732283464567677 ) ) ;
#46312 = AXIS2_PLACEMENT_3D ( 'NONE', #3283, #41168, #41577 ) ;
#46313 = CARTESIAN_POINT ( 'NONE',  ( -0.8202099737532799750, 0.2952755905511810774, -0.1292274648535930714 ) ) ;
#46314 = LINE ( 'NONE', #28630, #40740 ) ;
#46315 = ORIENTED_EDGE ( 'NONE', *, *, #78043, .F. ) ;
#46316 = CARTESIAN_POINT ( 'NONE',  ( -1.220472440944881054, -0.6692913385826771977, 8.415575281601705876E-17 ) ) ;
#46317 = CARTESIAN_POINT ( 'NONE',  ( -0.9120734908136475250, 0.1771653543307087630, 0.09757992244046791164 ) ) ;
#46318 = CARTESIAN_POINT ( 'NONE',  ( -0.1706036745406816491, -0.4281496062992124485, 0.4176697321401328655 ) ) ;
#46319 = CARTESIAN_POINT ( 'NONE',  ( -1.640419947506561060, -0.4281496062992127816, -0.4176697321401328100 ) ) ;
#46320 = CARTESIAN_POINT ( 'NONE',  ( -0.6430446194225712953, 0.05413385826771626580, -0.4176697321401330321 ) ) ;
#46321 = CARTESIAN_POINT ( 'NONE',  ( 0.4670766846051074284, 1.622013716815571716, -2.152792308923968889 ) ) ;
#46323 = CARTESIAN_POINT ( 'NONE',  ( 1.108923884514436242, -0.05778040916215522460, 0.4822834645669289988 ) ) ;
#46322 = CARTESIAN_POINT ( 'NONE',  ( 1.633858267716535639, -0.5400638737290844871, 0.3530559997133364547 ) ) ;
#46324 = CARTESIAN_POINT ( 'NONE',  ( 0.6955380577427828781, -0.4281496062992124485, 0.4176697321401328655 ) ) ;
#46325 = CARTESIAN_POINT ( 'NONE',  ( 0.1049643490035303689, 0.3917322834645670104, -2.347769028871391050 ) ) ;
#46326 = CARTESIAN_POINT ( 'NONE',  ( -1.559171609364246924, 0.2755905511811023723, 0.4177787735906735578 ) ) ;
#46327 = CARTESIAN_POINT ( 'NONE',  ( -1.528871391076114250, 0.2952755905511810774, -0.1292274648535930714 ) ) ;
#46328 = CARTESIAN_POINT ( 'NONE',  ( -0.3996062992125986035, -0.1070741851644056997, -0.04593175853018374721 ) ) ;
#46329 = ORIENTED_EDGE ( 'NONE', *, *, #23423, .T. ) ;
#46330 = CARTESIAN_POINT ( 'NONE',  ( -0.3937007874015740483, -0.1870078740157479769, 0.3641732283464567677 ) ) ;
#46331 = CARTESIAN_POINT ( 'NONE',  ( 0.1958661417322836440, -0.3392501089628017219, -1.816272965879265122 ) ) ;
#46332 = ORIENTED_EDGE ( 'NONE', *, *, #59403, .T. ) ;
#46333 = CARTESIAN_POINT ( 'NONE',  ( 0.1115485564304467270, -0.6692913385826773087, -0.1292274648535924053 ) ) ;
#46334 = CARTESIAN_POINT ( 'NONE',  ( 0.2362204724409456558, -0.1870078740157480879, -0.4822834645669291653 ) ) ;
#46335 = CARTESIAN_POINT ( 'NONE',  ( -0.7020997375328074108, -0.05778040916215522460, 0.4822834645669289988 ) ) ;
#46336 = CARTESIAN_POINT ( 'NONE',  ( 1.279527559055118724, -0.5400638737290845981, -0.3530559997133363437 ) ) ;
#46337 = CARTESIAN_POINT ( 'NONE',  ( -0.7086614173228339419, -0.1870078740157479769, 0.3641732283464567677 ) ) ;
#46338 = CARTESIAN_POINT ( 'NONE',  ( 0.8267716535433078384, -0.6692913385826771977, 8.415575281601705876E-17 ) ) ;
#46339 = CARTESIAN_POINT ( 'NONE',  ( 0.3937007874015754361, -0.1870078740157480601, -0.3641732283464567677 ) ) ;
#46340 = CARTESIAN_POINT ( 'NONE',  ( -0.2559055118110227234, -0.5400638737290844871, 0.3530559997133364547 ) ) ;
#46341 = CARTESIAN_POINT ( 'NONE',  ( 0.3392501089628018329, 0.1958661417322835052, -0.9986683482601557138 ) ) ;
#46342 = CARTESIAN_POINT ( 'NONE',  ( -0.6496062992125976043, 0.1660481256975883668, -0.3530559997133364547 ) ) ;
#46343 = CARTESIAN_POINT ( 'NONE',  ( 1.604771003085129433, 0.7270283685441705224, 0.1466069496707753106 ) ) ;
#46344 = CARTESIAN_POINT ( 'NONE',  ( 1.423884514435696413, -0.3162353388693409650, -0.4822834645669289433 ) ) ;
#46345 = CARTESIAN_POINT ( 'NONE',  ( 1.646981627296588035, -0.2845877964562159024, 0.3641732283464567677 ) ) ;
#46346 = ORIENTED_EDGE ( 'NONE', *, *, #42674, .F. ) ;
#46347 = CARTESIAN_POINT ( 'NONE',  ( 0.3917322834645670659, -0.1049643490035303273, -2.627972071687351363 ) ) ;
#46348 = CARTESIAN_POINT ( 'NONE',  ( -0.06561679790026180015, 0.05413385826771666132, 0.4176697321401328100 ) ) ;
#46349 = ORIENTED_EDGE ( 'NONE', *, *, #61973, .F. ) ;
#46350 = CARTESIAN_POINT ( 'NONE',  ( -1.351706036745406347, 0.05413385826771626580, -0.4176697321401330321 ) ) ;
#46351 = CARTESIAN_POINT ( 'NONE',  ( 1.607611548556431069, 0.2952755905511811885, 0.1292274648535926551 ) ) ;
#46352 = CARTESIAN_POINT ( 'NONE',  ( 1.456692913385827515, 0.2952755905511811885, 0.000000000000000000 ) ) ;
#46353 = B_SPLINE_CURVE_WITH_KNOTS ( 'NONE', 3,
 ( #75387, #30337, #74985, #48872, #5495, #42960, #49692, #68654 ),
 .UNSPECIFIED., .F., .F.,
 ( 4, 2, 2, 4 ),
 ( 0.07134069304684194368, 0.07377942048615132586, 0.07499878420580602389, 0.07621814792546072193 ),
 .UNSPECIFIED. ) ;
#46354 = CARTESIAN_POINT ( 'NONE',  ( 0.4133858267716541968, -0.5400638737290845981, -0.3530559997133363437 ) ) ;
#46355 = EDGE_CURVE ( 'NONE', #49627, #12829, #31604, .T. ) ;
#46356 = CARTESIAN_POINT ( 'NONE',  ( -0.1640419947506553400, -0.05778040916215560624, -0.4822834645669293319 ) ) ;
#46357 = CARTESIAN_POINT ( 'NONE',  ( 0.3917322834645670104, -0.1049643490035303411, -1.613517060367454237 ) ) ;
#46358 = CARTESIAN_POINT ( 'NONE',  ( -1.312335958005248715, -0.6046776061558809534, -0.2411417322834644161 ) ) ;
#46359 = CARTESIAN_POINT ( 'NONE',  ( -0.6955380577427815458, 0.05413385826771666132, 0.4176697321401328100 ) ) ;
#46360 =( GEOMETRIC_REPRESENTATION_CONTEXT ( 3 ) GLOBAL_UNCERTAINTY_ASSIGNED_CONTEXT ( ( #54574 ) ) GLOBAL_UNIT_ASSIGNED_CONTEXT ( ( #29310, #54137, #67624 ) ) REPRESENTATION_CONTEXT ( 'NONE', 'WORKASPACE' ) );
#46361 = CARTESIAN_POINT ( 'NONE',  ( -0.1443569553805765515, -0.3690944881889765550, -0.3153832671262227771 ) ) ;
#46362 = CARTESIAN_POINT ( 'NONE',  ( 1.528871391076116026, 0.2952755905511811885, 0.1292274648535926551 ) ) ;
#46363 = CARTESIAN_POINT ( 'NONE',  ( -0.6102362204724400829, 0.1660481256975885056, 0.3530559997133364547 ) ) ;
#46364 = CARTESIAN_POINT ( 'NONE',  ( -1.207349081364828880, 0.2306618581243847221, -0.2411417322834647770 ) ) ;
#46365 = CARTESIAN_POINT ( 'NONE',  ( 0.8267716535433077274, 0.2952755905511811885, 0.000000000000000000 ) ) ;
#46366 = CYLINDRICAL_SURFACE ( 'NONE', #63090, 3.543307086614173151 ) ;
#46367 = CARTESIAN_POINT ( 'NONE',  ( -0.1902887139107604098, 0.2952755905511810774, -0.1292274648535930714 ) ) ;
#46368 = CARTESIAN_POINT ( 'NONE',  ( -0.3674540682414692561, -0.5023911411419708095, -0.1820866141732282451 ) ) ;
#46370 = CARTESIAN_POINT ( 'NONE',  ( -0.9317585301837263412, 0.009842519685039463617, 0.3409548833797002576 ) ) ;
#46369 = CARTESIAN_POINT ( 'NONE',  ( 1.181102362204725198, -0.1870078740157479769, 0.3641732283464567677 ) ) ;
#46371 = CARTESIAN_POINT ( 'NONE',  ( 0.1265901696524990294, -0.4724409448818896462, -0.1620734908136483021 ) ) ;
#46372 = CARTESIAN_POINT ( 'NONE',  ( 1.686351706036745890, 0.1771653543307087630, 0.09757992244046791164 ) ) ;
#46373 = CARTESIAN_POINT ( 'NONE',  ( 1.292650918635171564, 0.2952755905511811885, 0.1292274648535926551 ) ) ;
#46374 = CONICAL_SURFACE ( 'NONE', #32925, 3.582677165354330562, 0.7853981633974415066 ) ;
#46375 = CARTESIAN_POINT ( 'NONE',  ( 0.3949938075777408852, 0.1058382717557500435, -0.04396325459317585588 ) ) ;
#46376 = CARTESIAN_POINT ( 'NONE',  ( -0.06561679790026180015, -0.4281496062992127816, -0.4176697321401328100 ) ) ;
#46377 = CARTESIAN_POINT ( 'NONE',  ( -1.561679790026246017, -0.4281496062992127816, -0.4176697321401328100 ) ) ;
#46378 = CARTESIAN_POINT ( 'NONE',  ( -1.686351706036744558, 0.2952755905511810774, -0.1292274648535930714 ) ) ;
#46379 = CARTESIAN_POINT ( 'NONE',  ( -0.3083989501312330295, -0.05778040916215522460, 0.4822834645669289988 ) ) ;
#46380 = CARTESIAN_POINT ( 'NONE',  ( 4.837279021331061486E-17, -0.3949938075777409963, -0.1555118110236220486 ) ) ;
#46381 = CARTESIAN_POINT ( 'NONE',  ( 1.653543307086614789, -0.1870078740157479769, 0.4822834645669291653 ) ) ;
#46382 = CARTESIAN_POINT ( 'NONE',  ( 0.6233595800524939223, -0.3162353388693405765, 0.4822834645669290543 ) ) ;
#46383 = CARTESIAN_POINT ( 'NONE',  ( 1.128608923884515169, -0.5023911411419708095, -0.1820866141732282451 ) ) ;
#46384 = CARTESIAN_POINT ( 'NONE',  ( 0.3129921259842520787, 1.496062992125984259, 0.000000000000000000 ) ) ;
#46385 = CARTESIAN_POINT ( 'NONE',  ( 0.4002624671916016896, -0.08942795157527998196, 0.3641732283464567121 ) ) ;
#46386 = CARTESIAN_POINT ( 'NONE',  ( -1.233595800524933894, -0.6046776061558809534, -0.2411417322834644161 ) ) ;
#46387 = CARTESIAN_POINT ( 'NONE',  ( 0.3460692066303959202, -0.1998031496062991630, -0.8116797900262466836 ) ) ;
#46388 = CARTESIAN_POINT ( 'NONE',  ( 1.240157480314961314, 0.1660481256975883668, -0.3530559997133364547 ) ) ;
#46389 = CARTESIAN_POINT ( 'NONE',  ( -0.2867679344610364334, -0.2867679344610367109, -0.5236220472440944462 ) ) ;
#46391 = CARTESIAN_POINT ( 'NONE',  ( 0.2362204724409451007, -0.4091458600556402980, -0.4835958005249343938 ) ) ;
#46390 = CARTESIAN_POINT ( 'NONE',  ( 0.4002624671916016896, -0.05778040916215522460, 0.4822834645669289988 ) ) ;
#46392 = CARTESIAN_POINT ( 'NONE',  ( 0.3025410870193226964, 2.784432375088962958E-17, -0.3464511005275205946 ) ) ;
#46393 = CARTESIAN_POINT ( 'NONE',  ( 0.3608923884514443348, 0.1771653543307087075, -0.09757992244046823083 ) ) ;
#46394 = CARTESIAN_POINT ( 'NONE',  ( 0.4986876640419954376, -0.6046776061558809534, -0.2411417322834644161 ) ) ;
#46395 = CARTESIAN_POINT ( 'NONE',  ( -0.7080320533160967544, 1.900312960331933976, 0.5309055118110236338 ) ) ;
#46396 = CARTESIAN_POINT ( 'NONE',  ( -0.9645669291338575535, -0.4536011799217367080, 0.2665933059059888421 ) ) ;
#46397 = CARTESIAN_POINT ( 'NONE',  ( -0.8398950131233589023, -0.6046776061558809534, -0.2411417322834644161 ) ) ;
#46398 = CARTESIAN_POINT ( 'NONE',  ( -1.673228346456691717, 0.1660481256975883668, -0.3530559997133364547 ) ) ;
#46399 = CARTESIAN_POINT ( 'NONE',  ( 0.8595800524934390507, -0.3162353388693405765, 0.4822834645669290543 ) ) ;
#46400 = CARTESIAN_POINT ( 'NONE',  ( 1.653543307086614789, -0.1870078740157479769, 0.4822834645669291653 ) ) ;
#46401 = CARTESIAN_POINT ( 'NONE',  ( -0.3963884504522706131, -0.02578378529929505406, -1.220472440944882608 ) ) ;
#46402 = CARTESIAN_POINT ( 'NONE',  ( 0.4724409448818904789, -0.1870078740157479769, 0.4822834645669291653 ) ) ;
#46403 = CARTESIAN_POINT ( 'NONE',  ( 0.2362204724409451007, -0.4091458600556402980, -2.845800524934383624 ) ) ;
#46404 = CARTESIAN_POINT ( 'NONE',  ( 1.607611548556431069, -0.6692913385826773087, -0.1292274648535924053 ) ) ;
#46405 = CARTESIAN_POINT ( 'NONE',  ( 1.299212598425197429, -0.6692913385826771977, 8.415575281601705876E-17 ) ) ;
#46406 = CARTESIAN_POINT ( 'NONE',  ( -1.640419947506561060, -0.3690944881889765550, -0.3153832671262227771 ) ) ;
#46407 = CARTESIAN_POINT ( 'NONE',  ( 1.364829396325460076, 0.1283753931104748280, 0.1820866141732283561 ) ) ;
#46408 = CARTESIAN_POINT ( 'NONE',  ( -1.187664041994749731, -0.2845877964562159024, 0.3641732283464567677 ) ) ;
#46409 = CARTESIAN_POINT ( 'NONE',  ( -0.2362204724409440182, -0.1870078740157479769, 0.3641732283464567677 ) ) ;
#46410 = CARTESIAN_POINT ( 'NONE',  ( -3.184294706754630777, 2.755905511811024056, 0.5314960629921260393 ) ) ;
#46411 = CARTESIAN_POINT ( 'NONE',  ( 0.3346456692913390985, 0.07958543189024085140, 0.2665933059059887866 ) ) ;
#46412 = CARTESIAN_POINT ( 'NONE',  ( 0.6824146981627303710, -0.6046776061558807314, 0.2411417322834647770 ) ) ;
#46413 = CARTESIAN_POINT ( 'NONE',  ( 1.272965879265092637, 0.05413385826771666132, 0.4176697321401328100 ) ) ;
#46414 = CARTESIAN_POINT ( 'NONE',  ( 0.1443569553805781891, 0.05413385826771626580, -0.4176697321401330321 ) ) ;
#46415 = EDGE_CURVE ( 'NONE', #53272, #74015, #35403, .T. ) ;
#46416 = CARTESIAN_POINT ( 'NONE',  ( -0.02624671916010428221, -0.5023911411419708095, 0.1820866141732285504 ) ) ;
#46417 = CARTESIAN_POINT ( 'NONE',  ( 1.043307086614173818, -0.5400638737290845981, -0.3530559997133363437 ) ) ;
#46418 = EDGE_CURVE ( 'NONE', #32355, #69205, #70286, .T. ) ;
#46419 = DIRECTION ( 'NONE',  ( 0.000000000000000000, -0.8660254037844387076, -0.4999999999999999445 ) ) ;
#46420 = CARTESIAN_POINT ( 'NONE',  ( -1.056430446194224881, 0.2952755905511810774, -0.1292274648535930714 ) ) ;
#46421 = CARTESIAN_POINT ( 'NONE',  ( 0.2925321140481932369, 0.2925321140481932369, -0.9251968503937008093 ) ) ;
#46422 = DIRECTION ( 'NONE',  ( 0.000000000000000000, -1.000000000000000000, 1.408710688920637755E-15 ) ) ;
#46423 = CARTESIAN_POINT ( 'NONE',  ( 0.1706036745406830368, 0.05413385826771666132, 0.4176697321401328100 ) ) ;
#46425 = AXIS2_PLACEMENT_3D ( 'NONE', #36435, #57836, #18730 ) ;
#46424 = CARTESIAN_POINT ( 'NONE',  ( -0.7808398950131222316, -0.3162353388693409650, -0.4822834645669289433 ) ) ;
#46426 = CARTESIAN_POINT ( 'NONE',  ( -0.2559055118110230564, 0.1660481256975883668, -0.3530559997133364547 ) ) ;
#46427 = CARTESIAN_POINT ( 'NONE',  ( 0.1998031496062992740, 0.3460692066303959757, -2.506561679790026087 ) ) ;
#46428 = CARTESIAN_POINT ( 'NONE',  ( -0.1974969037888706647, 0.3420746716998658843, -1.902887139107611869 ) ) ;
#46429 = CARTESIAN_POINT ( 'NONE',  ( 0.3917322834645670104, 2.398668435337828261E-17, -0.5826771653543306728 ) ) ;
#46430 = CARTESIAN_POINT ( 'NONE',  ( -0.3392501089628017219, -0.1958661417322836718, -0.8320209973753279753 ) ) ;
#46431 = CARTESIAN_POINT ( 'NONE',  ( -1.128608923884513837, -0.5023911411419708095, 0.1820866141732285504 ) ) ;
#46432 = CARTESIAN_POINT ( 'NONE',  ( 0.3917322834645669549, 0.1049643490035304660, -0.9041994750656167090 ) ) ;
#46433 = CARTESIAN_POINT ( 'NONE',  ( -1.719160104986876103, 0.05413385826771666132, 0.4176697321401328100 ) ) ;
#46434 = ADVANCED_FACE ( 'NONE', ( #69909 ), #26121, .T. ) ;
#46435 = CARTESIAN_POINT ( 'NONE',  ( -0.1974969037888704149, -0.3420746716998661063, -2.819553805774278388 ) ) ;
#46436 = CARTESIAN_POINT ( 'NONE',  ( 0.4593175853018380828, 0.05413385826771626580, -0.4176697321401330321 ) ) ;
#46437 = CARTESIAN_POINT ( 'NONE',  ( -0.4133858267716528645, 0.07958543189024071263, -0.2665933059059888421 ) ) ;
#46438 = EDGE_CURVE ( 'NONE', #37352, #37974, #50612, .T. ) ;
#46439 = CARTESIAN_POINT ( 'NONE',  ( 0.7677165354330716118, -0.5400638737290844871, 0.3530559997133364547 ) ) ;
#46440 = CARTESIAN_POINT ( 'NONE',  ( 0.4002624671916016896, -0.3162353388693409650, -0.4822834645669289433 ) ) ;
#46441 = CARTESIAN_POINT ( 'NONE',  ( 0.000000000000000000, 2.716535433070866645, 0.000000000000000000 ) ) ;
#46442 = CARTESIAN_POINT ( 'NONE',  ( 0.3460692066303959757, -0.1998031496062991907, -2.782152230971128848 ) ) ;
#46443 = CARTESIAN_POINT ( 'NONE',  ( 0.3392501089628018884, -0.1958661417322833942, -1.204087557251655394 ) ) ;
#46444 = CARTESIAN_POINT ( 'NONE',  ( 1.332020997375329197, -0.3162353388693405765, 0.4822834645669290543 ) ) ;
#46445 = CARTESIAN_POINT ( 'NONE',  ( 0.5511811023622054106, -0.1870078740157480879, -0.4822834645669291653 ) ) ;
#46446 = CARTESIAN_POINT ( 'NONE',  ( 0.1968503937007881344, 0.2952755905511811885, 0.000000000000000000 ) ) ;
#46447 = CARTESIAN_POINT ( 'NONE',  ( 1.332020997375328974, -0.05778040916215560624, -0.4822834645669293319 ) ) ;
#46448 = CARTESIAN_POINT ( 'NONE',  ( 1.082677165354331228, 0.1660481256975883668, -0.3530559997133364547 ) ) ;
#46449 = CARTESIAN_POINT ( 'NONE',  ( 0.1958661417322834775, 0.3392501089628018884, -0.7014435695538058235 ) ) ;
#46450 = CARTESIAN_POINT ( 'NONE',  ( 0.1049868766404206816, -0.6046776061558809534, -0.2411417322834644161 ) ) ;
#46451 = CARTESIAN_POINT ( 'NONE',  ( 0.8595800524934390507, -0.3162353388693405765, 0.4822834645669290543 ) ) ;
#46452 = CARTESIAN_POINT ( 'NONE',  ( -0.1837270341207340729, 0.2306618581243847221, -0.2411417322834647770 ) ) ;
#46453 = CARTESIAN_POINT ( 'NONE',  ( 1.279527559055118724, -0.4536011799217368745, -0.2665933059059886201 ) ) ;
#46454 = CARTESIAN_POINT ( 'NONE',  ( -1.482939632545930975, -0.4281496062992127816, -0.4176697321401328100 ) ) ;
#46455 = CARTESIAN_POINT ( 'NONE',  ( -1.351706036745406347, 0.05413385826771626580, -0.4176697321401330321 ) ) ;
#46456 = CARTESIAN_POINT ( 'NONE',  ( 0.7086614173228352742, -0.1870078740157480879, -0.4822834645669291653 ) ) ;
#46457 = CARTESIAN_POINT ( 'NONE',  ( 0.2143816077128068154, -0.3285422586328383132, -1.929133858267715551 ) ) ;
#46458 = CARTESIAN_POINT ( 'NONE',  ( -0.2867679344610365999, 0.2867679344610364889, -1.901574803149606252 ) ) ;
#46459 = ORIENTED_EDGE ( 'NONE', *, *, #66425, .F. ) ;
#46460 = CARTESIAN_POINT ( 'NONE',  ( 0.1070741851644054915, -0.3996062992125986035, -0.5577427821522309426 ) ) ;
#46461 = ORIENTED_EDGE ( 'NONE', *, *, #52742, .T. ) ;
#46462 = CARTESIAN_POINT ( 'NONE',  ( 1.122047244094488860, -0.5400638737290845981, -0.3530559997133363437 ) ) ;
#46463 = CARTESIAN_POINT ( 'NONE',  ( 1.030183727034121421, -0.2845877964562161244, -0.3641732283464567121 ) ) ;
#46464 = CARTESIAN_POINT ( 'NONE',  ( -0.7770624478417540448, -4.378520898609941727E-15, 0.4281989832122463091 ) ) ;
#46465 = CARTESIAN_POINT ( 'NONE',  ( -0.3634034883589671860, 1.231066118352837968, 2.723611671832316006 ) ) ;
#46466 = CARTESIAN_POINT ( 'NONE',  ( -0.4724409448818888135, -0.1265901696525008335, -1.148293963254593431 ) ) ;
#46467 = CARTESIAN_POINT ( 'NONE',  ( -0.3392501089628019995, 0.1958661417322832277, -1.370734908136483021 ) ) ;
#46468 = CARTESIAN_POINT ( 'NONE',  ( 1.161417322834646271, 0.1660481256975883668, -0.3530559997133364547 ) ) ;
#46469 = CARTESIAN_POINT ( 'NONE',  ( -1.528871391076114250, -0.6692913385826771977, 0.1292274648535927661 ) ) ;
#46470 = CARTESIAN_POINT ( 'NONE',  ( -0.4527559055118102749, 0.1660481256975885056, 0.3530559997133364547 ) ) ;
#46471 = CARTESIAN_POINT ( 'NONE',  ( 1.036745406824147508, -0.4281496062992127816, -0.4176697321401328100 ) ) ;
#46472 = ORIENTED_EDGE ( 'NONE', *, *, #23260, .T. ) ;
#46473 = CARTESIAN_POINT ( 'NONE',  ( -1.404199475065615932, 0.05413385826771666132, 0.4176697321401328100 ) ) ;
#46474 = CARTESIAN_POINT ( 'NONE',  ( 1.076935383196057305, 2.559055118110236560, 0.3149606299212599492 ) ) ;
#46475 = CARTESIAN_POINT ( 'NONE',  ( 0.000000000000000000, 2.755905511811024056, 0.000000000000000000 ) ) ;
#46476 = CARTESIAN_POINT ( 'NONE',  ( -1.043307086614172041, -0.4536011799217367080, 0.2665933059059888421 ) ) ;
#46477 = CARTESIAN_POINT ( 'NONE',  ( -1.397637795275589623, -0.5400638737290845981, -0.3530559997133363437 ) ) ;
#46478 = CARTESIAN_POINT ( 'NONE',  ( 0.4986876640419954376, -0.6046776061558809534, -0.2411417322834644161 ) ) ;
#46479 = AXIS2_PLACEMENT_3D ( 'NONE', #24524, #50190, #43867 ) ;
#46480 = ORIENTED_EDGE ( 'NONE', *, *, #27052, .T. ) ;
#46482 = CARTESIAN_POINT ( 'NONE',  ( -0.1938976377952756625, -0.1938976377952756625, -0.3740157480314971750 ) ) ;
#46481 = DIRECTION ( 'NONE',  ( 0.000000000000000000, 0.000000000000000000, -1.000000000000000000 ) ) ;
#46483 = CARTESIAN_POINT ( 'NONE',  ( 0.9317585301837276734, 0.05413385826771626580, -0.4176697321401330321 ) ) ;
#46484 = CARTESIAN_POINT ( 'NONE',  ( 1.587926509186352142, -0.004921259842519576551, 0.3153832671262227771 ) ) ;
#46485 = CARTESIAN_POINT ( 'NONE',  ( 0.3392501089628018329, 0.1958661417322835052, -0.6837077183388958757 ) ) ;
#46486 = CARTESIAN_POINT ( 'NONE',  ( -0.7874015748031489847, -0.1870078740157479769, 0.3641732283464567677 ) ) ;
#46487 = CARTESIAN_POINT ( 'NONE',  ( 1.633858267716535639, -0.5400638737290844871, 0.3530559997133364547 ) ) ;
#46488 = CARTESIAN_POINT ( 'NONE',  ( -1.157146581871515012E-16, 0.4724409448818898682, -0.7874015748031496509 ) ) ;
#46489 = CARTESIAN_POINT ( 'NONE',  ( 0.6364829396325465405, -0.05778040916215522460, 0.4822834645669289988 ) ) ;
#46490 = CARTESIAN_POINT ( 'NONE',  ( -0.8792650918635160906, -0.3690944881889763329, 0.3153832671262228327 ) ) ;
#46491 = CARTESIAN_POINT ( 'NONE',  ( 0.09186351706036799403, -0.3690944881889765550, -0.3153832671262227771 ) ) ;
#46492 = CARTESIAN_POINT ( 'NONE',  ( -0.4921259842519677963, -0.5400638737290844871, 0.3530559997133364547 ) ) ;
#46493 = CARTESIAN_POINT ( 'NONE',  ( -1.161417322834644716, 0.07958543189024085140, 0.2665933059059887866 ) ) ;
#46494 = CARTESIAN_POINT ( 'NONE',  ( -0.3392501089628019995, 0.1958661417322831999, 0.1344951199136988906 ) ) ;
#46495 = CARTESIAN_POINT ( 'NONE',  ( 0.9186351706036751663, -0.6046776061558807314, 0.2411417322834647770 ) ) ;
#46496 = ADVANCED_FACE ( 'NONE', ( #20238 ), #6352, .F. ) ;
#46497 = CARTESIAN_POINT ( 'NONE',  ( 0.4047984445375535922, 7.699586553780600482E-16, 0.3954985857520059711 ) ) ;
#46498 = CARTESIAN_POINT ( 'NONE',  ( -0.4091458600556405756, 0.2362204724409446288, -1.677821522309711266 ) ) ;
#46499 = CARTESIAN_POINT ( 'NONE',  ( -0.9514435695538050464, -0.3162353388693405765, 0.4822834645669290543 ) ) ;
#46500 = CARTESIAN_POINT ( 'NONE',  ( -0.2427821522309703550, -0.08942795157528024563, -0.3641732283464568787 ) ) ;
#46501 = CARTESIAN_POINT ( 'NONE',  ( -1.476377952755905110, 0.1660481256975885056, 0.3530559997133364547 ) ) ;
#46502 = CARTESIAN_POINT ( 'NONE',  ( 1.017060367454068803, -0.2845877964562159024, 0.3641732283464567677 ) ) ;
#46503 = CARTESIAN_POINT ( 'NONE',  ( -0.7020997375328076329, -0.2845877964562161244, -0.3641732283464567121 ) ) ;
#46504 = CARTESIAN_POINT ( 'NONE',  ( -1.017060367454067249, -0.3162353388693409650, -0.4822834645669289433 ) ) ;
#46505 = CARTESIAN_POINT ( 'NONE',  ( -1.194225721784776262, 0.05413385826771626580, -0.4176697321401330321 ) ) ;
#46506 = CARTESIAN_POINT ( 'NONE',  ( -1.555118110236219930, -0.5400638737290845981, -0.3530559997133363437 ) ) ;
#46507 = CARTESIAN_POINT ( 'NONE',  ( -0.1265901696524993347, 0.4724409448818896462, -2.130577427821521930 ) ) ;
#46508 = CARTESIAN_POINT ( 'NONE',  ( 1.076115485564305141, 0.1283753931104746893, -0.1820866141732285504 ) ) ;
#46509 = CARTESIAN_POINT ( 'NONE',  ( 0.4724409448818904789, -0.1870078740157480879, -0.4822834645669291653 ) ) ;
#46510 = CARTESIAN_POINT ( 'NONE',  ( -1.620734908136482577, 0.2952755905511811885, 0.1292274648535926551 ) ) ;
#46511 = CARTESIAN_POINT ( 'NONE',  ( -1.601049868766403650, -0.6046776061558807314, 0.2411417322834647770 ) ) ;
#46512 = ORIENTED_EDGE ( 'NONE', *, *, #18921, .F. ) ;
#46513 = CARTESIAN_POINT ( 'NONE',  ( 0.3996062992125986035, -0.1070741851644052972, -2.865485564304462329 ) ) ;
#46514 = CARTESIAN_POINT ( 'NONE',  ( -1.108923884514435132, -0.08942795157528024563, -0.3641732283464568787 ) ) ;
#46515 = CARTESIAN_POINT ( 'NONE',  ( -0.6561679790026240244, 0.2306618581243847221, -0.2411417322834647770 ) ) ;
#46516 = CARTESIAN_POINT ( 'NONE',  ( 0.7217847769028878924, -0.4281496062992127816, -0.4176697321401328100 ) ) ;
#46517 = AXIS2_PLACEMENT_3D ( 'NONE', #1067, #1478, #14535 ) ;
#46518 = CARTESIAN_POINT ( 'NONE',  ( -1.528871391076114250, 0.1771653543307087075, -0.09757992244046823083 ) ) ;
#46519 = CARTESIAN_POINT ( 'NONE',  ( -0.2925321140481932369, 0.2925321140481931259, -1.671259842519685179 ) ) ;
#46520 = CARTESIAN_POINT ( 'NONE',  ( -1.266404199475064773, -0.3162353388693405765, 0.4822834645669290543 ) ) ;
#46521 = VECTOR ( 'NONE', #82847, 39.37007874015748143 ) ;
#46522 = VECTOR ( 'NONE', #27138, 39.37007874015748143 ) ;
#46523 = CARTESIAN_POINT ( 'NONE',  ( 0.4790026246719168435, -0.3162353388693409650, -0.4822834645669289433 ) ) ;
#46524 = CARTESIAN_POINT ( 'NONE',  ( 0.6364829396325465405, -0.3162353388693409650, -0.4822834645669289433 ) ) ;
#46525 = CARTESIAN_POINT ( 'NONE',  ( 1.056430446194226436, -0.6692913385826773087, -0.1292274648535924053 ) ) ;
#46526 = CARTESIAN_POINT ( 'NONE',  ( 0.3996062992125985480, -0.1070741851644052972, -0.9757217847769029673 ) ) ;
#46527 = CARTESIAN_POINT ( 'NONE',  ( 0.1070741851644054915, -0.3996062992125986035, -1.345144356955380704 ) ) ;
#46528 = CARTESIAN_POINT ( 'NONE',  ( 0.1974969037888704704, 0.3420746716998660508, -0.4593175853018373056 ) ) ;
#46529 = CARTESIAN_POINT ( 'NONE',  ( 0.2470981898865924897, 1.132419612620494842, -1.607172560345370149 ) ) ;
#46530 = CARTESIAN_POINT ( 'NONE',  ( 0.2230971128608929543, -0.004921259842519870586, -0.3153832671262229437 ) ) ;
#46531 = CARTESIAN_POINT ( 'NONE',  ( 0.08530183727034192087, -0.3162353388693409650, -0.4822834645669289433 ) ) ;
#46532 = CARTESIAN_POINT ( 'NONE',  ( 1.272965879265092637, 0.05413385826771666132, 0.4176697321401328100 ) ) ;
#46533 = CARTESIAN_POINT ( 'NONE',  ( 4.837279021331061486E-17, -0.3949938075777409963, -1.730314960629921295 ) ) ;
#46534 = CARTESIAN_POINT ( 'NONE',  ( 0.4527559055118117182, 0.07958543189024071263, -0.2665933059059888421 ) ) ;
#46535 = CARTESIAN_POINT ( 'NONE',  ( -0.6627296587926501115, 0.2952755905511810774, -0.1292274648535930714 ) ) ;
#46536 = CARTESIAN_POINT ( 'NONE',  ( 1.482939632545932307, 0.05413385826771626580, -0.4176697321401330321 ) ) ;
#46537 = CARTESIAN_POINT ( 'NONE',  ( 0.3412073490813655186, -0.6046776061558809534, -0.2411417322834644161 ) ) ;
#46538 = CARTESIAN_POINT ( 'NONE',  ( 0.1265901696524990294, -0.4724409448818896462, -1.817585301837270517 ) ) ;
#46539 = CARTESIAN_POINT ( 'NONE',  ( 0.2661962643027124265, -0.2881610400590444709, -2.755905511811022723 ) ) ;
#46540 = TOROIDAL_SURFACE ( 'NONE', #10280, 0.1279527559055117503, 0.009842519685039369942 ) ;
#46541 = ORIENTED_EDGE ( 'NONE', *, *, #3802, .T. ) ;
#46542 = ORIENTED_EDGE ( 'NONE', *, *, #25459, .F. ) ;
#46543 = CARTESIAN_POINT ( 'NONE',  ( -1.541994750656167090, 0.2952755905511811885, 0.1292274648535926551 ) ) ;
#46544 = EDGE_CURVE ( 'NONE', #29401, #5577, #76242, .T. ) ;
#46546 = CARTESIAN_POINT ( 'NONE',  ( -1.312335958005248715, 0.2306618581243848609, 0.2411417322834645549 ) ) ;
#46545 = CARTESIAN_POINT ( 'NONE',  ( -1.122047244094487306, 0.07958543189024071263, -0.2665933059059888421 ) ) ;
#46547 = CARTESIAN_POINT ( 'NONE',  ( -0.3392501089628018329, -0.1958661417322836440, -2.494731340386139529 ) ) ;
#46548 = DIRECTION ( 'NONE',  ( 0.000000000000000000, 1.000000000000000000, 0.000000000000000000 ) ) ;
#46549 = CARTESIAN_POINT ( 'NONE',  ( -1.627296587926508442, 0.1283753931104748280, 0.1820866141732283561 ) ) ;
#46550 = CARTESIAN_POINT ( 'NONE',  ( -1.318897637795274802, -0.5400638737290845981, -0.3530559997133363437 ) ) ;
#46551 = CARTESIAN_POINT ( 'NONE',  ( -0.03280839895013062252, -0.6692913385826771977, 0.1292274648535927661 ) ) ;
#46552 = CARTESIAN_POINT ( 'NONE',  ( -1.089238845144356427, -0.4281496062992127816, -0.4176697321401328100 ) ) ;
#46553 = CARTESIAN_POINT ( 'NONE',  ( -0.3917322834645671215, 0.1049643490035301469, 0.1975065616797899160 ) ) ;
#46554 = CARTESIAN_POINT ( 'NONE',  ( 0.7349081364829402885, -0.6046776061558809534, -0.2411417322834644161 ) ) ;
#46555 = CARTESIAN_POINT ( 'NONE',  ( 0.1958661417322834775, 0.3392501089628018884, -1.711286089238845287 ) ) ;
#46556 = CARTESIAN_POINT ( 'NONE',  ( -1.410761154855641575, -0.2845877964562161244, -0.3641732283464567121 ) ) ;
#46557 = ORIENTED_EDGE ( 'NONE', *, *, #21129, .F. ) ;
#46558 = CARTESIAN_POINT ( 'NONE',  ( 0.3949938075777409963, 2.418639510665530435E-17, -2.165354330708661124 ) ) ;
#46559 = ORIENTED_EDGE ( 'NONE', *, *, #63918, .F. ) ;
#46560 = CARTESIAN_POINT ( 'NONE',  ( -1.719160104986876103, -0.004921259842519576551, 0.3153832671262227771 ) ) ;
#46561 = CARTESIAN_POINT ( 'NONE',  ( -1.332020997375327642, -0.3162353388693409650, -0.4822834645669289433 ) ) ;
#46562 = CARTESIAN_POINT ( 'NONE',  ( -1.299212598425196097, 0.2952755905511811885, 0.000000000000000000 ) ) ;
#46563 = CARTESIAN_POINT ( 'NONE',  ( 0.1998031496062992740, 0.3460692066303959757, -0.4593175853018372501 ) ) ;
#46564 = CARTESIAN_POINT ( 'NONE',  ( -1.732283464566928277, -0.1870078740157479769, 0.4822834645669291653 ) ) ;
#46565 = CARTESIAN_POINT ( 'NONE',  ( -1.509186351706035767, 0.05413385826771626580, -0.4176697321401330321 ) ) ;
#46566 = CARTESIAN_POINT ( 'NONE',  ( -1.476377952755905110, 0.1660481256975885056, 0.3530559997133364547 ) ) ;
#46567 = DIRECTION ( 'NONE',  ( -0.000000000000000000, 1.000000000000000000, -0.000000000000000000 ) ) ;
#46568 = EDGE_CURVE ( 'NONE', #73823, #38373, #71584, .T. ) ;
#46569 = CARTESIAN_POINT ( 'NONE',  ( 1.604771003085129433, 1.278209470906375156, -0.1466069496707750330 ) ) ;
#46570 = CARTESIAN_POINT ( 'NONE',  ( 0.1902887139107617975, -0.5511811023622048555, -0.09757992244046775898 ) ) ;
#46571 = CARTESIAN_POINT ( 'NONE',  ( -0.1958661417322834220, -0.3392501089628018884, -0.3077427821522311091 ) ) ;
#46572 = CARTESIAN_POINT ( 'NONE',  ( -0.9120734908136475250, 0.1771653543307087630, 0.09757992244046791164 ) ) ;
#46573 = CARTESIAN_POINT ( 'NONE',  ( -0.8989501312335946848, -0.6692913385826771977, 0.1292274648535927661 ) ) ;
#46574 = EDGE_CURVE ( 'NONE', #21301, #82069, #19821, .T. ) ;
#46575 = CARTESIAN_POINT ( 'NONE',  ( 0.8333333333333340365, 0.2952755905511810774, -0.1292274648535930714 ) ) ;
#46576 = CARTESIAN_POINT ( 'NONE',  ( -0.9448818897637790704, -0.1870078740157480879, -0.4822834645669291653 ) ) ;
#46577 = ORIENTED_EDGE ( 'NONE', *, *, #25498, .F. ) ;
#46578 = ORIENTED_EDGE ( 'NONE', *, *, #57708, .T. ) ;
#46579 = CARTESIAN_POINT ( 'NONE',  ( -0.8333333333333323711, 0.2952755905511811885, 0.1292274648535926551 ) ) ;
#46580 = CARTESIAN_POINT ( 'NONE',  ( 0.6758530183727039509, 0.2952755905511810774, -0.1292274648535930714 ) ) ;
#46581 = CARTESIAN_POINT ( 'NONE',  ( -1.620734908136482577, -0.5511811023622048555, -0.09757992244046775898 ) ) ;
#46582 = CARTESIAN_POINT ( 'NONE',  ( -1.699475065616797398, 0.2952755905511811885, 0.1292274648535926551 ) ) ;
#46583 = CARTESIAN_POINT ( 'NONE',  ( -0.2362204724409447953, -0.4091458600556404646, -1.325459317585301777 ) ) ;
#46584 = CARTESIAN_POINT ( 'NONE',  ( 2.153151837758401577, 1.453715418023198147, -0.4672341690643350698 ) ) ;
#46585 = CARTESIAN_POINT ( 'NONE',  ( 0.3917322834645669549, 0.1049643490035304660, -0.4317585301837270628 ) ) ;
#46586 = TOROIDAL_SURFACE ( 'NONE', #21061, 3.858267716535433323, 0.07874015748031495954 ) ;
#46587 = CARTESIAN_POINT ( 'NONE',  ( -0.3392501089628019995, 0.1958661417322832277, -2.315616797900262647 ) ) ;
#46588 = CARTESIAN_POINT ( 'NONE',  ( -0.3346456692913377662, 0.1660481256975883668, -0.3530559997133364547 ) ) ;
#46589 = CARTESIAN_POINT ( 'NONE',  ( -1.332020997375327642, -0.08942795157527998196, 0.3641732283464567121 ) ) ;
#46590 = CIRCLE ( 'NONE', #68115, 0.4724409448818898682 ) ;
#46591 = VECTOR ( 'NONE', #79812, 39.37007874015748143 ) ;
#46592 = CARTESIAN_POINT ( 'NONE',  ( -0.1070741851644056997, 0.3996062992125984925, 0.07414698162729654873 ) ) ;
#46594 = CARTESIAN_POINT ( 'NONE',  ( 0.06873123812453012238, 8.471767977567108961E-16, -0.4445507791589058955 ) ) ;
#46593 = CARTESIAN_POINT ( 'NONE',  ( -1.279527559055116948, -0.5400638737290844871, 0.3530559997133364547 ) ) ;
#46595 = CARTESIAN_POINT ( 'NONE',  ( -1.607611548556429737, -0.6692913385826771977, 0.1292274648535927661 ) ) ;
#46596 = CARTESIAN_POINT ( 'NONE',  ( -0.5643044619422565855, 0.05413385826771626580, -0.4176697321401330321 ) ) ;
#46597 = CARTESIAN_POINT ( 'NONE',  ( 0.3949938075777409963, 2.418639510665530743E-17, -2.872047244094488416 ) ) ;
#46598 = CARTESIAN_POINT ( 'NONE',  ( 0.5249343832021003964, 0.1283753931104746893, -0.1820866141732285504 ) ) ;
#46599 = CARTESIAN_POINT ( 'NONE',  ( 2.795275590551181466, 2.793565526369266916, 0.000000000000000000 ) ) ;
#46600 = CARTESIAN_POINT ( 'NONE',  ( 0.4724409448818904789, -0.1870078740157480601, -0.3641732283464567677 ) ) ;
#46601 = CARTESIAN_POINT ( 'NONE',  ( 1.213910761154856299, -0.5511811023622048555, -0.09757992244046775898 ) ) ;
#46602 = CARTESIAN_POINT ( 'NONE',  ( 1.115485564304462551, 0.05413385826771666132, 0.4176697321401328100 ) ) ;
#46603 = CARTESIAN_POINT ( 'NONE',  ( 0.1312335958005257930, 0.1283753931104746893, -0.1820866141732285504 ) ) ;
#46604 = CARTESIAN_POINT ( 'NONE',  ( 0.1049643490035304938, -0.3917322834645669549, -1.809711286089239035 ) ) ;
#46605 = CARTESIAN_POINT ( 'NONE',  ( -1.476377952755905110, 0.1660481256975885056, 0.3530559997133364547 ) ) ;
#46606 = CARTESIAN_POINT ( 'NONE',  ( -0.05905511811023545637, -0.4536011799217368745, -0.2665933059059886201 ) ) ;
#46607 = EDGE_CURVE ( 'NONE', #55113, #2780, #13897, .T. ) ;
#46608 = CARTESIAN_POINT ( 'NONE',  ( 0.4091458600556404646, -0.2362204724409448231, -0.1817585301837270351 ) ) ;
#46609 = CARTESIAN_POINT ( 'NONE',  ( -0.4330708661417315697, -0.5511811023622047445, 6.969142054262312111E-17 ) ) ;
#46610 = DIRECTION ( 'NONE',  ( -1.000000000000000000, 0.000000000000000000, 0.000000000000000000 ) ) ;
#46611 = CARTESIAN_POINT ( 'NONE',  ( 0.05249343832021075018, -0.6046776061558807314, 0.2411417322834647770 ) ) ;
#46612 = CARTESIAN_POINT ( 'NONE',  ( 0.4724409448818889246, 0.1265901696525005560, -0.6738845144356956363 ) ) ;
#46613 = EDGE_CURVE ( 'NONE', #62933, #17581, #65297, .T. ) ;
#46614 = CARTESIAN_POINT ( 'NONE',  ( 0.5118110236220478892, 0.1771653543307087630, 0.000000000000000000 ) ) ;
#46615 = CARTESIAN_POINT ( 'NONE',  ( -0.3805774278215216522, -0.3690944881889765550, -0.3153832671262227771 ) ) ;
#46616 = CARTESIAN_POINT ( 'NONE',  ( -0.3215223097112853146, -0.05778040916215560624, -0.4822834645669293319 ) ) ;
#46617 = CARTESIAN_POINT ( 'NONE',  ( -1.313877454013331780, 0.2929341459200028863, 0.7983292792091805090 ) ) ;
#46618 = CARTESIAN_POINT ( 'NONE',  ( -1.325459317585300889, -0.004921259842519576551, 0.3153832671262227771 ) ) ;
#46619 = CARTESIAN_POINT ( 'NONE',  ( 0.4624630002188662159, 0.1438724767639667779, -1.934761428466221789 ) ) ;
#46620 = CARTESIAN_POINT ( 'NONE',  ( 0.7283464566929143125, 0.1660481256975885056, 0.3530559997133364547 ) ) ;
#46621 = CARTESIAN_POINT ( 'NONE',  ( -0.7742782152230962556, -0.4281496062992127816, -0.4176697321401328100 ) ) ;
#46622 = CARTESIAN_POINT ( 'NONE',  ( -0.3996062992125986590, 0.1070741851644051723, -1.369422572178477404 ) ) ;
#46623 = CARTESIAN_POINT ( 'NONE',  ( 0.3917322834645670104, -0.1049643490035303411, -2.715879265091863726 ) ) ;
#46624 = CARTESIAN_POINT ( 'NONE',  ( -0.03280839895013062252, -0.5511811023622046335, 0.09757992244046803654 ) ) ;
#46625 = CARTESIAN_POINT ( 'NONE',  ( -1.017060367454067249, -0.05778040916215522460, 0.4822834645669289988 ) ) ;
#46626 = CARTESIAN_POINT ( 'NONE',  ( -1.056430446194224881, -0.5511811023622046335, 0.09757992244046803654 ) ) ;
#46627 = DIRECTION ( 'NONE',  ( 0.7071067811865462405, -0.000000000000000000, 0.7071067811865486830 ) ) ;
#46628 = CARTESIAN_POINT ( 'NONE',  ( -0.9645669291338575535, 0.07958543189024071263, -0.2665933059059888421 ) ) ;
#46629 = CARTESIAN_POINT ( 'NONE',  ( -0.4359958488159856316, 1.724409448818897905, 3.912791665790197992 ) ) ;
#46630 = CARTESIAN_POINT ( 'NONE',  ( 0.9645669291338588858, 0.1660481256975885056, 0.3530559997133364547 ) ) ;
#46631 = CARTESIAN_POINT ( 'NONE',  ( 0.2925321140481932369, -0.2925321140481932369, 0.05905511811023619884 ) ) ;
#46632 = CARTESIAN_POINT ( 'NONE',  ( 0.3392501089628018884, -0.1958661417322833942, -2.621410391897324832 ) ) ;
#46633 = FACE_BOUND ( 'NONE', #20577, .T. ) ;
#46634 = CARTESIAN_POINT ( 'NONE',  ( 1.509186351706037543, -0.3690944881889765550, -0.3153832671262227771 ) ) ;
#46635 = CARTESIAN_POINT ( 'NONE',  ( -1.358267716535432434, 0.1660481256975883668, -0.3530559997133364547 ) ) ;
#46636 = VECTOR ( 'NONE', #4705, 39.37007874015748143 ) ;
#46637 = CARTESIAN_POINT ( 'NONE',  ( 1.345144356955381593, -0.3162353388693409650, -0.4822834645669289433 ) ) ;
#46638 = CARTESIAN_POINT ( 'NONE',  ( 0.2867679344610365999, 0.2867679344610365999, -2.427165354330708347 ) ) ;
#46639 = CARTESIAN_POINT ( 'NONE',  ( 1.633858267716535639, -0.4536011799217367080, 0.2665933059059888421 ) ) ;
#46640 = CARTESIAN_POINT ( 'NONE',  ( 0.3346456692913393205, -0.5400638737290845981, -0.3530559997133363437 ) ) ;
#46641 = CARTESIAN_POINT ( 'NONE',  ( -0.5643044619422565855, -0.4281496062992124485, 0.4176697321401328655 ) ) ;
#46642 = PLANE ( 'NONE',  #38201 ) ;
#46643 = AXIS2_PLACEMENT_3D ( 'NONE', #19028, #62407, #24919 ) ;
#46645 = CARTESIAN_POINT ( 'NONE',  ( 3.937007874015748143, 1.537401574803149984, 2.901595197523589142E-16 ) ) ;
#46644 = CIRCLE ( 'NONE', #2265, 1.198416298106748767 ) ;
#46646 = CARTESIAN_POINT ( 'NONE',  ( 0.7742782152230978099, -0.3690944881889763329, 0.3153832671262228327 ) ) ;
#46647 = CARTESIAN_POINT ( 'NONE',  ( 0.3460692066303959202, 0.1998031496062993295, -1.548556430446194287 ) ) ;
#46648 = VERTEX_POINT ( 'NONE', #39164 ) ;
#46649 = CARTESIAN_POINT ( 'NONE',  ( -0.3917322834645670659, -7.196005306013484475E-17, -0.5085494995088732928 ) ) ;
#46650 = ORIENTED_EDGE ( 'NONE', *, *, #81093, .T. ) ;
#46651 = CARTESIAN_POINT ( 'NONE',  ( -0.4396325459317579898, 0.2952755905511811885, 0.1292274648535926551 ) ) ;
#46652 = PRODUCT ( 'Screw Bronze Bushing Sleeve Inserts', 'Screw Bronze Bushing Sleeve Inserts', '', ( #74669 ) ) ;
#46653 = CARTESIAN_POINT ( 'NONE',  ( 1.430446194225722500, 0.05413385826771666132, 0.4176697321401328100 ) ) ;
#46654 = CARTESIAN_POINT ( 'NONE',  ( 0.4002624671916016896, -0.05778040916215522460, 0.4822834645669289988 ) ) ;
#46655 = CARTESIAN_POINT ( 'NONE',  ( -0.3149606299212590610, -0.1870078740157480601, -0.3641732283464567677 ) ) ;
#46656 = CARTESIAN_POINT ( 'NONE',  ( 1.017060367454068803, -0.3162353388693405765, 0.4822834645669290543 ) ) ;
#46657 = CARTESIAN_POINT ( 'NONE',  ( -0.5905511811023613777, -0.6692913385826771977, 8.415575281601705876E-17 ) ) ;
#46658 = CARTESIAN_POINT ( 'NONE',  ( 0.1443569553805781891, -0.4281496062992124485, 0.4176697321401328655 ) ) ;
#46659 = CARTESIAN_POINT ( 'NONE',  ( -1.522309711286088607, -0.6046776061558807314, 0.2411417322834647770 ) ) ;
#46660 = CARTESIAN_POINT ( 'NONE',  ( 0.9711286089238851948, 0.2306618581243848609, 0.2411417322834645549 ) ) ;
#46661 = CARTESIAN_POINT ( 'NONE',  ( 1.082677165354331228, 0.1660481256975883668, -0.3530559997133364547 ) ) ;
#46662 = CARTESIAN_POINT ( 'NONE',  ( 0.1958661417322836440, -0.3392501089628017219, -0.7139107611548556331 ) ) ;
#46663 = CARTESIAN_POINT ( 'NONE',  ( 0.006561679790026889343, -0.2845877964562161244, -0.3641732283464567121 ) ) ;
#46664 = VERTEX_POINT ( 'NONE', #32859 ) ;
#46665 = CARTESIAN_POINT ( 'NONE',  ( -0.1058382717557503211, 0.3949938075777409408, -0.6364829396325458744 ) ) ;
#46666 = ORIENTED_EDGE ( 'NONE', *, *, #55977, .F. ) ;
#46667 = CARTESIAN_POINT ( 'NONE',  ( -0.4527559055118102749, 0.07958543189024085140, 0.2665933059059887866 ) ) ;
#46668 = CARTESIAN_POINT ( 'NONE',  ( 0.1246719160104994284, 0.2952755905511810774, -0.1292274648535930714 ) ) ;
#46669 = CARTESIAN_POINT ( 'NONE',  ( 2.867261597185502442, 1.070284760220068687, 0.08454815954498202946 ) ) ;
#46670 = CARTESIAN_POINT ( 'NONE',  ( -0.3018372703412066094, 0.05413385826771666132, 0.4176697321401328100 ) ) ;
#46671 = CARTESIAN_POINT ( 'NONE',  ( -0.4199475065616791736, 0.2306618581243847221, -0.2411417322834647770 ) ) ;
#46672 = CARTESIAN_POINT ( 'NONE',  ( -0.9383202099737524282, -0.3162353388693409650, -0.4822834645669289433 ) ) ;
#46673 = EDGE_CURVE ( 'NONE', #2570, #52886, #44702, .T. ) ;
#46674 = CARTESIAN_POINT ( 'NONE',  ( -1.200787401574802349, 0.1660481256975883668, -0.3530559997133364547 ) ) ;
#46675 = CARTESIAN_POINT ( 'NONE',  ( 1.325459317585302665, -0.3690944881889763329, 0.3153832671262228327 ) ) ;
#46676 = CARTESIAN_POINT ( 'NONE',  ( -0.5314960629921122726, 2.755905511811024056, -3.937007874015763687 ) ) ;
#46677 = CARTESIAN_POINT ( 'NONE',  ( -0.1471411879992342853, -4.378520898609941727E-15, 0.4281989832122466977 ) ) ;
#46678 = CARTESIAN_POINT ( 'NONE',  ( 0.7414698162729663755, -0.5511811023622048555, -0.09757992244046775898 ) ) ;
#46679 = CARTESIAN_POINT ( 'NONE',  ( 0.6299212598425204535, -0.1870078740157480879, -0.4822834645669291653 ) ) ;
#46680 = CARTESIAN_POINT ( 'NONE',  ( 0.2165354330708668673, -0.5400638737290844871, 0.3530559997133364547 ) ) ;
#46681 = CARTESIAN_POINT ( 'NONE',  ( -0.1998031496062994683, 0.3460692066303958092, -1.115485564304461885 ) ) ;
#46682 = CARTESIAN_POINT ( 'NONE',  ( -2.557182324916528859, 1.572090529166661588, 0.4732185887570796723 ) ) ;
#46683 = CARTESIAN_POINT ( 'NONE',  ( -9.787531504996566615E-17, 0.3996062992125985480, -0.5492125984251968740 ) ) ;
#46684 = CARTESIAN_POINT ( 'NONE',  ( -0.1998031496062994405, 0.3460692066303957537, -0.7198162729658792447 ) ) ;
#46685 = CARTESIAN_POINT ( 'NONE',  ( -0.4265091863517051496, 0.2952755905511810774, -0.1292274648535930714 ) ) ;
#46686 = CARTESIAN_POINT ( 'NONE',  ( -0.2362204724409451284, 0.4091458600556402425, -0.1706036745406823985 ) ) ;
#46687 = CARTESIAN_POINT ( 'NONE',  ( -0.3917322834645669549, -0.1049643490035306603, -2.177821522309711266 ) ) ;
#46688 = CARTESIAN_POINT ( 'NONE',  ( -1.043307086614172041, -0.4536011799217367080, 0.2665933059059888421 ) ) ;
#46689 = CARTESIAN_POINT ( 'NONE',  ( 0.9055118110236227702, -0.6692913385826771977, 8.415575281601705876E-17 ) ) ;
#46690 = CARTESIAN_POINT ( 'NONE',  ( 0.9776902887139113929, -0.6692913385826773087, -0.1292274648535924053 ) ) ;
#46691 = CARTESIAN_POINT ( 'NONE',  ( -0.2099737532808391705, 0.1283753931104748280, 0.1820866141732283561 ) ) ;
#46692 = CARTESIAN_POINT ( 'NONE',  ( 0.5118110236220478892, 0.2952755905511811885, 0.000000000000000000 ) ) ;
#46693 = CARTESIAN_POINT ( 'NONE',  ( 0.4091458600556404646, -0.2362204724409448231, -2.071522309711285814 ) ) ;
#46694 = CARTESIAN_POINT ( 'NONE',  ( 0.1312335958005257930, 0.1283753931104746893, -0.1820866141732285504 ) ) ;
#46695 = CARTESIAN_POINT ( 'NONE',  ( -0.2099737532808391705, -0.6046776061558809534, -0.2411417322834644161 ) ) ;
#46696 = CARTESIAN_POINT ( 'NONE',  ( 0.1058382717557500852, -0.3949938075777408852, -1.579396325459317740 ) ) ;
#46697 = CARTESIAN_POINT ( 'NONE',  ( -1.725721784776902190, -0.05778040916215522460, 0.4822834645669289988 ) ) ;
#46698 = CARTESIAN_POINT ( 'NONE',  ( 0.4593175853018379162, -0.3690944881889763329, 0.3153832671262228327 ) ) ;
#46699 = CARTESIAN_POINT ( 'NONE',  ( 1.033630966599880630, -4.927456884911482678E-16, 0.4445507791589062840 ) ) ;
#46700 = CARTESIAN_POINT ( 'NONE',  ( -0.7677165354330699465, 0.1660481256975885056, 0.3530559997133364547 ) ) ;
#46701 = CARTESIAN_POINT ( 'NONE',  ( -0.7742782152230962556, -0.3690944881889765550, -0.3153832671262227771 ) ) ;
#46702 = DIRECTION ( 'NONE',  ( -1.000000000000000000, 0.000000000000000000, 1.692413147294446216E-16 ) ) ;
#46703 = CARTESIAN_POINT ( 'NONE',  ( -0.6627296587926503335, -0.6692913385826771977, 0.1292274648535927661 ) ) ;
#46704 = CARTESIAN_POINT ( 'NONE',  ( -0.4790026246719152336, -0.05778040916215560624, -0.4822834645669293319 ) ) ;
#46705 = CARTESIAN_POINT ( 'NONE',  ( -0.006561679790025524116, -0.05778040916215560624, -0.4822834645669293319 ) ) ;
#46706 = CARTESIAN_POINT ( 'NONE',  ( 0.3460692066303959202, -0.1998031496062991630, -2.543963254593176071 ) ) ;
#46707 =( BOUNDED_CURVE ( )  B_SPLINE_CURVE ( 1, ( #31766, #44782 ),
 .UNSPECIFIED., .F., .F. ) 
 B_SPLINE_CURVE_WITH_KNOTS ( ( 2, 2 ),
 ( 0.000000000000000000, 0.002000000000000002644 ),
 .UNSPECIFIED. ) 
 CURVE ( )  GEOMETRIC_REPRESENTATION_ITEM ( )  RATIONAL_B_SPLINE_CURVE ( ( 0.9875488213027523443, 0.9875488213027523443 ) ) 
 REPRESENTATION_ITEM ( '' )  );
#46709 = CARTESIAN_POINT ( 'NONE',  ( -0.3917322834645669549, -7.196005306013483243E-17, -2.009167035924197098 ) ) ;
#46708 = AXIS2_PLACEMENT_3D ( 'NONE', #3882, #42581, #49307 ) ;
#46710 = CARTESIAN_POINT ( 'NONE',  ( -0.5314960629921123836, 2.702643891907236195, -3.896872718254348111 ) ) ;
#46711 = CARTESIAN_POINT ( 'NONE',  ( 0.7414698162729663755, 0.1771653543307087630, 0.09757992244046791164 ) ) ;
#46712 = CARTESIAN_POINT ( 'NONE',  ( 1.397637795275591177, -0.5400638737290844871, 0.3530559997133364547 ) ) ;
#46713 = CARTESIAN_POINT ( 'NONE',  ( -1.384514435695537005, 0.1771653543307087630, 0.09757992244046791164 ) ) ;
#46714 = CARTESIAN_POINT ( 'NONE',  ( -1.036745406824146176, -0.004921259842519870586, -0.3153832671262229437 ) ) ;
#46715 = CARTESIAN_POINT ( 'NONE',  ( -0.6955380577427815458, -0.4281496062992127816, -0.4176697321401328100 ) ) ;
#46716 = CARTESIAN_POINT ( 'NONE',  ( 0.09186351706036827158, -0.004921259842519576551, 0.3153832671262227771 ) ) ;
#46717 = DIRECTION ( 'NONE',  ( -0.000000000000000000, -1.000000000000000000, -0.000000000000000000 ) ) ;
#46718 = CARTESIAN_POINT ( 'NONE',  ( 0.9514435695538062676, -0.08942795157527998196, 0.3641732283464567121 ) ) ;
#46719 = CARTESIAN_POINT ( 'NONE',  ( 0.3477690288713918276, -0.6692913385826773087, -0.1292274648535924053 ) ) ;
#46720 = CARTESIAN_POINT ( 'NONE',  ( -0.1998031496062994405, 0.3460692066303957537, 0.2250656167979002698 ) ) ;
#46721 = CARTESIAN_POINT ( 'NONE',  ( -0.5774278215223089816, 0.2306618581243847221, -0.2411417322834647770 ) ) ;
#46722 = CARTESIAN_POINT ( 'NONE',  ( -0.3917322834645670104, -7.196005306013484475E-17, -1.226377952755905776 ) ) ;
#46723 = CARTESIAN_POINT ( 'NONE',  ( 1.561679790026247350, -0.3690944881889763329, 0.3153832671262228327 ) ) ;
#46724 = CARTESIAN_POINT ( 'NONE',  ( 0.4133858267716541968, 0.1660481256975885056, 0.3530559997133364547 ) ) ;
#46725 = CARTESIAN_POINT ( 'NONE',  ( 0.07217847769028949700, -0.3162353388693405765, 0.4822834645669290543 ) ) ;
#46726 = CARTESIAN_POINT ( 'NONE',  ( -0.01312335958005186876, -0.004921259842519870586, -0.3153832671262229437 ) ) ;
#46727 = CARTESIAN_POINT ( 'NONE',  ( 0.5639538267004613470, 0.004960608223780119466, 0.3437734562760182411 ) ) ;
#46728 = CARTESIAN_POINT ( 'NONE',  ( -0.2296587926509179312, -0.08942795157527998196, 0.3641732283464567121 ) ) ;
#46729 = CARTESIAN_POINT ( 'NONE',  ( 0.8727034120734913358, -0.05778040916215522460, 0.4822834645669289988 ) ) ;
#46730 = CARTESIAN_POINT ( 'NONE',  ( -0.8267716535433065062, -0.5511811023622047445, 6.969142054262312111E-17 ) ) ;
#46731 = CARTESIAN_POINT ( 'NONE',  ( -0.1070741851644056997, 0.3996062992125984925, -0.8707349081364830212 ) ) ;
#46732 = CARTESIAN_POINT ( 'NONE',  ( -1.135170603674539924, 0.2952755905511810774, -0.1292274648535930714 ) ) ;
#46733 = CARTESIAN_POINT ( 'NONE',  ( 0.1902887139107617975, 0.2066929133858267931, 0.1054918080437490802 ) ) ;
#46734 = EDGE_LOOP ( 'NONE', ( #9116, #4494 ) ) ;
#46735 = CARTESIAN_POINT ( 'NONE',  ( -1.364829396325458521, -0.6046776061558807314, 0.2411417322834647770 ) ) ;
#46736 = CARTESIAN_POINT ( 'NONE',  ( -1.240157480314959759, 0.07958543189024085140, 0.2665933059059887866 ) ) ;
#46737 = CARTESIAN_POINT ( 'NONE',  ( 0.1115485564304467270, -0.6692913385826773087, -0.1292274648535924053 ) ) ;
#46738 = CARTESIAN_POINT ( 'NONE',  ( -1.476377952755905110, -0.5400638737290845981, -0.3530559997133363437 ) ) ;
#46739 = CARTESIAN_POINT ( 'NONE',  ( -0.6561679790026240244, 0.2306618581243847221, -0.2411417322834647770 ) ) ;
#46740 = DIRECTION ( 'NONE',  ( -3.096699300667737957E-16, 1.000000000000000000, -0.000000000000000000 ) ) ;
#46742 = CARTESIAN_POINT ( 'NONE',  ( 1.141732283464567566, 0.2952755905511811885, 0.000000000000000000 ) ) ;
#46741 = CARTESIAN_POINT ( 'NONE',  ( 1.601049868766404982, -0.6046776061558809534, -0.2411417322834644161 ) ) ;
#46743 = CARTESIAN_POINT ( 'NONE',  ( 0.9645669291338591078, -0.5400638737290845981, -0.3530559997133363437 ) ) ;
#46744 = CARTESIAN_POINT ( 'NONE',  ( 0.2867679344610366554, -0.2867679344610365444, -2.295275590551181022 ) ) ;
#46745 = CARTESIAN_POINT ( 'NONE',  ( 1.587926509186352142, 0.05413385826771666132, 0.4176697321401328100 ) ) ;
#46746 = CARTESIAN_POINT ( 'NONE',  ( -1.496062992125983815, -0.1870078740157480879, -0.4822834645669291653 ) ) ;
#46747 = CARTESIAN_POINT ( 'NONE',  ( -0.1998031496062991907, -0.3460692066303959757, -0.3805774278215223183 ) ) ;
#46748 = VERTEX_POINT ( 'NONE', #47980 ) ;
#46749 = CARTESIAN_POINT ( 'NONE',  ( -0.4855643044619415427, -0.004921259842519870586, -0.3153832671262229437 ) ) ;
#46750 = CARTESIAN_POINT ( 'NONE',  ( -0.3392501089628019995, 0.1958661417322832277, -2.380577427821522374 ) ) ;
#46751 = ORIENTED_EDGE ( 'NONE', *, *, #6175, .T. ) ;
#46752 = CARTESIAN_POINT ( 'NONE',  ( 0.2559055118110243332, -0.5400638737290845981, -0.3530559997133363437 ) ) ;
#46753 = CARTESIAN_POINT ( 'NONE',  ( -0.07874015748031421014, -0.1870078740157480879, -0.4822834645669291653 ) ) ;
#46754 = CARTESIAN_POINT ( 'NONE',  ( -0.8005249343832011588, 0.05413385826771626580, -0.4176697321401330321 ) ) ;
#46755 = CARTESIAN_POINT ( 'NONE',  ( 1.364829396325460076, 0.2306618581243848609, 0.2411417322834645549 ) ) ;
#46756 = CARTESIAN_POINT ( 'NONE',  ( -1.030183727034119867, -0.2845877964562159024, 0.3641732283464567677 ) ) ;
#46757 = CARTESIAN_POINT ( 'NONE',  ( 0.05807346738891932397, 1.066559990163497229, -1.546459320796472303 ) ) ;
#46758 = CARTESIAN_POINT ( 'NONE',  ( 0.8202099737532814183, -0.6692913385826773087, -0.1292274648535924053 ) ) ;
#46759 = CARTESIAN_POINT ( 'NONE',  ( 0.4593175853018379162, -0.3690944881889763329, 0.3153832671262228327 ) ) ;
#46760 = CARTESIAN_POINT ( 'NONE',  ( -0.4527559055118102749, -0.5400638737290845981, -0.3530559997133363437 ) ) ;
#46761 = CARTESIAN_POINT ( 'NONE',  ( 0.2867679344610365999, -0.2867679344610365999, -0.9658599493100242794 ) ) ;
#46762 = CARTESIAN_POINT ( 'NONE',  ( -1.128608923884513837, 0.2306618581243847221, -0.2411417322834647770 ) ) ;
#46763 = CARTESIAN_POINT ( 'NONE',  ( -1.607611548556429737, -0.5511811023622046335, 0.09757992244046803654 ) ) ;
#46764 = EDGE_CURVE ( 'NONE', #6265, #40586, #46314, .T. ) ;
#46765 = CARTESIAN_POINT ( 'NONE',  ( 1.430446194225722500, -0.4281496062992127816, -0.4176697321401328100 ) ) ;
#46766 = CARTESIAN_POINT ( 'NONE',  ( 1.535433070866142558, 0.1771653543307087630, 0.000000000000000000 ) ) ;
#46767 = VERTEX_POINT ( 'NONE', #14363 ) ;
#46768 = CARTESIAN_POINT ( 'NONE',  ( -0.1049643490035302301, -0.3917322834645671770, -2.431121677986564311 ) ) ;
#46769 = CARTESIAN_POINT ( 'NONE',  ( 0.1574803149606306130, -0.1870078740157480879, -0.4822834645669291653 ) ) ;
#46770 = ORIENTED_EDGE ( 'NONE', *, *, #67786, .F. ) ;
#46771 = VECTOR ( 'NONE', #50851, 39.37007874015748143 ) ;
#46772 = CARTESIAN_POINT ( 'NONE',  ( 0.8595800524934390507, -0.08942795157528024563, -0.3641732283464568787 ) ) ;
#46773 = CARTESIAN_POINT ( 'NONE',  ( -1.286089238845143479, -0.6046776061558807314, 0.2411417322834647770 ) ) ;
#46774 = CARTESIAN_POINT ( 'NONE',  ( 1.049868766404200127, -0.6046776061558809534, -0.2411417322834644161 ) ) ;
#46775 = CARTESIAN_POINT ( 'NONE',  ( 1.227034120734908917, -0.6692913385826771977, 0.1292274648535927661 ) ) ;
#46776 = CARTESIAN_POINT ( 'NONE',  ( 0.1902887139107617975, 0.2952755905511811885, 0.1292274648535926551 ) ) ;
#46777 = CARTESIAN_POINT ( 'NONE',  ( -0.4133858267716528645, -0.5400638737290844871, 0.3530559997133364547 ) ) ;
#46778 = CARTESIAN_POINT ( 'NONE',  ( -0.3917322834645670104, -7.196005306013484475E-17, -2.013779527559055094 ) ) ;
#46779 = CARTESIAN_POINT ( 'NONE',  ( -1.253280839895012377, -0.05778040916215522460, 0.4822834645669289988 ) ) ;
#46780 = CARTESIAN_POINT ( 'NONE',  ( -0.7677165354330699465, -0.5400638737290845981, -0.3530559997133363437 ) ) ;
#46781 = CARTESIAN_POINT ( 'NONE',  ( -0.4330708661417315697, -0.5511811023622047445, 6.969142054262312111E-17 ) ) ;
#46782 = CARTESIAN_POINT ( 'NONE',  ( 1.640419947506562393, -0.4281496062992124485, 0.4176697321401328655 ) ) ;
#46783 = CARTESIAN_POINT ( 'NONE',  ( -0.7152230971128602510, -0.05778040916215560624, -0.4822834645669293319 ) ) ;
#46784 = DIRECTION ( 'NONE',  ( -3.491481338843132961E-15, -0.000000000000000000, 1.000000000000000000 ) ) ;
#46785 = CARTESIAN_POINT ( 'NONE',  ( 0.6496062992125991586, 0.1660481256975885056, 0.3530559997133364547 ) ) ;
#46786 = CARTESIAN_POINT ( 'NONE',  ( -0.3460692066303958092, -0.1998031496062994683, -1.784776902887138972 ) ) ;
#46787 = CARTESIAN_POINT ( 'NONE',  ( 0.8785612751854029456, 3.421639014772782816E-16, 0.3464511005275203726 ) ) ;
#46788 = CARTESIAN_POINT ( 'NONE',  ( -0.3215223097112853146, -0.05778040916215560624, -0.4822834645669293319 ) ) ;
#46790 = CARTESIAN_POINT ( 'NONE',  ( -1.603475055217291612, 0.4410854135902512185, 0.04573490813648251746 ) ) ;
#46789 = CARTESIAN_POINT ( 'NONE',  ( 0.8333333333333340365, -0.5511811023622046335, 0.09757992244046803654 ) ) ;
#46791 = CARTESIAN_POINT ( 'NONE',  ( -0.3458507752293906723, -0.3458507752293910609, -0.6082677165354329896 ) ) ;
#46792 = CARTESIAN_POINT ( 'NONE',  ( 1.095800524934383846, -0.08942795157528024563, -0.3641732283464568787 ) ) ;
#46793 = CARTESIAN_POINT ( 'NONE',  ( 1.089238845144357537, -0.4281496062992124485, 0.4176697321401328655 ) ) ;
#46794 = CARTESIAN_POINT ( 'NONE',  ( 0.3420746716998660508, 0.1974969037888705814, -0.05052493438320211638 ) ) ;
#46795 = CARTESIAN_POINT ( 'NONE',  ( -0.5183727034120726440, -0.6692913385826773087, -0.1292274648535924053 ) ) ;
#46796 = CARTESIAN_POINT ( 'NONE',  ( -1.515748031496062076, -0.5400638737290844871, 0.3530559997133364547 ) ) ;
#46797 = CARTESIAN_POINT ( 'NONE',  ( -1.646981627296586703, -0.3162353388693409650, -0.4822834645669289433 ) ) ;
#46798 = CARTESIAN_POINT ( 'NONE',  ( -0.05249343832020938322, -0.6046776061558809534, -0.2411417322834644161 ) ) ;
#46799 = CARTESIAN_POINT ( 'NONE',  ( -0.3949938075777409963, -7.255918531996591613E-17, -0.4311023622047245318 ) ) ;
#46800 = CARTESIAN_POINT ( 'NONE',  ( 1.167979002624672580, -0.4281496062992124485, 0.4176697321401328655 ) ) ;
#46801 = CARTESIAN_POINT ( 'NONE',  ( 0.6430446194225728496, 0.05413385826771666132, 0.4176697321401328100 ) ) ;
#46802 = CARTESIAN_POINT ( 'NONE',  ( 1.161417322834646493, -0.4536011799217367080, 0.2665933059059888421 ) ) ;
#46803 = CARTESIAN_POINT ( 'NONE',  ( 0.3125698167429954988, 1.368940321741649369, 0.01652806838128066322 ) ) ;
#46804 = CARTESIAN_POINT ( 'NONE',  ( 0.4133858267716541968, 0.07958543189024085140, 0.2665933059059887866 ) ) ;
#46805 = CARTESIAN_POINT ( 'NONE',  ( -1.076115485564303809, 0.1539470093639523085, 0.1968503937007873850 ) ) ;
#46806 = CARTESIAN_POINT ( 'NONE',  ( 0.1998031496062994128, -0.3460692066303957537, -1.270997375328084100 ) ) ;
#46807 = CARTESIAN_POINT ( 'NONE',  ( 0.6233595800524942554, -0.05778040916215560624, -0.4822834645669293319 ) ) ;
#46808 = CARTESIAN_POINT ( 'NONE',  ( -0.3392501089628019995, 0.1958661417322832277, -0.4908136482939632339 ) ) ;
#46810 = CARTESIAN_POINT ( 'NONE',  ( 0.6423408027444581503, 0.000000000000000000, 0.3464511005275205946 ) ) ;
#46809 = CARTESIAN_POINT ( 'NONE',  ( 0.2690288713910767848, 0.2952755905511811885, 0.1292274648535926551 ) ) ;
#46811 = CARTESIAN_POINT ( 'NONE',  ( 0.000000000000000000, 0.000000000000000000, 0.1574803149606299191 ) ) ;
#46812 = CARTESIAN_POINT ( 'NONE',  ( 0.2624671916010504757, -0.5023911411419708095, -0.1820866141732282451 ) ) ;
#46813 = CARTESIAN_POINT ( 'NONE',  ( 0.3477690288713918276, -0.6692913385826773087, -0.1292274648535924053 ) ) ;
#46814 = CARTESIAN_POINT ( 'NONE',  ( 0.7283464566929142014, 0.1012011053420777407, 0.2882089793578256898 ) ) ;
#46815 = CARTESIAN_POINT ( 'NONE',  ( -0.7874015748031489847, -0.1870078740157479769, 0.3641732283464567677 ) ) ;
#46816 = CARTESIAN_POINT ( 'NONE',  ( -1.023622047244094002, -0.1870078740157480879, -0.4822834645669291653 ) ) ;
#46817 = CARTESIAN_POINT ( 'NONE',  ( -1.351706036745406347, 0.05413385826771626580, -0.4176697321401330321 ) ) ;
#46818 = CARTESIAN_POINT ( 'NONE',  ( 0.4921259842519691285, -0.5400638737290845981, -0.3530559997133363437 ) ) ;
#46819 = CARTESIAN_POINT ( 'NONE',  ( 1.437007874015748810, -0.5400638737290845981, -0.3530559997133363437 ) ) ;
#46820 = CARTESIAN_POINT ( 'NONE',  ( -1.559171609364246924, 1.299212598425196985, 0.4177787735906735578 ) ) ;
#46821 = CARTESIAN_POINT ( 'NONE',  ( 0.5511811023622054106, -0.1870078740157480879, -0.4822834645669291653 ) ) ;
#46822 = CARTESIAN_POINT ( 'NONE',  ( -0.3458507752293909498, 0.3458507752293907833, -2.773622047244094002 ) ) ;
#46823 = CARTESIAN_POINT ( 'NONE',  ( 4.821444151489972621E-16, 1.062992125984252745, 3.937007874015748143 ) ) ;
#46824 = CARTESIAN_POINT ( 'NONE',  ( 1.371391076115485941, 0.2952755905511811885, 0.1292274648535926551 ) ) ;
#46825 = CARTESIAN_POINT ( 'NONE',  ( -1.292650918635170010, -0.5511811023622046335, 0.09757992244046803654 ) ) ;
#46826 = CARTESIAN_POINT ( 'NONE',  ( 1.312335958005250269, -0.5023911411419708095, 0.1820866141732285504 ) ) ;
#46827 = CARTESIAN_POINT ( 'NONE',  ( -1.496062992125983815, -0.1870078740157479769, 0.3641732283464567677 ) ) ;
#46828 = CARTESIAN_POINT ( 'NONE',  ( -0.6430446194225712953, -0.004921259842519870586, -0.3153832671262229437 ) ) ;
#46829 = CARTESIAN_POINT ( 'NONE',  ( -3.210901144579272781, 2.729659898143634411, 0.5314960629921260393 ) ) ;
#46830 = CARTESIAN_POINT ( 'NONE',  ( 0.5839895013123367340, -0.5511811023622048555, -0.09757992244046775898 ) ) ;
#46831 = CARTESIAN_POINT ( 'NONE',  ( 8.195543980992789655E-16, -0.1870078740157480879, -0.4822834645669291653 ) ) ;
#46832 = CARTESIAN_POINT ( 'NONE',  ( 1.023622047244095112, -0.1870078740157480879, -0.4822834645669291653 ) ) ;
#46833 = CARTESIAN_POINT ( 'NONE',  ( 0.2099737532808405305, -0.6046776061558807314, 0.2411417322834647770 ) ) ;
#46834 = CARTESIAN_POINT ( 'NONE',  ( 0.01968503937007930540, 0.07958543189024085140, 0.2665933059059887866 ) ) ;
#46835 = CARTESIAN_POINT ( 'NONE',  ( 1.266404199475066328, -0.05778040916215522460, 0.4822834645669289988 ) ) ;
#46836 = PLANE ( 'NONE',  #3032 ) ;
#46837 = CARTESIAN_POINT ( 'NONE',  ( -0.9120734908136475250, 0.2952755905511811885, 0.1292274648535926551 ) ) ;
#46838 = CARTESIAN_POINT ( 'NONE',  ( -0.3460692066303960868, 0.1998031496062990242, -0.9711286089238845287 ) ) ;
#46839 = CARTESIAN_POINT ( 'NONE',  ( 0.3460692066303959202, -0.1998031496062991630, -2.858923884514435798 ) ) ;
#46840 = CARTESIAN_POINT ( 'NONE',  ( -1.017060367454067249, -0.05778040916215522460, 0.4822834645669289988 ) ) ;
#46841 = CARTESIAN_POINT ( 'NONE',  ( -0.01312335958005186876, -0.4281496062992124485, 0.4176697321401328655 ) ) ;
#46842 = CARTESIAN_POINT ( 'NONE',  ( -0.1998031496062994683, 0.3460692066303958092, -2.532808398950130879 ) ) ;
#46843 = CARTESIAN_POINT ( 'NONE',  ( 0.1058382717557499880, 0.3949938075777411073, -1.725721784776902856 ) ) ;
#46844 = CARTESIAN_POINT ( 'NONE',  ( 0.1049643490035303689, 0.3917322834645670104, -0.6154855643044617741 ) ) ;
#46845 = CARTESIAN_POINT ( 'NONE',  ( 3.890406373195415490, 2.716724272663529227, -0.5314960629921260393 ) ) ;
#46846 = CARTESIAN_POINT ( 'NONE',  ( -1.450131233595799651, -0.5511811023622046335, 0.09757992244046803654 ) ) ;
#46847 = CARTESIAN_POINT ( 'NONE',  ( 0.3392501089628018884, -0.1958661417322834220, -1.041994750656167756 ) ) ;
#46848 = CARTESIAN_POINT ( 'NONE',  ( -1.607611548556429737, -0.6692913385826771977, 0.1292274648535927661 ) ) ;
#46849 = CARTESIAN_POINT ( 'NONE',  ( -9.594673741351310580E-17, 0.3917322834645669549, 0.07744713730414881647 ) ) ;
#46850 = CARTESIAN_POINT ( 'NONE',  ( 0.4658792650918641698, -0.05778040916215560624, -0.4822834645669293319 ) ) ;
#46851 = CARTESIAN_POINT ( 'NONE',  ( -0.5577427821522301654, -0.08942795157528024563, -0.3641732283464568787 ) ) ;
#46853 = EDGE_CURVE ( 'NONE', #20068, #65211, #33701, .T. ) ;
#46852 = CARTESIAN_POINT ( 'NONE',  ( 1.036745406824147508, -0.4281496062992127816, -0.4176697321401328100 ) ) ;
#46854 = CARTESIAN_POINT ( 'NONE',  ( 0.4855643044619428750, 0.05413385826771666132, 0.4176697321401328100 ) ) ;
#46855 = DIRECTION ( 'NONE',  ( 0.000000000000000000, 0.000000000000000000, -1.000000000000000000 ) ) ;
#46856 = CARTESIAN_POINT ( 'NONE',  ( -0.3996062992125987146, 0.1070741851644051862, -2.552493438320210029 ) ) ;
#46857 = CARTESIAN_POINT ( 'NONE',  ( 0.2867679344610366554, -0.2867679344610365999, -1.197525877461629307 ) ) ;
#46858 = CARTESIAN_POINT ( 'NONE',  ( 1.292650918635171564, -0.6692913385826773087, -0.1292274648535924053 ) ) ;
#46859 = CARTESIAN_POINT ( 'NONE',  ( 0.1771653543307093182, 0.1660481256975885056, 0.3530559997133364547 ) ) ;
#46860 = CARTESIAN_POINT ( 'NONE',  ( 1.489501312335958172, -0.05778040916215560624, -0.4822834645669293319 ) ) ;
#46861 = CARTESIAN_POINT ( 'NONE',  ( 0.6955380577427828781, -0.4281496062992124485, 0.4176697321401328655 ) ) ;
#46862 = CARTESIAN_POINT ( 'NONE',  ( -9.594673741351313045E-17, 0.3917322834645670104, -0.5570866141732284671 ) ) ;
#46863 = CARTESIAN_POINT ( 'NONE',  ( 0.07217847769028949700, -0.05778040916215560624, -0.4822834645669293319 ) ) ;
#46864 = CARTESIAN_POINT ( 'NONE',  ( 0.7086614173228353852, -0.1870078740157479769, 0.4822834645669291653 ) ) ;
#46865 = CARTESIAN_POINT ( 'NONE',  ( -0.08530183727034056085, -0.3162353388693405765, 0.4822834645669290543 ) ) ;
#46866 = CARTESIAN_POINT ( 'NONE',  ( 0.5643044619422579178, -0.004921259842519576551, 0.3153832671262227771 ) ) ;
#46867 = CARTESIAN_POINT ( 'NONE',  ( -1.450131233595799651, -0.6692913385826771977, 0.1292274648535927661 ) ) ;
#46868 = CARTESIAN_POINT ( 'NONE',  ( -1.548556430446193399, 0.2306618581243848609, 0.2411417322834645549 ) ) ;
#46869 = CARTESIAN_POINT ( 'NONE',  ( 0.6233595800524939223, -0.3162353388693405765, 0.4822834645669290543 ) ) ;
#46870 = CARTESIAN_POINT ( 'NONE',  ( -0.1789624962996142488, -0.3486222174635806859, -1.929133858267717549 ) ) ;
#46871 = CARTESIAN_POINT ( 'NONE',  ( 0.3917322834645669549, 0.1049643490035304660, -1.849081364829396223 ) ) ;
#46872 = ORIENTED_EDGE ( 'NONE', *, *, #26230, .T. ) ;
#46873 = CARTESIAN_POINT ( 'NONE',  ( -0.3996062992125986035, -0.1070741851644056997, -0.5183727034120735322 ) ) ;
#46874 = ORIENTED_EDGE ( 'NONE', *, *, #16485, .T. ) ;
#46875 = CARTESIAN_POINT ( 'NONE',  ( 1.325459317585302665, -0.4281496062992124485, 0.4176697321401328655 ) ) ;
#46876 = CARTESIAN_POINT ( 'NONE',  ( 1.056430446194226436, -0.5511811023622048555, -0.09757992244046775898 ) ) ;
#46877 = PLANE ( 'NONE',  #57220 ) ;
#46878 = DIRECTION ( 'NONE',  ( -3.096699300667737957E-16, 1.000000000000000000, -0.000000000000000000 ) ) ;
#46879 = CARTESIAN_POINT ( 'NONE',  ( 0.3970677821444033584, 0.02963302784745526844, -1.929133858267716439 ) ) ;
#46880 = CARTESIAN_POINT ( 'NONE',  ( -0.2867679344610364334, -0.2867679344610367109, -1.088582677165354173 ) ) ;
#46881 = CARTESIAN_POINT ( 'NONE',  ( 1.246719160104987623, -0.4281496062992124485, 0.4176697321401328655 ) ) ;
#46882 = CARTESIAN_POINT ( 'NONE',  ( -0.3990339831393152625, -0.0003067303410125883515, -1.929133858267716217 ) ) ;
#46883 = CARTESIAN_POINT ( 'NONE',  ( -0.1771653543307080136, -0.5400638737290844871, 0.3530559997133364547 ) ) ;
#46884 = CARTESIAN_POINT ( 'NONE',  ( 1.259842519685040019, -0.1870078740157479769, 0.4822834645669291653 ) ) ;
#46885 = ORIENTED_EDGE ( 'NONE', *, *, #13561, .F. ) ;
#46886 = EDGE_CURVE ( 'NONE', #57436, #29775, #16107, .T. ) ;
#46887 = CARTESIAN_POINT ( 'NONE',  ( -1.719160104986876103, 0.05413385826771666132, 0.4176697321401328100 ) ) ;
#46888 = CARTESIAN_POINT ( 'NONE',  ( 0.3503937007874015075, 0.3044824468161027586, -0.01968503937007903132 ) ) ;
#46889 = PRODUCT_CONTEXT ( 'NONE', #13801, 'mechanical' ) ;
#46890 = CARTESIAN_POINT ( 'NONE',  ( 1.482939632545932307, -0.3690944881889763329, 0.3153832671262228327 ) ) ;
#46891 = LINE ( 'NONE', #14106, #29119 ) ;
#46892 = CARTESIAN_POINT ( 'NONE',  ( -1.069553805774277722, -0.5511811023622048555, -0.09757992244046775898 ) ) ;
#46893 = CARTESIAN_POINT ( 'NONE',  ( -1.450131233595799651, 0.2952755905511810774, -0.1292274648535930714 ) ) ;
#46894 = CARTESIAN_POINT ( 'NONE',  ( 0.7152230971128616943, -0.05778040916215522460, 0.4822834645669289988 ) ) ;
#46895 = ORIENTED_EDGE ( 'NONE', *, *, #1251, .F. ) ;
#46897 = CARTESIAN_POINT ( 'NONE',  ( 2.795275590551181466, 1.968503937007874960, 0.000000000000000000 ) ) ;
#46896 = CARTESIAN_POINT ( 'NONE',  ( 1.476377952755906442, -0.5400638737290844871, 0.3530559997133364547 ) ) ;
#46898 = CARTESIAN_POINT ( 'NONE',  ( -0.6758530183727028406, -0.5511811023622048555, -0.09757992244046775898 ) ) ;
#46899 = CARTESIAN_POINT ( 'NONE',  ( 0.8136482939632553313, -0.6046776061558809534, -0.2411417322834644161 ) ) ;
#46900 = CARTESIAN_POINT ( 'NONE',  ( -1.482939632545930975, -0.4281496062992127816, -0.4176697321401328100 ) ) ;
#46901 = CARTESIAN_POINT ( 'NONE',  ( 0.3917322834645669549, 2.398668435337827645E-17, -1.300505618601362601 ) ) ;
#46902 = CARTESIAN_POINT ( 'NONE',  ( -0.9317585301837263412, -0.004921259842519576551, 0.3153832671262227771 ) ) ;
#46903 = CARTESIAN_POINT ( 'NONE',  ( -1.476377952755905110, 0.07958543189024085140, 0.2665933059059887866 ) ) ;
#46904 = CYLINDRICAL_SURFACE ( 'NONE', #43797, 0.3149606299212597826 ) ;
#46905 = CARTESIAN_POINT ( 'NONE',  ( 0.4921259842519691285, 0.1660481256975885056, 0.3530559997133364547 ) ) ;
#46906 = CARTESIAN_POINT ( 'NONE',  ( -0.9908136482939626788, 0.1771653543307087630, 0.09757992244046791164 ) ) ;
#46907 = CARTESIAN_POINT ( 'NONE',  ( -0.1640419947506555343, -0.2845877964562159024, 0.3641732283464567677 ) ) ;
#46908 = CARTESIAN_POINT ( 'NONE',  ( -0.1312335958005241554, 0.2306618581243848609, 0.2411417322834645549 ) ) ;
#46909 = CARTESIAN_POINT ( 'NONE',  ( -1.587926509186350810, -0.004921259842519870586, -0.3153832671262229437 ) ) ;
#46910 = CARTESIAN_POINT ( 'NONE',  ( -0.1049643490035307158, 0.3917322834645670104, -0.003300155676852285953 ) ) ;
#46911 = CARTESIAN_POINT ( 'NONE',  ( 0.6036745406824153282, -0.6046776061558807314, 0.2411417322834647770 ) ) ;
#46912 = EDGE_CURVE ( 'NONE', #74748, #78909, #9281, .T. ) ;
#46913 = CARTESIAN_POINT ( 'NONE',  ( 0.4051969335537412009, 7.699586553780600482E-16, 0.3791483426435171555 ) ) ;
#46914 = CARTESIAN_POINT ( 'NONE',  ( 0.4724409448818898682, 2.892866454678787531E-17, -1.454724409448818756 ) ) ;
#46915 = CARTESIAN_POINT ( 'NONE',  ( -0.5839895013123351797, 0.2952755905511810774, -0.1292274648535930714 ) ) ;
#46916 = AXIS2_PLACEMENT_3D ( 'NONE', #71425, #51204, #83217 ) ;
#46917 = CARTESIAN_POINT ( 'NONE',  ( -0.04593175853018302557, -0.5511811023622048555, -0.09757992244046775898 ) ) ;
#46918 = CARTESIAN_POINT ( 'NONE',  ( -1.456692913385826182, 0.2952755905511811885, 0.000000000000000000 ) ) ;
#46919 = CARTESIAN_POINT ( 'NONE',  ( 0.4199475065616805614, 0.1283753931104748280, 0.1820866141732283561 ) ) ;
#46920 = CARTESIAN_POINT ( 'NONE',  ( -0.5774278215223089816, 0.1283753931104746893, -0.1820866141732285504 ) ) ;
#46921 = CARTESIAN_POINT ( 'NONE',  ( -1.095800524934382292, -0.05778040916215522460, 0.4822834645669289988 ) ) ;
#46922 = CARTESIAN_POINT ( 'NONE',  ( -1.476377952755905110, -0.5400638737290845981, -0.3530559997133363437 ) ) ;
#46923 = CARTESIAN_POINT ( 'NONE',  ( -1.463254593175852492, 0.2952755905511811885, 0.1292274648535926551 ) ) ;
#46924 = CARTESIAN_POINT ( 'NONE',  ( -2.199130528046420221E-22, 1.075705580628688596, 0.2362204724409449064 ) ) ;
#46925 = CARTESIAN_POINT ( 'NONE',  ( 0.7020997375328090762, -0.2845877964562159024, 0.3641732283464567677 ) ) ;
#46926 = CARTESIAN_POINT ( 'NONE',  ( 0.4199475065616805614, 0.2306618581243848609, 0.2411417322834645549 ) ) ;
#46927 = CARTESIAN_POINT ( 'NONE',  ( -1.476377952755905110, 0.1660481256975885056, 0.3530559997133364547 ) ) ;
#46928 = CARTESIAN_POINT ( 'NONE',  ( 1.509186351706037543, -0.3690944881889765550, -0.3153832671262227771 ) ) ;
#46929 = EDGE_LOOP ( 'NONE', ( #7001, #7848, #671, #9621 ) ) ;
#46930 = B_SPLINE_CURVE_WITH_KNOTS ( 'NONE', 3,
 ( #36274, #61946, #4286, #24459 ),
 .UNSPECIFIED., .F., .F.,
 ( 4, 4 ),
 ( 9.992028926250184212E-07, 0.001428690226504376057 ),
 .UNSPECIFIED. ) ;
#46931 = CARTESIAN_POINT ( 'NONE',  ( 0.1070741851644053388, 0.3996062992125986035, -2.747375328083988766 ) ) ;
#46932 = CARTESIAN_POINT ( 'NONE',  ( -1.095800524934382292, -0.2845877964562161244, -0.3641732283464567121 ) ) ;
#46933 = CARTESIAN_POINT ( 'NONE',  ( -0.4396325459317577122, -0.6692913385826773087, -0.1292274648535924053 ) ) ;
#46934 = CARTESIAN_POINT ( 'NONE',  ( 0.4133858267716541968, -0.5400638737290845981, -0.3530559997133363437 ) ) ;
#46935 = CARTESIAN_POINT ( 'NONE',  ( -1.371391076115484831, 0.1771653543307087075, -0.09757992244046823083 ) ) ;
#46936 = CARTESIAN_POINT ( 'NONE',  ( 0.3460692066303958092, 0.1998031496062993018, -1.625328083989501460 ) ) ;
#46937 = CARTESIAN_POINT ( 'NONE',  ( -1.371391076115484831, 0.2952755905511810774, -0.1292274648535930714 ) ) ;
#46938 = CARTESIAN_POINT ( 'NONE',  ( 0.5380577427821529035, -0.4281496062992124485, 0.4176697321401328655 ) ) ;
#46939 = CARTESIAN_POINT ( 'NONE',  ( 0.1509186351706045259, -0.05778040916215560624, -0.4822834645669293319 ) ) ;
#46940 = CARTESIAN_POINT ( 'NONE',  ( 1.345144356955381593, -0.3162353388693409650, -0.4822834645669289433 ) ) ;
#46941 = DIRECTION ( 'NONE',  ( -0.7071067811865462405, -2.189697074797793155E-16, -0.7071067811865486830 ) ) ;
#46942 = CARTESIAN_POINT ( 'NONE',  ( 0.1998031496062992740, 0.3460692066303959757, -1.561679790026246684 ) ) ;
#46943 = CARTESIAN_POINT ( 'NONE',  ( -0.1058382717557497937, -0.3949938075777411628, -0.5446194225721784354 ) ) ;
#46944 = CARTESIAN_POINT ( 'NONE',  ( -9.594673741351313045E-17, 0.3917322834645670104, -0.1496062992125983815 ) ) ;
#46945 = CARTESIAN_POINT ( 'NONE',  ( 5.463695987328526437E-16, -0.1870078740157479769, 0.3641732283464567677 ) ) ;
#46946 = CARTESIAN_POINT ( 'NONE',  ( -0.1837270341207343505, -0.6046776061558807314, 0.2411417322834647770 ) ) ;
#46947 = CARTESIAN_POINT ( 'NONE',  ( 1.391076115485564868, -0.6046776061558807314, 0.2411417322834647770 ) ) ;
#46948 = CARTESIAN_POINT ( 'NONE',  ( 0.3949938075777408852, 0.1058382717557500435, -1.776246719160105236 ) ) ;
#46949 = CARTESIAN_POINT ( 'NONE',  ( 8.195543980992789655E-16, -0.1870078740157480601, -0.3641732283464567677 ) ) ;
#46950 = CARTESIAN_POINT ( 'NONE',  ( -1.108923884514435132, -0.05778040916215560624, -0.4822834645669293319 ) ) ;
#46951 = CARTESIAN_POINT ( 'NONE',  ( -1.496062992125983815, -0.1870078740157479769, 0.4822834645669291653 ) ) ;
#46952 = CARTESIAN_POINT ( 'NONE',  ( 0.3458507752293908943, 0.3458507752293908943, -2.185039370078739829 ) ) ;
#46953 = CARTESIAN_POINT ( 'NONE',  ( 0.3788256970788764222, -0.1002886991238087361, -2.755905511811022279 ) ) ;
#46954 = ORIENTED_EDGE ( 'NONE', *, *, #38297, .T. ) ;
#46955 = VERTEX_POINT ( 'NONE', #41667 ) ;
#46956 = CARTESIAN_POINT ( 'NONE',  ( 1.404199475065617264, -0.4281496062992124485, 0.4176697321401328655 ) ) ;
#46957 = CARTESIAN_POINT ( 'NONE',  ( -1.673228346456691717, 0.1660481256975883668, -0.3530559997133364547 ) ) ;
#46959 = CARTESIAN_POINT ( 'NONE',  ( -1.358267716535432434, -0.5400638737290844871, 0.3530559997133364547 ) ) ;
#46958 = CARTESIAN_POINT ( 'NONE',  ( -1.036745406824146176, -0.3690944881889763329, 0.3153832671262228327 ) ) ;
#46960 = CARTESIAN_POINT ( 'NONE',  ( -0.1958661417322836440, 0.3392501089628016664, -2.455361261645982562 ) ) ;
#46961 = CARTESIAN_POINT ( 'NONE',  ( -0.9580052493438311334, 0.009842519685039147898, -0.3409548833797004797 ) ) ;
#46962 = CARTESIAN_POINT ( 'NONE',  ( 1.056430446194226658, 0.2952755905511811885, 0.1292274648535926551 ) ) ;
#46963 = CARTESIAN_POINT ( 'NONE',  ( -1.633858267716534529, -0.5400638737290845981, -0.3530559997133363437 ) ) ;
#46964 = CARTESIAN_POINT ( 'NONE',  ( -0.2165354330708654795, -0.5400638737290845981, -0.3530559997133363437 ) ) ;
#46965 = CARTESIAN_POINT ( 'NONE',  ( -0.09186351706036689768, 0.05413385826771626580, -0.4176697321401330321 ) ) ;
#46966 = CARTESIAN_POINT ( 'NONE',  ( -1.095800524934382292, -0.3162353388693409650, -0.4822834645669289433 ) ) ;
#46967 = CARTESIAN_POINT ( 'NONE',  ( 0.3917322834645669549, 2.398668435337827645E-17, -2.717828453247031817 ) ) ;
#46968 = CARTESIAN_POINT ( 'NONE',  ( 0.7808398950131240079, -0.3162353388693405765, 0.4822834645669290543 ) ) ;
#46969 = CARTESIAN_POINT ( 'NONE',  ( -0.3917322834645670104, -7.196005306013484475E-17, -1.921259842519684957 ) ) ;
#46970 = CARTESIAN_POINT ( 'NONE',  ( -1.279527559055116948, 0.07958543189024071263, -0.2665933059059888421 ) ) ;
#46971 = EDGE_LOOP ( 'NONE', ( #43329, #81496, #73403, #37756, #29892, #14811 ) ) ;
#46972 = CARTESIAN_POINT ( 'NONE',  ( -9.674558042662121740E-17, 0.3949938075777409963, -2.204724409448819422 ) ) ;
#46973 = ORIENTED_EDGE ( 'NONE', *, *, #78501, .F. ) ;
#46974 = DIRECTION ( 'NONE',  ( 0.000000000000000000, -1.000000000000000000, 1.734723475976806108E-16 ) ) ;
#46975 = CARTESIAN_POINT ( 'NONE',  ( -1.108923884514435132, -0.3162353388693405765, 0.4822834645669290543 ) ) ;
#46976 = CARTESIAN_POINT ( 'NONE',  ( -1.279527559055116948, 0.1660481256975883668, -0.3530559997133364547 ) ) ;
#46977 = CARTESIAN_POINT ( 'NONE',  ( -9.787531504996567848E-17, 0.3996062992125986035, -0.7874015748031496509 ) ) ;
#46978 = CARTESIAN_POINT ( 'NONE',  ( -1.345144356955379816, -0.05778040916215560624, -0.4822834645669293319 ) ) ;
#46979 = CARTESIAN_POINT ( 'NONE',  ( 3.886287458032462006, 2.165354330708661568, -0.6299212598425196763 ) ) ;
#46980 = CARTESIAN_POINT ( 'NONE',  ( -1.541994750656167090, -0.6692913385826773087, -0.1292274648535924053 ) ) ;
#46981 = LINE ( 'NONE', #8287, #35104 ) ;
#46982 = CARTESIAN_POINT ( 'NONE',  ( 0.1958661417322834775, 0.3392501089628018884, -0.07152230971128617498 ) ) ;
#46983 = CARTESIAN_POINT ( 'NONE',  ( 0.02624671916010564918, -0.5023911411419708095, -0.1820866141732282451 ) ) ;
#46984 = CARTESIAN_POINT ( 'NONE',  ( 0.1958661417322836440, -0.3392501089628017219, -0.8064304461942258806 ) ) ;
#46985 = CARTESIAN_POINT ( 'NONE',  ( -0.9580052493438311334, -0.3690944881889763329, 0.3153832671262228327 ) ) ;
#46986 = CARTESIAN_POINT ( 'NONE',  ( -1.233595800524933894, -0.6046776061558809534, -0.2411417322834644161 ) ) ;
#46987 = CARTESIAN_POINT ( 'NONE',  ( 0.8792650918635177559, -0.4281496062992127816, -0.4176697321401328100 ) ) ;
#46988 = CARTESIAN_POINT ( 'NONE',  ( -1.062992125984250968, -0.6692913385826771977, 8.415575281601705876E-17 ) ) ;
#46989 = CARTESIAN_POINT ( 'NONE',  ( -0.1049643490035307020, 0.3917322834645669549, 0.001312335958005294862 ) ) ;
#46990 = ORIENTED_EDGE ( 'NONE', *, *, #50488, .T. ) ;
#46991 = EDGE_CURVE ( 'NONE', #30272, #32285, #42120, .T. ) ;
#46992 = CARTESIAN_POINT ( 'NONE',  ( -1.259842519685038686, -0.1870078740157480879, -0.4822834645669291653 ) ) ;
#46993 = CARTESIAN_POINT ( 'NONE',  ( 0.7808398950131240079, -0.3162353388693405765, 0.4822834645669290543 ) ) ;
#46994 = CARTESIAN_POINT ( 'NONE',  ( -1.404199475065615932, -0.004921259842519576551, 0.3153832671262227771 ) ) ;
#46995 = CARTESIAN_POINT ( 'NONE',  ( -0.1248512358867407135, 1.054133277639911714, 0.2754420493137687553 ) ) ;
#46996 = CARTESIAN_POINT ( 'NONE',  ( -1.157146581871515012E-16, 0.4724409448818898682, -1.417322834645669216 ) ) ;
#46997 = CARTESIAN_POINT ( 'NONE',  ( 1.964414453380805892, 1.188885443925065566, -0.3231744412229926033 ) ) ;
#46998 = CARTESIAN_POINT ( 'NONE',  ( -0.1958661417322834220, -0.3392501089628018884, -0.5301837270341206443 ) ) ;
#46999 = CARTESIAN_POINT ( 'NONE',  ( -0.1049643490035307020, 0.3917322834645669549, -2.610892388451443669 ) ) ;
#47000 = CARTESIAN_POINT ( 'NONE',  ( -0.1706036745406816491, 0.05413385826771626580, -0.4176697321401330321 ) ) ;
#47001 = CARTESIAN_POINT ( 'NONE',  ( -1.620734908136482577, 0.1771653543307087630, 0.09757992244046791164 ) ) ;
#47002 = CARTESIAN_POINT ( 'NONE',  ( 0.3996062992125984925, 0.1070741851644054637, -0.2014435695538057958 ) ) ;
#47004 = CARTESIAN_POINT ( 'NONE',  ( -0.4706608522957314578, 1.597527518877483788, 2.563288228875758801 ) ) ;
#47003 = CARTESIAN_POINT ( 'NONE',  ( -1.679790026246718693, 0.2306618581243847221, -0.2411417322834647770 ) ) ;
#47005 = CARTESIAN_POINT ( 'NONE',  ( -1.246719160104986512, 0.05413385826771666132, 0.4176697321401328100 ) ) ;
#47006 = CARTESIAN_POINT ( 'NONE',  ( -0.2493438320209966919, 0.05413385826771626580, -0.4176697321401330321 ) ) ;
#47007 = CARTESIAN_POINT ( 'NONE',  ( -0.1049643490035306742, 0.3917322834645668994, 0.07088545751412257678 ) ) ;
#47008 = CARTESIAN_POINT ( 'NONE',  ( 0.6036745406824153282, -0.5023911411419708095, 0.1820866141732285504 ) ) ;
#47009 = CARTESIAN_POINT ( 'NONE',  ( 0.3917322834645670104, 2.398668435337828261E-17, -0.04527559055118119541 ) ) ;
#47010 = CARTESIAN_POINT ( 'NONE',  ( 0.5052493438320218022, -0.5511811023622048555, -0.09757992244046775898 ) ) ;
#47011 = CARTESIAN_POINT ( 'NONE',  ( 0.9120734908136489683, -0.5511811023622046335, 0.09757992244046803654 ) ) ;
#47012 = CARTESIAN_POINT ( 'NONE',  ( 0.9908136482939640111, 0.2952755905511810774, -0.1292274648535930714 ) ) ;
#47013 = CARTESIAN_POINT ( 'NONE',  ( 0.07217847769028949700, -0.2845877964562159024, 0.3641732283464567677 ) ) ;
#47014 = CARTESIAN_POINT ( 'NONE',  ( -0.1049643490035302024, -0.3917322834645671215, -1.954068241469816503 ) ) ;
#47015 = CARTESIAN_POINT ( 'NONE',  ( -1.332020997375327642, -0.05778040916215522460, 0.4822834645669289988 ) ) ;
#47016 = CARTESIAN_POINT ( 'NONE',  ( -0.2952755905511804668, 0.07958543189024085140, 0.2665933059059887866 ) ) ;
#47017 = EDGE_CURVE ( 'NONE', #32253, #5025, #60202, .T. ) ;
#47018 = CARTESIAN_POINT ( 'NONE',  ( -1.305774278215222184, 0.1771653543307087630, 0.09757992244046791164 ) ) ;
#47019 = CARTESIAN_POINT ( 'NONE',  ( 0.3458507752293908943, 0.3458507752293908943, -0.2145669291338583029 ) ) ;
#47020 = CARTESIAN_POINT ( 'NONE',  ( -0.7808398950131222316, -0.2845877964562161244, -0.3641732283464567121 ) ) ;
#47021 = EDGE_CURVE ( 'NONE', #15514, #31453, #21898, .T. ) ;
#47022 = FACE_OUTER_BOUND ( 'NONE', #82810, .T. ) ;
#47023 = CARTESIAN_POINT ( 'NONE',  ( -0.1377952755905504645, -0.5400638737290845981, -0.3530559997133363437 ) ) ;
#47024 = CARTESIAN_POINT ( 'NONE',  ( 0.6889763779527560139, 1.446433227339393149E-17, -0.1181102362204724116 ) ) ;
#47025 = CARTESIAN_POINT ( 'NONE',  ( 0.6299212598425204535, -0.1870078740157479769, 0.3641732283464567677 ) ) ;
#47026 = CARTESIAN_POINT ( 'NONE',  ( -0.4002624671916004129, -0.08942795157528024563, -0.3641732283464568787 ) ) ;
#47027 = CARTESIAN_POINT ( 'NONE',  ( -0.4921259842519677963, 0.1660481256975883668, -0.3530559997133364547 ) ) ;
#47028 = FACE_OUTER_BOUND ( 'NONE', #61352, .T. ) ;
#47029 = CARTESIAN_POINT ( 'NONE',  ( -1.167979002624671470, -0.004921259842519576551, 0.3153832671262227771 ) ) ;
#47030 = DIRECTION ( 'NONE',  ( 0.000000000000000000, -1.000000000000000000, 0.000000000000000000 ) ) ;
#47031 = CARTESIAN_POINT ( 'NONE',  ( 0.4396325459317593221, 0.2952755905511810774, -0.1292274648535930714 ) ) ;
#47032 = CARTESIAN_POINT ( 'NONE',  ( -0.2925321140481930149, -0.2925321140481933480, -1.395669291338582196 ) ) ;
#47033 = CARTESIAN_POINT ( 'NONE',  ( 1.541994750656168645, -0.6692913385826771977, 0.1292274648535927661 ) ) ;
#47034 = CARTESIAN_POINT ( 'NONE',  ( -0.01968503937007793844, -0.4536011799217367080, 0.2665933059059888421 ) ) ;
#47035 = CARTESIAN_POINT ( 'NONE',  ( -1.528871391076114250, -0.6692913385826771977, 0.1292274648535927661 ) ) ;
#47036 = CARTESIAN_POINT ( 'NONE',  ( -1.555118110236219930, -0.4536011799217368745, -0.2665933059059886201 ) ) ;
#47037 = CARTESIAN_POINT ( 'NONE',  ( 1.417322834645670104, -0.1870078740157480879, -0.4822834645669291653 ) ) ;
#47038 = EDGE_CURVE ( 'NONE', #17151, #22673, #40430, .T. ) ;
#47039 = CARTESIAN_POINT ( 'NONE',  ( -0.6430446194225716283, -0.3690944881889763329, 0.3153832671262228327 ) ) ;
#47040 = CARTESIAN_POINT ( 'NONE',  ( 0.1998031496062994128, -0.3460692066303957537, -0.01115485564304463835 ) ) ;
#47041 = CARTESIAN_POINT ( 'NONE',  ( 0.9842519685039375910, 0.2952755905511811885, 0.000000000000000000 ) ) ;
#47042 = CARTESIAN_POINT ( 'NONE',  ( 0.3996062992125986590, -0.1070741851644053111, -0.1115485564304461857 ) ) ;
#47043 = CARTESIAN_POINT ( 'NONE',  ( -0.3917322834645670659, -7.196005306013484475E-17, -2.713273908957691827 ) ) ;
#47044 = ADVANCED_FACE ( 'NONE', ( #1720 ), #62244, .F. ) ;
#47045 = CARTESIAN_POINT ( 'NONE',  ( 0.7186703366786207914, -1.374501131054255944E-15, 0.4445507791589066726 ) ) ;
#47046 = CARTESIAN_POINT ( 'NONE',  ( 1.515748031496063186, -0.4536011799217368745, -0.2665933059059886201 ) ) ;
#47047 = CARTESIAN_POINT ( 'NONE',  ( -1.332020997375327642, -0.3162353388693409650, -0.4822834645669289433 ) ) ;
#47048 = CARTESIAN_POINT ( 'NONE',  ( 1.384514435695538337, -0.6692913385826771977, 0.1292274648535927661 ) ) ;
#47049 = CARTESIAN_POINT ( 'NONE',  ( -0.3917322834645669549, -0.1049643490035306603, -2.492782152230970993 ) ) ;
#47050 = CARTESIAN_POINT ( 'NONE',  ( 1.332020997375329197, -0.2845877964562159024, 0.3641732283464567677 ) ) ;
#47051 = CARTESIAN_POINT ( 'NONE',  ( 0.02624671916010564918, -0.6046776061558809534, -0.2411417322834644161 ) ) ;
#47052 = CARTESIAN_POINT ( 'NONE',  ( -0.4396325459317577122, -0.6692913385826773087, -0.1292274648535924053 ) ) ;
#47053 = CARTESIAN_POINT ( 'NONE',  ( 1.679790026246720025, 0.2306618581243848609, 0.2411417322834645549 ) ) ;
#47054 = DIRECTION ( 'NONE',  ( -1.000000000000000000, -0.000000000000000000, -0.000000000000000000 ) ) ;
#47055 = CARTESIAN_POINT ( 'NONE',  ( 0.2362204724409456558, -0.1870078740157480601, -0.3641732283464567677 ) ) ;
#47056 = ORIENTED_EDGE ( 'NONE', *, *, #48666, .F. ) ;
#47057 = CARTESIAN_POINT ( 'NONE',  ( 0.3917322834645670659, -0.1049643490035303273, -0.4232476622385321074 ) ) ;
#47058 = VERTEX_POINT ( 'NONE', #72007 ) ;
#47059 = CARTESIAN_POINT ( 'NONE',  ( -0.3871391076115479057, -0.3162353388693409650, -0.4822834645669289433 ) ) ;
#47060 = CARTESIAN_POINT ( 'NONE',  ( 1.515748031496063186, -0.5400638737290845981, -0.3530559997133363437 ) ) ;
#47061 = CARTESIAN_POINT ( 'NONE',  ( 0.3477690288713918276, -0.6692913385826773087, -0.1292274648535924053 ) ) ;
#47062 = CARTESIAN_POINT ( 'NONE',  ( -0.4133858267716528645, -0.4536011799217367080, 0.2665933059059888421 ) ) ;
#47063 = CARTESIAN_POINT ( 'NONE',  ( 1.036745406824147731, 0.05413385826771666132, 0.4176697321401328100 ) ) ;
#47064 = CARTESIAN_POINT ( 'NONE',  ( -0.9842519685039360366, 0.2952755905511811885, 0.000000000000000000 ) ) ;
#47065 = CARTESIAN_POINT ( 'NONE',  ( 0.1837270341207354329, 0.2306618581243848609, 0.2411417322834645549 ) ) ;
#47066 = CARTESIAN_POINT ( 'NONE',  ( -0.9448818897637790704, -0.1870078740157479769, 0.4822834645669291653 ) ) ;
#47067 = CARTESIAN_POINT ( 'NONE',  ( 1.200787401574803681, -0.5400638737290845981, -0.3530559997133363437 ) ) ;
#47068 = CARTESIAN_POINT ( 'NONE',  ( 1.069553805774278610, -0.6692913385826771977, 0.1292274648535927661 ) ) ;
#47069 = ADVANCED_FACE ( 'NONE', ( #79169 ), #79757, .F. ) ;
#47070 = CARTESIAN_POINT ( 'NONE',  ( 1.154855643044620184, -0.6046776061558807314, 0.2411417322834647770 ) ) ;
#47071 = CARTESIAN_POINT ( 'NONE',  ( -0.2867679344610365999, 0.2867679344610364889, -0.7992125984251968740 ) ) ;
#47072 = CARTESIAN_POINT ( 'NONE',  ( 0.09842519685039434474, 0.07958543189024085140, 0.2665933059059887866 ) ) ;
#47073 = ORIENTED_EDGE ( 'NONE', *, *, #59455, .F. ) ;
#47074 = CARTESIAN_POINT ( 'NONE',  ( 0.3420746716998659953, 0.1974969037888705536, -1.076115485564304475 ) ) ;
#47075 = ORIENTED_EDGE ( 'NONE', *, *, #26715, .F. ) ;
#47076 = CARTESIAN_POINT ( 'NONE',  ( -0.9711286089238838626, -0.5023911411419708095, 0.1820866141732285504 ) ) ;
#47077 = CARTESIAN_POINT ( 'NONE',  ( -0.1509186351706028884, -0.3162353388693409650, -0.4822834645669289433 ) ) ;
#47078 = CARTESIAN_POINT ( 'NONE',  ( 2.841478809456089216, 1.098283573398297852, 0.1802708669123707919 ) ) ;
#47079 = CARTESIAN_POINT ( 'NONE',  ( -0.2034120734908131112, -0.6692913385826773087, -0.1292274648535924053 ) ) ;
#47080 = CARTESIAN_POINT ( 'NONE',  ( -0.3937007874015740483, -0.1870078740157480879, -0.4822834645669291653 ) ) ;
#47081 = CARTESIAN_POINT ( 'NONE',  ( -0.8727034120734901146, -0.3162353388693405765, 0.4822834645669290543 ) ) ;
#47082 = CARTESIAN_POINT ( 'NONE',  ( -1.548556430446193399, 0.2306618581243848609, 0.2411417322834645549 ) ) ;
#47083 = EDGE_CURVE ( 'NONE', #37352, #32456, #36679, .T. ) ;
#47084 = CARTESIAN_POINT ( 'NONE',  ( 1.404199475065617708, -0.004921259842519870586, -0.3153832671262229437 ) ) ;
#47085 = CARTESIAN_POINT ( 'NONE',  ( -1.502624671916009680, -0.3162353388693405765, 0.4822834645669290543 ) ) ;
#47086 = CARTESIAN_POINT ( 'NONE',  ( 0.2845468109762787079, 0.07963338598832106485, 5.543284456214099265 ) ) ;
#47087 = CARTESIAN_POINT ( 'NONE',  ( 0.3477690288713918276, 0.1771653543307087630, 0.09757992244046791164 ) ) ;
#47088 = CARTESIAN_POINT ( 'NONE',  ( 0.2427821522309719648, -0.05778040916215522460, 0.4822834645669289988 ) ) ;
#47089 = CARTESIAN_POINT ( 'NONE',  ( 0.5314960629921267055, -0.5400638737290844871, 0.3530559997133364547 ) ) ;
#47090 = ORIENTED_EDGE ( 'NONE', *, *, #81662, .F. ) ;
#47091 = CARTESIAN_POINT ( 'NONE',  ( 0.1998031496062992740, 0.3460692066303959757, -1.876640419947506411 ) ) ;
#47092 = CARTESIAN_POINT ( 'NONE',  ( -0.6171485355042630738, 0.004960608223778823628, 0.3437734562760190182 ) ) ;
#47093 = CARTESIAN_POINT ( 'NONE',  ( 0.2925321140481932369, 0.2925321140481932369, -1.159448818897637734 ) ) ;
#47094 = CARTESIAN_POINT ( 'NONE',  ( 0.3460692066303958092, 0.1998031496062993018, -0.3654855643044619407 ) ) ;
#47095 = CARTESIAN_POINT ( 'NONE',  ( -0.7020997375328076329, -0.3162353388693409650, -0.4822834645669289433 ) ) ;
#47096 = CARTESIAN_POINT ( 'NONE',  ( 0.3996062992125986035, 2.446882876249141962E-17, -2.952755905511811108 ) ) ;
#47097 = EDGE_CURVE ( 'NONE', #34868, #10035, #5752, .T. ) ;
#47098 = CARTESIAN_POINT ( 'NONE',  ( 0.2867679344610365999, -0.2867679344610365444, -1.915354330708661124 ) ) ;
#47099 = CARTESIAN_POINT ( 'NONE',  ( -1.633858267716534529, 0.07958543189024085140, 0.2665933059059887866 ) ) ;
#47100 = CARTESIAN_POINT ( 'NONE',  ( 0.8792650918635177559, -0.4281496062992127816, -0.4176697321401328100 ) ) ;
#47101 = CARTESIAN_POINT ( 'NONE',  ( 0.7874015748031503170, -0.1870078740157480879, -0.4822834645669291653 ) ) ;
#47102 = CARTESIAN_POINT ( 'NONE',  ( -0.3280839895013117347, -0.004921259842519870586, -0.3153832671262229437 ) ) ;
#47103 = CARTESIAN_POINT ( 'NONE',  ( 0.1509186351706042484, -0.3162353388693405765, 0.4822834645669290543 ) ) ;
#47104 = CARTESIAN_POINT ( 'NONE',  ( 0.4091458600556403535, 0.2362204724409449896, -2.097769028871391050 ) ) ;
#47105 = CARTESIAN_POINT ( 'NONE',  ( -0.1246719160104980823, -0.5511811023622048555, -0.09757992244046775898 ) ) ;
#47106 = CARTESIAN_POINT ( 'NONE',  ( 0.1640419947506569498, -0.05778040916215522460, 0.4822834645669289988 ) ) ;
#47107 = CARTESIAN_POINT ( 'NONE',  ( -0.3949938075777408852, -0.1058382717557502933, -1.382545931758530688 ) ) ;
#47108 = CARTESIAN_POINT ( 'NONE',  ( 1.568241469816273437, -0.2845877964562159024, 0.3641732283464567677 ) ) ;
#47109 = CARTESIAN_POINT ( 'NONE',  ( 0.1574803149606306130, -0.1870078740157479769, 0.3641732283464567677 ) ) ;
#47110 = CARTESIAN_POINT ( 'NONE',  ( 1.555118110236221041, 0.07958543189024071263, -0.2665933059059888421 ) ) ;
#47111 = CARTESIAN_POINT ( 'NONE',  ( -0.6364829396325453192, -0.3162353388693405765, 0.4822834645669290543 ) ) ;
#47112 = CONICAL_SURFACE ( 'NONE', #56534, 0.1190944881889763746, 0.8726646259971682085 ) ;
#47113 = CARTESIAN_POINT ( 'NONE',  ( -0.7086614173228339419, -0.1870078740157479769, 0.3641732283464567677 ) ) ;
#47114 = CARTESIAN_POINT ( 'NONE',  ( -1.033961166703848411, -1.283732188437465593E-15, -0.4281993546915532911 ) ) ;
#47115 = CARTESIAN_POINT ( 'NONE',  ( -0.7480314960629914633, 0.2952755905511811885, 0.000000000000000000 ) ) ;
#47116 = CARTESIAN_POINT ( 'NONE',  ( -0.6692913385826764205, 0.2952755905511811885, 0.000000000000000000 ) ) ;
#47117 = CARTESIAN_POINT ( 'NONE',  ( -0.03937007874015669567, 0.2952755905511811885, 0.000000000000000000 ) ) ;
#47118 = CARTESIAN_POINT ( 'NONE',  ( -0.1070741851644056997, 0.3996062992125984925, -2.445538057742782101 ) ) ;
#47119 = CARTESIAN_POINT ( 'NONE',  ( -0.3917322834645668994, -0.1049643490035306742, -2.015728715714224517 ) ) ;
#47120 = CARTESIAN_POINT ( 'NONE',  ( -0.5314960629921124946, 2.725289161120229675, -3.884611959489590483 ) ) ;
#47121 = CARTESIAN_POINT ( 'NONE',  ( 0.9448818897637802916, -0.1870078740157480601, -0.3641732283464567677 ) ) ;
#47122 = CARTESIAN_POINT ( 'NONE',  ( 1.423884514435696191, -0.05778040916215522460, 0.4822834645669289988 ) ) ;
#47123 = CARTESIAN_POINT ( 'NONE',  ( -1.207349081364828880, 0.1283753931104746893, -0.1820866141732285504 ) ) ;
#47124 = CARTESIAN_POINT ( 'NONE',  ( 0.9645669291338591078, -0.5400638737290845981, -0.3530559997133363437 ) ) ;
#47125 = CARTESIAN_POINT ( 'NONE',  ( -1.167979002624671470, -0.3690944881889765550, -0.3153832671262227771 ) ) ;
#47126 = CARTESIAN_POINT ( 'NONE',  ( -0.6430446194225716283, -0.4281496062992124485, 0.4176697321401328655 ) ) ;
#47127 = CARTESIAN_POINT ( 'NONE',  ( 0.1771653543307093182, -0.4536011799217368745, -0.2665933059059886201 ) ) ;
#47128 = DIRECTION ( 'NONE',  ( 1.000000000000000000, 0.000000000000000000, 0.000000000000000000 ) ) ;
#47129 = CARTESIAN_POINT ( 'NONE',  ( 0.7020997375328090762, -0.08942795157528024563, -0.3641732283464568787 ) ) ;
#47130 = CARTESIAN_POINT ( 'NONE',  ( 0.2165354330708668673, -0.5400638737290844871, 0.3530559997133364547 ) ) ;
#47131 = CARTESIAN_POINT ( 'NONE',  ( -0.3996062992125985480, -7.340648628747423112E-17, -0.1161417322834645827 ) ) ;
#47132 = CARTESIAN_POINT ( 'NONE',  ( -0.8005249343832013809, -0.4281496062992124485, 0.4176697321401328655 ) ) ;
#47133 = CARTESIAN_POINT ( 'NONE',  ( 4.797336870675656522E-17, -0.3917322834645670104, -1.423228346456693050 ) ) ;
#47134 = CARTESIAN_POINT ( 'NONE',  ( 1.200787401574803681, -0.4536011799217368745, -0.2665933059059886201 ) ) ;
#47135 = CARTESIAN_POINT ( 'NONE',  ( 0.4658792650918641698, -0.05778040916215560624, -0.4822834645669293319 ) ) ;
#47136 = CARTESIAN_POINT ( 'NONE',  ( -0.3805774278215216522, 0.05413385826771666132, 0.4176697321401328100 ) ) ;
#47137 = CARTESIAN_POINT ( 'NONE',  ( -0.3740157480314953431, 0.07958543189024085140, 0.2665933059059887866 ) ) ;
#47138 = DIRECTION ( 'NONE',  ( 0.000000000000000000, 0.000000000000000000, 1.000000000000000000 ) ) ;
#47139 = CARTESIAN_POINT ( 'NONE',  ( 0.02624671916010564918, -0.5023911411419708095, -0.1820866141732282451 ) ) ;
#47140 = CARTESIAN_POINT ( 'NONE',  ( 0.5118110236220480003, -0.6692913385826771977, 8.415575281601705876E-17 ) ) ;
#47141 = EDGE_CURVE ( 'NONE', #32861, #60543, #38024, .T. ) ;
#47142 = CARTESIAN_POINT ( 'NONE',  ( -0.8398950131233589023, -0.5023911411419708095, -0.1820866141732282451 ) ) ;
#47143 = CARTESIAN_POINT ( 'NONE',  ( 0.3996062992125984925, 0.1070741851644054637, -1.146325459317585116 ) ) ;
#47144 = CARTESIAN_POINT ( 'NONE',  ( -1.023622047244093558, -0.1870078740157479769, 0.4822834645669291653 ) ) ;
#47145 = CARTESIAN_POINT ( 'NONE',  ( 0.8561328129276796206, 8.471767977567108961E-16, -0.4445507791589058955 ) ) ;
#47146 = VERTEX_POINT ( 'NONE', #9691 ) ;
#47147 = CARTESIAN_POINT ( 'NONE',  ( -1.233595800524933894, 0.1283753931104748280, 0.1820866141732283561 ) ) ;
#47148 = CARTESIAN_POINT ( 'NONE',  ( 0.04593175853018440641, 0.2952755905511810774, -0.1292274648535930714 ) ) ;
#47149 = CARTESIAN_POINT ( 'NONE',  ( 0.3990339831394616454, 0.0003067303408301115422, -1.220472440944881720 ) ) ;
#47150 = CARTESIAN_POINT ( 'NONE',  ( -0.6036745406824141069, -0.6046776061558809534, -0.2411417322834644161 ) ) ;
#47151 = CARTESIAN_POINT ( 'NONE',  ( 0.4562819726585566893, 1.668167360224330986, -2.130140035730256454 ) ) ;
#47153 = CARTESIAN_POINT ( 'NONE',  ( 1.135170603674541256, 0.2952755905511811885, 0.1292274648535926551 ) ) ;
#47152 = CARTESIAN_POINT ( 'NONE',  ( 0.4800390104732029095, 1.504150543744002810, -0.5309055118110237448 ) ) ;
#47154 = CARTESIAN_POINT ( 'NONE',  ( 0.7152230971128616943, -0.05778040916215522460, 0.4822834645669289988 ) ) ;
#47155 = CARTESIAN_POINT ( 'NONE',  ( 0.000000000000000000, 2.755905511811024056, 0.000000000000000000 ) ) ;
#47156 = CARTESIAN_POINT ( 'NONE',  ( 1.489501312335958172, -0.05778040916215560624, -0.4822834645669293319 ) ) ;
#47157 = CARTESIAN_POINT ( 'NONE',  ( -1.318897637795274802, -0.5400638737290845981, -0.3530559997133363437 ) ) ;
#47158 = CARTESIAN_POINT ( 'NONE',  ( -0.2925321140481930704, -0.2925321140481933480, -0.3740157480314960092 ) ) ;
#47159 = ORIENTED_EDGE ( 'NONE', *, *, #66845, .F. ) ;
#47160 = CARTESIAN_POINT ( 'NONE',  ( -0.3346456692913377662, 0.07958543189024071263, -0.2665933059059888421 ) ) ;
#47161 = CARTESIAN_POINT ( 'NONE',  ( 0.1958661417322836440, -0.3392501089628017219, -2.131233595800524849 ) ) ;
#47162 = ORIENTED_EDGE ( 'NONE', *, *, #45233, .T. ) ;
#47163 = CARTESIAN_POINT ( 'NONE',  ( 0.8727034120734912248, -0.3162353388693409650, -0.4822834645669289433 ) ) ;
#47164 = CARTESIAN_POINT ( 'NONE',  ( -0.1574803149606292529, -0.1870078740157479769, 0.4822834645669291653 ) ) ;
#47165 = CARTESIAN_POINT ( 'NONE',  ( -0.8530183727034112984, 0.05413385826771666132, 0.4176697321401328100 ) ) ;
#47166 = CARTESIAN_POINT ( 'NONE',  ( 1.568241469816273659, -0.05778040916215560624, -0.4822834645669293319 ) ) ;
#47167 = CARTESIAN_POINT ( 'NONE',  ( -1.076115485564303809, -0.5023911411419708095, -0.1820866141732282451 ) ) ;
#47168 = CARTESIAN_POINT ( 'NONE',  ( -0.4697362858026991606, 1.605934398054998047, -2.565479853601120297 ) ) ;
#47169 = CARTESIAN_POINT ( 'NONE',  ( 0.2493438320209980519, 0.05413385826771666132, 0.4176697321401328100 ) ) ;
#47170 = CARTESIAN_POINT ( 'NONE',  ( 0.5511811023622054106, -0.1870078740157480601, -0.3641732283464567677 ) ) ;
#47171 = AXIS2_PLACEMENT_3D ( 'NONE', #76147, #32343, #18487 ) ;
#47172 = CARTESIAN_POINT ( 'NONE',  ( -1.003937007874014853, 0.1660481256975885056, 0.3530559997133364547 ) ) ;
#47173 = CARTESIAN_POINT ( 'NONE',  ( -0.1958661417322834497, -0.3392501089628018884, -1.562972810202412521 ) ) ;
#47174 = CARTESIAN_POINT ( 'NONE',  ( -1.377952755905511140, -0.6692913385826771977, 8.415575281601705876E-17 ) ) ;
#47175 = DIRECTION ( 'NONE',  ( 0.000000000000000000, 0.000000000000000000, -1.000000000000000000 ) ) ;
#47176 = CARTESIAN_POINT ( 'NONE',  ( 1.220472440944882608, 0.2952755905511811885, 0.000000000000000000 ) ) ;
#47177 = CARTESIAN_POINT ( 'NONE',  ( 1.259842519685040019, -0.1870078740157480601, -0.3641732283464567677 ) ) ;
#47178 = ORIENTED_EDGE ( 'NONE', *, *, #60737, .F. ) ;
#47179 = CARTESIAN_POINT ( 'NONE',  ( -0.3949938075777411628, 0.1058382717557497937, 0.1246719160104986374 ) ) ;
#47180 = CARTESIAN_POINT ( 'NONE',  ( -0.2493438320209966919, -0.4281496062992124485, 0.4176697321401328655 ) ) ;
#47181 = ORIENTED_EDGE ( 'NONE', *, *, #2120, .F. ) ;
#47182 = CARTESIAN_POINT ( 'NONE',  ( 0.9186351706036751663, -0.5023911411419708095, 0.1820866141732285504 ) ) ;
#47183 = CARTESIAN_POINT ( 'NONE',  ( -1.167979002624671470, -0.4281496062992127816, -0.4176697321401328100 ) ) ;
#47184 = CARTESIAN_POINT ( 'NONE',  ( 0.8858267716535438430, -0.5400638737290845981, -0.3530559997133363437 ) ) ;
#47185 = CARTESIAN_POINT ( 'NONE',  ( 0.7677165354330716118, -0.5400638737290844871, 0.3530559997133364547 ) ) ;
#47186 = CARTESIAN_POINT ( 'NONE',  ( 0.4068241469816279987, -0.4281496062992127816, -0.4176697321401328100 ) ) ;
#47187 = CARTESIAN_POINT ( 'NONE',  ( -0.5577427821522301654, -0.3162353388693405765, 0.4822834645669290543 ) ) ;
#47188 = CARTESIAN_POINT ( 'NONE',  ( -0.1958661417322836718, 0.3392501089628017219, -1.672572178477690352 ) ) ;
#47189 = CARTESIAN_POINT ( 'NONE',  ( -1.568241469816272105, -0.05778040916215522460, 0.4822834645669289988 ) ) ;
#47190 = CARTESIAN_POINT ( 'NONE',  ( -0.7808398950131222316, -0.3162353388693409650, -0.4822834645669289433 ) ) ;
#47191 = CARTESIAN_POINT ( 'NONE',  ( -0.6036745406824141069, -0.5023911411419708095, -0.1820866141732282451 ) ) ;
#47192 = CARTESIAN_POINT ( 'NONE',  ( -0.1011035889004385513, 0.3790285851608858336, 9.764066473168825796E-18 ) ) ;
#47193 = CONICAL_SURFACE ( 'NONE', #64616, 2.165354330708661568, 0.7853981633974500554 ) ;
#47194 = CARTESIAN_POINT ( 'NONE',  ( 1.528871391076116026, 0.2952755905511811885, 0.1292274648535926551 ) ) ;
#47195 = CARTESIAN_POINT ( 'NONE',  ( -0.5577427821522301654, -0.05778040916215560624, -0.4822834645669293319 ) ) ;
#47196 = CARTESIAN_POINT ( 'NONE',  ( 0.1070741851644053388, 0.3996062992125986035, 0.08727034120734905587 ) ) ;
#47197 = CARTESIAN_POINT ( 'NONE',  ( 0.5643044619422579178, -0.4281496062992127816, -0.4176697321401328100 ) ) ;
#47198 = CARTESIAN_POINT ( 'NONE',  ( 0.3996062992125986035, 0.1070741851644054776, -2.014435695538057569 ) ) ;
#47199 = FACE_OUTER_BOUND ( 'NONE', #47392, .T. ) ;
#47200 =( BOUNDED_SURFACE ( )  B_SPLINE_SURFACE ( 1, 2, ( 
 ( #20669, #33709, #1729, #40439, #52213, #51790, #7196, #71593, #78338, #46322, #65716, #59370, #14783, #27385, #46741, #66119, #8455, #2140, #67366, #10534, #55528, #17272, #61861, #61035, #3798, #2972, #22736, #66956, #48811, #60622, #60210, #16441, #67781, #9288, #29461, #55119, #41270, #80425, #22325, #23142, #9700, #28638, #74095, #73263, #21907, #35370, #81237, #68196, #41674, #3385, #79592, #2560, #29047, #74510, #54296, #15611, #61450, #4202, #16857, #42086, #48395, #28218, #10119, #54719, #47988, #35781, #42492, #80828, #36190, #29866, #8866, #23553, #47569, #34544, #49221, #73687, #74927, #53877, #16027, #66535, #34959, #80010, #50048, #57176, #69420, #25609, #44541, #43305, #57596, #69003, #6257, #62690, #75742, #49635, #5032, #25198, #50864, #31935, #4607, #30700, #18083, #23968, #76564, #63513, #75328, #56364, #11354, #83286, #51272, #81657, #76974, #82063, #62270, #18892, #24376, #42900, #76153, #38245, #63923, #43718, #11775, #5440, #31101, #36592, #68595, #70232, #10935, #37012, #37428, #5843, #12587, #56768, #12177, #37835, #30279, #63101, #55942, #17675, #31519, #82875, #82468, #24783, #50452, #18493, #44136, #69828, #14268, #33609, #32768, #6677, #19725, #51690, #59685, #77393, #8357, #38663, #65616, #40340, #32349, #26458, #34024, #52111, #58010, #20149, #53368, #52531, #71496, #375, #45383, #64759, #20571, #26030, #7098, #26871, #71079, #19304, #2040, #46222, #39927, #7947, #45799, #13422, #27705, #58435, #13008, #44956, #7526, #71918, #66021, #33196, #797, #59272, #58864, #70652, #64341, #39078, #1628, #65190, #27287, #52945, #77819, #13844, #39502, #78659, #1222, #20980, #78239, #46640, #72335, #14683, #79079, #34859, #55021, #79487, #36092, #16752, #40749, #54611, #23043, #28120, #35678, #3281, #80729, #68090, #35266, #60931, #41983, #28946, #21802, #79906, #48710, #9598, #22636, #73993, #29361, #47466, #42391, #10435, #61763, #9187, #66432, #80320, #60109, #61344, #4103, #74408, #29769, #73158, #2870, #22222, #28533, #15507, #41166, #21396, #47051, #54190, #2462, #72743, #53775, #48296, #15091, #3696, #8768, #34442, #66855, #60521, #47878, #16340, #67677, #73583, #10013, #15928, #41575, #67265, #49119, #5342, #56669, #55842, #18397, #76053, #30180, #69323, #11255, #12076, #81961, #49536, #63003, #62172, #10837, #56265, #70132, #57078, #30599, #75645, #68497, #74825, #17985, #37734, #75231, #4511, #50356, #50767, #63408, #31001, #37330, #17169, #11673, #24276, #36913, #49947, #5743, #43621, #82369, #24688, #81139, #76468, #36497, #23454, #44039, #62589, #18795, #42803, #4931, #69732, #44439, #81551, #31414, #82773, #25095, #38147, #12483, #23869, #63819, #17574, #6158, #43207, #55430, #68903, #77288, #14165, #39822, #78558, #76869, #19619, #6996, #12903, #65510, #52424, #38562, #45281, #273, #20884, #14584, #70548, #72235, #70976, #51173, #7842, #13321, #46535, #65081, #27183, #52847, #38974, #51587, #77714, #20044, #25508, #40237, #33509, #65920, #57909, #32663, #78134, #59171, #45696, #1118, #26769, #1529, #25928, #31833, #19201, #20467, #46120, #64242, #71392, #58756, #6577, #57494, #71815, #58330, #83185, #44850, #32248, #64657, #26348, #692, #39398, #52009, #13741, #7419, #33089, #9912, #66758, #28435, #21297, #1943, #54094, #73899, #28019, #14992, #3185, #3601, #48204, #41484, #73486, #27605, #47784, #9092, #47369, #60424, #16240, #79809, #15836, #2775, #33922, #29266, #46950, #59586, #67170, #73059, #54930, #53266, #15409, #34765, #80637, #78976, #41069, #22541, #22126, #74310, #35584, #8671, #22949, #34342, #48616, #53678, #9499, #40649, #79386, #41887, #67580, #16657, #72642, #21705, #35172, #66333, #61247, #28849, #60007, #60833, #2363, #42297, #8257, #54511, #80225, #55750, #4012, #75961, #23775, #31318, #17891, #63314, #5652, #81458, #4420, #30506, #56168, #61671, #50672, #18299, #56983, #10748, #43116, #5245, #43943, #81871, #37234, #62912, #69638, #62080, #11983, #29676, #56576, #82277, #74726, #24183, #11574, #23359, #82680, #24595, #68813, #37637, #24997, #18705, #76371, #62493, #30909, #30087, #49852, #68408 ),
 ( #67994, #10340, #17485, #17075, #36001, #49030, #75552, #55339, #50263, #81047, #42712, #49446, #36405, #75140, #43528, #69227, #11159, #36818, #4828, #38462, #70037, #39296, #58655, #57808, #31735, #44754, #76774, #1431, #19106, #33414, #63724, #7318, #65411, #57400, #51487, #59076, #77190, #83091, #45175, #78458, #77618, #13230, #25412, #70450, #6482, #45601, #51076, #32152, #51911, #12808, #44346, #27087, #71295, #64983, #32987, #70881, #64148, #52750, #175, #38048, #12391, #32567, #13643, #7749, #58229, #25828, #1022, #596, #6064, #19522, #38880, #26675, #6896, #52330, #78036, #64559, #26252, #19951, #20366, #46018, #71712, #14067, #39720, #21198, #2676, #20783, #59905, #80125, #46852, #61148, #41786, #65826, #79709, #48105, #53162, #60736, #28335, #22444, #9812, #60328, #53997, #67067, #22025, #72547, #21608, #73803, #34664, #47685, #15730, #54414, #14894, #67478, #35484, #3500, #34243, #8159, #73380, #1844, #3088, #29166, #16139, #54835, #40554, #27923, #47268, #53581, #66235, #9400, #41386, #46439, #72129, #33824, #28752, #66654, #35070, #14487, #27505, #8573, #2257, #40141, #79290, #59490, #78874, #72958, #15309, #40972, #8991, #36306, #57612, #80945, #38679, #19321, #42202, #56064, #25625, #29576, #37129, #4725, #83303, #70669, #36712, #62387, #43426, #30399, #23261, #81358, #51288, #11054, #24083, #75453, #31951, #48930, #44973, #13025, #64357, #10651, #67898, #81773, #61572, #62813, #6694, #76991, #32364, #74630, #4319, #23670, #29984, #16974, #42614, #80540, #22852, #55648, #3915, #48512, #55239, #49753, #74213, #6275, #16558, #10236, #68314, #35903, #61982, #17791, #69123, #49342, #75042, #17388, #43019, #68713, #11472, #72352, #71511, #45397, #58453, #7113, #15106, #32784, #47065, #77408, #20996, #79093, #71094, #65205, #46658, #13437, #14699, #8783, #53386, #52545, #78675, #77833, #14282, #812, #40355, #52125, #51706, #7962, #59287, #26475, #66034, #8372, #20163, #71933, #13858, #34038, #1236, #45813, #65631, #64774, #39093, #58878, #72757, #59700, #33214, #39517, #2055, #58026, #21412, #78254, #27719, #7542, #39946, #26885, #40762, #20585, #19743, #33624, #1644, #46237, #66447, #390, #27302, #52961, #26048, #74422, #60945, #28549, #41998, #41182, #73174, #35283, #49137, #36106, #9613, #54625, #47481, #28135, #80336, #16769, #54206, #66872, #29375, #29783, #42406, #67693, #16354, #53791, #74007, #3296, #73601, #28960, #68104, #22651, #10028, #48310, #60125, #55445, #15524, #2476, #35693, #15943, #81154, #79502, #41590, #61358, #23470, #21818, #67280, #48725, #3712, #17185, #61777, #34875, #74841, #60536, #42818, #79922, #55036, #9202, #22238, #10450, #4118, #68512, #2887, #47893, #80743, #23057, #34456, #31430, #17591, #24292, #62606, #57510, #76886, #49551, #51188, #81977, #30196, #18810, #49963, #83201, #44054, #6172, #31847, #75660, #30617, #56684, #82385, #4526, #19216, #44457, #25523, #36929, #69338, #57092, #70147, #24702, #63423, #5760, #12499, #4947, #38161, #55858, #82788, #25109, #43222, #50371, #37749, #75246, #44864, #76483, #50782, #18001, #81568, #11270, #68920, #10852, #56280, #36513, #23886, #63835, #62189, #43635, #11688, #37346, #63019, #5356, #31016, #76069, #69746, #18411, #12092, #13335, #32678, #71828, #25943, #58345, #78149, #287, #21310, #1955, #14178, #65525, #7856, #13755, #38988, #53280, #706, #64257, #78990, #58769, #39836, #8270, #1132, #52023, #59185, #26782, #70564, #27617, #51601, #52861, #33103, #33522, #1543, #77304, #64671, #26363, #27197, #7010, #78571, #20480, #52438, #70991, #46134, #12919, #77729, #46550, #20058, #38576, #33935, #32262, #20897, #14597, #19634, #72248, #40250, #65933, #59600, #6591, #57923, #45295, #45711, #71408, #39412, #65095, #7433, #73914, #41901, #80650, #73073, #10353, #36013, #4025, #60437, #34355, #54525, #28033, #29280, #61684, #16671, #81058, #41083, #54107, #47797, #79823, #15422, #66772, #68008, #29689, #22139, #53691, #55352, #79399, #60847, #46963, #3614, #15005, #72655, #34778, #22963, #21718, #80240, #22556, #48629, #60021, #42310, #9105, #40662, #67595, #61260 ) ),
 .UNSPECIFIED., .F., .F., .F. ) 
 B_SPLINE_SURFACE_WITH_KNOTS ( ( 2, 2 ),
 ( 3, 2, 2, 2, 2, 2, 2, 2, 2, 2, 2, 2, 2, 2, 2, 2, 2, 2, 2, 2, 2, 2, 2, 2, 2, 2, 2, 2, 2, 2, 2, 2, 2, 2, 2, 2, 2, 2, 2, 2, 2, 2, 2, 2, 2, 2, 2, 2, 2, 2, 2, 2, 2, 2, 2, 2, 2, 2, 2, 2, 2, 2, 2, 2, 2, 2, 2, 2, 2, 2, 2, 2, 2, 2, 2, 2, 2, 2, 2, 2, 2, 2, 2, 2, 2, 2, 2, 2, 2, 2, 2, 2, 2, 2, 2, 2, 2, 2, 2, 2, 2, 2, 2, 2, 2, 2, 2, 2, 2, 2, 2, 2, 2, 2, 2, 2, 2, 2, 2, 2, 2, 2, 2, 2, 2, 2, 2, 2, 2, 2, 2, 2, 2, 2, 2, 2, 2, 2, 2, 2, 2, 2, 2, 2, 2, 2, 2, 2, 2, 2, 2, 2, 2, 2, 2, 2, 2, 2, 2, 2, 2, 2, 2, 2, 2, 2, 2, 2, 2, 2, 2, 2, 2, 2, 2, 2, 2, 2, 2, 2, 2, 2, 2, 2, 2, 2, 2, 2, 2, 2, 2, 2, 2, 2, 2, 2, 2, 2, 2, 2, 2, 2, 2, 2, 2, 2, 2, 2, 2, 2, 2, 2, 2, 2, 2, 2, 2, 2, 2, 2, 2, 2, 2, 2, 2, 2, 2, 2, 2, 2, 2, 2, 2, 2, 2, 2, 2, 2, 2, 2, 2, 2, 2, 2, 2, 2, 2, 2, 2, 2, 2, 2, 2, 2, 2, 3 ),
 ( 0.000000000000000000, 1.000000000000000000 ),
 ( 0.000000000000000000, 0.003787878787878787984, 0.007575757575757575968, 0.01136363636363636395, 0.01515151515151515194, 0.01893939393939393992, 0.02272727272727272790, 0.02651515151515151589, 0.03030303030303030387, 0.03409090909090908839, 0.03787878787878787984, 0.04166666666666666435, 0.04545454545454545581, 0.04924242424242424032, 0.05303030303030303177, 0.05681818181818181629, 0.06060606060606060774, 0.06439393939393939226, 0.06818181818181817677, 0.07196969696969697516, 0.07575757575757575968, 0.07954545454545454419, 0.08333333333333332871, 0.08712121212121212710, 0.09090909090909091161, 0.09469696969696969613, 0.09848484848484848064, 0.1022727272727272790, 0.1060606060606060635, 0.1098484848484848481, 0.1136363636363636326, 0.1174242424242424310, 0.1212121212121212155, 0.1250000000000000000, 0.1287878787878787845, 0.1325757575757575690, 0.1363636363636363535, 0.1401515151515151381, 0.1439393939393939503, 0.1477272727272727348, 0.1515151515151515194, 0.1553030303030303039, 0.1590909090909090884, 0.1628787878787878729, 0.1666666666666666574, 0.1704545454545454419, 0.1742424242424242542, 0.1780303030303030387, 0.1818181818181818232, 0.1856060606060606077, 0.1893939393939393923, 0.1931818181818181768, 0.1969696969696969613, 0.2007575757575757458, 0.2045454545454545581, 0.2083333333333333426, 0.2121212121212121271, 0.2159090909090909116, 0.2196969696969696961, 0.2234848484848484806, 0.2272727272727272652, 0.2310606060606060497, 0.2348484848484848619, 0.2386363636363636465, 0.2424242424242424310, 0.2462121212121212155, 0.2500000000000000000, 0.2537878787878787845, 0.2575757575757575690, 0.2613636363636363535, 0.2651515151515151381, 0.2689393939393939226, 0.2727272727272727071, 0.2765151515151514916, 0.2803030303030302761, 0.2840909090909091161, 0.2878787878787879007, 0.2916666666666666852, 0.2954545454545454697, 0.2992424242424242542, 0.3030303030303030387, 0.3068181818181818232, 0.3106060606060606077, 0.3143939393939393923, 0.3181818181818181768, 0.3219696969696969613, 0.3257575757575757458, 0.3295454545454545303, 0.3333333333333333148, 0.3371212121212120993, 0.3409090909090908839, 0.3446969696969697239, 0.3484848484848485084, 0.3522727272727272929, 0.3560606060606060774, 0.3598484848484848619, 0.3636363636363636465, 0.3674242424242424310, 0.3712121212121212155, 0.3750000000000000000, 0.3787878787878787845, 0.3825757575757575690, 0.3863636363636363535, 0.3901515151515151381, 0.3939393939393939226, 0.3977272727272727071, 0.4015151515151514916, 0.4053030303030302761, 0.4090909090909091161, 0.4128787878787879007, 0.4166666666666666852, 0.4204545454545454697, 0.4242424242424242542, 0.4280303030303030387, 0.4318181818181818232, 0.4356060606060606077, 0.4393939393939393923, 0.4431818181818181768, 0.4469696969696969613, 0.4507575757575757458, 0.4545454545454545303, 0.4583333333333333148, 0.4621212121212120993, 0.4659090909090908839, 0.4696969696969697239, 0.4734848484848485084, 0.4772727272727272929, 0.4810606060606060774, 0.4848484848484848619, 0.4886363636363636465, 0.4924242424242424310, 0.4962121212121212155, 0.5000000000000000000, 0.5037878787878787845, 0.5075757575757575690, 0.5113636363636363535, 0.5151515151515151381, 0.5189393939393939226, 0.5227272727272727071, 0.5265151515151514916, 0.5303030303030302761, 0.5340909090909090606, 0.5378787878787878451, 0.5416666666666666297, 0.5454545454545454142, 0.5492424242424241987, 0.5530303030303029832, 0.5568181818181817677, 0.5606060606060605522, 0.5643939393939394478, 0.5681818181818182323, 0.5719696969696970168, 0.5757575757575758013, 0.5795454545454545858, 0.5833333333333333703, 0.5871212121212121549, 0.5909090909090909394, 0.5946969696969697239, 0.5984848484848485084, 0.6022727272727272929, 0.6060606060606060774, 0.6098484848484848619, 0.6136363636363636465, 0.6174242424242424310, 0.6212121212121212155, 0.6250000000000000000, 0.6287878787878787845, 0.6325757575757575690, 0.6363636363636363535, 0.6401515151515151381, 0.6439393939393939226, 0.6477272727272727071, 0.6515151515151514916, 0.6553030303030302761, 0.6590909090909090606, 0.6628787878787878451, 0.6666666666666666297, 0.6704545454545454142, 0.6742424242424241987, 0.6780303030303029832, 0.6818181818181817677, 0.6856060606060605522, 0.6893939393939394478, 0.6931818181818182323, 0.6969696969696970168, 0.7007575757575758013, 0.7045454545454545858, 0.7083333333333333703, 0.7121212121212121549, 0.7159090909090909394, 0.7196969696969697239, 0.7234848484848485084, 0.7272727272727272929, 0.7310606060606060774, 0.7348484848484848619, 0.7386363636363636465, 0.7424242424242424310, 0.7462121212121212155, 0.7500000000000000000, 0.7537878787878787845, 0.7575757575757575690, 0.7613636363636363535, 0.7651515151515151381, 0.7689393939393939226, 0.7727272727272727071, 0.7765151515151514916, 0.7803030303030302761, 0.7840909090909090606, 0.7878787878787878451, 0.7916666666666666297, 0.7954545454545454142, 0.7992424242424241987, 0.8030303030303029832, 0.8068181818181817677, 0.8106060606060605522, 0.8143939393939394478, 0.8181818181818182323, 0.8219696969696970168, 0.8257575757575758013, 0.8295454545454545858, 0.8333333333333333703, 0.8371212121212121549, 0.8409090909090909394, 0.8446969696969697239, 0.8484848484848485084, 0.8522727272727272929, 0.8560606060606060774, 0.8598484848484848619, 0.8636363636363636465, 0.8674242424242424310, 0.8712121212121212155, 0.8750000000000000000, 0.8787878787878787845, 0.8825757575757575690, 0.8863636363636363535, 0.8901515151515151381, 0.8939393939393939226, 0.8977272727272727071, 0.9015151515151514916, 0.9053030303030302761, 0.9090909090909090606, 0.9128787878787878451, 0.9166666666666666297, 0.9204545454545454142, 0.9242424242424241987, 0.9280303030303029832, 0.9318181818181817677, 0.9356060606060605522, 0.9393939393939394478, 0.9431818181818182323, 0.9469696969696970168, 0.9507575757575758013, 0.9545454545454545858, 0.9583333333333333703, 0.9621212121212121549, 0.9659090909090909394 ),
 .UNSPECIFIED. ) 
 GEOMETRIC_REPRESENTATION_ITEM ( )  RATIONAL_B_SPLINE_SURFACE ( (
 ( 1.000000000000000000, 0.9659258262890683122, 1.000000000000000000, 0.9659258262890683122, 1.000000000000000000, 0.9659258262890683122, 1.000000000000000000, 0.9659258262890683122, 1.000000000000000000, 0.9659258262890683122, 1.000000000000000000, 0.9659258262890683122, 1.000000000000000000, 0.9659258262890683122, 1.000000000000000000, 0.9659258262890683122, 1.000000000000000000, 0.9659258262890683122, 1.000000000000000000, 0.9659258262890683122, 1.000000000000000000, 0.9659258262890683122, 1.000000000000000000, 0.9659258262890683122, 1.000000000000000000, 0.9659258262890683122, 1.000000000000000000, 0.9659258262890683122, 1.000000000000000000, 0.9659258262890683122, 1.000000000000000000, 0.9659258262890683122, 1.000000000000000000, 0.9659258262890683122, 1.000000000000000000, 0.9659258262890683122, 1.000000000000000000, 0.9659258262890683122, 1.000000000000000000, 0.9659258262890683122, 1.000000000000000000, 0.9659258262890683122, 1.000000000000000000, 0.9659258262890683122, 1.000000000000000000, 0.9659258262890683122, 1.000000000000000000, 0.9659258262890683122, 1.000000000000000000, 0.9659258262890683122, 1.000000000000000000, 0.9659258262890683122, 1.000000000000000000, 0.9659258262890683122, 1.000000000000000000, 0.9659258262890683122, 1.000000000000000000, 0.9659258262890683122, 1.000000000000000000, 0.9659258262890683122, 1.000000000000000000, 0.9659258262890683122, 1.000000000000000000, 0.9659258262890683122, 1.000000000000000000, 0.9659258262890683122, 1.000000000000000000, 0.9659258262890683122, 1.000000000000000000, 0.9659258262890683122, 1.000000000000000000, 0.9659258262890683122, 1.000000000000000000, 0.9659258262890683122, 1.000000000000000000, 0.9659258262890683122, 1.000000000000000000, 0.9659258262890683122, 1.000000000000000000, 0.9659258262890683122, 1.000000000000000000, 0.9659258262890683122, 1.000000000000000000, 0.9659258262890683122, 1.000000000000000000, 0.9659258262890683122, 1.000000000000000000, 0.9659258262890683122, 1.000000000000000000, 0.9659258262890683122, 1.000000000000000000, 0.9659258262890683122, 1.000000000000000000, 0.9659258262890683122, 1.000000000000000000, 0.9659258262890683122, 1.000000000000000000, 0.9659258262890683122, 1.000000000000000000, 0.9659258262890683122, 1.000000000000000000, 0.9659258262890683122, 1.000000000000000000, 0.9659258262890683122, 1.000000000000000000, 0.9659258262890683122, 1.000000000000000000, 0.9659258262890683122, 1.000000000000000000, 0.9659258262890683122, 1.000000000000000000, 0.9659258262890683122, 1.000000000000000000, 0.9659258262890683122, 1.000000000000000000, 0.9659258262890683122, 1.000000000000000000, 0.9659258262890683122, 1.000000000000000000, 0.9659258262890683122, 1.000000000000000000, 0.9659258262890683122, 1.000000000000000000, 0.9659258262890683122, 1.000000000000000000, 0.9659258262890683122, 1.000000000000000000, 0.9659258262890683122, 1.000000000000000000, 0.9659258262890683122, 1.000000000000000000, 0.9659258262890683122, 1.000000000000000000, 0.9659258262890683122, 1.000000000000000000, 0.9659258262890683122, 1.000000000000000000, 0.9659258262890683122, 1.000000000000000000, 0.9659258262890683122, 1.000000000000000000, 0.9659258262890683122, 1.000000000000000000, 0.9659258262890683122, 1.000000000000000000, 0.9659258262890683122, 1.000000000000000000, 0.9659258262890683122, 1.000000000000000000, 0.9659258262890683122, 1.000000000000000000, 0.9659258262890683122, 1.000000000000000000, 0.9659258262890683122, 1.000000000000000000, 0.9659258262890683122, 1.000000000000000000, 0.9659258262890683122, 1.000000000000000000, 0.9659258262890683122, 1.000000000000000000, 0.9659258262890683122, 1.000000000000000000, 0.9659258262890683122, 1.000000000000000000, 0.9659258262890683122, 1.000000000000000000, 0.9659258262890683122, 1.000000000000000000, 0.9659258262890683122, 1.000000000000000000, 0.9659258262890683122, 1.000000000000000000, 0.9659258262890683122, 1.000000000000000000, 0.9659258262890683122, 1.000000000000000000, 0.9659258262890683122, 1.000000000000000000, 0.9659258262890683122, 1.000000000000000000, 0.9659258262890683122, 1.000000000000000000, 0.9659258262890683122, 1.000000000000000000, 0.9659258262890683122, 1.000000000000000000, 0.9659258262890683122, 1.000000000000000000, 0.9659258262890683122, 1.000000000000000000, 0.9659258262890683122, 1.000000000000000000, 0.9659258262890683122, 1.000000000000000000, 0.9659258262890683122, 1.000000000000000000, 0.9659258262890683122, 1.000000000000000000, 0.9659258262890683122, 1.000000000000000000, 0.9659258262890683122, 1.000000000000000000, 0.9659258262890683122, 1.000000000000000000, 0.9659258262890683122, 1.000000000000000000, 0.9659258262890683122, 1.000000000000000000, 0.9659258262890683122, 1.000000000000000000, 0.9659258262890683122, 1.000000000000000000, 0.9659258262890683122, 1.000000000000000000, 0.9659258262890683122, 1.000000000000000000, 0.9659258262890683122, 1.000000000000000000, 0.9659258262890683122, 1.000000000000000000, 0.9659258262890683122, 1.000000000000000000, 0.9659258262890683122, 1.000000000000000000, 0.9659258262890683122, 1.000000000000000000, 0.9659258262890683122, 1.000000000000000000, 0.9659258262890683122, 1.000000000000000000, 0.9659258262890683122, 1.000000000000000000, 0.9659258262890683122, 1.000000000000000000, 0.9659258262890683122, 1.000000000000000000, 0.9659258262890683122, 1.000000000000000000, 0.9659258262890683122, 1.000000000000000000, 0.9659258262890683122, 1.000000000000000000, 0.9659258262890683122, 1.000000000000000000, 0.9659258262890683122, 1.000000000000000000, 0.9659258262890683122, 1.000000000000000000, 0.9659258262890683122, 1.000000000000000000, 0.9659258262890683122, 1.000000000000000000, 0.9659258262890683122, 1.000000000000000000, 0.9659258262890683122, 1.000000000000000000, 0.9659258262890683122, 1.000000000000000000, 0.9659258262890683122, 1.000000000000000000, 0.9659258262890683122, 1.000000000000000000, 0.9659258262890683122, 1.000000000000000000, 0.9659258262890683122, 1.000000000000000000, 0.9659258262890683122, 1.000000000000000000, 0.9659258262890683122, 1.000000000000000000, 0.9659258262890683122, 1.000000000000000000, 0.9659258262890683122, 1.000000000000000000, 0.9659258262890683122, 1.000000000000000000, 0.9659258262890683122, 1.000000000000000000, 0.9659258262890683122, 1.000000000000000000, 0.9659258262890683122, 1.000000000000000000, 0.9659258262890683122, 1.000000000000000000, 0.9659258262890683122, 1.000000000000000000, 0.9659258262890683122, 1.000000000000000000, 0.9659258262890683122, 1.000000000000000000, 0.9659258262890683122, 1.000000000000000000, 0.9659258262890683122, 1.000000000000000000, 0.9659258262890683122, 1.000000000000000000, 0.9659258262890683122, 1.000000000000000000, 0.9659258262890683122, 1.000000000000000000, 0.9659258262890683122, 1.000000000000000000, 0.9659258262890683122, 1.000000000000000000, 0.9659258262890683122, 1.000000000000000000, 0.9659258262890683122, 1.000000000000000000, 0.9659258262890683122, 1.000000000000000000, 0.9659258262890683122, 1.000000000000000000, 0.9659258262890683122, 1.000000000000000000, 0.9659258262890683122, 1.000000000000000000, 0.9659258262890683122, 1.000000000000000000, 0.9659258262890683122, 1.000000000000000000, 0.9659258262890683122, 1.000000000000000000, 0.9659258262890683122, 1.000000000000000000, 0.9659258262890683122, 1.000000000000000000, 0.9659258262890683122, 1.000000000000000000, 0.9659258262890683122, 1.000000000000000000, 0.9659258262890683122, 1.000000000000000000, 0.9659258262890683122, 1.000000000000000000, 0.9659258262890683122, 1.000000000000000000, 0.9659258262890683122, 1.000000000000000000, 0.9659258262890683122, 1.000000000000000000, 0.9659258262890683122, 1.000000000000000000, 0.9659258262890683122, 1.000000000000000000, 0.9659258262890683122, 1.000000000000000000, 0.9659258262890683122, 1.000000000000000000, 0.9659258262890683122, 1.000000000000000000, 0.9659258262890683122, 1.000000000000000000, 0.9659258262890683122, 1.000000000000000000, 0.9659258262890683122, 1.000000000000000000, 0.9659258262890683122, 1.000000000000000000, 0.9659258262890683122, 1.000000000000000000, 0.9659258262890683122, 1.000000000000000000, 0.9659258262890683122, 1.000000000000000000, 0.9659258262890683122, 1.000000000000000000, 0.9659258262890683122, 1.000000000000000000, 0.9659258262890683122, 1.000000000000000000, 0.9659258262890683122, 1.000000000000000000, 0.9659258262890683122, 1.000000000000000000, 0.9659258262890683122, 1.000000000000000000, 0.9659258262890683122, 1.000000000000000000, 0.9659258262890683122, 1.000000000000000000, 0.9659258262890683122, 1.000000000000000000, 0.9659258262890683122, 1.000000000000000000, 0.9659258262890683122, 1.000000000000000000, 0.9659258262890683122, 1.000000000000000000, 0.9659258262890683122, 1.000000000000000000, 0.9659258262890683122, 1.000000000000000000, 0.9659258262890683122, 1.000000000000000000, 0.9659258262890683122, 1.000000000000000000, 0.9659258262890683122, 1.000000000000000000, 0.9659258262890683122, 1.000000000000000000, 0.9659258262890683122, 1.000000000000000000, 0.9659258262890683122, 1.000000000000000000, 0.9659258262890683122, 1.000000000000000000, 0.9659258262890683122, 1.000000000000000000, 0.9659258262890683122, 1.000000000000000000, 0.9659258262890683122, 1.000000000000000000, 0.9659258262890683122, 1.000000000000000000, 0.9659258262890683122, 1.000000000000000000, 0.9659258262890683122, 1.000000000000000000, 0.9659258262890683122, 1.000000000000000000, 0.9659258262890683122, 1.000000000000000000, 0.9659258262890683122, 1.000000000000000000, 0.9659258262890683122, 1.000000000000000000, 0.9659258262890683122, 1.000000000000000000, 0.9659258262890683122, 1.000000000000000000, 0.9659258262890683122, 1.000000000000000000, 0.9659258262890683122, 1.000000000000000000, 0.9659258262890683122, 1.000000000000000000, 0.9659258262890683122, 1.000000000000000000, 0.9659258262890683122, 1.000000000000000000, 0.9659258262890683122, 1.000000000000000000, 0.9659258262890683122, 1.000000000000000000, 0.9659258262890683122, 1.000000000000000000, 0.9659258262890683122, 1.000000000000000000, 0.9659258262890683122, 1.000000000000000000, 0.9659258262890683122, 1.000000000000000000, 0.9659258262890683122, 1.000000000000000000, 0.9659258262890683122, 1.000000000000000000, 0.9659258262890683122, 1.000000000000000000, 0.9659258262890683122, 1.000000000000000000, 0.9659258262890683122, 1.000000000000000000, 0.9659258262890683122, 1.000000000000000000, 0.9659258262890683122, 1.000000000000000000, 0.9659258262890683122, 1.000000000000000000, 0.9659258262890683122, 1.000000000000000000, 0.9659258262890683122, 1.000000000000000000, 0.9659258262890683122, 1.000000000000000000, 0.9659258262890683122, 1.000000000000000000, 0.9659258262890683122, 1.000000000000000000, 0.9659258262890683122, 1.000000000000000000, 0.9659258262890683122, 1.000000000000000000, 0.9659258262890683122, 1.000000000000000000, 0.9659258262890683122, 1.000000000000000000, 0.9659258262890683122, 1.000000000000000000, 0.9659258262890683122, 1.000000000000000000, 0.9659258262890683122, 1.000000000000000000, 0.9659258262890683122, 1.000000000000000000, 0.9659258262890683122, 1.000000000000000000, 0.9659258262890683122, 1.000000000000000000, 0.9659258262890683122, 1.000000000000000000, 0.9659258262890683122, 1.000000000000000000, 0.9659258262890683122, 1.000000000000000000, 0.9659258262890683122, 1.000000000000000000, 0.9659258262890683122, 1.000000000000000000, 0.9659258262890683122, 1.000000000000000000),
 ( 1.000000000000000000, 0.9659258262890683122, 1.000000000000000000, 0.9659258262890683122, 1.000000000000000000, 0.9659258262890683122, 1.000000000000000000, 0.9659258262890683122, 1.000000000000000000, 0.9659258262890683122, 1.000000000000000000, 0.9659258262890683122, 1.000000000000000000, 0.9659258262890683122, 1.000000000000000000, 0.9659258262890683122, 1.000000000000000000, 0.9659258262890683122, 1.000000000000000000, 0.9659258262890683122, 1.000000000000000000, 0.9659258262890683122, 1.000000000000000000, 0.9659258262890683122, 1.000000000000000000, 0.9659258262890683122, 1.000000000000000000, 0.9659258262890683122, 1.000000000000000000, 0.9659258262890683122, 1.000000000000000000, 0.9659258262890683122, 1.000000000000000000, 0.9659258262890683122, 1.000000000000000000, 0.9659258262890683122, 1.000000000000000000, 0.9659258262890683122, 1.000000000000000000, 0.9659258262890683122, 1.000000000000000000, 0.9659258262890683122, 1.000000000000000000, 0.9659258262890683122, 1.000000000000000000, 0.9659258262890683122, 1.000000000000000000, 0.9659258262890683122, 1.000000000000000000, 0.9659258262890683122, 1.000000000000000000, 0.9659258262890683122, 1.000000000000000000, 0.9659258262890683122, 1.000000000000000000, 0.9659258262890683122, 1.000000000000000000, 0.9659258262890683122, 1.000000000000000000, 0.9659258262890683122, 1.000000000000000000, 0.9659258262890683122, 1.000000000000000000, 0.9659258262890683122, 1.000000000000000000, 0.9659258262890683122, 1.000000000000000000, 0.9659258262890683122, 1.000000000000000000, 0.9659258262890683122, 1.000000000000000000, 0.9659258262890683122, 1.000000000000000000, 0.9659258262890683122, 1.000000000000000000, 0.9659258262890683122, 1.000000000000000000, 0.9659258262890683122, 1.000000000000000000, 0.9659258262890683122, 1.000000000000000000, 0.9659258262890683122, 1.000000000000000000, 0.9659258262890683122, 1.000000000000000000, 0.9659258262890683122, 1.000000000000000000, 0.9659258262890683122, 1.000000000000000000, 0.9659258262890683122, 1.000000000000000000, 0.9659258262890683122, 1.000000000000000000, 0.9659258262890683122, 1.000000000000000000, 0.9659258262890683122, 1.000000000000000000, 0.9659258262890683122, 1.000000000000000000, 0.9659258262890683122, 1.000000000000000000, 0.9659258262890683122, 1.000000000000000000, 0.9659258262890683122, 1.000000000000000000, 0.9659258262890683122, 1.000000000000000000, 0.9659258262890683122, 1.000000000000000000, 0.9659258262890683122, 1.000000000000000000, 0.9659258262890683122, 1.000000000000000000, 0.9659258262890683122, 1.000000000000000000, 0.9659258262890683122, 1.000000000000000000, 0.9659258262890683122, 1.000000000000000000, 0.9659258262890683122, 1.000000000000000000, 0.9659258262890683122, 1.000000000000000000, 0.9659258262890683122, 1.000000000000000000, 0.9659258262890683122, 1.000000000000000000, 0.9659258262890683122, 1.000000000000000000, 0.9659258262890683122, 1.000000000000000000, 0.9659258262890683122, 1.000000000000000000, 0.9659258262890683122, 1.000000000000000000, 0.9659258262890683122, 1.000000000000000000, 0.9659258262890683122, 1.000000000000000000, 0.9659258262890683122, 1.000000000000000000, 0.9659258262890683122, 1.000000000000000000, 0.9659258262890683122, 1.000000000000000000, 0.9659258262890683122, 1.000000000000000000, 0.9659258262890683122, 1.000000000000000000, 0.9659258262890683122, 1.000000000000000000, 0.9659258262890683122, 1.000000000000000000, 0.9659258262890683122, 1.000000000000000000, 0.9659258262890683122, 1.000000000000000000, 0.9659258262890683122, 1.000000000000000000, 0.9659258262890683122, 1.000000000000000000, 0.9659258262890683122, 1.000000000000000000, 0.9659258262890683122, 1.000000000000000000, 0.9659258262890683122, 1.000000000000000000, 0.9659258262890683122, 1.000000000000000000, 0.9659258262890683122, 1.000000000000000000, 0.9659258262890683122, 1.000000000000000000, 0.9659258262890683122, 1.000000000000000000, 0.9659258262890683122, 1.000000000000000000, 0.9659258262890683122, 1.000000000000000000, 0.9659258262890683122, 1.000000000000000000, 0.9659258262890683122, 1.000000000000000000, 0.9659258262890683122, 1.000000000000000000, 0.9659258262890683122, 1.000000000000000000, 0.9659258262890683122, 1.000000000000000000, 0.9659258262890683122, 1.000000000000000000, 0.9659258262890683122, 1.000000000000000000, 0.9659258262890683122, 1.000000000000000000, 0.9659258262890683122, 1.000000000000000000, 0.9659258262890683122, 1.000000000000000000, 0.9659258262890683122, 1.000000000000000000, 0.9659258262890683122, 1.000000000000000000, 0.9659258262890683122, 1.000000000000000000, 0.9659258262890683122, 1.000000000000000000, 0.9659258262890683122, 1.000000000000000000, 0.9659258262890683122, 1.000000000000000000, 0.9659258262890683122, 1.000000000000000000, 0.9659258262890683122, 1.000000000000000000, 0.9659258262890683122, 1.000000000000000000, 0.9659258262890683122, 1.000000000000000000, 0.9659258262890683122, 1.000000000000000000, 0.9659258262890683122, 1.000000000000000000, 0.9659258262890683122, 1.000000000000000000, 0.9659258262890683122, 1.000000000000000000, 0.9659258262890683122, 1.000000000000000000, 0.9659258262890683122, 1.000000000000000000, 0.9659258262890683122, 1.000000000000000000, 0.9659258262890683122, 1.000000000000000000, 0.9659258262890683122, 1.000000000000000000, 0.9659258262890683122, 1.000000000000000000, 0.9659258262890683122, 1.000000000000000000, 0.9659258262890683122, 1.000000000000000000, 0.9659258262890683122, 1.000000000000000000, 0.9659258262890683122, 1.000000000000000000, 0.9659258262890683122, 1.000000000000000000, 0.9659258262890683122, 1.000000000000000000, 0.9659258262890683122, 1.000000000000000000, 0.9659258262890683122, 1.000000000000000000, 0.9659258262890683122, 1.000000000000000000, 0.9659258262890683122, 1.000000000000000000, 0.9659258262890683122, 1.000000000000000000, 0.9659258262890683122, 1.000000000000000000, 0.9659258262890683122, 1.000000000000000000, 0.9659258262890683122, 1.000000000000000000, 0.9659258262890683122, 1.000000000000000000, 0.9659258262890683122, 1.000000000000000000, 0.9659258262890683122, 1.000000000000000000, 0.9659258262890683122, 1.000000000000000000, 0.9659258262890683122, 1.000000000000000000, 0.9659258262890683122, 1.000000000000000000, 0.9659258262890683122, 1.000000000000000000, 0.9659258262890683122, 1.000000000000000000, 0.9659258262890683122, 1.000000000000000000, 0.9659258262890683122, 1.000000000000000000, 0.9659258262890683122, 1.000000000000000000, 0.9659258262890683122, 1.000000000000000000, 0.9659258262890683122, 1.000000000000000000, 0.9659258262890683122, 1.000000000000000000, 0.9659258262890683122, 1.000000000000000000, 0.9659258262890683122, 1.000000000000000000, 0.9659258262890683122, 1.000000000000000000, 0.9659258262890683122, 1.000000000000000000, 0.9659258262890683122, 1.000000000000000000, 0.9659258262890683122, 1.000000000000000000, 0.9659258262890683122, 1.000000000000000000, 0.9659258262890683122, 1.000000000000000000, 0.9659258262890683122, 1.000000000000000000, 0.9659258262890683122, 1.000000000000000000, 0.9659258262890683122, 1.000000000000000000, 0.9659258262890683122, 1.000000000000000000, 0.9659258262890683122, 1.000000000000000000, 0.9659258262890683122, 1.000000000000000000, 0.9659258262890683122, 1.000000000000000000, 0.9659258262890683122, 1.000000000000000000, 0.9659258262890683122, 1.000000000000000000, 0.9659258262890683122, 1.000000000000000000, 0.9659258262890683122, 1.000000000000000000, 0.9659258262890683122, 1.000000000000000000, 0.9659258262890683122, 1.000000000000000000, 0.9659258262890683122, 1.000000000000000000, 0.9659258262890683122, 1.000000000000000000, 0.9659258262890683122, 1.000000000000000000, 0.9659258262890683122, 1.000000000000000000, 0.9659258262890683122, 1.000000000000000000, 0.9659258262890683122, 1.000000000000000000, 0.9659258262890683122, 1.000000000000000000, 0.9659258262890683122, 1.000000000000000000, 0.9659258262890683122, 1.000000000000000000, 0.9659258262890683122, 1.000000000000000000, 0.9659258262890683122, 1.000000000000000000, 0.9659258262890683122, 1.000000000000000000, 0.9659258262890683122, 1.000000000000000000, 0.9659258262890683122, 1.000000000000000000, 0.9659258262890683122, 1.000000000000000000, 0.9659258262890683122, 1.000000000000000000, 0.9659258262890683122, 1.000000000000000000, 0.9659258262890683122, 1.000000000000000000, 0.9659258262890683122, 1.000000000000000000, 0.9659258262890683122, 1.000000000000000000, 0.9659258262890683122, 1.000000000000000000, 0.9659258262890683122, 1.000000000000000000, 0.9659258262890683122, 1.000000000000000000, 0.9659258262890683122, 1.000000000000000000, 0.9659258262890683122, 1.000000000000000000, 0.9659258262890683122, 1.000000000000000000, 0.9659258262890683122, 1.000000000000000000, 0.9659258262890683122, 1.000000000000000000, 0.9659258262890683122, 1.000000000000000000, 0.9659258262890683122, 1.000000000000000000, 0.9659258262890683122, 1.000000000000000000, 0.9659258262890683122, 1.000000000000000000, 0.9659258262890683122, 1.000000000000000000, 0.9659258262890683122, 1.000000000000000000, 0.9659258262890683122, 1.000000000000000000, 0.9659258262890683122, 1.000000000000000000, 0.9659258262890683122, 1.000000000000000000, 0.9659258262890683122, 1.000000000000000000, 0.9659258262890683122, 1.000000000000000000, 0.9659258262890683122, 1.000000000000000000, 0.9659258262890683122, 1.000000000000000000, 0.9659258262890683122, 1.000000000000000000, 0.9659258262890683122, 1.000000000000000000, 0.9659258262890683122, 1.000000000000000000, 0.9659258262890683122, 1.000000000000000000, 0.9659258262890683122, 1.000000000000000000, 0.9659258262890683122, 1.000000000000000000, 0.9659258262890683122, 1.000000000000000000, 0.9659258262890683122, 1.000000000000000000, 0.9659258262890683122, 1.000000000000000000, 0.9659258262890683122, 1.000000000000000000, 0.9659258262890683122, 1.000000000000000000, 0.9659258262890683122, 1.000000000000000000, 0.9659258262890683122, 1.000000000000000000, 0.9659258262890683122, 1.000000000000000000, 0.9659258262890683122, 1.000000000000000000, 0.9659258262890683122, 1.000000000000000000, 0.9659258262890683122, 1.000000000000000000, 0.9659258262890683122, 1.000000000000000000, 0.9659258262890683122, 1.000000000000000000, 0.9659258262890683122, 1.000000000000000000, 0.9659258262890683122, 1.000000000000000000, 0.9659258262890683122, 1.000000000000000000, 0.9659258262890683122, 1.000000000000000000, 0.9659258262890683122, 1.000000000000000000, 0.9659258262890683122, 1.000000000000000000, 0.9659258262890683122, 1.000000000000000000, 0.9659258262890683122, 1.000000000000000000, 0.9659258262890683122, 1.000000000000000000, 0.9659258262890683122, 1.000000000000000000, 0.9659258262890683122, 1.000000000000000000, 0.9659258262890683122, 1.000000000000000000, 0.9659258262890683122, 1.000000000000000000, 0.9659258262890683122, 1.000000000000000000, 0.9659258262890683122, 1.000000000000000000, 0.9659258262890683122, 1.000000000000000000, 0.9659258262890683122, 1.000000000000000000, 0.9659258262890683122, 1.000000000000000000, 0.9659258262890683122, 1.000000000000000000, 0.9659258262890683122, 1.000000000000000000, 0.9659258262890683122, 1.000000000000000000, 0.9659258262890683122, 1.000000000000000000, 0.9659258262890683122, 1.000000000000000000, 0.9659258262890683122, 1.000000000000000000, 0.9659258262890683122, 1.000000000000000000, 0.9659258262890683122, 1.000000000000000000, 0.9659258262890683122, 1.000000000000000000) ) ) 
 REPRESENTATION_ITEM ( '' )  SURFACE ( )  );
#47201 = CARTESIAN_POINT ( 'NONE',  ( -0.2230971128608915943, 0.05413385826771666132, 0.4176697321401328100 ) ) ;
#47203 = CARTESIAN_POINT ( 'NONE',  ( 0.4849061582275022153, 1.967896864084103914, -0.4921425059946357705 ) ) ;
#47202 = CARTESIAN_POINT ( 'NONE',  ( 1.194225721784777594, -0.004921259842519576551, 0.3153832671262227771 ) ) ;
#47204 = CARTESIAN_POINT ( 'NONE',  ( -0.4724409448818898682, -8.678599364036362592E-17, -0.5885826771653542844 ) ) ;
#47205 = CARTESIAN_POINT ( 'NONE',  ( 1.003937007874016407, -0.4536011799217367080, 0.2665933059059888421 ) ) ;
#47206 = CARTESIAN_POINT ( 'NONE',  ( 1.246719160104987623, -0.4281496062992124485, 0.4176697321401328655 ) ) ;
#47207 = CARTESIAN_POINT ( 'NONE',  ( -0.3949938075777411073, 0.1058382717557497660, -0.2670603674540682482 ) ) ;
#47208 = CARTESIAN_POINT ( 'NONE',  ( -0.3149606299212590610, -0.1870078740157479769, 0.4822834645669291653 ) ) ;
#47209 = CARTESIAN_POINT ( 'NONE',  ( -1.594488188976377119, 0.1660481256975883668, -0.3530559997133364547 ) ) ;
#47210 = CARTESIAN_POINT ( 'NONE',  ( 1.364829396325459854, -0.5023911411419708095, -0.1820866141732282451 ) ) ;
#47211 = CARTESIAN_POINT ( 'NONE',  ( 0.01312335958005323398, 0.05413385826771666132, 0.4176697321401328100 ) ) ;
#47212 = CARTESIAN_POINT ( 'NONE',  ( -0.3949938075777409963, -7.255918531996591613E-17, -0.5885826771653542844 ) ) ;
#47213 = CARTESIAN_POINT ( 'NONE',  ( 1.233595800524935227, 0.2306618581243847221, -0.2411417322834647770 ) ) ;
#47214 = CARTESIAN_POINT ( 'NONE',  ( 0.3871391076115492380, -0.05778040916215560624, -0.4822834645669293319 ) ) ;
#47215 = CARTESIAN_POINT ( 'NONE',  ( 0.4986876640419954376, -0.5023911411419708095, -0.1820866141732282451 ) ) ;
#47216 = CARTESIAN_POINT ( 'NONE',  ( 0.4091458600556404646, -0.2362204724409448231, -0.1817585301837270351 ) ) ;
#47217 = CARTESIAN_POINT ( 'NONE',  ( 0.3149606299212606708, -0.1870078740157480601, -0.3641732283464567677 ) ) ;
#47218 = CARTESIAN_POINT ( 'NONE',  ( -1.036041590146031366, -2.613618158232546091E-15, -0.3464511005275220379 ) ) ;
#47219 = B_SPLINE_CURVE_WITH_KNOTS ( 'NONE', 3,
 ( #59761, #53445, #60185, #66509, #10091, #29436, #2537, #67342, #41245, #9675 ),
 .UNSPECIFIED., .F., .F.,
 ( 4, 2, 2, 2, 4 ),
 ( 0.000000000000000000, 0.2500000000000000000, 0.3750000000000000000, 0.5000000000000000000, 1.000000000000000000 ),
 .UNSPECIFIED. ) ;
#47220 = CARTESIAN_POINT ( 'NONE',  ( -0.2925321140481932369, 0.2925321140481931259, -1.513779527559055094 ) ) ;
#47221 = CARTESIAN_POINT ( 'NONE',  ( 0.6299212598425204535, -0.1870078740157480879, -0.4822834645669291653 ) ) ;
#47222 = CARTESIAN_POINT ( 'NONE',  ( -0.3392501089628019995, 0.1958661417322832277, -1.278215223097112885 ) ) ;
#47223 = DIRECTION ( 'NONE',  ( -3.096699300667737957E-16, 1.000000000000000000, -0.000000000000000000 ) ) ;
#47224 = LINE ( 'NONE', #72913, #11012 ) ;
#47225 = CARTESIAN_POINT ( 'NONE',  ( 0.03280839895013198948, 0.1771653543307087630, 0.09757992244046791164 ) ) ;
#47226 = CARTESIAN_POINT ( 'NONE',  ( -0.07217847769028787330, -0.05778040916215522460, 0.4822834645669289988 ) ) ;
#47227 = CARTESIAN_POINT ( 'NONE',  ( 1.509186351706037543, -0.004921259842519576551, 0.3153832671262227771 ) ) ;
#47228 = CARTESIAN_POINT ( 'NONE',  ( -1.384514435695537005, 0.1771653543307087630, 0.09757992244046791164 ) ) ;
#47229 = CARTESIAN_POINT ( 'NONE',  ( -1.030183727034119867, -0.05778040916215560624, -0.4822834645669293319 ) ) ;
#47230 = AXIS2_PLACEMENT_3D ( 'NONE', #30842, #48960, #75890 ) ;
#47231 = CARTESIAN_POINT ( 'NONE',  ( 0.5511811023622055217, -0.1870078740157479769, 0.4822834645669291653 ) ) ;
#47232 = CARTESIAN_POINT ( 'NONE',  ( 1.391076115485564868, 0.2306618581243847221, -0.2411417322834647770 ) ) ;
#47233 = CARTESIAN_POINT ( 'NONE',  ( 0.1133856558944469489, 0.2726377952755905665, 0.1574803149606299191 ) ) ;
#47234 = CARTESIAN_POINT ( 'NONE',  ( 0.4658792650918640033, -0.3162353388693405765, 0.4822834645669290543 ) ) ;
#47235 = CARTESIAN_POINT ( 'NONE',  ( 0.4724409448818897572, -0.1265901696524988906, -2.865485564304462329 ) ) ;
#47236 = CARTESIAN_POINT ( 'NONE',  ( 0.4177787735907000366, 0.4110443821404751730, -1.382006255033530806 ) ) ;
#47237 = CARTESIAN_POINT ( 'NONE',  ( 1.148293963254593875, -0.6692913385826771977, 0.1292274648535927661 ) ) ;
#47238 = CARTESIAN_POINT ( 'NONE',  ( -1.345144356955379816, -0.08942795157528024563, -0.3641732283464568787 ) ) ;
#47239 = CARTESIAN_POINT ( 'NONE',  ( 1.358267716535433323, 0.07958543189024085140, 0.2665933059059887866 ) ) ;
#47240 = CARTESIAN_POINT ( 'NONE',  ( -1.377952755905511140, -0.5511811023622047445, 6.969142054262312111E-17 ) ) ;
#47241 = CARTESIAN_POINT ( 'NONE',  ( -0.8070866141732276899, 0.07958543189024071263, -0.2665933059059888421 ) ) ;
#47242 = EDGE_CURVE ( 'NONE', #1065, #22644, #14028, .T. ) ;
#47243 = CARTESIAN_POINT ( 'NONE',  ( 1.528871391076116026, -0.6692913385826773087, -0.1292274648535924053 ) ) ;
#47244 = CARTESIAN_POINT ( 'NONE',  ( 0.5577427821522314977, -0.2845877964562161244, -0.3641732283464567121 ) ) ;
#47245 = CARTESIAN_POINT ( 'NONE',  ( 0.3149606299212606708, -0.1870078740157480879, -0.4822834645669291653 ) ) ;
#47246 = CARTESIAN_POINT ( 'NONE',  ( 1.167979002624672580, 0.05413385826771626580, -0.4176697321401330321 ) ) ;
#47247 = CARTESIAN_POINT ( 'NONE',  ( 0.2230971128608932319, -0.4281496062992124485, 0.4176697321401328655 ) ) ;
#47248 = CARTESIAN_POINT ( 'NONE',  ( 5.463695987328526437E-16, -0.1870078740157479769, 0.3641732283464567677 ) ) ;
#47249 = CARTESIAN_POINT ( 'NONE',  ( 1.049868766404200127, -0.6046776061558809534, -0.2411417322834644161 ) ) ;
#47250 = CARTESIAN_POINT ( 'NONE',  ( -0.1968503937007867743, 0.2066929133858268208, 0.000000000000000000 ) ) ;
#47251 = CARTESIAN_POINT ( 'NONE',  ( -1.108923884514435132, -0.3162353388693405765, 0.4822834645669290543 ) ) ;
#47252 = CARTESIAN_POINT ( 'NONE',  ( -0.2925321140481932369, 0.2925321140481931814, -0.8070866141732283561 ) ) ;
#47253 = CARTESIAN_POINT ( 'NONE',  ( -0.2321974025225331806, 1.091524521067366083, 0.2110349409267623655 ) ) ;
#47254 = CARTESIAN_POINT ( 'NONE',  ( -0.8005249343832011588, 0.05413385826771626580, -0.4176697321401330321 ) ) ;
#47255 = CARTESIAN_POINT ( 'NONE',  ( -0.1115485564304456306, 0.2952755905511810774, -0.1292274648535930714 ) ) ;
#47256 = CARTESIAN_POINT ( 'NONE',  ( -0.1070741851644051862, -0.3996062992125987146, -2.591863517060367439 ) ) ;
#47257 = CARTESIAN_POINT ( 'NONE',  ( 0.3420746716998660508, -0.1974969037888703871, -2.309711286089239035 ) ) ;
#47258 = ORIENTED_EDGE ( 'NONE', *, *, #32702, .F. ) ;
#47259 = CARTESIAN_POINT ( 'NONE',  ( -0.1958661417322836718, 0.3392501089628017219, -0.9501312335958004285 ) ) ;
#47260 = CARTESIAN_POINT ( 'NONE',  ( 1.023622047244095112, -0.1870078740157480879, -0.4822834645669291653 ) ) ;
#47261 = CARTESIAN_POINT ( 'NONE',  ( 3.842312626974349943, 2.753838553078471918, -0.5314960629921259283 ) ) ;
#47262 = CARTESIAN_POINT ( 'NONE',  ( -1.502624671916009680, -0.08942795157528024563, -0.3641732283464568787 ) ) ;
#47263 = CARTESIAN_POINT ( 'NONE',  ( 0.3917322834645670104, -0.1049643490035303411, -1.206036745406823707 ) ) ;
#47264 = CARTESIAN_POINT ( 'NONE',  ( 1.574803149606299746, -0.1870078740157479769, 0.3641732283464567677 ) ) ;
#47265 = CARTESIAN_POINT ( 'NONE',  ( 0.2867679344610365999, -0.2867679344610365999, -0.3359386894675047142 ) ) ;
#47266 = CARTESIAN_POINT ( 'NONE',  ( -0.1706036745406816491, 0.05413385826771626580, -0.4176697321401330321 ) ) ;
#47267 = CARTESIAN_POINT ( 'NONE',  ( -0.4921259842519677963, -0.4536011799217367080, 0.2665933059059888421 ) ) ;
#47268 = CARTESIAN_POINT ( 'NONE',  ( 0.8005249343832027131, 0.05413385826771666132, 0.4176697321401328100 ) ) ;
#47269 = CARTESIAN_POINT ( 'NONE',  ( 0.4921259842519691285, 0.1660481256975885056, 0.3530559997133364547 ) ) ;
#47270 = CARTESIAN_POINT ( 'NONE',  ( -1.157146581871515012E-16, 0.4724409448818898682, -0.07677165354330710290 ) ) ;
#47271 = LINE ( 'NONE', #42618, #51643 ) ;
#47272 = CARTESIAN_POINT ( 'NONE',  ( 0.1958661417322836718, -0.3392501089628017219, -1.820885457514122452 ) ) ;
#47273 = CARTESIAN_POINT ( 'NONE',  ( 1.364829396325460076, 0.2306618581243848609, 0.2411417322834645549 ) ) ;
#47274 = CARTESIAN_POINT ( 'NONE',  ( 0.2296587926509192634, -0.05778040916215560624, -0.4822834645669293319 ) ) ;
#47275 = CARTESIAN_POINT ( 'NONE',  ( -1.043307086614172041, -0.5400638737290844871, 0.3530559997133364547 ) ) ;
#47276 = CARTESIAN_POINT ( 'NONE',  ( 1.318897637795276356, 0.1660481256975883668, -0.3530559997133364547 ) ) ;
#47277 = CARTESIAN_POINT ( 'NONE',  ( 0.7808398950131241190, -0.05778040916215560624, -0.4822834645669293319 ) ) ;
#47278 = CARTESIAN_POINT ( 'NONE',  ( 4.797336870675656522E-17, -0.3917322834645670104, -0.6358267716535433989 ) ) ;
#47279 = CARTESIAN_POINT ( 'NONE',  ( 5.463695987328526437E-16, -0.1870078740157479769, 0.4822834645669291653 ) ) ;
#47280 = CARTESIAN_POINT ( 'NONE',  ( 0.5183727034120741983, -0.6692913385826771977, 0.1292274648535927661 ) ) ;
#47281 = CARTESIAN_POINT ( 'NONE',  ( 0.1509186351706045259, -0.05778040916215560624, -0.4822834645669293319 ) ) ;
#47282 = CARTESIAN_POINT ( 'NONE',  ( 0.9120734908136490793, 0.1771653543307087075, -0.09757992244046823083 ) ) ;
#47283 = CARTESIAN_POINT ( 'NONE',  ( -1.522309711286088607, 0.2306618581243847221, -0.2411417322834647770 ) ) ;
#47284 = CARTESIAN_POINT ( 'NONE',  ( -1.496062992125983815, -0.1870078740157480879, -0.4822834645669291653 ) ) ;
#47285 = CARTESIAN_POINT ( 'NONE',  ( 0.5643044619422579178, -0.4281496062992127816, -0.4176697321401328100 ) ) ;
#47286 = CIRCLE ( 'NONE', #75549, 3.858267716535433323 ) ;
#47287 = CARTESIAN_POINT ( 'NONE',  ( -0.3458507752293909498, 0.3458507752293908388, -0.5688976377952755792 ) ) ;
#47288 = CARTESIAN_POINT ( 'NONE',  ( 0.1958661417322834775, 0.3392501089628018884, -2.183727034120734878 ) ) ;
#47289 = ORIENTED_EDGE ( 'NONE', *, *, #26230, .F. ) ;
#47290 = CARTESIAN_POINT ( 'NONE',  ( -0.3460692066303958092, -0.1998031496062994683, -0.5249343832020997302 ) ) ;
#47291 = EDGE_LOOP ( 'NONE', ( #4600, #67684, #22131 ) ) ;
#47292 = CARTESIAN_POINT ( 'NONE',  ( 0.9514435695538062676, -0.3162353388693409650, -0.4822834645669289433 ) ) ;
#47293 = CARTESIAN_POINT ( 'NONE',  ( 0.5446194225721792126, -0.08942795157528024563, -0.3641732283464568787 ) ) ;
#47294 = FACE_OUTER_BOUND ( 'NONE', #74001, .T. ) ;
#47295 = CARTESIAN_POINT ( 'NONE',  ( 0.000000000000000000, 0.7086614173228346081, 0.000000000000000000 ) ) ;
#47296 = DIRECTION ( 'NONE',  ( 0.000000000000000000, 0.000000000000000000, 1.000000000000000000 ) ) ;
#47297 = CARTESIAN_POINT ( 'NONE',  ( 0.1958661417322834775, 0.3392501089628018884, -1.173884514435695525 ) ) ;
#47298 = CARTESIAN_POINT ( 'NONE',  ( -0.3996062992125985480, -7.340648628747423112E-17, -1.848425196850393526 ) ) ;
#47299 = CARTESIAN_POINT ( 'NONE',  ( -1.614173228346455824, 0.2952755905511811885, 0.000000000000000000 ) ) ;
#47300 = CARTESIAN_POINT ( 'NONE',  ( -0.2362204724409442680, -0.1870078740157480879, -0.4822834645669291653 ) ) ;
#47301 = CARTESIAN_POINT ( 'NONE',  ( 0.8923884514435701520, -0.6046776061558809534, -0.2411417322834644161 ) ) ;
#47302 = ORIENTED_EDGE ( 'NONE', *, *, #67469, .F. ) ;
#47303 = CARTESIAN_POINT ( 'NONE',  ( -1.548556430446193399, 0.2306618581243848609, 0.2411417322834645549 ) ) ;
#47304 = CARTESIAN_POINT ( 'NONE',  ( 1.620734908136483465, -0.5511811023622046335, 0.09757992244046803654 ) ) ;
#47305 = DIRECTION ( 'NONE',  ( -9.948661822760397493E-18, 1.000000000000000000, -6.123233995736777129E-17 ) ) ;
#47306 = CARTESIAN_POINT ( 'NONE',  ( 1.463254593175853824, -0.5511811023622046335, 0.09757992244046803654 ) ) ;
#47307 = CARTESIAN_POINT ( 'NONE',  ( -0.3503937007874015630, 0.3733313776025732333, -0.4921259842519685179 ) ) ;
#47308 = CARTESIAN_POINT ( 'NONE',  ( -1.305774278215222184, 0.1771653543307087630, 0.09757992244046791164 ) ) ;
#47309 = CARTESIAN_POINT ( 'NONE',  ( -0.3392501089628019995, 0.1958661417322832277, 0.1391076115485564701 ) ) ;
#47310 = CARTESIAN_POINT ( 'NONE',  ( 0.2493438320209980519, 0.05413385826771666132, 0.4176697321401328100 ) ) ;
#47311 = ORIENTED_EDGE ( 'NONE', *, *, #38741, .F. ) ;
#47313 = DIRECTION ( 'NONE',  ( 0.000000000000000000, 0.000000000000000000, -1.000000000000000000 ) ) ;
#47312 = CARTESIAN_POINT ( 'NONE',  ( 1.574803149606299746, -0.1870078740157480879, -0.4822834645669291653 ) ) ;
#47314 = CARTESIAN_POINT ( 'NONE',  ( -0.6430446194225716283, -0.3690944881889763329, 0.3153832671262228327 ) ) ;
#47315 = CARTESIAN_POINT ( 'NONE',  ( 0.8070866141732289112, -0.5400638737290845981, -0.3530559997133363437 ) ) ;
#47316 = CARTESIAN_POINT ( 'NONE',  ( 1.371391076115485719, -0.5511811023622048555, -0.09757992244046775898 ) ) ;
#47317 = CARTESIAN_POINT ( 'NONE',  ( -0.3392501089628019439, 0.1958661417322832554, -1.366122416501625469 ) ) ;
#47318 = CARTESIAN_POINT ( 'NONE',  ( -0.7808398950131225646, -0.08942795157527998196, 0.3641732283464567121 ) ) ;
#47319 = CARTESIAN_POINT ( 'NONE',  ( -1.384514435695537005, -0.5511811023622048555, -0.09757992244046775898 ) ) ;
#47320 = CARTESIAN_POINT ( 'NONE',  ( 0.01582383426708340937, 1.954428616053095924, 0.3129921259842521342 ) ) ;
#47321 = CARTESIAN_POINT ( 'NONE',  ( 0.4593175853018379162, -0.4281496062992124485, 0.4176697321401328655 ) ) ;
#47322 = CARTESIAN_POINT ( 'NONE',  ( -0.8202099737532799750, 0.1771653543307087075, -0.09757992244046823083 ) ) ;
#47323 = CARTESIAN_POINT ( 'NONE',  ( -0.4068241469816267775, -0.004921259842519870586, -0.3153832671262229437 ) ) ;
#47324 = CARTESIAN_POINT ( 'NONE',  ( -0.1968503937007867743, -0.6692913385826771977, 8.415575281601705876E-17 ) ) ;
#47325 = CARTESIAN_POINT ( 'NONE',  ( -1.535433070866141225, -0.5511811023622047445, 6.969142054262312111E-17 ) ) ;
#47326 = CARTESIAN_POINT ( 'NONE',  ( -0.3392501089628019995, 0.1958661417322831999, -0.02298519504693102150 ) ) ;
#47327 = CARTESIAN_POINT ( 'NONE',  ( 0.5314960629921264834, 0.1660481256975883668, -0.3530559997133364547 ) ) ;
#47328 = B_SPLINE_CURVE_WITH_KNOTS ( 'NONE', 3,
 ( #32921, #21542, #46790, #58587 ),
 .UNSPECIFIED., .F., .F.,
 ( 4, 4 ),
 ( 1.999999999897049408E-07, 0.006970199999999935128 ),
 .UNSPECIFIED. ) ;
#47329 = ADVANCED_FACE ( 'NONE', ( #29039 ), #35362, .F. ) ;
#47330 = LINE ( 'NONE', #2324, #51115 ) ;
#47331 = CARTESIAN_POINT ( 'NONE',  ( 0.4091458600556404646, -0.2362204724409448231, -1.599081364829396223 ) ) ;
#47332 = CARTESIAN_POINT ( 'NONE',  ( -0.6561679790026240244, -0.6046776061558807314, 0.2411417322834647770 ) ) ;
#47333 = CARTESIAN_POINT ( 'NONE',  ( -0.1640419947506555343, -0.2845877964562159024, 0.3641732283464567677 ) ) ;
#47334 = CARTESIAN_POINT ( 'NONE',  ( -1.417322834645668772, -0.1870078740157480879, -0.4822834645669291653 ) ) ;
#47335 = CARTESIAN_POINT ( 'NONE',  ( 0.3608923884514443348, -0.5511811023622046335, 0.09757992244046803654 ) ) ;
#47336 = CARTESIAN_POINT ( 'NONE',  ( -0.7545931758530177724, 0.1771653543307087630, 0.09757992244046791164 ) ) ;
#47337 = CARTESIAN_POINT ( 'NONE',  ( -0.9645669291338575535, -0.5400638737290844871, 0.3530559997133364547 ) ) ;
#47338 = CARTESIAN_POINT ( 'NONE',  ( 1.587926509186352142, -0.004921259842519576551, 0.3153832671262227771 ) ) ;
#47339 = CARTESIAN_POINT ( 'NONE',  ( 1.456692913385827515, -0.6692913385826771977, 8.415575281601705876E-17 ) ) ;
#47340 = CARTESIAN_POINT ( 'NONE',  ( 1.082677165354331228, 0.1012011053420775880, -0.2882089793578256898 ) ) ;
#47341 = CARTESIAN_POINT ( 'NONE',  ( 0.9776902887139113929, -0.5511811023622048555, -0.09757992244046775898 ) ) ;
#47342 = PRODUCT_DEFINITION_SHAPE ( 'NONE', 'NONE',  #83321 ) ;
#47343 = CARTESIAN_POINT ( 'NONE',  ( 0.2493438320209980519, 0.05413385826771666132, 0.4176697321401328100 ) ) ;
#47344 = CARTESIAN_POINT ( 'NONE',  ( 2.543486866223389153, 2.716535433070866645, -0.5314960629921260393 ) ) ;
#47345 = CARTESIAN_POINT ( 'NONE',  ( 1.581364829396326277, -0.08942795157527998196, 0.3641732283464567121 ) ) ;
#47346 = CIRCLE ( 'NONE', #60754, 3.937007874015748143 ) ;
#47347 = ORIENTED_EDGE ( 'NONE', *, *, #80947, .T. ) ;
#47348 = CARTESIAN_POINT ( 'NONE',  ( -0.3996062992125986590, 0.1070741851644051723, -2.786745406824146620 ) ) ;
#47349 = CARTESIAN_POINT ( 'NONE',  ( -1.135170603674539924, 0.1771653543307087075, -0.09757992244046823083 ) ) ;
#47350 = CARTESIAN_POINT ( 'NONE',  ( -0.3805774278215216522, 0.05413385826771666132, 0.4176697321401328100 ) ) ;
#47351 = CARTESIAN_POINT ( 'NONE',  ( 0.1115485564304467270, -0.6692913385826773087, -0.1292274648535924053 ) ) ;
#47352 = CARTESIAN_POINT ( 'NONE',  ( -1.522309711286088607, 0.1283753931104746893, -0.1820866141732285504 ) ) ;
#47353 = CARTESIAN_POINT ( 'NONE',  ( -0.2925321140481930149, -0.2925321140481933480, -1.868110236220472675 ) ) ;
#47354 = CARTESIAN_POINT ( 'NONE',  ( -1.423884514435694859, -0.3162353388693405765, 0.4822834645669290543 ) ) ;
#47355 = CARTESIAN_POINT ( 'NONE',  ( 0.3018372703412079971, 0.05413385826771626580, -0.4176697321401330321 ) ) ;
#47356 = CARTESIAN_POINT ( 'NONE',  ( -0.07217847769028787330, -0.05778040916215522460, 0.4822834645669289988 ) ) ;
#47357 = CARTESIAN_POINT ( 'NONE',  ( 1.200787401574803681, -0.5400638737290845981, -0.3530559997133363437 ) ) ;
#47358 = CARTESIAN_POINT ( 'NONE',  ( -0.3996062992125984925, -0.1070741851644056719, -0.9101049868766404316 ) ) ;
#47359 = CARTESIAN_POINT ( 'NONE',  ( 0.3996062992125986035, 2.446882876249141962E-17, -1.220472440944881942 ) ) ;
#47360 = CARTESIAN_POINT ( 'NONE',  ( 0.3949938075777409408, 0.1058382717557500574, -0.9120734908136481911 ) ) ;
#47361 = CARTESIAN_POINT ( 'NONE',  ( 0.1070741851644053527, 0.3996062992125986590, -2.670603674540682260 ) ) ;
#47362 = CARTESIAN_POINT ( 'NONE',  ( -0.2867679344610366554, 0.2867679344610365444, -0.1692913385826771144 ) ) ;
#47363 = CARTESIAN_POINT ( 'NONE',  ( -0.07217847769028813698, -0.2845877964562161244, -0.3641732283464567121 ) ) ;
#47364 = CARTESIAN_POINT ( 'NONE',  ( -0.3871391076115479057, -0.3162353388693409650, -0.4822834645669289433 ) ) ;
#47365 = CARTESIAN_POINT ( 'NONE',  ( 0.9711286089238851948, 0.2306618581243848609, 0.2411417322834645549 ) ) ;
#47366 = CARTESIAN_POINT ( 'NONE',  ( -0.3949938075777408852, -0.1058382717557502933, -1.697506561679790194 ) ) ;
#47367 = B_SPLINE_CURVE_WITH_KNOTS ( 'NONE', 3,
 ( #14534, #38926, #38513, #6111 ),
 .UNSPECIFIED., .F., .F.,
 ( 4, 4 ),
 ( 1.999999999927407068E-07, 0.006970199999999936863 ),
 .UNSPECIFIED. ) ;
#47368 = CARTESIAN_POINT ( 'NONE',  ( -0.04593175853018302557, 0.1771653543307087630, 0.09757992244046791164 ) ) ;
#47369 = CARTESIAN_POINT ( 'NONE',  ( -1.056430446194224881, -0.6692913385826771977, 0.1292274648535927661 ) ) ;
#47370 = CARTESIAN_POINT ( 'NONE',  ( -1.463254593175852492, 0.2952755905511811885, 0.1292274648535926551 ) ) ;
#47371 = CARTESIAN_POINT ( 'NONE',  ( -0.2362204724409451284, 0.4091458600556402425, -2.060367454068241511 ) ) ;
#47372 = CARTESIAN_POINT ( 'NONE',  ( 1.603475055217291612, 1.330568129716842130, -0.04573490813648244807 ) ) ;
#47373 = VERTEX_POINT ( 'NONE', #3790 ) ;
#47374 = VERTEX_POINT ( 'NONE', #49214 ) ;
#47375 = CARTESIAN_POINT ( 'NONE',  ( 1.115485564304462551, 0.05413385826771666132, 0.4176697321401328100 ) ) ;
#47376 = CARTESIAN_POINT ( 'NONE',  ( 1.515748031496063186, -0.4536011799217368745, -0.2665933059059886201 ) ) ;
#47378 = CARTESIAN_POINT ( 'NONE',  ( -1.108923884514435132, -0.05778040916215560624, -0.4822834645669293319 ) ) ;
#47377 = CARTESIAN_POINT ( 'NONE',  ( -1.095800524934382292, -0.2845877964562161244, -0.3641732283464567121 ) ) ;
#47379 = CARTESIAN_POINT ( 'NONE',  ( -0.1958661417322834497, -0.3392501089628018884, -2.350374385005562505 ) ) ;
#47380 = LINE ( 'NONE', #54105, #23543 ) ;
#47381 = CARTESIAN_POINT ( 'NONE',  ( 1.233595800524935227, 0.2306618581243847221, -0.2411417322834647770 ) ) ;
#47382 = CARTESIAN_POINT ( 'NONE',  ( -0.4724409448818898682, -8.678599364036362592E-17, -2.401574803149606474 ) ) ;
#47383 = CARTESIAN_POINT ( 'NONE',  ( -0.03937007874015669567, -0.6692913385826771977, 8.415575281601705876E-17 ) ) ;
#47384 = CARTESIAN_POINT ( 'NONE',  ( -0.1574803149606292529, -0.1870078740157479769, 0.4822834645669291653 ) ) ;
#47385 = CARTESIAN_POINT ( 'NONE',  ( -1.312335958005248715, 0.2306618581243848609, 0.2411417322834645549 ) ) ;
#47386 = CARTESIAN_POINT ( 'NONE',  ( 0.3917322834645668994, -0.1049643490035303134, -2.868747088417636704 ) ) ;
#47387 = CARTESIAN_POINT ( 'NONE',  ( 0.5708661417322841158, -0.5400638737290845981, -0.3530559997133363437 ) ) ;
#47388 = CARTESIAN_POINT ( 'NONE',  ( -0.1958661417322834220, -0.3392501089628018884, -1.947506561679789971 ) ) ;
#47389 = CARTESIAN_POINT ( 'NONE',  ( -1.161417322834644716, 0.07958543189024085140, 0.2665933059059887866 ) ) ;
#47390 = ORIENTED_EDGE ( 'NONE', *, *, #32695, .F. ) ;
#47391 = CARTESIAN_POINT ( 'NONE',  ( -0.3420746716998661618, 0.1974969037888702206, -2.230971128608923770 ) ) ;
#47392 = EDGE_LOOP ( 'NONE', ( #81478, #77506, #14381, #18499 ) ) ;
#47393 = CARTESIAN_POINT ( 'NONE',  ( -1.592472994958951560, 1.379238946755884987, 0.4472770027453138453 ) ) ;
#47394 = CARTESIAN_POINT ( 'NONE',  ( -1.574803149606298636, -0.1870078740157479769, 0.4822834645669291653 ) ) ;
#47395 = CARTESIAN_POINT ( 'NONE',  ( 1.417322834645670104, -0.1870078740157479769, 0.4822834645669291653 ) ) ;
#47396 = CARTESIAN_POINT ( 'NONE',  ( -0.3460692066303960868, 0.1998031496062990242, -0.4986876640419947715 ) ) ;
#47397 = CARTESIAN_POINT ( 'NONE',  ( -1.640419947506561060, -0.4281496062992127816, -0.4176697321401328100 ) ) ;
#47398 = CARTESIAN_POINT ( 'NONE',  ( -1.653543307086613234, -0.1870078740157480879, -0.4822834645669291653 ) ) ;
#47399 = CARTESIAN_POINT ( 'NONE',  ( 3.184294706754630777, 2.755905511811024056, -0.5314960629921260393 ) ) ;
#47401 = CARTESIAN_POINT ( 'NONE',  ( -0.3543307086614165824, 0.2952755905511811885, 0.000000000000000000 ) ) ;
#47400 = B_SPLINE_CURVE_WITH_KNOTS ( 'NONE', 3,
 ( #73843, #23303, #62025, #66698 ),
 .UNSPECIFIED., .F., .F.,
 ( 4, 4 ),
 ( 3.593986969204291827E-07, 0.001287825409103289694 ),
 .UNSPECIFIED. ) ;
#47402 = CARTESIAN_POINT ( 'NONE',  ( -0.1958661417322836718, 0.3392501089628017219, 0.05971128608923875758 ) ) ;
#47403 = VECTOR ( 'NONE', #12642, 39.37007874015748143 ) ;
#47404 = CARTESIAN_POINT ( 'NONE',  ( -0.3805774278215216522, -0.004921259842519576551, 0.3153832671262227771 ) ) ;
#47405 = CARTESIAN_POINT ( 'NONE',  ( -0.7283464566929126471, 0.07958543189024071263, -0.2665933059059888421 ) ) ;
#47406 = CARTESIAN_POINT ( 'NONE',  ( -1.043307086614172041, -0.5400638737290844871, 0.3530559997133364547 ) ) ;
#47407 = CARTESIAN_POINT ( 'NONE',  ( 0.9186351706036751663, -0.6046776061558807314, 0.2411417322834647770 ) ) ;
#47408 = CARTESIAN_POINT ( 'NONE',  ( -0.9776902887139098386, 0.2952755905511810774, -0.1292274648535930714 ) ) ;
#47409 = CARTESIAN_POINT ( 'NONE',  ( -0.3917322834645671215, 0.1049643490035301469, -0.02493438320209968861 ) ) ;
#47410 = ORIENTED_EDGE ( 'NONE', *, *, #39907, .T. ) ;
#47411 = CARTESIAN_POINT ( 'NONE',  ( -1.384514435695537005, -0.6692913385826773087, -0.1292274648535924053 ) ) ;
#47412 = CARTESIAN_POINT ( 'NONE',  ( -1.555118110236219930, 0.07958543189024085140, 0.2665933059059887866 ) ) ;
#47413 = CARTESIAN_POINT ( 'NONE',  ( 0.4724409448818897572, -0.1265901696524988906, -1.371391076115485053 ) ) ;
#47414 = DIRECTION ( 'NONE',  ( 0.000000000000000000, 0.000000000000000000, -1.000000000000000000 ) ) ;
#47415 = CARTESIAN_POINT ( 'NONE',  ( -0.3392501089628019995, 0.1958661417322832277, -0.6482939632545930975 ) ) ;
#47416 = CARTESIAN_POINT ( 'NONE',  ( -0.2867679344610364334, -0.2867679344610367109, -2.348425196850393970 ) ) ;
#47417 = CARTESIAN_POINT ( 'NONE',  ( -0.1837270341207340729, 0.2306618581243847221, -0.2411417322834647770 ) ) ;
#47418 = CARTESIAN_POINT ( 'NONE',  ( 1.469816272965879911, -0.6046776061558807314, 0.2411417322834647770 ) ) ;
#47419 = CARTESIAN_POINT ( 'NONE',  ( 0.2925321140481932369, -0.2925321140481931814, -0.01771653543307089712 ) ) ;
#47421 = CARTESIAN_POINT ( 'NONE',  ( -0.6496062992125976043, 0.1012011053420775880, -0.2882089793578256898 ) ) ;
#47420 = CARTESIAN_POINT ( 'NONE',  ( 0.4606732211678801203, 2.401574803149606030, -0.5309055118110237448 ) ) ;
#47422 = CARTESIAN_POINT ( 'NONE',  ( -1.286089238845143479, -0.6046776061558807314, 0.2411417322834647770 ) ) ;
#47423 = CARTESIAN_POINT ( 'NONE',  ( -0.2427821522309703550, -0.05778040916215560624, -0.4822834645669293319 ) ) ;
#47424 = CARTESIAN_POINT ( 'NONE',  ( -0.2867679344610364334, -0.2867679344610368219, 0.1758723341545424812 ) ) ;
#47425 = CARTESIAN_POINT ( 'NONE',  ( 0.4790026246719167324, -0.08942795157527998196, 0.3641732283464567121 ) ) ;
#47426 = DIRECTION ( 'NONE',  ( 1.000000000000000000, 1.601283208593976204E-15, 0.000000000000000000 ) ) ;
#47427 = CARTESIAN_POINT ( 'NONE',  ( 0.4986876640419954376, -0.5023911411419708095, -0.1820866141732282451 ) ) ;
#47428 = CARTESIAN_POINT ( 'NONE',  ( 0.7480314960629927956, -0.5511811023622047445, 6.969142054262312111E-17 ) ) ;
#47429 = CARTESIAN_POINT ( 'NONE',  ( 1.043307086614173818, -0.5400638737290845981, -0.3530559997133363437 ) ) ;
#47430 = CARTESIAN_POINT ( 'NONE',  ( -0.4658792650918627265, -0.2845877964562161244, -0.3641732283464567121 ) ) ;
#47431 = CARTESIAN_POINT ( 'NONE',  ( -0.1049643490035307020, 0.3917322834645669549, -1.730971128608923992 ) ) ;
#47432 = CARTESIAN_POINT ( 'NONE',  ( -1.371391076115484609, -0.6692913385826771977, 0.1292274648535927661 ) ) ;
#47433 = CARTESIAN_POINT ( 'NONE',  ( -0.1443569553805768291, -0.004921259842519576551, 0.3153832671262227771 ) ) ;
#47434 = CARTESIAN_POINT ( 'NONE',  ( -1.108923884514435132, -0.08942795157528024563, -0.3641732283464568787 ) ) ;
#47435 = CARTESIAN_POINT ( 'NONE',  ( -0.4091458600556405756, 0.2362204724409446288, -0.4179790026246719137 ) ) ;
#47436 = CARTESIAN_POINT ( 'NONE',  ( -0.7152230971128602510, -0.2845877964562159024, 0.3641732283464567677 ) ) ;
#47437 = CARTESIAN_POINT ( 'NONE',  ( -0.2493438320209966919, -0.4281496062992124485, 0.4176697321401328655 ) ) ;
#47438 = DIRECTION ( 'NONE',  ( 0.000000000000000000, 0.000000000000000000, -1.000000000000000000 ) ) ;
#47439 = CARTESIAN_POINT ( 'NONE',  ( 0.3477690288713918276, 0.1771653543307087630, 0.09757992244046791164 ) ) ;
#47440 = CARTESIAN_POINT ( 'NONE',  ( -0.2887139107611542133, 0.1283753931104748280, 0.1820866141732283561 ) ) ;
#47441 = CARTESIAN_POINT ( 'NONE',  ( -0.8792650918635160906, -0.4281496062992124485, 0.4176697321401328655 ) ) ;
#47442 = CARTESIAN_POINT ( 'NONE',  ( -1.601049868766403650, -0.6046776061558807314, 0.2411417322834647770 ) ) ;
#47443 = CARTESIAN_POINT ( 'NONE',  ( -0.9973753280839886548, 0.1283753931104748280, 0.1820866141732283561 ) ) ;
#47444 = DIRECTION ( 'NONE',  ( -0.000000000000000000, -1.000000000000000000, -0.000000000000000000 ) ) ;
#47445 = CARTESIAN_POINT ( 'NONE',  ( 0.3674540682414705883, -0.6046776061558807314, 0.2411417322834647770 ) ) ;
#47446 = CARTESIAN_POINT ( 'NONE',  ( -0.2925321140481930149, -0.2925321140481933480, -1.710629921259842812 ) ) ;
#47447 = CARTESIAN_POINT ( 'NONE',  ( 2.795275590551181466, 0.4724409448818907564, -3.234977217930338483E-16 ) ) ;
#47448 = CARTESIAN_POINT ( 'NONE',  ( -0.1574803149606292529, -0.1870078740157479769, 0.3641732283464567677 ) ) ;
#47449 = CARTESIAN_POINT ( 'NONE',  ( -0.09186351706036689768, 0.05413385826771626580, -0.4176697321401330321 ) ) ;
#47450 = CARTESIAN_POINT ( 'NONE',  ( -1.502624671916009680, -0.3162353388693405765, 0.4822834645669290543 ) ) ;
#47451 = CARTESIAN_POINT ( 'NONE',  ( -1.515748031496062076, -0.4536011799217367080, 0.2665933059059888421 ) ) ;
#47452 = CARTESIAN_POINT ( 'NONE',  ( 1.266404199475066328, -0.3162353388693409650, -0.4822834645669289433 ) ) ;
#47453 = B_SPLINE_CURVE_WITH_KNOTS ( 'NONE', 3,
 ( #22808, #23213, #3870, #67023, #3041, #22400, #48883, #28706, #29529, #10190, #16513, #60691, #42156, #60282, #16094, #36262, #54368, #17341, #81310, #21979, #35858, #55599, #53950, #67433, #3454, #23624, #79663, #9767, #74583, #29121, #42970, #61931, #80080, #74996, #47641, #68666, #49295, #67851 ),
 .UNSPECIFIED., .F., .F.,
 ( 4, 2, 2, 2, 2, 2, 2, 2, 2, 2, 2, 2, 2, 2, 2, 2, 2, 2, 4 ),
 ( 0.000000000000000000, 0.003207193274590009260, 0.004810789911885013891, 0.006414386549180018521, 0.007216184867827522137, 0.008017983186475025753, 0.009621579823770036455, 0.01042337814241754181, 0.01122517646106504716, 0.01282877309836005786, 0.01363057141700756147, 0.01443236973565506683, 0.01603596637295007926, 0.01763956301024508649, 0.01924315964754010067, 0.02084675628483511137, 0.02245035292213012207, 0.02405394955942513277, 0.02565754619672014347 ),
 .UNSPECIFIED. ) ;
#47454 = CARTESIAN_POINT ( 'NONE',  ( -0.8398950131233589023, -0.5023911411419708095, -0.1820866141732282451 ) ) ;
#47455 = CARTESIAN_POINT ( 'NONE',  ( 0.4581548273333326815, 1.539554514603150404, 0.5309055118110234117 ) ) ;
#47456 = CARTESIAN_POINT ( 'NONE',  ( -0.1070741851644051862, -0.3996062992125987146, -0.07217847769028871985 ) ) ;
#47457 = CARTESIAN_POINT ( 'NONE',  ( -0.3917322834645670104, -0.1049643490035307020, -2.404874958826459075 ) ) ;
#47458 = CARTESIAN_POINT ( 'NONE',  ( -3.890345922373659615, 2.716830163678111365, -0.5314960629921260393 ) ) ;
#47459 = EDGE_CURVE ( 'NONE', #53683, #35624, #36613, .T. ) ;
#47460 = CARTESIAN_POINT ( 'NONE',  ( 0.9448818897637802916, -0.1870078740157479769, 0.3641732283464567677 ) ) ;
#47461 = CARTESIAN_POINT ( 'NONE',  ( -0.4724409448818898682, 5.785732909357575061E-17, -2.755905511811024056 ) ) ;
#47462 = CARTESIAN_POINT ( 'NONE',  ( 0.8136482939632553313, 0.2306618581243848609, 0.2411417322834645549 ) ) ;
#47463 = CARTESIAN_POINT ( 'NONE',  ( 0.1958661417322834775, 0.3392501089628018884, -2.591207349081364519 ) ) ;
#47464 = CARTESIAN_POINT ( 'NONE',  ( 1.240157480314961314, 0.07958543189024071263, -0.2665933059059888421 ) ) ;
#47465 = EDGE_CURVE ( 'NONE', #16450, #78262, #42078, .T. ) ;
#47466 = CARTESIAN_POINT ( 'NONE',  ( 0.1509186351706045259, -0.05778040916215560624, -0.4822834645669293319 ) ) ;
#47467 = CARTESIAN_POINT ( 'NONE',  ( -0.5577427821522301654, -0.3162353388693405765, 0.4822834645669290543 ) ) ;
#47468 = CARTESIAN_POINT ( 'NONE',  ( 1.522309711286089939, 0.2306618581243848609, 0.2411417322834645549 ) ) ;
#47469 = CARTESIAN_POINT ( 'NONE',  ( -0.4724409448818899238, 0.1265901696524986686, -0.6627296587926508886 ) ) ;
#47470 = CARTESIAN_POINT ( 'NONE',  ( 0.1998031496062994405, -0.3460692066303958092, -1.981627296587926690 ) ) ;
#47471 = CARTESIAN_POINT ( 'NONE',  ( 0.2165354330708668673, 0.07958543189024071263, -0.2665933059059888421 ) ) ;
#47472 = ORIENTED_EDGE ( 'NONE', *, *, #32543, .F. ) ;
#47473 = CARTESIAN_POINT ( 'NONE',  ( 0.3917322834645670659, -0.1049643490035303273, -0.2657673472779021884 ) ) ;
#47474 = VERTEX_POINT ( 'NONE', #56355 ) ;
#47475 = CARTESIAN_POINT ( 'NONE',  ( -0.3215223097112853146, -0.3162353388693405765, 0.4822834645669290543 ) ) ;
#47476 = CARTESIAN_POINT ( 'NONE',  ( 1.200787401574803681, -0.5400638737290845981, -0.3530559997133363437 ) ) ;
#47477 = CARTESIAN_POINT ( 'NONE',  ( 0.1902887139107617975, -0.6692913385826773087, -0.1292274648535924053 ) ) ;
#47478 = CARTESIAN_POINT ( 'NONE',  ( -0.3412073490813641308, 0.1283753931104746893, -0.1820866141732285504 ) ) ;
#47479 = CARTESIAN_POINT ( 'NONE',  ( 0.6430446194225729606, -0.4281496062992127816, -0.4176697321401328100 ) ) ;
#47480 = CARTESIAN_POINT ( 'NONE',  ( -1.036745406824146176, -0.4281496062992124485, 0.4176697321401328655 ) ) ;
#47481 = CARTESIAN_POINT ( 'NONE',  ( -0.2624671916010490880, 0.2306618581243847221, -0.2411417322834647770 ) ) ;
#47482 = CARTESIAN_POINT ( 'NONE',  ( -0.9514435695538050464, -0.3162353388693405765, 0.4822834645669290543 ) ) ;
#47483 = CARTESIAN_POINT ( 'NONE',  ( 1.095800524934383846, -0.3162353388693405765, 0.4822834645669290543 ) ) ;
#47484 = CARTESIAN_POINT ( 'NONE',  ( 1.056430446194226436, -0.6692913385826773087, -0.1292274648535924053 ) ) ;
#47485 = CARTESIAN_POINT ( 'NONE',  ( 0.8202099737532814183, -0.6692913385826773087, -0.1292274648535924053 ) ) ;
#47486 = EDGE_CURVE ( 'NONE', #23063, #5054, #7628, .T. ) ;
#47487 = CARTESIAN_POINT ( 'NONE',  ( 0.3917322834645670104, -0.1049643490035303411, -0.5761154855643042527 ) ) ;
#47488 = CARTESIAN_POINT ( 'NONE',  ( -0.006561679790025524116, -0.08942795157528024563, -0.3641732283464568787 ) ) ;
#47489 = ORIENTED_EDGE ( 'NONE', *, *, #37822, .F. ) ;
#47490 = CARTESIAN_POINT ( 'NONE',  ( 0.2891555358219910499, -0.2891555358219909944, -1.200787401574803237 ) ) ;
#47491 = ORIENTED_EDGE ( 'NONE', *, *, #42958, .T. ) ;
#47492 = CARTESIAN_POINT ( 'NONE',  ( -0.7152230971128602510, -0.08942795157528024563, -0.3641732283464568787 ) ) ;
#47493 = CARTESIAN_POINT ( 'NONE',  ( 0.05905511811023709395, -0.5400638737290844871, 0.3530559997133364547 ) ) ;
#47494 = CARTESIAN_POINT ( 'NONE',  ( 2.873989802184792719, 1.063020117359137817, -0.01785754392581748520 ) ) ;
#47495 = CARTESIAN_POINT ( 'NONE',  ( -0.4396325459317579898, 0.2952755905511811885, 0.1292274648535926551 ) ) ;
#47496 = CARTESIAN_POINT ( 'NONE',  ( -0.5905511811023615998, 0.2952755905511811885, 0.000000000000000000 ) ) ;
#47497 = CARTESIAN_POINT ( 'NONE',  ( -1.207349081364828436, -0.6046776061558807314, 0.2411417322834647770 ) ) ;
#47498 = CARTESIAN_POINT ( 'NONE',  ( -1.443569553805773564, -0.6046776061558807314, 0.2411417322834647770 ) ) ;
#47499 = CARTESIAN_POINT ( 'NONE',  ( 1.305774278215223960, -0.5511811023622046335, 0.09757992244046803654 ) ) ;
#47500 = CARTESIAN_POINT ( 'NONE',  ( 0.4724409448818898127, -0.1265901696524988629, -1.056430446194225770 ) ) ;
#47501 = CARTESIAN_POINT ( 'NONE',  ( 0.2896775404227472372, 0.05826908593210169962, 5.534257978450463966 ) ) ;
#47502 = CARTESIAN_POINT ( 'NONE',  ( 0.4199475065616803948, -0.5023911411419708095, -0.1820866141732282451 ) ) ;
#47503 = AXIS2_PLACEMENT_3D ( 'NONE', #68168, #16832, #10511 ) ;
#47504 = CARTESIAN_POINT ( 'NONE',  ( 0.2034120734908144990, -0.6692913385826771977, 0.1292274648535927661 ) ) ;
#47505 = CARTESIAN_POINT ( 'NONE',  ( 0.2821522309711292364, 0.2952755905511810774, -0.1292274648535930714 ) ) ;
#47506 = ORIENTED_EDGE ( 'NONE', *, *, #12502, .T. ) ;
#47507 = CARTESIAN_POINT ( 'NONE',  ( -0.3996062992125986035, -7.340648628747425578E-17, -1.614173228346456712 ) ) ;
#47508 = CARTESIAN_POINT ( 'NONE',  ( 0.000000000000000000, 2.755905511811024056, 0.000000000000000000 ) ) ;
#47509 = ORIENTED_EDGE ( 'NONE', *, *, #19828, .T. ) ;
#47510 = CARTESIAN_POINT ( 'NONE',  ( 0.3996062992125984925, 0.1070741851644054637, -1.303805774278215202 ) ) ;
#47511 = CARTESIAN_POINT ( 'NONE',  ( -0.1998031496062994405, 0.3460692066303957537, -0.5623359580052492701 ) ) ;
#47512 = CARTESIAN_POINT ( 'NONE',  ( -0.4068241469816267775, 0.05413385826771626580, -0.4176697321401330321 ) ) ;
#47513 = CARTESIAN_POINT ( 'NONE',  ( 0.4724409448818896462, 0.1265901696524990294, 0.03280839895013123314 ) ) ;
#47514 = CARTESIAN_POINT ( 'NONE',  ( -0.3392501089628019995, 0.1958661417322832277, -2.473097112860892288 ) ) ;
#47515 = CARTESIAN_POINT ( 'NONE',  ( -1.522309711286088607, -0.5023911411419708095, 0.1820866141732285504 ) ) ;
#47516 = CARTESIAN_POINT ( 'NONE',  ( 0.8070866141732288002, 0.1660481256975885056, 0.3530559997133364547 ) ) ;
#47517 = CARTESIAN_POINT ( 'NONE',  ( 0.7349081364829403995, 0.2306618581243848609, 0.2411417322834645549 ) ) ;
#47518 = CARTESIAN_POINT ( 'NONE',  ( -0.1049868766404193215, -0.5023911411419708095, 0.1820866141732285504 ) ) ;
#47519 = CARTESIAN_POINT ( 'NONE',  ( -0.1246719160104980823, 0.2952755905511811885, 0.1292274648535926551 ) ) ;
#47520 = CARTESIAN_POINT ( 'NONE',  ( -0.4724409448818899238, 0.1265901696524986686, -1.841863517060367439 ) ) ;
#47521 = CARTESIAN_POINT ( 'NONE',  ( -0.09186351706036663400, -0.3690944881889763329, 0.3153832671262228327 ) ) ;
#47522 = CARTESIAN_POINT ( 'NONE',  ( -0.5446194225721777693, -0.3162353388693409650, -0.4822834645669289433 ) ) ;
#47523 = AXIS2_PLACEMENT_3D ( 'NONE', #35295, #4129, #80754 ) ;
#47524 = CARTESIAN_POINT ( 'NONE',  ( -0.1974969037888704149, -0.3420746716998661063, -1.717191601049868677 ) ) ;
#47525 = CARTESIAN_POINT ( 'NONE',  ( -1.482939632545930975, -0.4281496062992127816, -0.4176697321401328100 ) ) ;
#47526 = CARTESIAN_POINT ( 'NONE',  ( 0.1312335958005255154, -0.5023911411419708095, 0.1820866141732285504 ) ) ;
#47527 = CARTESIAN_POINT ( 'NONE',  ( 1.548556430446194954, 0.1283753931104746893, -0.1820866141732285504 ) ) ;
#47528 = CARTESIAN_POINT ( 'NONE',  ( -1.200787401574802349, 0.1660481256975883668, -0.3530559997133364547 ) ) ;
#47529 = CARTESIAN_POINT ( 'NONE',  ( -0.6889763779527552368, 0.07958543189024085140, 0.2665933059059887866 ) ) ;
#47530 = CARTESIAN_POINT ( 'NONE',  ( 0.000000000000000000, 2.716535433070866645, 0.000000000000000000 ) ) ;
#47531 = CARTESIAN_POINT ( 'NONE',  ( -1.345144356955379816, -0.05778040916215560624, -0.4822834645669293319 ) ) ;
#47532 = CARTESIAN_POINT ( 'NONE',  ( -0.6561679790026240244, 0.2306618581243847221, -0.2411417322834647770 ) ) ;
#47533 = CARTESIAN_POINT ( 'NONE',  ( 0.1115485564304470323, 0.2952755905511811885, 0.1292274648535926551 ) ) ;
#47534 = CARTESIAN_POINT ( 'NONE',  ( 0.2925321140481932369, 0.2925321140481932369, -2.419291338582676865 ) ) ;
#47535 = CARTESIAN_POINT ( 'NONE',  ( -9.594673741351310580E-17, 0.3917322834645669549, -2.284757587105299859 ) ) ;
#47536 = CARTESIAN_POINT ( 'NONE',  ( 0.5314960629920856272, 2.753838553078471918, 3.842312626974355716 ) ) ;
#47537 = CARTESIAN_POINT ( 'NONE',  ( 0.4461942257217856311, 0.1283753931104746893, -0.1820866141732285504 ) ) ;
#47538 = EDGE_CURVE ( 'NONE', #76587, #42095, #29681, .T. ) ;
#47539 = CARTESIAN_POINT ( 'NONE',  ( 0.9055118110236227702, -0.6692913385826771977, 8.415575281601705876E-17 ) ) ;
#47540 = CARTESIAN_POINT ( 'NONE',  ( -1.069553805774277722, 0.1771653543307087630, 0.09757992244046791164 ) ) ;
#47541 = CARTESIAN_POINT ( 'NONE',  ( 1.227034120734908917, 0.2952755905511810774, -0.1292274648535930714 ) ) ;
#47542 = CARTESIAN_POINT ( 'NONE',  ( -1.384514435695537005, 0.1771653543307087630, 0.09757992244046791164 ) ) ;
#47543 = CARTESIAN_POINT ( 'NONE',  ( -0.3280839895013117347, -0.4281496062992124485, 0.4176697321401328655 ) ) ;
#47544 = CARTESIAN_POINT ( 'NONE',  ( 0.1181102362204730916, 0.1771653543307087630, 0.000000000000000000 ) ) ;
#47545 = DIRECTION ( 'NONE',  ( 0.000000000000000000, 1.000000000000000000, 0.000000000000000000 ) ) ;
#47546 = CARTESIAN_POINT ( 'NONE',  ( 0.5511811023622054106, -0.1870078740157480601, -0.3641732283464567677 ) ) ;
#47547 = EDGE_CURVE ( 'NONE', #18898, #69738, #7151, .T. ) ;
#47548 = CARTESIAN_POINT ( 'NONE',  ( -0.2165354330708654795, 0.1660481256975885056, 0.3530559997133364547 ) ) ;
#47549 = CARTESIAN_POINT ( 'NONE',  ( 0.1998031496062994128, -0.3460692066303957537, -0.4835958005249343938 ) ) ;
#47550 = CARTESIAN_POINT ( 'NONE',  ( -0.6430446194225716283, -0.4281496062992124485, 0.4176697321401328655 ) ) ;
#47551 = CARTESIAN_POINT ( 'NONE',  ( 0.1958661417322834775, 0.3392501089628018884, -1.646325459317585338 ) ) ;
#47552 = CARTESIAN_POINT ( 'NONE',  ( 1.003937007874016185, 0.07958543189024071263, -0.2665933059059888421 ) ) ;
#47553 = CARTESIAN_POINT ( 'NONE',  ( 0.2559055118110243332, 0.1660481256975885056, 0.3530559997133364547 ) ) ;
#47554 = CARTESIAN_POINT ( 'NONE',  ( -0.1968503937007867743, 0.2952755905511811885, 0.000000000000000000 ) ) ;
#47555 = CARTESIAN_POINT ( 'NONE',  ( -0.1968503937007867743, 0.1771653543307087630, 0.000000000000000000 ) ) ;
#47556 = CARTESIAN_POINT ( 'NONE',  ( -0.6167979002624665030, -0.3690944881889765550, -0.3153832671262227771 ) ) ;
#47557 = CARTESIAN_POINT ( 'NONE',  ( 0.4133858267716541968, 0.1660481256975885056, 0.3530559997133364547 ) ) ;
#47558 = CARTESIAN_POINT ( 'NONE',  ( -0.7217847769028863381, -0.004921259842519870586, -0.3153832671262229437 ) ) ;
#47559 = CARTESIAN_POINT ( 'NONE',  ( -0.1998031496062991630, -0.3460692066303959202, -0.7723097112860892732 ) ) ;
#47560 = CARTESIAN_POINT ( 'NONE',  ( -1.279527559055116948, 0.1660481256975883668, -0.3530559997133364547 ) ) ;
#47561 = DIRECTION ( 'NONE',  ( -0.000000000000000000, 1.000000000000000000, -0.000000000000000000 ) ) ;
#47562 = ORIENTED_EDGE ( 'NONE', *, *, #21129, .T. ) ;
#47563 = AXIS2_PLACEMENT_3D ( 'NONE', #4855, #62104, #43553 ) ;
#47564 = CARTESIAN_POINT ( 'NONE',  ( -1.036745406824146176, -0.004921259842519870586, -0.3153832671262229437 ) ) ;
#47565 = CARTESIAN_POINT ( 'NONE',  ( -0.3740157480314953431, -0.5400638737290845981, -0.3530559997133363437 ) ) ;
#47566 = CARTESIAN_POINT ( 'NONE',  ( 0.3981765293560903807, 0.002049465651542591027, -1.220472440944881720 ) ) ;
#47567 = CARTESIAN_POINT ( 'NONE',  ( -0.5971128608923877978, -0.6692913385826773087, -0.1292274648535924053 ) ) ;
#47568 = PLANE ( 'NONE',  #8215 ) ;
#47569 = CARTESIAN_POINT ( 'NONE',  ( 1.220472440944882608, 0.2952755905511811885, 0.000000000000000000 ) ) ;
#47570 = CARTESIAN_POINT ( 'NONE',  ( 1.023622047244095334, -0.1870078740157479769, 0.4822834645669291653 ) ) ;
#47571 = LINE ( 'NONE', #80427, #39533 ) ;
#47572 = CARTESIAN_POINT ( 'NONE',  ( -39.19291338582677753, 5.691349986800547090E-15, 0.000000000000000000 ) ) ;
#47573 = CARTESIAN_POINT ( 'NONE',  ( 0.2952755905511810219, -0.005994596871347899689, 5.524802951929911110 ) ) ;
#47574 = CARTESIAN_POINT ( 'NONE',  ( -1.699475065616797398, 0.2952755905511811885, 0.1292274648535926551 ) ) ;
#47575 = CARTESIAN_POINT ( 'NONE',  ( -0.1070741851644056997, 0.3996062992125986035, -0.4790026246719158998 ) ) ;
#47576 = EDGE_LOOP ( 'NONE', ( #16246, #60013, #51948, #37659 ) ) ;
#47577 = CARTESIAN_POINT ( 'NONE',  ( -0.5971128608923877978, -0.5511811023622048555, -0.09757992244046775898 ) ) ;
#47579 = CARTESIAN_POINT ( 'NONE',  ( 0.1049643490035304938, -0.3917322834645669549, -2.282152230971128404 ) ) ;
#47578 = AXIS2_PLACEMENT_3D ( 'NONE', #11298, #17619, #55471 ) ;
#47580 = ORIENTED_EDGE ( 'NONE', *, *, #1832, .T. ) ;
#47581 = CARTESIAN_POINT ( 'NONE',  ( 0.7545931758530188826, -0.6692913385826771977, 0.1292274648535927661 ) ) ;
#47582 = CARTESIAN_POINT ( 'NONE',  ( 0.05249343832021075018, 0.2306618581243847221, -0.2411417322834647770 ) ) ;
#47583 = CARTESIAN_POINT ( 'NONE',  ( -0.6430446194225712953, 0.05413385826771626580, -0.4176697321401330321 ) ) ;
#47584 = CARTESIAN_POINT ( 'NONE',  ( 1.423884514435696413, -0.3162353388693409650, -0.4822834645669289433 ) ) ;
#47585 = CARTESIAN_POINT ( 'NONE',  ( -1.430446194225720724, -0.004921259842519870586, -0.3153832671262229437 ) ) ;
#47586 = CARTESIAN_POINT ( 'NONE',  ( -3.886287458032462006, 2.165354330708662012, -0.6299212598425202314 ) ) ;
#47587 = CARTESIAN_POINT ( 'NONE',  ( 0.4002624671916016896, -0.05778040916215522460, 0.4822834645669289988 ) ) ;
#47588 = CARTESIAN_POINT ( 'NONE',  ( 0.6167979002624678353, -0.3690944881889763329, 0.3153832671262228327 ) ) ;
#47589 = CARTESIAN_POINT ( 'NONE',  ( -0.6430446194225712953, 0.05413385826771626580, -0.4176697321401330321 ) ) ;
#47590 = CARTESIAN_POINT ( 'NONE',  ( -0.1958661417322834497, -0.3392501089628018884, -1.720453125163043051 ) ) ;
#47591 = CARTESIAN_POINT ( 'NONE',  ( -1.259842519685038686, -0.1870078740157480879, -0.4822834645669291653 ) ) ;
#47592 = DIRECTION ( 'NONE',  ( 0.000000000000000000, 0.000000000000000000, -1.000000000000000000 ) ) ;
#47593 = CARTESIAN_POINT ( 'NONE',  ( 0.8792650918635177559, 0.05413385826771666132, 0.4176697321401328100 ) ) ;
#47594 = CARTESIAN_POINT ( 'NONE',  ( 1.423884514435696413, -0.2845877964562161244, -0.3641732283464567121 ) ) ;
#47595 = ORIENTED_EDGE ( 'NONE', *, *, #24051, .F. ) ;
#47596 = CARTESIAN_POINT ( 'NONE',  ( 0.3392501089628018884, -0.1958661417322833942, -2.936371021818584115 ) ) ;
#47597 = CARTESIAN_POINT ( 'NONE',  ( -0.4593175853018364174, -0.4281496062992127816, -0.4176697321401328100 ) ) ;
#47598 = ORIENTED_EDGE ( 'NONE', *, *, #28057, .F. ) ;
#47599 = CARTESIAN_POINT ( 'NONE',  ( 0.5183727034120741983, 0.1771653543307087075, -0.09757992244046823083 ) ) ;
#47600 = CARTESIAN_POINT ( 'NONE',  ( -1.069553805774277722, 0.2952755905511811885, 0.1292274648535926551 ) ) ;
#47601 = CARTESIAN_POINT ( 'NONE',  ( 0.8727034120734912248, -0.3162353388693409650, -0.4822834645669289433 ) ) ;
#47602 = CARTESIAN_POINT ( 'NONE',  ( 0.9580052493438326877, 0.05413385826771666132, 0.4176697321401328100 ) ) ;
#47603 = CARTESIAN_POINT ( 'NONE',  ( -0.1377952755905504645, 0.1660481256975885056, 0.3530559997133364547 ) ) ;
#47604 = CARTESIAN_POINT ( 'NONE',  ( -0.5118110236220466680, 0.2952755905511811885, 0.000000000000000000 ) ) ;
#47605 = CARTESIAN_POINT ( 'NONE',  ( -0.3917322834645671215, 0.1049643490035301469, -2.164698162729658648 ) ) ;
#47606 = CARTESIAN_POINT ( 'NONE',  ( 1.528871391076116026, -0.5511811023622048555, -0.09757992244046775898 ) ) ;
#47607 = CARTESIAN_POINT ( 'NONE',  ( -0.4265091863517051496, -0.6692913385826771977, 0.1292274648535927661 ) ) ;
#47608 = CARTESIAN_POINT ( 'NONE',  ( -0.3674540682414689785, 0.1283753931104748280, 0.1820866141732283561 ) ) ;
#47609 = CARTESIAN_POINT ( 'NONE',  ( 1.227034120734908917, 0.2952755905511810774, -0.1292274648535930714 ) ) ;
#47610 = CARTESIAN_POINT ( 'NONE',  ( -0.9973753280839886548, -0.6046776061558809534, -0.2411417322834644161 ) ) ;
#47611 = CARTESIAN_POINT ( 'NONE',  ( -0.3996062992125986590, 0.1070741851644051723, 0.04790026246719158304 ) ) ;
#47612 = CARTESIAN_POINT ( 'NONE',  ( 0.7152230971128614723, -0.3162353388693409650, -0.4822834645669289433 ) ) ;
#47613 = CARTESIAN_POINT ( 'NONE',  ( 4.893765752498283924E-17, -0.3996062992125986035, -1.968503937007873850 ) ) ;
#47614 = CARTESIAN_POINT ( 'NONE',  ( 3.913952425448613770, 1.327060745706139411, 0.4255134223640585911 ) ) ;
#47615 =( BOUNDED_CURVE ( )  B_SPLINE_CURVE ( 2, ( #13085, #78734, #38738, #32422, #58084, #450, #26105, #51767, #19806, #77469, #71153, #13494, #64835 ),
 .UNSPECIFIED., .F., .F. ) 
 B_SPLINE_CURVE_WITH_KNOTS ( ( 3, 2, 2, 2, 2, 2, 3 ),
 ( 0.7875000000000000888, 0.7916666666666667407, 0.7958333333333333925, 0.8000000000000000444, 0.8041666666666666963, 0.8083333333333333481, 0.8125000000000000000 ),
 .UNSPECIFIED. ) 
 CURVE ( )  GEOMETRIC_REPRESENTATION_ITEM ( )  RATIONAL_B_SPLINE_CURVE ( ( 0.9999999999999991118, 0.9659258262890692004, 1.000000000000000000, 0.9659258262890683122, 1.000000000000000000, 0.9659258262890683122, 1.000000000000000000, 0.9659258262890683122, 1.000000000000000000, 0.9659258262890683122, 1.000000000000000000, 0.9659258262890683122, 1.000000000000000000 ) ) 
 REPRESENTATION_ITEM ( '' )  );
#47616 = CARTESIAN_POINT ( 'NONE',  ( -0.3149606299212590610, -0.1870078740157480879, -0.4822834645669291653 ) ) ;
#47617 = CARTESIAN_POINT ( 'NONE',  ( -1.003937007874014853, 0.07958543189024085140, 0.2665933059059887866 ) ) ;
#47618 = CARTESIAN_POINT ( 'NONE',  ( 1.148293963254593875, -0.5511811023622046335, 0.09757992244046803654 ) ) ;
#47619 = CARTESIAN_POINT ( 'NONE',  ( 0.1265901696524989462, 0.4724409448818897572, -0.8576115485564304031 ) ) ;
#47620 = CARTESIAN_POINT ( 'NONE',  ( 1.292650918635171564, -0.5511811023622048555, -0.09757992244046775898 ) ) ;
#47621 = ADVANCED_FACE ( 'NONE', ( #37004 ), #69412, .F. ) ;
#47622 = CARTESIAN_POINT ( 'NONE',  ( 0.7611548556430451917, -0.6046776061558807314, 0.2411417322834647770 ) ) ;
#47623 = CARTESIAN_POINT ( 'NONE',  ( 0.2891555358219910499, 0.2891555358219910499, -0.3720472440944882497 ) ) ;
#47624 = CARTESIAN_POINT ( 'NONE',  ( -0.3674540682414692561, -0.6046776061558809534, -0.2411417322834644161 ) ) ;
#47625 = FACE_OUTER_BOUND ( 'NONE', #78751, .T. ) ;
#47626 = AXIS2_PLACEMENT_3D ( 'NONE', #65753, #77958, #33341 ) ;
#47627 = CARTESIAN_POINT ( 'NONE',  ( 1.528871391076116026, -0.5511811023622048555, -0.09757992244046775898 ) ) ;
#47628 = CARTESIAN_POINT ( 'NONE',  ( -0.7414698162729651543, 0.2952755905511810774, -0.1292274648535930714 ) ) ;
#47629 = EDGE_CURVE ( 'NONE', #53888, #42092, #15539, .T. ) ;
#47630 = CARTESIAN_POINT ( 'NONE',  ( -0.1058382717557497660, -0.3949938075777411073, -0.6213910761154856077 ) ) ;
#47631 = CARTESIAN_POINT ( 'NONE',  ( 1.318897637795276356, -0.5400638737290844871, 0.3530559997133364547 ) ) ;
#47632 = CARTESIAN_POINT ( 'NONE',  ( 0.09842519685039434474, -0.5400638737290845981, -0.3530559997133363437 ) ) ;
#47633 = CARTESIAN_POINT ( 'NONE',  ( 0.4133858267716541968, 0.07958543189024085140, 0.2665933059059887866 ) ) ;
#47634 = CARTESIAN_POINT ( 'NONE',  ( -0.07848924910222174200, 1.069269829744720290, -1.119403926637735358 ) ) ;
#47635 = CARTESIAN_POINT ( 'NONE',  ( 0.4199475065616805614, 0.1283753931104748280, 0.1820866141732283561 ) ) ;
#47636 = CARTESIAN_POINT ( 'NONE',  ( 3.937007874015748143, 2.165354330708661568, -0.3149606299212595606 ) ) ;
#47637 = CARTESIAN_POINT ( 'NONE',  ( -0.1070741851644056997, 0.3996062992125984925, -1.343175853018372834 ) ) ;
#47638 = CARTESIAN_POINT ( 'NONE',  ( 0.5774278215223104249, 0.2306618581243848609, 0.2411417322834645549 ) ) ;
#47639 = CARTESIAN_POINT ( 'NONE',  ( 0.3917322834645670104, 2.398668435337828261E-17, -1.055118110236220375 ) ) ;
#47640 = CARTESIAN_POINT ( 'NONE',  ( 1.417322834645670104, -0.1870078740157480601, -0.3641732283464567677 ) ) ;
#47641 = CARTESIAN_POINT ( 'NONE',  ( -0.1716039559346191345, -0.3527845929029423400, -1.489137855930806014E-17 ) ) ;
#47642 = CARTESIAN_POINT ( 'NONE',  ( -0.1509186351706028884, -0.08942795157527998196, 0.3641732283464567121 ) ) ;
#47643 = CIRCLE ( 'NONE', #67853, 0.5118110236220472231 ) ;
#47644 = CARTESIAN_POINT ( 'NONE',  ( 0.3083989501312343062, -0.05778040916215560624, -0.4822834645669293319 ) ) ;
#47645 = CARTESIAN_POINT ( 'NONE',  ( 1.351706036745407680, -0.004921259842519576551, 0.3153832671262227771 ) ) ;
#47646 = CARTESIAN_POINT ( 'NONE',  ( -1.528871391076114250, 0.1771653543307087075, -0.09757992244046823083 ) ) ;
#47647 = CARTESIAN_POINT ( 'NONE',  ( -1.509186351706035767, 0.05413385826771626580, -0.4176697321401330321 ) ) ;
#47648 = CARTESIAN_POINT ( 'NONE',  ( 0.6299212598425204535, -0.1870078740157480879, -0.4822834645669291653 ) ) ;
#47649 = CARTESIAN_POINT ( 'NONE',  ( 1.673228346456693494, 0.1660481256975885056, 0.3530559997133364547 ) ) ;
#47650 = CARTESIAN_POINT ( 'NONE',  ( 1.614173228346457378, 1.330640075373405118, -0.1372047244094476148 ) ) ;
#47651 = CARTESIAN_POINT ( 'NONE',  ( 0.4330708661417329575, -0.6692913385826771977, 8.415575281601705876E-17 ) ) ;
#47652 = CARTESIAN_POINT ( 'NONE',  ( 1.174540682414699111, -0.3162353388693405765, 0.4822834645669290543 ) ) ;
#47653 = CARTESIAN_POINT ( 'NONE',  ( 1.049868766404200349, 0.2306618581243848609, 0.2411417322834645549 ) ) ;
#47654 = DIRECTION ( 'NONE',  ( 0.000000000000000000, 0.000000000000000000, 1.000000000000000000 ) ) ;
#47655 = CARTESIAN_POINT ( 'NONE',  ( 1.154855643044620184, -0.5023911411419708095, 0.1820866141732285504 ) ) ;
#47656 = CARTESIAN_POINT ( 'NONE',  ( -1.653543307086613234, -0.1870078740157479769, 0.3641732283464567677 ) ) ;
#47657 = CARTESIAN_POINT ( 'NONE',  ( -0.9317585301837263412, -0.3690944881889765550, -0.3153832671262227771 ) ) ;
#47658 = CARTESIAN_POINT ( 'NONE',  ( 0.4091458600556403535, 0.2362204724409449896, -2.020997375328084100 ) ) ;
#47659 = CARTESIAN_POINT ( 'NONE',  ( 0.5971128608923890191, -0.5511811023622046335, 0.09757992244046803654 ) ) ;
#47660 = CARTESIAN_POINT ( 'NONE',  ( 0.01312335958005323398, -0.4281496062992127816, -0.4176697321401328100 ) ) ;
#47661 = CARTESIAN_POINT ( 'NONE',  ( 0.7939632545931766261, -0.05778040916215522460, 0.4822834645669289988 ) ) ;
#47662 = CARTESIAN_POINT ( 'NONE',  ( -0.4790026246719152336, -0.05778040916215560624, -0.4822834645669293319 ) ) ;
#47663 = CARTESIAN_POINT ( 'NONE',  ( 0.1443569553805781891, -0.3690944881889763329, 0.3153832671262228327 ) ) ;
#47664 = CARTESIAN_POINT ( 'NONE',  ( 1.351706036745407458, -0.4281496062992127816, -0.4176697321401328100 ) ) ;
#47665 = CARTESIAN_POINT ( 'NONE',  ( -1.573327616418469521, 1.128537896298102305, 0.2406134192599649613 ) ) ;
#47666 = CARTESIAN_POINT ( 'NONE',  ( -1.017060367454067249, -0.3162353388693409650, -0.4822834645669289433 ) ) ;
#47668 = CARTESIAN_POINT ( 'NONE',  ( -0.3460692066303958092, -0.1998031496062994683, -0.8398950131233595684 ) ) ;
#47667 = DIRECTION ( 'NONE',  ( 0.000000000000000000, -1.000000000000000000, 0.000000000000000000 ) ) ;
#47669 = CARTESIAN_POINT ( 'NONE',  ( -0.1938976377952756625, -0.1938976377952756625, -0.3740157480314971750 ) ) ;
#47670 = CARTESIAN_POINT ( 'NONE',  ( -0.7217847769028863381, -0.4281496062992124485, 0.4176697321401328655 ) ) ;
#47671 = CARTESIAN_POINT ( 'NONE',  ( -0.4330708661417315697, 0.2952755905511811885, 0.000000000000000000 ) ) ;
#47672 = CARTESIAN_POINT ( 'NONE',  ( 5.785732909357575061E-17, -0.4724409448818898682, 0.07874015748031495954 ) ) ;
#47673 = CARTESIAN_POINT ( 'NONE',  ( -0.2891555358219908833, -0.2891555358219912164, -2.421259842519685623 ) ) ;
#47674 = ORIENTED_EDGE ( 'NONE', *, *, #51210, .F. ) ;
#47675 = CARTESIAN_POINT ( 'NONE',  ( 0.8136482939632553313, -0.5023911411419708095, -0.1820866141732282451 ) ) ;
#47676 = CARTESIAN_POINT ( 'NONE',  ( 0.3392501089628018329, 0.1958661417322835607, -1.068241469816272771 ) ) ;
#47677 = CARTESIAN_POINT ( 'NONE',  ( 1.292650918635171564, 0.2952755905511811885, 0.1292274648535926551 ) ) ;
#47678 = DIRECTION ( 'NONE',  ( -1.000000000000000000, -0.000000000000000000, -0.000000000000000000 ) ) ;
#47679 = CARTESIAN_POINT ( 'NONE',  ( -1.561679790026246017, -0.004921259842519576551, 0.3153832671262227771 ) ) ;
#47680 = DIRECTION ( 'NONE',  ( -3.096699300667737957E-16, 1.000000000000000000, -0.000000000000000000 ) ) ;
#47681 = CARTESIAN_POINT ( 'NONE',  ( -1.706036745406823485, 0.2306618581243848609, 0.2411417322834645549 ) ) ;
#47682 = CARTESIAN_POINT ( 'NONE',  ( -9.594673741351310580E-17, 0.3917322834645669549, -0.2375134926171111049 ) ) ;
#47683 = CARTESIAN_POINT ( 'NONE',  ( -0.09842519685039295696, -0.5400638737290844871, 0.3530559997133364547 ) ) ;
#47684 = CARTESIAN_POINT ( 'NONE',  ( -0.6561679790026240244, -0.5023911411419708095, 0.1820866141732285504 ) ) ;
#47685 = CARTESIAN_POINT ( 'NONE',  ( 0.9120734908136489683, -0.6692913385826771977, 0.1292274648535927661 ) ) ;
#47686 = CARTESIAN_POINT ( 'NONE',  ( 0.1181102362204730916, -0.6692913385826771977, 8.415575281601705876E-17 ) ) ;
#47687 =( BOUNDED_SURFACE ( )  B_SPLINE_SURFACE ( 3, 2, ( 
 ( #40276, #9950, #79018, #65959, #22165, #53717, #35623, #54550, #14622, #22581, #28060, #33963, #21744, #48242, #41109, #22989, #41927, #60046, #54968, #59625, #48654, #61286, #73525, #1980, #21337, #46989, #2402, #3638, #79424, #47409, #15450, #66797, #9132, #2813, #34803, #67207, #73938, #67620, #29715, #75177, #56206, #74765, #62117, #30125, #68850, #81907, #17521, #4869, #30542, #49067, #81083, #36444, #4460, #16695, #24219, #74351, #68033, #49484, #43154, #55789, #23400, #42335, #10378, #11198, #36035, #42749, #61709, #36857, #62531, #17114, #10784, #4049, #55377, #81495, #68444, #23811, #59068, #51480, #40546, #25820, #66227, #70874, #45168, #26242, #14479, #51902, #38871, #27079, #27495, #72121, #65403, #14057, #77183, #71703, #32978, #71285, #64550, #78027, #19515, #57800, #26666, #167, #53152, #13223, #6887, #39712, #13633, #78864, #52740, #32144, #40132, #45592, #32557, #39285, #46429, #58645, #14886, #33816, #58220, #46844, #586, #72538, #21190, #7740, #77609, #19942, #64972, #7308, #1013, #52321, #20356, #46007, #33406, #1423, #78449, #20775, #65818, #8151, #59482, #1835, #54824, #23249, #73371, #80115, #16128, #42191, #48918, #80528, #3904, #29564, #22016, #28326, #54403, #22433, #2248, #74619, #16963, #27914, #9802, #29155, #28742, #60318, #80933, #42602, #61137, #10224, #2667, #35891, #48092, #35473, #47259, #53987, #73792, #3489, #72949, #8565, #15300, #53573, #41774, #67467, #34234, #66644, #8981, #74200, #79700, #22840, #34654, #16546, #47676, #79282, #48499, #67886, #15720, #61561, #55226, #41376, #59896, #67057, #21597, #35060, #9390, #40962, #60726, #3077, #24888, #37118, #5953, #55636, #75441, #50557, #11876, #4308, #81345, #17780, #10640, #31208, #36701, #11042, #30387, #69526, #23660, #56053, #75847, #49330, #18996, #82981, #37528, #63203, #5543, #11460, #62375, #50966, #81762, #5136, #56876, #18595, #30801, #24072, #57284, #4713, #49741, #43822, #36295, #29972, #68701, #76260, #56466, #82569, #44238, #75032, #43414, #69112, #69927, #62802, #12283, #18189, #24484, #25300, #82168, #50151, #17377, #37939, #63616, #76663, #31622, #43007, #68304, #61969, #77082, #77926, #78767, #40038, #13118, #913, #26570, #7641, #52223, #45065, #45489, #14380, #58547, #32455, #6370, #38770, #32042, #33311, #51800, #58117, #13956, #57701, #20257, #25717, #26978, #484, #19840, #70768, #33718, #7208, #8057, #63, #1329, #20679, #46331, #59380, #58973, #65724, #64447, #6783, #26139, #1738, #52643, #12696, #27395, #77505, #78347, #51377, #45906, #71186, #13528, #38355, #72024, #53055, #71603, #39184, #44645, #64868, #19414, #32878, #39613, #70342, #65302, #64030, #73695, #67374, #74103, #34967, #8877, #66128, #15201, #8465, #9708, #28228, #34553, #16035, #34135, #28646, #2150, #3394, #60219, #79601, #47161, #10127, #66964, #67791, #59796, #61044, #80433, #22743, #35792, #35379, #16449, #72853, #21503, #2569, #61459, #29057, #72443, #42094, #53887, #54728, #27817, #54306, #21917, #47579, #14792, #48403, #3807, #22335, #15621, #29469, #73272, #53477, #40861, #79187, #55127, #80017, #21091, #41681, #46750, #40449, #66544, #41278, #9297, #47996, #60630, #2981, #4616, #23150, #43725, #49232, #23561, #42908, #82071, #36199, #68603, #5040, #10542, #31527, #12185, #24384, #75750, #18091, #23976, #74935, #63520, #10943, #17683, #50055, #31108, #43313, #36600, #69835, #17280, #62278, #56372, #48819, #42503, #81246, #63109, #69011, #69429, #11782, #4210, #30287, #55953, #37435, #81666, #5447, #30709, #37020, #37842, #11363, #49644, #61869, #56775, #75336, #5850, #18500, #68205, #82475, #24791, #29874, #50459, #80837, #76163, #62701, #44143, #74519, #16866, #55536, #57603, #58017, #70660, #46229, #83293, #25616, #32775, #82885, #18899, #51279, #39509, #19734, #20156, #804, #63930 ),
 ( #12594, #25205, #39085, #13016, #52538, #52118, #57183, #13851, #38670, #50871, #64348, #71503, #382, #39937, #58871, #76982, #71926, #76571, #14275, #20578, #13429, #44549, #70239, #65623, #19311, #7954, #38253, #44964, #32356, #6266, #31942, #45389, #6685, #26038, #77826, #65198, #51698, #45806, #77400, #71086, #64766, #7105, #7534, #58444, #33206, #78246, #26467, #1229, #26878, #79494, #21809, #27294, #16347, #74000, #52952, #34867, #54197, #53782, #2047, #22643, #48303, #2878, #35274, #27711, #60938, #47473, #60528, #72343, #53377, #73165, #28540, #14691, #41990, #40347, #78667, #41173, #66864, #67685, #8363, #34030, #15935, #79085, #15516, #59691, #41582, #21403, #20987, #9194, #79913, #47057, #22230, #47885, #72749, #73592, #15097, #67272, #60117, #40754, #9605, #59279, #3288, #66438, #46649, #8775, #28953, #2468, #33616, #54618, #34448, #1635, #66026, #28127, #80329, #49543, #29368, #61351, #25832, #29776, #57812, #55028, #55437, #68504, #23050, #35686, #55850, #23461, #80736, #4939, #24283, #61770, #56272, #51491, #74833, #81559, #17582, #44758, #77194, #81968, #6486, #32156, #49128, #81146, #23878, #75238, #3705, #19526, #45180, #48717, #11262, #30608, #30187, #4110, #179, #10020, #62597, #12812, #17177, #38467, #43214, #36920, #74415, #42810, #68910, #49954, #16760, #42399, #68097, #10443, #75652, #17992, #36099, #10844, #36504, #70454, #62180, #64152, #4518, #53166, #64987, #64563, #20787, #72134, #71299, #33828, #8163, #45605, #1435, #26679, #27509, #14071, #1026, #14492, #13234, #59494, #78879, #39724, #79294, #6900, #21612, #26256, #600, #7322, #21202, #32991, #77622, #65830, #66239, #46857, #46443, #52754, #32571, #27091, #71716, #52334, #72551, #58660, #14898, #59080, #65417, #38884, #8576, #51915, #58233, #78462, #78040, #34247, #1848, #70885, #40558, #59909, #40145, #7753, #2262, #20370, #19955, #13647, #39300, #27927, #53585, #46022, #33418, #10239, #68318, #34669, #54418, #29580, #74217, #66658, #60332, #80129, #72962, #35909, #15735, #73384, #9404, #48517, #2680, #35074, #54839, #28340, #81362, #61986, #16562, #42207, #67902, #73807, #41390, #29989, #60740, #67482, #61576, #80950, #9817, #3092, #36310, #67072, #28756, #22856, #15313, #8996, #47690, #55243, #35488, #3919, #23265, #54001, #22448, #48109, #48934, #16144, #74635, #80544, #3504, #16978, #4323, #41791, #61152, #42619, #29171, #55652, #10655, #79713, #47272, #40976, #22029, #56892, #57718, #19013, #75458, #63220, #5560, #69944, #31224, #24088, #24501, #76680, #37545, #11478, #68717, #17796, #11059, #12299, #30816, #37134, #76279, #36717, #82585, #4730, #5970, #62819, #82184, #49758, #12712, #69543, #70357, #62393, #63632, #82997, #25318, #38371, #37955, #44661, #43431, #69128, #5152, #64047, #31639, #75046, #6387, #56481, #57299, #30404, #24904, #50167, #75863, #17392, #50982, #18205, #32058, #43841, #11892, #50573, #49347, #23675, #43023, #18611, #56071, #81778, #44254, #38788, #13137, #77523, #65741, #19858, #6802, #78365, #78784, #40054, #33328, #65320, #19431, #39630, #930, #39203, #59397, #45507, #8074, #71621, #77944, #25734, #21109, #64465, #51395, #7658, #64886, #46768, #20696, #81, #33737, #13547, #77099, #7225, #14398, #26587, #66146, #1755, #504, #14809, #45082, #40468, #72460, #58990, #70786, #32473, #8483, #71204, #34152, #58135, #32897, #58564, #26157, #51818, #45923, #52240, #20273, #46347, #27412, #13973, #72042, #1346, #26996, #52659, #53073, #10145, #16883, #22759, #55144, #80855, #73290, #79619, #22352, #48012, #53495, #42521, #68224, #79204, #61060, #80449, #80033, #28245, #48836, #74537, #29073, #61476, #53905, #3824, #73711, #3411, #15219, #21936, #16051, #54744, #40879, #10558, #66561, #21520, #67390, #9724, #59813, #34571, #60238, #42111, #47596, #41697, #2586 ),
 ( #48421, #23167, #16466, #35395, #74120, #47179, #67808, #60647, #15638, #35810, #41295, #29485, #2168, #54324, #27834, #72871, #8894, #66980, #9313, #34983, #2997, #28663, #36216, #76178, #49661, #29890, #43327, #50474, #62717, #18915, #37859, #36617, #50886, #55553, #76586, #82900, #75765, #81262, #4226, #44565, #55969, #25220, #23577, #81682, #11378, #49248, #61885, #82086, #75351, #74951, #31124, #18515, #4632, #82491, #70256, #17699, #24400, #43740, #69850, #17297, #24807, #31542, #57198, #69027, #23993, #50070, #18107, #42924, #68619, #10959, #62295, #37450, #56791, #56387, #30303, #37035, #5055, #5462, #63535, #30725, #5866, #69445, #63124, #11797, #44158, #12201, #39524, #51296, #1652, #76999, #57620, #20170, #45820, #27309, #70678, #13034, #78261, #32371, #52134, #38687, #20592, #6702, #6283, #71519, #13865, #64365, #58885, #33222, #58035, #26483, #51715, #52552, #39101, #26056, #65212, #38269, #1244, #46244, #64783, #21003, #31959, #46665, #19330, #25633, #398, #77416, #52968, #78652, #78682, #59295, #77841, #44982, #63946, #12611, #19752, #45406, #71102, #13445, #7121, #32792, #58461, #821, #7549, #26893, #71940, #14289, #39953, #65639, #7969, #33632, #60544, #79931, #22658, #29383, #35291, #67700, #10036, #2484, #8791, #34883, #2895, #66042, #55043, #80750, #8380, #73609, #9620, #9210, #40770, #61367, #3719, #41597, #74014, #66455, #16361, #28559, #15951, #27727, #34464, #54215, #67287, #53394, #23064, #79101, #34045, #22246, #47901, #72359, #47074, #72765, #54632, #60133, #60953, #15116, #80345, #28143, #59708, #3303, #28968, #53799, #48317, #42006, #79511, #35700, #21827, #14707, #15532, #47490, #40362, #2063, #21420, #73182, #41190, #66880, #42414, #57098, #4125, #61785, #42825, #31023, #68518, #55451, #43640, #44059, #5362, #81984, #30622, #68111, #4952, #49559, #4532, #24708, #10859, #56691, #36934, #43229, #74429, #69751, #29790, #16776, #56287, #30202, #12097, #69343, #48732, #82390, #62195, #10459, #55864, #63024, #75253, #31435, #50376, #36519, #11275, #62612, #36113, #82793, #5766, #81160, #49968, #11694, #68926, #17192, #37755, #63430, #18006, #76074, #81574, #18416, #24298, #75666, #23476, #23893, #37351, #49143, #74848, #17597, #63841, #70153, #32685, #58352, #14186, #83207, #25529, #7441, #44872, #64678, #51194, #33112, #19222, #18815, #713, #26372, #76892, #71416, #45719, #70571, #38995, #64263, #65104, #51607, #38584, #52030, #50787, #13763, #58780, #77312, #33530, #44462, #59193, #6179, #38167, #12925, #1140, #6597, #31854, #20067, #20488, #26790, #77736, #7017, #12506, #39420, #25949, #32269, #52447, #57929, #78157, #13341, #19642, #76488, #46142, #57516, #293, #71837, #45302, #39844, #65533, #25115, #7866, #70998, #78579, #8694, #15858, #28042, #67604, #3210, #1963, #16265, #20905, #41910, #48227, #41092, #46558, #52869, #9935, #21319, #73923, #72256, #46972, #60030, #14605, #27206, #47391, #15015, #40259, #79832, #41507, #53288, #47807, #35607, #66356, #73082, #9115, #35195, #1552, #73510, #80250, #22566, #40671, #60856, #78999, #67192, #15432, #79409, #65942, #8278, #33944, #59608, #66781, #34364, #27625, #22149, #72666, #9523, #2385, #53700, #21728, #28872, #34787, #60446, #54534, #2798, #28457, #54117, #75982, #24617, #17507, #80660, #29290, #18323, #81067, #50284, #22972, #23383, #36429, #74333, #3623, #23796, #74749, #48639, #56191, #75575, #29699, #24204, #43964, #42733, #49468, #68836, #11598, #69660, #49875, #56598, #82298, #17098, #49051, #75162, #43139, #54953, #12004, #61269, #16680, #62515, #81893, #81479, #55362, #42319, #68018, #30528, #62934, #68429, #5267, #11182, #4853, #10362, #10769, #36843, #17915, #36022, #61694, #4034, #62102, #43551, #69252, #4445, #30110, #55772, #37258, #30931, #77214, #38070, #19972, #31759, #31339 ),
 ( #26274, #77640, #6504, #46040, #57005, #71734, #76391, #50694, #57421, #45623, #83115, #44366, #32590, #33007, #71317, #70903, #19543, #82701, #45201, #38487, #76796, #13666, #13253, #38902, #25020, #64582, #64171, #19127, #39318, #25433, #65003, #25850, #32175, #63336, #58677, #18724, #5672, #6919, #44776, #1042, #58253, #37658, #7339, #51099, #70058, #70473, #51935, #57830, #20388, #26696, #63746, #52351, #12412, #78058, #6085, #618, #12830, #198, #51510, #33845, #61901, #59097, #59511, #72567, #27109, #39741, #59926, #27527, #1452, #10160, #29500, #65846, #61492, #29905, #78897, #2282, #21630, #48852, #55569, #3840, #10574, #36231, #53182, #1865, #27944, #53602, #7770, #81277, #23593, #33437, #15331, #35826, #34266, #8179, #4242, #49264, #66676, #16898, #21218, #42537, #79311, #40996, #52772, #46873, #47290, #55160, #78480, #14089, #20804, #46460, #72979, #80870, #65437, #72154, #14509, #23182, #14914, #74553, #40162, #68239, #40574, #66255, #8594, #76192, #75367, #37874, #12217, #49676, #5478, #30739, #31555, #18122, #5070, #18529, #17312, #63548, #57212, #43754, #23531, #68635, #25648, #30318, #4647, #69044, #82914, #11393, #81697, #69865, #70271, #69460, #50899, #17714, #31973, #12625, #36634, #50489, #18930, #24008, #24821, #74966, #38284, #43342, #31139, #56806, #5882, #82505, #37050, #75780, #44578, #44172, #62732, #62310, #56402, #55986, #25234, #82101, #24414, #76599, #50084, #63960, #11810, #6297, #37465, #63138, #57633, #42940, #10974, #14723, #64379, #7984, #27324, #52984, #40376, #39968, #46681, #19766, #51729, #7135, #66059, #33648, #19345, #72374, #39115, #1667, #58048, #58900, #32808, #77855, #44995, #59311, #78697, #52568, #45835, #21020, #64796, #38700, #77431, #414, #8395, #26908, #34062, #20608, #14308, #59725, #6715, #58475, #2080, #78276, #70694, #32385, #839, #77013, #65655, #45419, #71115, #13458, #46260, #26070, #26497, #1260, #52149, #51310, #13047, #71955, #20184, #71533, #13881, #39540, #65228, #7566, #33238, #28984, #61386, #73625, #41208, #16793, #53815, #79529, #3320, #53410, #72781, #28160, #10053, #15967, #74030, #54651, #34483, #21843, #73199, #16377, #47507, #80361, #60969, #67303, #67717, #42430, #2912, #68130, #15549, #66896, #22674, #79118, #15131, #9226, #35716, #41614, #42023, #48333, #60149, #34899, #60561, #3735, #28575, #29399, #55058, #9638, #80766, #10475, #54232, #79949, #23081, #22262, #36128, #48748, #40787, #74447, #61801, #2501, #27745, #21436, #47091, #47920, #35307, #66472, #8807, #82002, #36536, #68944, #76092, #56305, #81594, #23494, #30220, #49160, #63042, #17615, #23911, #69361, #74866, #49986, #17209, #56709, #49576, #43246, #62212, #12115, #4974, #69771, #42842, #31041, #24727, #50395, #37773, #5380, #18436, #4550, #55883, #75272, #63448, #82408, #55467, #44078, #11294, #5784, #68535, #24316, #36953, #62630, #81177, #31454, #4141, #43659, #30640, #29806, #75684, #18025, #11715, #37371, #10875, #54922, #61663, #48607, #42289, #17068, #66750, #3176, #4004, #22940, #15400, #9085, #28841, #21698, #67986, #47777, #22117, #41476, #80629, #34756, #67161, #3593, #60416, #30079, #10741, #74302, #16648, #10331, #22533, #73478, #62073, #9490, #16231, #35993, #29669, #41878, #35164, #42705, #41061, #55330, #23351, #28426, #29258, #79379, #74719, #15828, #35576, #61239, #81039, #49023, #79801, #80217, #68402, #9904, #60825, #2767, #54503, #54086, #36398, #48195, #73891, #4411, #67572, #47361, #73050, #38041, #69218, #30901, #81863, #44747, #18291, #19098, #68804, #12383, #31728, #57392, #70442, #44339, #51068, #24175, #56160, #11566, #12800, #63716, #23767, #76768, #43518, #6057, #62485, #63306, #37225, #82269, #49438, #83083, #25405, #56975, #50254, #38455, #62902, #43108, #49844, #4819, #64141, #31311, #6474, #24989, #18697 ) ),
 .UNSPECIFIED., .F., .F., .F. ) 
 B_SPLINE_SURFACE_WITH_KNOTS ( ( 4, 4 ),
 ( 3, 2, 2, 2, 2, 2, 2, 2, 2, 2, 2, 2, 2, 2, 2, 2, 2, 2, 2, 2, 2, 2, 2, 2, 2, 2, 2, 2, 2, 2, 2, 2, 2, 2, 2, 2, 2, 2, 2, 2, 2, 2, 2, 2, 2, 2, 2, 2, 2, 2, 2, 2, 2, 2, 2, 2, 2, 2, 2, 2, 2, 2, 2, 2, 2, 2, 2, 2, 2, 2, 2, 2, 2, 2, 2, 2, 2, 2, 2, 2, 2, 2, 2, 2, 2, 2, 2, 2, 2, 2, 2, 2, 2, 2, 2, 2, 2, 2, 2, 2, 2, 2, 2, 2, 2, 2, 2, 2, 2, 2, 2, 2, 2, 2, 2, 2, 2, 2, 2, 2, 2, 2, 2, 2, 2, 2, 2, 2, 2, 2, 2, 2, 2, 2, 2, 2, 2, 2, 2, 2, 2, 2, 2, 2, 2, 2, 2, 2, 2, 2, 2, 2, 2, 2, 2, 2, 2, 2, 2, 2, 2, 2, 2, 2, 2, 2, 2, 2, 2, 2, 2, 2, 2, 2, 2, 2, 2, 2, 2, 2, 2, 2, 2, 2, 2, 2, 2, 2, 2, 2, 2, 2, 2, 2, 2, 2, 2, 2, 2, 2, 2, 2, 2, 2, 2, 2, 2, 2, 2, 2, 2, 2, 2, 2, 2, 2, 2, 2, 2, 2, 2, 2, 2, 2, 2, 2, 2, 2, 2, 2, 2, 2, 2, 2, 2, 2, 2, 3 ),
 ( 0.000000000000000000, 1.000000000000000000 ),
 ( 0.000000000000000000, 0.004166666666666666609, 0.008333333333333333218, 0.01250000000000000069, 0.01666666666666666644, 0.02083333333333333218, 0.02500000000000000139, 0.02916666666666666713, 0.03333333333333333287, 0.03749999999999999861, 0.04166666666666666435, 0.04583333333333333010, 0.05000000000000000278, 0.05416666666666666852, 0.05833333333333333426, 0.06250000000000000000, 0.06666666666666666574, 0.07083333333333333148, 0.07499999999999999722, 0.07916666666666666297, 0.08333333333333332871, 0.08749999999999999445, 0.09166666666666666019, 0.09583333333333333981, 0.1000000000000000056, 0.1041666666666666713, 0.1083333333333333370, 0.1125000000000000028, 0.1166666666666666685, 0.1208333333333333343, 0.1250000000000000000, 0.1291666666666666796, 0.1333333333333333315, 0.1375000000000000111, 0.1416666666666666630, 0.1458333333333333426, 0.1499999999999999944, 0.1541666666666666741, 0.1583333333333333259, 0.1625000000000000056, 0.1666666666666666574, 0.1708333333333333370, 0.1749999999999999889, 0.1791666666666666685, 0.1833333333333333204, 0.1875000000000000000, 0.1916666666666666796, 0.1958333333333333315, 0.2000000000000000111, 0.2041666666666666630, 0.2083333333333333426, 0.2124999999999999944, 0.2166666666666666741, 0.2208333333333333259, 0.2250000000000000056, 0.2291666666666666574, 0.2333333333333333370, 0.2374999999999999889, 0.2416666666666666685, 0.2458333333333333204, 0.2500000000000000000, 0.2541666666666666519, 0.2583333333333333592, 0.2625000000000000111, 0.2666666666666666630, 0.2708333333333333148, 0.2750000000000000222, 0.2791666666666666741, 0.2833333333333333259, 0.2874999999999999778, 0.2916666666666666852, 0.2958333333333333370, 0.2999999999999999889, 0.3041666666666666408, 0.3083333333333333481, 0.3125000000000000000, 0.3166666666666666519, 0.3208333333333333592, 0.3250000000000000111, 0.3291666666666666630, 0.3333333333333333148, 0.3375000000000000222, 0.3416666666666666741, 0.3458333333333333259, 0.3499999999999999778, 0.3541666666666666852, 0.3583333333333333370, 0.3624999999999999889, 0.3666666666666666408, 0.3708333333333333481, 0.3750000000000000000, 0.3791666666666666519, 0.3833333333333333592, 0.3875000000000000111, 0.3916666666666666630, 0.3958333333333333148, 0.4000000000000000222, 0.4041666666666666741, 0.4083333333333333259, 0.4124999999999999778, 0.4166666666666666852, 0.4208333333333333370, 0.4249999999999999889, 0.4291666666666666408, 0.4333333333333333481, 0.4375000000000000000, 0.4416666666666666519, 0.4458333333333333592, 0.4500000000000000111, 0.4541666666666666630, 0.4583333333333333148, 0.4625000000000000222, 0.4666666666666666741, 0.4708333333333333259, 0.4749999999999999778, 0.4791666666666666852, 0.4833333333333333370, 0.4874999999999999889, 0.4916666666666666408, 0.4958333333333333481, 0.5000000000000000000, 0.5041666666666666519, 0.5083333333333333037, 0.5124999999999999556, 0.5166666666666667185, 0.5208333333333333703, 0.5250000000000000222, 0.5291666666666666741, 0.5333333333333333259, 0.5374999999999999778, 0.5416666666666666297, 0.5458333333333332815, 0.5500000000000000444, 0.5541666666666666963, 0.5583333333333333481, 0.5625000000000000000, 0.5666666666666666519, 0.5708333333333333037, 0.5749999999999999556, 0.5791666666666667185, 0.5833333333333333703, 0.5875000000000000222, 0.5916666666666666741, 0.5958333333333333259, 0.5999999999999999778, 0.6041666666666666297, 0.6083333333333332815, 0.6125000000000000444, 0.6166666666666666963, 0.6208333333333333481, 0.6250000000000000000, 0.6291666666666666519, 0.6333333333333333037, 0.6374999999999999556, 0.6416666666666667185, 0.6458333333333333703, 0.6500000000000000222, 0.6541666666666666741, 0.6583333333333333259, 0.6624999999999999778, 0.6666666666666666297, 0.6708333333333332815, 0.6750000000000000444, 0.6791666666666666963, 0.6833333333333333481, 0.6875000000000000000, 0.6916666666666666519, 0.6958333333333333037, 0.6999999999999999556, 0.7041666666666667185, 0.7083333333333333703, 0.7125000000000000222, 0.7166666666666666741, 0.7208333333333333259, 0.7249999999999999778, 0.7291666666666666297, 0.7333333333333332815, 0.7375000000000000444, 0.7416666666666666963, 0.7458333333333333481, 0.7500000000000000000, 0.7541666666666666519, 0.7583333333333333037, 0.7624999999999999556, 0.7666666666666667185, 0.7708333333333333703, 0.7750000000000000222, 0.7791666666666666741, 0.7833333333333333259, 0.7874999999999999778, 0.7916666666666666297, 0.7958333333333332815, 0.8000000000000000444, 0.8041666666666666963, 0.8083333333333333481, 0.8125000000000000000, 0.8166666666666666519, 0.8208333333333333037, 0.8249999999999999556, 0.8291666666666667185, 0.8333333333333333703, 0.8375000000000000222, 0.8416666666666666741, 0.8458333333333333259, 0.8499999999999999778, 0.8541666666666666297, 0.8583333333333332815, 0.8625000000000000444, 0.8666666666666666963, 0.8708333333333333481, 0.8750000000000000000, 0.8791666666666666519, 0.8833333333333333037, 0.8874999999999999556, 0.8916666666666667185, 0.8958333333333333703, 0.9000000000000000222, 0.9041666666666666741, 0.9083333333333333259, 0.9124999999999999778, 0.9166666666666666297, 0.9208333333333332815, 0.9250000000000000444, 0.9291666666666666963, 0.9333333333333333481, 0.9375000000000000000, 0.9416666666666666519, 0.9458333333333333037, 0.9499999999999999556, 0.9541666666666667185, 0.9583333333333333703, 0.9625000000000000222, 0.9666666666666666741, 0.9708333333333333259, 0.9749999999999999778, 0.9791666666666666297, 0.9833333333333332815, 0.9875000000000000444 ),
 .UNSPECIFIED. ) 
 GEOMETRIC_REPRESENTATION_ITEM ( )  RATIONAL_B_SPLINE_SURFACE ( (
 ( 1.000000000000000000, 0.9659258262890683122, 1.000000000000000000, 0.9659258262890683122, 1.000000000000000000, 0.9659258262890683122, 1.000000000000000000, 0.9659258262890683122, 1.000000000000000000, 0.9659258262890683122, 1.000000000000000000, 0.9659258262890683122, 1.000000000000000000, 0.9659258262890683122, 1.000000000000000000, 0.9659258262890683122, 1.000000000000000000, 0.9659258262890683122, 1.000000000000000000, 0.9659258262890683122, 1.000000000000000000, 0.9659258262890683122, 1.000000000000000000, 0.9659258262890683122, 1.000000000000000000, 0.9659258262890683122, 1.000000000000000000, 0.9659258262890683122, 1.000000000000000000, 0.9659258262890683122, 1.000000000000000000, 0.9659258262890683122, 1.000000000000000000, 0.9659258262890683122, 1.000000000000000000, 0.9659258262890683122, 1.000000000000000000, 0.9659258262890683122, 1.000000000000000000, 0.9659258262890683122, 1.000000000000000000, 0.9659258262890683122, 1.000000000000000000, 0.9659258262890683122, 1.000000000000000000, 0.9659258262890683122, 1.000000000000000000, 0.9659258262890683122, 1.000000000000000000, 0.9659258262890683122, 1.000000000000000000, 0.9659258262890683122, 1.000000000000000000, 0.9659258262890683122, 1.000000000000000000, 0.9659258262890683122, 1.000000000000000000, 0.9659258262890683122, 1.000000000000000000, 0.9659258262890683122, 1.000000000000000000, 0.9659258262890683122, 1.000000000000000000, 0.9659258262890683122, 1.000000000000000000, 0.9659258262890683122, 1.000000000000000000, 0.9659258262890683122, 1.000000000000000000, 0.9659258262890683122, 1.000000000000000000, 0.9659258262890683122, 1.000000000000000000, 0.9659258262890683122, 1.000000000000000000, 0.9659258262890683122, 1.000000000000000000, 0.9659258262890683122, 1.000000000000000000, 0.9659258262890683122, 1.000000000000000000, 0.9659258262890683122, 1.000000000000000000, 0.9659258262890683122, 1.000000000000000000, 0.9659258262890683122, 1.000000000000000000, 0.9659258262890683122, 1.000000000000000000, 0.9659258262890683122, 1.000000000000000000, 0.9659258262890683122, 1.000000000000000000, 0.9659258262890683122, 1.000000000000000000, 0.9659258262890683122, 1.000000000000000000, 0.9659258262890683122, 1.000000000000000000, 0.9659258262890683122, 1.000000000000000000, 0.9659258262890683122, 1.000000000000000000, 0.9659258262890683122, 1.000000000000000000, 0.9659258262890683122, 1.000000000000000000, 0.9659258262890683122, 1.000000000000000000, 0.9659258262890683122, 1.000000000000000000, 0.9659258262890683122, 1.000000000000000000, 0.9659258262890683122, 1.000000000000000000, 0.9659258262890683122, 1.000000000000000000, 0.9659258262890683122, 1.000000000000000000, 0.9659258262890683122, 1.000000000000000000, 0.9659258262890683122, 1.000000000000000000, 0.9659258262890683122, 1.000000000000000000, 0.9659258262890683122, 1.000000000000000000, 0.9659258262890683122, 1.000000000000000000, 0.9659258262890683122, 1.000000000000000000, 0.9659258262890683122, 1.000000000000000000, 0.9659258262890683122, 1.000000000000000000, 0.9659258262890683122, 1.000000000000000000, 0.9659258262890683122, 1.000000000000000000, 0.9659258262890683122, 1.000000000000000000, 0.9659258262890683122, 1.000000000000000000, 0.9659258262890683122, 1.000000000000000000, 0.9659258262890683122, 1.000000000000000000, 0.9659258262890683122, 1.000000000000000000, 0.9659258262890683122, 1.000000000000000000, 0.9659258262890683122, 1.000000000000000000, 0.9659258262890683122, 1.000000000000000000, 0.9659258262890683122, 1.000000000000000000, 0.9659258262890683122, 1.000000000000000000, 0.9659258262890683122, 1.000000000000000000, 0.9659258262890683122, 1.000000000000000000, 0.9659258262890683122, 1.000000000000000000, 0.9659258262890683122, 1.000000000000000000, 0.9659258262890683122, 1.000000000000000000, 0.9659258262890683122, 1.000000000000000000, 0.9659258262890683122, 1.000000000000000000, 0.9659258262890683122, 1.000000000000000000, 0.9659258262890683122, 1.000000000000000000, 0.9659258262890683122, 1.000000000000000000, 0.9659258262890683122, 1.000000000000000000, 0.9659258262890683122, 1.000000000000000000, 0.9659258262890683122, 1.000000000000000000, 0.9659258262890683122, 1.000000000000000000, 0.9659258262890683122, 1.000000000000000000, 0.9659258262890683122, 1.000000000000000000, 0.9659258262890683122, 1.000000000000000000, 0.9659258262890683122, 1.000000000000000000, 0.9659258262890683122, 1.000000000000000000, 0.9659258262890683122, 1.000000000000000000, 0.9659258262890683122, 1.000000000000000000, 0.9659258262890683122, 1.000000000000000000, 0.9659258262890683122, 1.000000000000000000, 0.9659258262890683122, 1.000000000000000000, 0.9659258262890683122, 1.000000000000000000, 0.9659258262890683122, 1.000000000000000000, 0.9659258262890683122, 1.000000000000000000, 0.9659258262890683122, 1.000000000000000000, 0.9659258262890683122, 1.000000000000000000, 0.9659258262890683122, 1.000000000000000000, 0.9659258262890683122, 1.000000000000000000, 0.9659258262890683122, 1.000000000000000000, 0.9659258262890683122, 1.000000000000000000, 0.9659258262890683122, 1.000000000000000000, 0.9659258262890683122, 1.000000000000000000, 0.9659258262890683122, 1.000000000000000000, 0.9659258262890683122, 1.000000000000000000, 0.9659258262890683122, 1.000000000000000000, 0.9659258262890683122, 1.000000000000000000, 0.9659258262890683122, 1.000000000000000000, 0.9659258262890683122, 1.000000000000000000, 0.9659258262890683122, 1.000000000000000000, 0.9659258262890683122, 1.000000000000000000, 0.9659258262890683122, 1.000000000000000000, 0.9659258262890683122, 1.000000000000000000, 0.9659258262890683122, 1.000000000000000000, 0.9659258262890683122, 1.000000000000000000, 0.9659258262890683122, 1.000000000000000000, 0.9659258262890683122, 1.000000000000000000, 0.9659258262890683122, 1.000000000000000000, 0.9659258262890683122, 1.000000000000000000, 0.9659258262890683122, 1.000000000000000000, 0.9659258262890683122, 1.000000000000000000, 0.9659258262890683122, 1.000000000000000000, 0.9659258262890683122, 1.000000000000000000, 0.9659258262890683122, 1.000000000000000000, 0.9659258262890683122, 1.000000000000000000, 0.9659258262890683122, 1.000000000000000000, 0.9659258262890683122, 1.000000000000000000, 0.9659258262890683122, 1.000000000000000000, 0.9659258262890683122, 1.000000000000000000, 0.9659258262890683122, 1.000000000000000000, 0.9659258262890683122, 1.000000000000000000, 0.9659258262890683122, 1.000000000000000000, 0.9659258262890683122, 1.000000000000000000, 0.9659258262890683122, 1.000000000000000000, 0.9659258262890683122, 1.000000000000000000, 0.9659258262890683122, 1.000000000000000000, 0.9659258262890683122, 1.000000000000000000, 0.9659258262890683122, 1.000000000000000000, 0.9659258262890683122, 1.000000000000000000, 0.9659258262890683122, 1.000000000000000000, 0.9659258262890683122, 1.000000000000000000, 0.9659258262890683122, 1.000000000000000000, 0.9659258262890683122, 1.000000000000000000, 0.9659258262890683122, 1.000000000000000000, 0.9659258262890683122, 1.000000000000000000, 0.9659258262890683122, 1.000000000000000000, 0.9659258262890683122, 1.000000000000000000, 0.9659258262890683122, 1.000000000000000000, 0.9659258262890683122, 1.000000000000000000, 0.9659258262890683122, 1.000000000000000000, 0.9659258262890683122, 1.000000000000000000, 0.9659258262890683122, 1.000000000000000000, 0.9659258262890683122, 1.000000000000000000, 0.9659258262890683122, 1.000000000000000000, 0.9659258262890683122, 1.000000000000000000, 0.9659258262890683122, 1.000000000000000000, 0.9659258262890683122, 1.000000000000000000, 0.9659258262890683122, 1.000000000000000000, 0.9659258262890683122, 1.000000000000000000, 0.9659258262890683122, 1.000000000000000000, 0.9659258262890683122, 1.000000000000000000, 0.9659258262890683122, 1.000000000000000000, 0.9659258262890683122, 1.000000000000000000, 0.9659258262890683122, 1.000000000000000000, 0.9659258262890683122, 1.000000000000000000, 0.9659258262890683122, 1.000000000000000000, 0.9659258262890683122, 1.000000000000000000, 0.9659258262890683122, 1.000000000000000000, 0.9659258262890683122, 1.000000000000000000, 0.9659258262890683122, 1.000000000000000000, 0.9659258262890683122, 1.000000000000000000, 0.9659258262890683122, 1.000000000000000000, 0.9659258262890683122, 1.000000000000000000, 0.9659258262890683122, 1.000000000000000000, 0.9659258262890683122, 1.000000000000000000, 0.9659258262890683122, 1.000000000000000000, 0.9659258262890683122, 1.000000000000000000, 0.9659258262890683122, 1.000000000000000000, 0.9659258262890683122, 1.000000000000000000, 0.9659258262890683122, 1.000000000000000000, 0.9659258262890683122, 1.000000000000000000, 0.9659258262890683122, 1.000000000000000000, 0.9659258262890683122, 1.000000000000000000, 0.9659258262890683122, 1.000000000000000000, 0.9659258262890683122, 1.000000000000000000, 0.9659258262890683122, 1.000000000000000000, 0.9659258262890683122, 1.000000000000000000, 0.9659258262890683122, 1.000000000000000000, 0.9659258262890683122, 1.000000000000000000, 0.9659258262890683122, 1.000000000000000000, 0.9659258262890683122, 1.000000000000000000, 0.9659258262890683122, 1.000000000000000000, 0.9659258262890683122, 1.000000000000000000, 0.9659258262890683122, 1.000000000000000000, 0.9659258262890683122, 1.000000000000000000, 0.9659258262890683122, 1.000000000000000000, 0.9659258262890683122, 1.000000000000000000, 0.9659258262890683122, 1.000000000000000000, 0.9659258262890683122, 1.000000000000000000, 0.9659258262890683122, 1.000000000000000000, 0.9659258262890683122, 1.000000000000000000, 0.9659258262890683122, 1.000000000000000000, 0.9659258262890683122, 1.000000000000000000, 0.9659258262890683122, 1.000000000000000000, 0.9659258262890683122, 1.000000000000000000, 0.9659258262890683122, 1.000000000000000000, 0.9659258262890683122, 1.000000000000000000, 0.9659258262890683122, 1.000000000000000000, 0.9659258262890683122, 1.000000000000000000, 0.9659258262890683122, 1.000000000000000000, 0.9659258262890683122, 1.000000000000000000, 0.9659258262890683122, 1.000000000000000000, 0.9659258262890683122, 1.000000000000000000, 0.9659258262890683122, 1.000000000000000000, 0.9659258262890683122, 1.000000000000000000, 0.9659258262890683122, 1.000000000000000000, 0.9659258262890683122, 1.000000000000000000, 0.9659258262890683122, 1.000000000000000000, 0.9659258262890683122, 1.000000000000000000, 0.9659258262890683122, 1.000000000000000000, 0.9659258262890683122, 1.000000000000000000, 0.9659258262890683122, 1.000000000000000000, 0.9659258262890683122, 1.000000000000000000, 0.9659258262890683122, 1.000000000000000000, 0.9659258262890683122, 1.000000000000000000, 0.9659258262890683122, 1.000000000000000000),
 ( 0.8047378541243613848, 0.7773170766911654539, 0.8047378541243613848, 0.7773170766911654539, 0.8047378541243613848, 0.7773170766911654539, 0.8047378541243613848, 0.7773170766911654539, 0.8047378541243613848, 0.7773170766911654539, 0.8047378541243613848, 0.7773170766911654539, 0.8047378541243613848, 0.7773170766911654539, 0.8047378541243613848, 0.7773170766911654539, 0.8047378541243613848, 0.7773170766911654539, 0.8047378541243613848, 0.7773170766911654539, 0.8047378541243613848, 0.7773170766911654539, 0.8047378541243613848, 0.7773170766911654539, 0.8047378541243613848, 0.7773170766911654539, 0.8047378541243613848, 0.7773170766911654539, 0.8047378541243613848, 0.7773170766911654539, 0.8047378541243613848, 0.7773170766911654539, 0.8047378541243613848, 0.7773170766911654539, 0.8047378541243613848, 0.7773170766911654539, 0.8047378541243613848, 0.7773170766911654539, 0.8047378541243613848, 0.7773170766911654539, 0.8047378541243613848, 0.7773170766911654539, 0.8047378541243613848, 0.7773170766911654539, 0.8047378541243613848, 0.7773170766911654539, 0.8047378541243613848, 0.7773170766911654539, 0.8047378541243613848, 0.7773170766911654539, 0.8047378541243613848, 0.7773170766911654539, 0.8047378541243613848, 0.7773170766911654539, 0.8047378541243613848, 0.7773170766911654539, 0.8047378541243613848, 0.7773170766911654539, 0.8047378541243613848, 0.7773170766911654539, 0.8047378541243613848, 0.7773170766911654539, 0.8047378541243613848, 0.7773170766911654539, 0.8047378541243613848, 0.7773170766911654539, 0.8047378541243613848, 0.7773170766911654539, 0.8047378541243613848, 0.7773170766911654539, 0.8047378541243613848, 0.7773170766911654539, 0.8047378541243613848, 0.7773170766911654539, 0.8047378541243613848, 0.7773170766911654539, 0.8047378541243613848, 0.7773170766911654539, 0.8047378541243613848, 0.7773170766911654539, 0.8047378541243613848, 0.7773170766911654539, 0.8047378541243613848, 0.7773170766911654539, 0.8047378541243613848, 0.7773170766911654539, 0.8047378541243613848, 0.7773170766911654539, 0.8047378541243613848, 0.7773170766911654539, 0.8047378541243613848, 0.7773170766911654539, 0.8047378541243613848, 0.7773170766911654539, 0.8047378541243613848, 0.7773170766911654539, 0.8047378541243613848, 0.7773170766911654539, 0.8047378541243613848, 0.7773170766911654539, 0.8047378541243613848, 0.7773170766911654539, 0.8047378541243613848, 0.7773170766911654539, 0.8047378541243613848, 0.7773170766911654539, 0.8047378541243613848, 0.7773170766911654539, 0.8047378541243613848, 0.7773170766911654539, 0.8047378541243613848, 0.7773170766911654539, 0.8047378541243613848, 0.7773170766911654539, 0.8047378541243613848, 0.7773170766911654539, 0.8047378541243613848, 0.7773170766911654539, 0.8047378541243613848, 0.7773170766911654539, 0.8047378541243613848, 0.7773170766911654539, 0.8047378541243613848, 0.7773170766911654539, 0.8047378541243613848, 0.7773170766911654539, 0.8047378541243613848, 0.7773170766911654539, 0.8047378541243613848, 0.7773170766911654539, 0.8047378541243613848, 0.7773170766911654539, 0.8047378541243613848, 0.7773170766911654539, 0.8047378541243613848, 0.7773170766911654539, 0.8047378541243613848, 0.7773170766911654539, 0.8047378541243613848, 0.7773170766911654539, 0.8047378541243613848, 0.7773170766911654539, 0.8047378541243613848, 0.7773170766911654539, 0.8047378541243613848, 0.7773170766911654539, 0.8047378541243613848, 0.7773170766911654539, 0.8047378541243613848, 0.7773170766911654539, 0.8047378541243613848, 0.7773170766911654539, 0.8047378541243613848, 0.7773170766911654539, 0.8047378541243613848, 0.7773170766911654539, 0.8047378541243613848, 0.7773170766911654539, 0.8047378541243613848, 0.7773170766911654539, 0.8047378541243613848, 0.7773170766911654539, 0.8047378541243613848, 0.7773170766911654539, 0.8047378541243613848, 0.7773170766911654539, 0.8047378541243613848, 0.7773170766911654539, 0.8047378541243613848, 0.7773170766911654539, 0.8047378541243613848, 0.7773170766911654539, 0.8047378541243613848, 0.7773170766911654539, 0.8047378541243613848, 0.7773170766911654539, 0.8047378541243613848, 0.7773170766911654539, 0.8047378541243613848, 0.7773170766911654539, 0.8047378541243613848, 0.7773170766911654539, 0.8047378541243613848, 0.7773170766911654539, 0.8047378541243613848, 0.7773170766911654539, 0.8047378541243613848, 0.7773170766911654539, 0.8047378541243613848, 0.7773170766911654539, 0.8047378541243613848, 0.7773170766911654539, 0.8047378541243613848, 0.7773170766911654539, 0.8047378541243613848, 0.7773170766911654539, 0.8047378541243613848, 0.7773170766911654539, 0.8047378541243613848, 0.7773170766911654539, 0.8047378541243613848, 0.7773170766911654539, 0.8047378541243613848, 0.7773170766911654539, 0.8047378541243613848, 0.7773170766911654539, 0.8047378541243613848, 0.7773170766911654539, 0.8047378541243613848, 0.7773170766911654539, 0.8047378541243613848, 0.7773170766911654539, 0.8047378541243613848, 0.7773170766911654539, 0.8047378541243613848, 0.7773170766911654539, 0.8047378541243613848, 0.7773170766911654539, 0.8047378541243613848, 0.7773170766911654539, 0.8047378541243613848, 0.7773170766911654539, 0.8047378541243613848, 0.7773170766911654539, 0.8047378541243613848, 0.7773170766911654539, 0.8047378541243613848, 0.7773170766911654539, 0.8047378541243613848, 0.7773170766911654539, 0.8047378541243613848, 0.7773170766911654539, 0.8047378541243613848, 0.7773170766911654539, 0.8047378541243613848, 0.7773170766911654539, 0.8047378541243613848, 0.7773170766911654539, 0.8047378541243613848, 0.7773170766911654539, 0.8047378541243613848, 0.7773170766911654539, 0.8047378541243613848, 0.7773170766911654539, 0.8047378541243613848, 0.7773170766911654539, 0.8047378541243613848, 0.7773170766911654539, 0.8047378541243613848, 0.7773170766911654539, 0.8047378541243613848, 0.7773170766911654539, 0.8047378541243613848, 0.7773170766911654539, 0.8047378541243613848, 0.7773170766911654539, 0.8047378541243613848, 0.7773170766911654539, 0.8047378541243613848, 0.7773170766911654539, 0.8047378541243613848, 0.7773170766911654539, 0.8047378541243613848, 0.7773170766911654539, 0.8047378541243613848, 0.7773170766911654539, 0.8047378541243613848, 0.7773170766911654539, 0.8047378541243613848, 0.7773170766911654539, 0.8047378541243613848, 0.7773170766911654539, 0.8047378541243613848, 0.7773170766911654539, 0.8047378541243613848, 0.7773170766911654539, 0.8047378541243613848, 0.7773170766911654539, 0.8047378541243613848, 0.7773170766911654539, 0.8047378541243613848, 0.7773170766911654539, 0.8047378541243613848, 0.7773170766911654539, 0.8047378541243613848, 0.7773170766911654539, 0.8047378541243613848, 0.7773170766911654539, 0.8047378541243613848, 0.7773170766911654539, 0.8047378541243613848, 0.7773170766911654539, 0.8047378541243613848, 0.7773170766911654539, 0.8047378541243613848, 0.7773170766911654539, 0.8047378541243613848, 0.7773170766911654539, 0.8047378541243613848, 0.7773170766911654539, 0.8047378541243613848, 0.7773170766911654539, 0.8047378541243613848, 0.7773170766911654539, 0.8047378541243613848, 0.7773170766911654539, 0.8047378541243613848, 0.7773170766911654539, 0.8047378541243613848, 0.7773170766911654539, 0.8047378541243613848, 0.7773170766911654539, 0.8047378541243613848, 0.7773170766911654539, 0.8047378541243613848, 0.7773170766911654539, 0.8047378541243613848, 0.7773170766911654539, 0.8047378541243613848, 0.7773170766911654539, 0.8047378541243613848, 0.7773170766911654539, 0.8047378541243613848, 0.7773170766911654539, 0.8047378541243613848, 0.7773170766911654539, 0.8047378541243613848, 0.7773170766911654539, 0.8047378541243613848, 0.7773170766911654539, 0.8047378541243613848, 0.7773170766911654539, 0.8047378541243613848, 0.7773170766911654539, 0.8047378541243613848, 0.7773170766911654539, 0.8047378541243613848, 0.7773170766911654539, 0.8047378541243613848, 0.7773170766911654539, 0.8047378541243613848, 0.7773170766911654539, 0.8047378541243613848, 0.7773170766911654539, 0.8047378541243613848, 0.7773170766911654539, 0.8047378541243613848, 0.7773170766911654539, 0.8047378541243613848, 0.7773170766911654539, 0.8047378541243613848, 0.7773170766911654539, 0.8047378541243613848, 0.7773170766911654539, 0.8047378541243613848, 0.7773170766911654539, 0.8047378541243613848, 0.7773170766911654539, 0.8047378541243613848, 0.7773170766911654539, 0.8047378541243613848, 0.7773170766911654539, 0.8047378541243613848, 0.7773170766911654539, 0.8047378541243613848, 0.7773170766911654539, 0.8047378541243613848, 0.7773170766911654539, 0.8047378541243613848, 0.7773170766911654539, 0.8047378541243613848, 0.7773170766911654539, 0.8047378541243613848, 0.7773170766911654539, 0.8047378541243613848, 0.7773170766911654539, 0.8047378541243613848, 0.7773170766911654539, 0.8047378541243613848, 0.7773170766911654539, 0.8047378541243613848, 0.7773170766911654539, 0.8047378541243613848, 0.7773170766911654539, 0.8047378541243613848, 0.7773170766911654539, 0.8047378541243613848, 0.7773170766911654539, 0.8047378541243613848, 0.7773170766911654539, 0.8047378541243613848, 0.7773170766911654539, 0.8047378541243613848, 0.7773170766911654539, 0.8047378541243613848, 0.7773170766911654539, 0.8047378541243613848, 0.7773170766911654539, 0.8047378541243613848, 0.7773170766911654539, 0.8047378541243613848, 0.7773170766911654539, 0.8047378541243613848, 0.7773170766911654539, 0.8047378541243613848, 0.7773170766911654539, 0.8047378541243613848, 0.7773170766911654539, 0.8047378541243613848, 0.7773170766911654539, 0.8047378541243613848, 0.7773170766911654539, 0.8047378541243613848, 0.7773170766911654539, 0.8047378541243613848, 0.7773170766911654539, 0.8047378541243613848, 0.7773170766911654539, 0.8047378541243613848, 0.7773170766911654539, 0.8047378541243613848, 0.7773170766911654539, 0.8047378541243613848, 0.7773170766911654539, 0.8047378541243613848, 0.7773170766911654539, 0.8047378541243613848, 0.7773170766911654539, 0.8047378541243613848, 0.7773170766911654539, 0.8047378541243613848, 0.7773170766911654539, 0.8047378541243613848, 0.7773170766911654539, 0.8047378541243613848, 0.7773170766911654539, 0.8047378541243613848, 0.7773170766911654539, 0.8047378541243613848, 0.7773170766911654539, 0.8047378541243613848, 0.7773170766911654539, 0.8047378541243613848, 0.7773170766911654539, 0.8047378541243613848, 0.7773170766911654539, 0.8047378541243613848, 0.7773170766911654539, 0.8047378541243613848, 0.7773170766911654539, 0.8047378541243613848, 0.7773170766911654539, 0.8047378541243613848, 0.7773170766911654539, 0.8047378541243613848, 0.7773170766911654539, 0.8047378541243613848, 0.7773170766911654539, 0.8047378541243613848, 0.7773170766911654539, 0.8047378541243613848, 0.7773170766911654539, 0.8047378541243613848, 0.7773170766911654539, 0.8047378541243613848, 0.7773170766911654539, 0.8047378541243613848, 0.7773170766911654539, 0.8047378541243613848, 0.7773170766911654539, 0.8047378541243613848, 0.7773170766911654539, 0.8047378541243613848, 0.7773170766911654539, 0.8047378541243613848),
 ( 0.8047378541243613848, 0.7773170766911654539, 0.8047378541243613848, 0.7773170766911654539, 0.8047378541243613848, 0.7773170766911654539, 0.8047378541243613848, 0.7773170766911654539, 0.8047378541243613848, 0.7773170766911654539, 0.8047378541243613848, 0.7773170766911654539, 0.8047378541243613848, 0.7773170766911654539, 0.8047378541243613848, 0.7773170766911654539, 0.8047378541243613848, 0.7773170766911654539, 0.8047378541243613848, 0.7773170766911654539, 0.8047378541243613848, 0.7773170766911654539, 0.8047378541243613848, 0.7773170766911654539, 0.8047378541243613848, 0.7773170766911654539, 0.8047378541243613848, 0.7773170766911654539, 0.8047378541243613848, 0.7773170766911654539, 0.8047378541243613848, 0.7773170766911654539, 0.8047378541243613848, 0.7773170766911654539, 0.8047378541243613848, 0.7773170766911654539, 0.8047378541243613848, 0.7773170766911654539, 0.8047378541243613848, 0.7773170766911654539, 0.8047378541243613848, 0.7773170766911654539, 0.8047378541243613848, 0.7773170766911654539, 0.8047378541243613848, 0.7773170766911654539, 0.8047378541243613848, 0.7773170766911654539, 0.8047378541243613848, 0.7773170766911654539, 0.8047378541243613848, 0.7773170766911654539, 0.8047378541243613848, 0.7773170766911654539, 0.8047378541243613848, 0.7773170766911654539, 0.8047378541243613848, 0.7773170766911654539, 0.8047378541243613848, 0.7773170766911654539, 0.8047378541243613848, 0.7773170766911654539, 0.8047378541243613848, 0.7773170766911654539, 0.8047378541243613848, 0.7773170766911654539, 0.8047378541243613848, 0.7773170766911654539, 0.8047378541243613848, 0.7773170766911654539, 0.8047378541243613848, 0.7773170766911654539, 0.8047378541243613848, 0.7773170766911654539, 0.8047378541243613848, 0.7773170766911654539, 0.8047378541243613848, 0.7773170766911654539, 0.8047378541243613848, 0.7773170766911654539, 0.8047378541243613848, 0.7773170766911654539, 0.8047378541243613848, 0.7773170766911654539, 0.8047378541243613848, 0.7773170766911654539, 0.8047378541243613848, 0.7773170766911654539, 0.8047378541243613848, 0.7773170766911654539, 0.8047378541243613848, 0.7773170766911654539, 0.8047378541243613848, 0.7773170766911654539, 0.8047378541243613848, 0.7773170766911654539, 0.8047378541243613848, 0.7773170766911654539, 0.8047378541243613848, 0.7773170766911654539, 0.8047378541243613848, 0.7773170766911654539, 0.8047378541243613848, 0.7773170766911654539, 0.8047378541243613848, 0.7773170766911654539, 0.8047378541243613848, 0.7773170766911654539, 0.8047378541243613848, 0.7773170766911654539, 0.8047378541243613848, 0.7773170766911654539, 0.8047378541243613848, 0.7773170766911654539, 0.8047378541243613848, 0.7773170766911654539, 0.8047378541243613848, 0.7773170766911654539, 0.8047378541243613848, 0.7773170766911654539, 0.8047378541243613848, 0.7773170766911654539, 0.8047378541243613848, 0.7773170766911654539, 0.8047378541243613848, 0.7773170766911654539, 0.8047378541243613848, 0.7773170766911654539, 0.8047378541243613848, 0.7773170766911654539, 0.8047378541243613848, 0.7773170766911654539, 0.8047378541243613848, 0.7773170766911654539, 0.8047378541243613848, 0.7773170766911654539, 0.8047378541243613848, 0.7773170766911654539, 0.8047378541243613848, 0.7773170766911654539, 0.8047378541243613848, 0.7773170766911654539, 0.8047378541243613848, 0.7773170766911654539, 0.8047378541243613848, 0.7773170766911654539, 0.8047378541243613848, 0.7773170766911654539, 0.8047378541243613848, 0.7773170766911654539, 0.8047378541243613848, 0.7773170766911654539, 0.8047378541243613848, 0.7773170766911654539, 0.8047378541243613848, 0.7773170766911654539, 0.8047378541243613848, 0.7773170766911654539, 0.8047378541243613848, 0.7773170766911654539, 0.8047378541243613848, 0.7773170766911654539, 0.8047378541243613848, 0.7773170766911654539, 0.8047378541243613848, 0.7773170766911654539, 0.8047378541243613848, 0.7773170766911654539, 0.8047378541243613848, 0.7773170766911654539, 0.8047378541243613848, 0.7773170766911654539, 0.8047378541243613848, 0.7773170766911654539, 0.8047378541243613848, 0.7773170766911654539, 0.8047378541243613848, 0.7773170766911654539, 0.8047378541243613848, 0.7773170766911654539, 0.8047378541243613848, 0.7773170766911654539, 0.8047378541243613848, 0.7773170766911654539, 0.8047378541243613848, 0.7773170766911654539, 0.8047378541243613848, 0.7773170766911654539, 0.8047378541243613848, 0.7773170766911654539, 0.8047378541243613848, 0.7773170766911654539, 0.8047378541243613848, 0.7773170766911654539, 0.8047378541243613848, 0.7773170766911654539, 0.8047378541243613848, 0.7773170766911654539, 0.8047378541243613848, 0.7773170766911654539, 0.8047378541243613848, 0.7773170766911654539, 0.8047378541243613848, 0.7773170766911654539, 0.8047378541243613848, 0.7773170766911654539, 0.8047378541243613848, 0.7773170766911654539, 0.8047378541243613848, 0.7773170766911654539, 0.8047378541243613848, 0.7773170766911654539, 0.8047378541243613848, 0.7773170766911654539, 0.8047378541243613848, 0.7773170766911654539, 0.8047378541243613848, 0.7773170766911654539, 0.8047378541243613848, 0.7773170766911654539, 0.8047378541243613848, 0.7773170766911654539, 0.8047378541243613848, 0.7773170766911654539, 0.8047378541243613848, 0.7773170766911654539, 0.8047378541243613848, 0.7773170766911654539, 0.8047378541243613848, 0.7773170766911654539, 0.8047378541243613848, 0.7773170766911654539, 0.8047378541243613848, 0.7773170766911654539, 0.8047378541243613848, 0.7773170766911654539, 0.8047378541243613848, 0.7773170766911654539, 0.8047378541243613848, 0.7773170766911654539, 0.8047378541243613848, 0.7773170766911654539, 0.8047378541243613848, 0.7773170766911654539, 0.8047378541243613848, 0.7773170766911654539, 0.8047378541243613848, 0.7773170766911654539, 0.8047378541243613848, 0.7773170766911654539, 0.8047378541243613848, 0.7773170766911654539, 0.8047378541243613848, 0.7773170766911654539, 0.8047378541243613848, 0.7773170766911654539, 0.8047378541243613848, 0.7773170766911654539, 0.8047378541243613848, 0.7773170766911654539, 0.8047378541243613848, 0.7773170766911654539, 0.8047378541243613848, 0.7773170766911654539, 0.8047378541243613848, 0.7773170766911654539, 0.8047378541243613848, 0.7773170766911654539, 0.8047378541243613848, 0.7773170766911654539, 0.8047378541243613848, 0.7773170766911654539, 0.8047378541243613848, 0.7773170766911654539, 0.8047378541243613848, 0.7773170766911654539, 0.8047378541243613848, 0.7773170766911654539, 0.8047378541243613848, 0.7773170766911654539, 0.8047378541243613848, 0.7773170766911654539, 0.8047378541243613848, 0.7773170766911654539, 0.8047378541243613848, 0.7773170766911654539, 0.8047378541243613848, 0.7773170766911654539, 0.8047378541243613848, 0.7773170766911654539, 0.8047378541243613848, 0.7773170766911654539, 0.8047378541243613848, 0.7773170766911654539, 0.8047378541243613848, 0.7773170766911654539, 0.8047378541243613848, 0.7773170766911654539, 0.8047378541243613848, 0.7773170766911654539, 0.8047378541243613848, 0.7773170766911654539, 0.8047378541243613848, 0.7773170766911654539, 0.8047378541243613848, 0.7773170766911654539, 0.8047378541243613848, 0.7773170766911654539, 0.8047378541243613848, 0.7773170766911654539, 0.8047378541243613848, 0.7773170766911654539, 0.8047378541243613848, 0.7773170766911654539, 0.8047378541243613848, 0.7773170766911654539, 0.8047378541243613848, 0.7773170766911654539, 0.8047378541243613848, 0.7773170766911654539, 0.8047378541243613848, 0.7773170766911654539, 0.8047378541243613848, 0.7773170766911654539, 0.8047378541243613848, 0.7773170766911654539, 0.8047378541243613848, 0.7773170766911654539, 0.8047378541243613848, 0.7773170766911654539, 0.8047378541243613848, 0.7773170766911654539, 0.8047378541243613848, 0.7773170766911654539, 0.8047378541243613848, 0.7773170766911654539, 0.8047378541243613848, 0.7773170766911654539, 0.8047378541243613848, 0.7773170766911654539, 0.8047378541243613848, 0.7773170766911654539, 0.8047378541243613848, 0.7773170766911654539, 0.8047378541243613848, 0.7773170766911654539, 0.8047378541243613848, 0.7773170766911654539, 0.8047378541243613848, 0.7773170766911654539, 0.8047378541243613848, 0.7773170766911654539, 0.8047378541243613848, 0.7773170766911654539, 0.8047378541243613848, 0.7773170766911654539, 0.8047378541243613848, 0.7773170766911654539, 0.8047378541243613848, 0.7773170766911654539, 0.8047378541243613848, 0.7773170766911654539, 0.8047378541243613848, 0.7773170766911654539, 0.8047378541243613848, 0.7773170766911654539, 0.8047378541243613848, 0.7773170766911654539, 0.8047378541243613848, 0.7773170766911654539, 0.8047378541243613848, 0.7773170766911654539, 0.8047378541243613848, 0.7773170766911654539, 0.8047378541243613848, 0.7773170766911654539, 0.8047378541243613848, 0.7773170766911654539, 0.8047378541243613848, 0.7773170766911654539, 0.8047378541243613848, 0.7773170766911654539, 0.8047378541243613848, 0.7773170766911654539, 0.8047378541243613848, 0.7773170766911654539, 0.8047378541243613848, 0.7773170766911654539, 0.8047378541243613848, 0.7773170766911654539, 0.8047378541243613848, 0.7773170766911654539, 0.8047378541243613848, 0.7773170766911654539, 0.8047378541243613848, 0.7773170766911654539, 0.8047378541243613848, 0.7773170766911654539, 0.8047378541243613848, 0.7773170766911654539, 0.8047378541243613848, 0.7773170766911654539, 0.8047378541243613848, 0.7773170766911654539, 0.8047378541243613848, 0.7773170766911654539, 0.8047378541243613848, 0.7773170766911654539, 0.8047378541243613848, 0.7773170766911654539, 0.8047378541243613848, 0.7773170766911654539, 0.8047378541243613848, 0.7773170766911654539, 0.8047378541243613848, 0.7773170766911654539, 0.8047378541243613848, 0.7773170766911654539, 0.8047378541243613848, 0.7773170766911654539, 0.8047378541243613848, 0.7773170766911654539, 0.8047378541243613848, 0.7773170766911654539, 0.8047378541243613848, 0.7773170766911654539, 0.8047378541243613848, 0.7773170766911654539, 0.8047378541243613848, 0.7773170766911654539, 0.8047378541243613848, 0.7773170766911654539, 0.8047378541243613848, 0.7773170766911654539, 0.8047378541243613848, 0.7773170766911654539, 0.8047378541243613848, 0.7773170766911654539, 0.8047378541243613848, 0.7773170766911654539, 0.8047378541243613848, 0.7773170766911654539, 0.8047378541243613848, 0.7773170766911654539, 0.8047378541243613848, 0.7773170766911654539, 0.8047378541243613848, 0.7773170766911654539, 0.8047378541243613848, 0.7773170766911654539, 0.8047378541243613848, 0.7773170766911654539, 0.8047378541243613848, 0.7773170766911654539, 0.8047378541243613848, 0.7773170766911654539, 0.8047378541243613848, 0.7773170766911654539, 0.8047378541243613848, 0.7773170766911654539, 0.8047378541243613848, 0.7773170766911654539, 0.8047378541243613848, 0.7773170766911654539, 0.8047378541243613848, 0.7773170766911654539, 0.8047378541243613848, 0.7773170766911654539, 0.8047378541243613848, 0.7773170766911654539, 0.8047378541243613848, 0.7773170766911654539, 0.8047378541243613848, 0.7773170766911654539, 0.8047378541243613848),
 ( 1.000000000000000000, 0.9659258262890683122, 1.000000000000000000, 0.9659258262890683122, 1.000000000000000000, 0.9659258262890683122, 1.000000000000000000, 0.9659258262890683122, 1.000000000000000000, 0.9659258262890683122, 1.000000000000000000, 0.9659258262890683122, 1.000000000000000000, 0.9659258262890683122, 1.000000000000000000, 0.9659258262890683122, 1.000000000000000000, 0.9659258262890683122, 1.000000000000000000, 0.9659258262890683122, 1.000000000000000000, 0.9659258262890683122, 1.000000000000000000, 0.9659258262890683122, 1.000000000000000000, 0.9659258262890683122, 1.000000000000000000, 0.9659258262890683122, 1.000000000000000000, 0.9659258262890683122, 1.000000000000000000, 0.9659258262890683122, 1.000000000000000000, 0.9659258262890683122, 1.000000000000000000, 0.9659258262890683122, 1.000000000000000000, 0.9659258262890683122, 1.000000000000000000, 0.9659258262890683122, 1.000000000000000000, 0.9659258262890683122, 1.000000000000000000, 0.9659258262890683122, 1.000000000000000000, 0.9659258262890683122, 1.000000000000000000, 0.9659258262890683122, 1.000000000000000000, 0.9659258262890683122, 1.000000000000000000, 0.9659258262890683122, 1.000000000000000000, 0.9659258262890683122, 1.000000000000000000, 0.9659258262890683122, 1.000000000000000000, 0.9659258262890683122, 1.000000000000000000, 0.9659258262890683122, 1.000000000000000000, 0.9659258262890683122, 1.000000000000000000, 0.9659258262890683122, 1.000000000000000000, 0.9659258262890683122, 1.000000000000000000, 0.9659258262890683122, 1.000000000000000000, 0.9659258262890683122, 1.000000000000000000, 0.9659258262890683122, 1.000000000000000000, 0.9659258262890683122, 1.000000000000000000, 0.9659258262890683122, 1.000000000000000000, 0.9659258262890683122, 1.000000000000000000, 0.9659258262890683122, 1.000000000000000000, 0.9659258262890683122, 1.000000000000000000, 0.9659258262890683122, 1.000000000000000000, 0.9659258262890683122, 1.000000000000000000, 0.9659258262890683122, 1.000000000000000000, 0.9659258262890683122, 1.000000000000000000, 0.9659258262890683122, 1.000000000000000000, 0.9659258262890683122, 1.000000000000000000, 0.9659258262890683122, 1.000000000000000000, 0.9659258262890683122, 1.000000000000000000, 0.9659258262890683122, 1.000000000000000000, 0.9659258262890683122, 1.000000000000000000, 0.9659258262890683122, 1.000000000000000000, 0.9659258262890683122, 1.000000000000000000, 0.9659258262890683122, 1.000000000000000000, 0.9659258262890683122, 1.000000000000000000, 0.9659258262890683122, 1.000000000000000000, 0.9659258262890683122, 1.000000000000000000, 0.9659258262890683122, 1.000000000000000000, 0.9659258262890683122, 1.000000000000000000, 0.9659258262890683122, 1.000000000000000000, 0.9659258262890683122, 1.000000000000000000, 0.9659258262890683122, 1.000000000000000000, 0.9659258262890683122, 1.000000000000000000, 0.9659258262890683122, 1.000000000000000000, 0.9659258262890683122, 1.000000000000000000, 0.9659258262890683122, 1.000000000000000000, 0.9659258262890683122, 1.000000000000000000, 0.9659258262890683122, 1.000000000000000000, 0.9659258262890683122, 1.000000000000000000, 0.9659258262890683122, 1.000000000000000000, 0.9659258262890683122, 1.000000000000000000, 0.9659258262890683122, 1.000000000000000000, 0.9659258262890683122, 1.000000000000000000, 0.9659258262890683122, 1.000000000000000000, 0.9659258262890683122, 1.000000000000000000, 0.9659258262890683122, 1.000000000000000000, 0.9659258262890683122, 1.000000000000000000, 0.9659258262890683122, 1.000000000000000000, 0.9659258262890683122, 1.000000000000000000, 0.9659258262890683122, 1.000000000000000000, 0.9659258262890683122, 1.000000000000000000, 0.9659258262890683122, 1.000000000000000000, 0.9659258262890683122, 1.000000000000000000, 0.9659258262890683122, 1.000000000000000000, 0.9659258262890683122, 1.000000000000000000, 0.9659258262890683122, 1.000000000000000000, 0.9659258262890683122, 1.000000000000000000, 0.9659258262890683122, 1.000000000000000000, 0.9659258262890683122, 1.000000000000000000, 0.9659258262890683122, 1.000000000000000000, 0.9659258262890683122, 1.000000000000000000, 0.9659258262890683122, 1.000000000000000000, 0.9659258262890683122, 1.000000000000000000, 0.9659258262890683122, 1.000000000000000000, 0.9659258262890683122, 1.000000000000000000, 0.9659258262890683122, 1.000000000000000000, 0.9659258262890683122, 1.000000000000000000, 0.9659258262890683122, 1.000000000000000000, 0.9659258262890683122, 1.000000000000000000, 0.9659258262890683122, 1.000000000000000000, 0.9659258262890683122, 1.000000000000000000, 0.9659258262890683122, 1.000000000000000000, 0.9659258262890683122, 1.000000000000000000, 0.9659258262890683122, 1.000000000000000000, 0.9659258262890683122, 1.000000000000000000, 0.9659258262890683122, 1.000000000000000000, 0.9659258262890683122, 1.000000000000000000, 0.9659258262890683122, 1.000000000000000000, 0.9659258262890683122, 1.000000000000000000, 0.9659258262890683122, 1.000000000000000000, 0.9659258262890683122, 1.000000000000000000, 0.9659258262890683122, 1.000000000000000000, 0.9659258262890683122, 1.000000000000000000, 0.9659258262890683122, 1.000000000000000000, 0.9659258262890683122, 1.000000000000000000, 0.9659258262890683122, 1.000000000000000000, 0.9659258262890683122, 1.000000000000000000, 0.9659258262890683122, 1.000000000000000000, 0.9659258262890683122, 1.000000000000000000, 0.9659258262890683122, 1.000000000000000000, 0.9659258262890683122, 1.000000000000000000, 0.9659258262890683122, 1.000000000000000000, 0.9659258262890683122, 1.000000000000000000, 0.9659258262890683122, 1.000000000000000000, 0.9659258262890683122, 1.000000000000000000, 0.9659258262890683122, 1.000000000000000000, 0.9659258262890683122, 1.000000000000000000, 0.9659258262890683122, 1.000000000000000000, 0.9659258262890683122, 1.000000000000000000, 0.9659258262890683122, 1.000000000000000000, 0.9659258262890683122, 1.000000000000000000, 0.9659258262890683122, 1.000000000000000000, 0.9659258262890683122, 1.000000000000000000, 0.9659258262890683122, 1.000000000000000000, 0.9659258262890683122, 1.000000000000000000, 0.9659258262890683122, 1.000000000000000000, 0.9659258262890683122, 1.000000000000000000, 0.9659258262890683122, 1.000000000000000000, 0.9659258262890683122, 1.000000000000000000, 0.9659258262890683122, 1.000000000000000000, 0.9659258262890683122, 1.000000000000000000, 0.9659258262890683122, 1.000000000000000000, 0.9659258262890683122, 1.000000000000000000, 0.9659258262890683122, 1.000000000000000000, 0.9659258262890683122, 1.000000000000000000, 0.9659258262890683122, 1.000000000000000000, 0.9659258262890683122, 1.000000000000000000, 0.9659258262890683122, 1.000000000000000000, 0.9659258262890683122, 1.000000000000000000, 0.9659258262890683122, 1.000000000000000000, 0.9659258262890683122, 1.000000000000000000, 0.9659258262890683122, 1.000000000000000000, 0.9659258262890683122, 1.000000000000000000, 0.9659258262890683122, 1.000000000000000000, 0.9659258262890683122, 1.000000000000000000, 0.9659258262890683122, 1.000000000000000000, 0.9659258262890683122, 1.000000000000000000, 0.9659258262890683122, 1.000000000000000000, 0.9659258262890683122, 1.000000000000000000, 0.9659258262890683122, 1.000000000000000000, 0.9659258262890683122, 1.000000000000000000, 0.9659258262890683122, 1.000000000000000000, 0.9659258262890683122, 1.000000000000000000, 0.9659258262890683122, 1.000000000000000000, 0.9659258262890683122, 1.000000000000000000, 0.9659258262890683122, 1.000000000000000000, 0.9659258262890683122, 1.000000000000000000, 0.9659258262890683122, 1.000000000000000000, 0.9659258262890683122, 1.000000000000000000, 0.9659258262890683122, 1.000000000000000000, 0.9659258262890683122, 1.000000000000000000, 0.9659258262890683122, 1.000000000000000000, 0.9659258262890683122, 1.000000000000000000, 0.9659258262890683122, 1.000000000000000000, 0.9659258262890683122, 1.000000000000000000, 0.9659258262890683122, 1.000000000000000000, 0.9659258262890683122, 1.000000000000000000, 0.9659258262890683122, 1.000000000000000000, 0.9659258262890683122, 1.000000000000000000, 0.9659258262890683122, 1.000000000000000000, 0.9659258262890683122, 1.000000000000000000, 0.9659258262890683122, 1.000000000000000000, 0.9659258262890683122, 1.000000000000000000, 0.9659258262890683122, 1.000000000000000000, 0.9659258262890683122, 1.000000000000000000, 0.9659258262890683122, 1.000000000000000000, 0.9659258262890683122, 1.000000000000000000, 0.9659258262890683122, 1.000000000000000000, 0.9659258262890683122, 1.000000000000000000, 0.9659258262890683122, 1.000000000000000000, 0.9659258262890683122, 1.000000000000000000, 0.9659258262890683122, 1.000000000000000000, 0.9659258262890683122, 1.000000000000000000, 0.9659258262890683122, 1.000000000000000000, 0.9659258262890683122, 1.000000000000000000, 0.9659258262890683122, 1.000000000000000000, 0.9659258262890683122, 1.000000000000000000, 0.9659258262890683122, 1.000000000000000000, 0.9659258262890683122, 1.000000000000000000, 0.9659258262890683122, 1.000000000000000000, 0.9659258262890683122, 1.000000000000000000, 0.9659258262890683122, 1.000000000000000000, 0.9659258262890683122, 1.000000000000000000, 0.9659258262890683122, 1.000000000000000000, 0.9659258262890683122, 1.000000000000000000, 0.9659258262890683122, 1.000000000000000000, 0.9659258262890683122, 1.000000000000000000, 0.9659258262890683122, 1.000000000000000000, 0.9659258262890683122, 1.000000000000000000, 0.9659258262890683122, 1.000000000000000000, 0.9659258262890683122, 1.000000000000000000, 0.9659258262890683122, 1.000000000000000000, 0.9659258262890683122, 1.000000000000000000, 0.9659258262890683122, 1.000000000000000000, 0.9659258262890683122, 1.000000000000000000, 0.9659258262890683122, 1.000000000000000000, 0.9659258262890683122, 1.000000000000000000, 0.9659258262890683122, 1.000000000000000000, 0.9659258262890683122, 1.000000000000000000, 0.9659258262890683122, 1.000000000000000000, 0.9659258262890683122, 1.000000000000000000, 0.9659258262890683122, 1.000000000000000000, 0.9659258262890683122, 1.000000000000000000, 0.9659258262890683122, 1.000000000000000000, 0.9659258262890683122, 1.000000000000000000, 0.9659258262890683122, 1.000000000000000000, 0.9659258262890683122, 1.000000000000000000, 0.9659258262890683122, 1.000000000000000000, 0.9659258262890683122, 1.000000000000000000, 0.9659258262890683122, 1.000000000000000000, 0.9659258262890683122, 1.000000000000000000, 0.9659258262890683122, 1.000000000000000000, 0.9659258262890683122, 1.000000000000000000, 0.9659258262890683122, 1.000000000000000000, 0.9659258262890683122, 1.000000000000000000, 0.9659258262890683122, 1.000000000000000000, 0.9659258262890683122, 1.000000000000000000) ) ) 
 REPRESENTATION_ITEM ( '' )  SURFACE ( )  );
#47688 = DIRECTION ( 'NONE',  ( 1.000000000000000000, 0.000000000000000000, 0.000000000000000000 ) ) ;
#47689 = CARTESIAN_POINT ( 'NONE',  ( 0.4724409448818897017, 0.1265901696524990294, -1.069553805774278166 ) ) ;
#47690 = CARTESIAN_POINT ( 'NONE',  ( 0.3392501089628018884, -0.1958661417322833942, -1.676528502133545206 ) ) ;
#47691 = CARTESIAN_POINT ( 'NONE',  ( 0.7611548556430454138, 0.2306618581243847221, -0.2411417322834647770 ) ) ;
#47692 = CARTESIAN_POINT ( 'NONE',  ( 0.2559055118110243332, -0.5400638737290845981, -0.3530559997133363437 ) ) ;
#47693 = CARTESIAN_POINT ( 'NONE',  ( -0.9514435695538050464, -0.05778040916215560624, -0.4822834645669293319 ) ) ;
#47694 = CARTESIAN_POINT ( 'NONE',  ( 1.266404199475066328, -0.05778040916215522460, 0.4822834645669289988 ) ) ;
#47695 = CARTESIAN_POINT ( 'NONE',  ( 0.9055118110236227702, 0.2952755905511811885, 0.000000000000000000 ) ) ;
#47696 = CARTESIAN_POINT ( 'NONE',  ( 0.1049643490035303689, 0.3917322834645670104, -0.8654855643044619962 ) ) ;
#47697 = CARTESIAN_POINT ( 'NONE',  ( -0.3215223097112853146, -0.3162353388693405765, 0.4822834645669290543 ) ) ;
#47698 = CARTESIAN_POINT ( 'NONE',  ( 0.6036745406824154392, 0.2306618581243847221, -0.2411417322834647770 ) ) ;
#47699 = CARTESIAN_POINT ( 'NONE',  ( -0.1902887139107604098, 0.2952755905511810774, -0.1292274648535930714 ) ) ;
#47700 = CARTESIAN_POINT ( 'NONE',  ( 0.8202099737532814183, -0.5511811023622048555, -0.09757992244046775898 ) ) ;
#47701 = CARTESIAN_POINT ( 'NONE',  ( -1.286089238845143479, -0.6046776061558807314, 0.2411417322834647770 ) ) ;
#47702 = CARTESIAN_POINT ( 'NONE',  ( -1.699475065616797398, 0.2952755905511811885, 0.1292274648535926551 ) ) ;
#47703 = CARTESIAN_POINT ( 'NONE',  ( 0.3477690288713918276, 0.2952755905511811885, 0.1292274648535926551 ) ) ;
#47704 = LINE ( 'NONE', #74232, #62763 ) ;
#47705 = CARTESIAN_POINT ( 'NONE',  ( 0.2867679344610365999, -0.2867679344610365444, -2.452755905511811108 ) ) ;
#47706 = EDGE_LOOP ( 'NONE', ( #7425, #60429, #17778, #72360 ) ) ;
#47707 = EDGE_LOOP ( 'NONE', ( #6804, #74446, #77083 ) ) ;
#47708 = CARTESIAN_POINT ( 'NONE',  ( 1.017060367454068803, -0.3162353388693405765, 0.4822834645669290543 ) ) ;
#47709 = CARTESIAN_POINT ( 'NONE',  ( 0.7217847769028878924, -0.3690944881889765550, -0.3153832671262227771 ) ) ;
#47710 = CARTESIAN_POINT ( 'NONE',  ( 0.4653577321740434147, 1.629972608277053148, 2.149112266099304502 ) ) ;
#47711 = CARTESIAN_POINT ( 'NONE',  ( -0.4478287522207295979, 1.694786963789534084, 3.911458005082129041 ) ) ;
#47712 = DIRECTION ( 'NONE',  ( -1.000000000000000000, 1.445602896647338917E-16, -0.000000000000000000 ) ) ;
#47713 = CARTESIAN_POINT ( 'NONE',  ( 0.3917322834645670104, -0.1049643490035303411, -1.298556430446194510 ) ) ;
#47714 = B_SPLINE_CURVE_WITH_KNOTS ( 'NONE', 3,
 ( #6484, #38050, #75963, #38464, #37236, #32154, #76373 ),
 .UNSPECIFIED., .F., .F.,
 ( 4, 3, 4 ),
 ( 1.387778780781445521E-17, 0.001246230184515555910, 0.002492489877932651133 ),
 .UNSPECIFIED. ) ;
#47715 = EDGE_CURVE ( 'NONE', #65845, #71339, #27595, .T. ) ;
#47716 = CARTESIAN_POINT ( 'NONE',  ( 0.3460692066303958092, 0.1998031496062993018, -2.255249343832020692 ) ) ;
#47717 = CARTESIAN_POINT ( 'NONE',  ( -0.9776902887139098386, 0.2952755905511810774, -0.1292274648535930714 ) ) ;
#47718 = CARTESIAN_POINT ( 'NONE',  ( -0.5708661417322828946, 0.1660481256975883668, -0.3530559997133364547 ) ) ;
#47719 = CARTESIAN_POINT ( 'NONE',  ( 1.161417322834646271, 0.1660481256975883668, -0.3530559997133364547 ) ) ;
#47720 = ORIENTED_EDGE ( 'NONE', *, *, #17120, .F. ) ;
#47721 = CARTESIAN_POINT ( 'NONE',  ( 1.253280839895013710, -0.3162353388693405765, 0.4822834645669290543 ) ) ;
#47722 = CARTESIAN_POINT ( 'NONE',  ( -1.313877454013331780, 1.062992125984252079, 0.8967544760595740350 ) ) ;
#47723 = DIRECTION ( 'NONE',  ( -0.000000000000000000, -1.000000000000000000, -0.000000000000000000 ) ) ;
#47724 = CARTESIAN_POINT ( 'NONE',  ( -1.614173228346456712, 0.4405861044731111953, -0.1372047244094478091 ) ) ;
#47725 = CARTESIAN_POINT ( 'NONE',  ( -1.220472440944881054, -0.5511811023622047445, 6.969142054262312111E-17 ) ) ;
#47726 = DIRECTION ( 'NONE',  ( -3.096699300667737957E-16, 1.000000000000000000, -0.000000000000000000 ) ) ;
#47727 = CARTESIAN_POINT ( 'NONE',  ( 0.1837270341207357105, -0.6046776061558809534, -0.2411417322834644161 ) ) ;
#47729 = DIRECTION ( 'NONE',  ( -1.000000000000000000, -3.050063254464715288E-16, 0.000000000000000000 ) ) ;
#47728 = CARTESIAN_POINT ( 'NONE',  ( 1.548556430446194954, 0.2306618581243847221, -0.2411417322834647770 ) ) ;
#47730 = CARTESIAN_POINT ( 'NONE',  ( -1.246719160104986512, -0.004921259842519576551, 0.3153832671262227771 ) ) ;
#47731 = CARTESIAN_POINT ( 'NONE',  ( 0.8595800524934390507, -0.3162353388693405765, 0.4822834645669290543 ) ) ;
#47732 = CARTESIAN_POINT ( 'NONE',  ( 1.423884514435696191, -0.08942795157527998196, 0.3641732283464567121 ) ) ;
#47733 = CARTESIAN_POINT ( 'NONE',  ( -0.3392501089628018329, -0.1958661417322836440, -1.392369135661730262 ) ) ;
#47734 = CARTESIAN_POINT ( 'NONE',  ( -0.8333333333333323711, -0.5511811023622048555, -0.09757992244046775898 ) ) ;
#47735 = CARTESIAN_POINT ( 'NONE',  ( 1.555118110236221041, 0.1660481256975883668, -0.3530559997133364547 ) ) ;
#47736 = CARTESIAN_POINT ( 'NONE',  ( 1.348312163386739426, 0.2755905511811023723, 0.7386866130305692613 ) ) ;
#47737 = CARTESIAN_POINT ( 'NONE',  ( -0.05249343832020938322, -0.6046776061558809534, -0.2411417322834644161 ) ) ;
#47738 = CARTESIAN_POINT ( 'NONE',  ( -0.9448818897637790704, -0.1870078740157480601, -0.3641732283464567677 ) ) ;
#47739 = CARTESIAN_POINT ( 'NONE',  ( -0.2559055118110230564, 0.07958543189024071263, -0.2665933059059888421 ) ) ;
#47740 = CARTESIAN_POINT ( 'NONE',  ( -0.09186351706036689768, 0.05413385826771626580, -0.4176697321401330321 ) ) ;
#47741 = CARTESIAN_POINT ( 'NONE',  ( -1.423884514435694859, -0.08942795157528024563, -0.3641732283464568787 ) ) ;
#47742 = CARTESIAN_POINT ( 'NONE',  ( -0.2867679344610367109, 0.2867679344610365444, -0.4888644601387945876 ) ) ;
#47743 = CARTESIAN_POINT ( 'NONE',  ( 0.3937007874015754361, -0.1870078740157480879, -0.4822834645669291653 ) ) ;
#47744 = LINE ( 'NONE', #35132, #29635 ) ;
#47745 = CARTESIAN_POINT ( 'NONE',  ( 0.1265901696524990294, -0.4724409448818896462, -1.736876640419947604 ) ) ;
#47746 = AXIS2_PLACEMENT_3D ( 'NONE', #28715, #34626, #61533 ) ;
#47747 = CARTESIAN_POINT ( 'NONE',  ( -0.6758530183727028406, -0.6692913385826773087, -0.1292274648535924053 ) ) ;
#47748 = CARTESIAN_POINT ( 'NONE',  ( -0.1377952755905504645, 0.07958543189024085140, 0.2665933059059887866 ) ) ;
#47749 = CARTESIAN_POINT ( 'NONE',  ( -1.377952755905511140, -0.6692913385826771977, 8.415575281601705876E-17 ) ) ;
#47750 = CARTESIAN_POINT ( 'NONE',  ( 0.1902887139107617975, -0.6692913385826773087, -0.1292274648535924053 ) ) ;
#47751 = CARTESIAN_POINT ( 'NONE',  ( 0.5643044619422579178, -0.004921259842519576551, 0.3153832671262227771 ) ) ;
#47752 = VECTOR ( 'NONE', #22961, 39.37007874015748143 ) ;
#47753 = CARTESIAN_POINT ( 'NONE',  ( -0.7939632545931754048, -0.2845877964562159024, 0.3641732283464567677 ) ) ;
#47754 = CARTESIAN_POINT ( 'NONE',  ( -0.9776902887139098386, -0.6692913385826771977, 0.1292274648535927661 ) ) ;
#47755 = CARTESIAN_POINT ( 'NONE',  ( -1.561679790026246017, 0.05413385826771666132, 0.4176697321401328100 ) ) ;
#47756 = CARTESIAN_POINT ( 'NONE',  ( 1.522309711286089939, 0.2306618581243848609, 0.2411417322834645549 ) ) ;
#47757 = DIRECTION ( 'NONE',  ( 1.000000000000000000, 0.000000000000000000, 0.000000000000000000 ) ) ;
#47758 = CARTESIAN_POINT ( 'NONE',  ( 1.069553805774278832, 0.1771653543307087075, -0.09757992244046823083 ) ) ;
#47759 = CARTESIAN_POINT ( 'NONE',  ( 0.7086614173228353852, -0.1870078740157479769, 0.4822834645669291653 ) ) ;
#47760 = DIRECTION ( 'NONE',  ( 1.000000000000000000, 8.462065736472229849E-17, -0.000000000000000000 ) ) ;
#47761 = CARTESIAN_POINT ( 'NONE',  ( 1.259842519685040019, -0.1870078740157479769, 0.3641732283464567677 ) ) ;
#47762 = EDGE_LOOP ( 'NONE', ( #58156, #14291, #21808, #18501 ) ) ;
#47763 = CARTESIAN_POINT ( 'NONE',  ( -0.6955380577427815458, 0.05413385826771666132, 0.4176697321401328100 ) ) ;
#47764 = CARTESIAN_POINT ( 'NONE',  ( -0.3996062992125984925, -0.1070741851644056858, -2.799868766404198794 ) ) ;
#47765 = CARTESIAN_POINT ( 'NONE',  ( -1.364829396325458521, -0.5023911411419708095, 0.1820866141732285504 ) ) ;
#47766 = CARTESIAN_POINT ( 'NONE',  ( -0.5774278215223089816, -0.6046776061558807314, 0.2411417322834647770 ) ) ;
#47767 = CARTESIAN_POINT ( 'NONE',  ( 0.4790026246719167324, -0.05778040916215522460, 0.4822834645669289988 ) ) ;
#47768 = CARTESIAN_POINT ( 'NONE',  ( -1.686351706036744558, 0.1771653543307087075, -0.09757992244046823083 ) ) ;
#47769 = CARTESIAN_POINT ( 'NONE',  ( 0.1070741851644054776, -0.3996062992125984925, -2.051837270341207109 ) ) ;
#47770 = CARTESIAN_POINT ( 'NONE',  ( -1.253280839895012377, -0.05778040916215522460, 0.4822834645669289988 ) ) ;
#47771 = CARTESIAN_POINT ( 'NONE',  ( 0.3871391076115493490, -0.3162353388693405765, 0.4822834645669290543 ) ) ;
#47772 = CARTESIAN_POINT ( 'NONE',  ( -0.1312335958005241554, -0.6046776061558809534, -0.2411417322834644161 ) ) ;
#47773 = CARTESIAN_POINT ( 'NONE',  ( 1.062992125984252745, -0.6692913385826771977, 8.415575281601705876E-17 ) ) ;
#47774 = CARTESIAN_POINT ( 'NONE',  ( 0.01968503937007875723, 2.410722045565656378E-17, -0.1968503937007874405 ) ) ;
#47775 = CARTESIAN_POINT ( 'NONE',  ( 0.3460692066303959202, 0.1998031496062993295, -1.863517060367454015 ) ) ;
#47776 = CARTESIAN_POINT ( 'NONE',  ( -0.2891555358219911054, 0.2891555358219909388, -0.9645669291338583307 ) ) ;
#47777 = CARTESIAN_POINT ( 'NONE',  ( 0.1070741851644053527, 0.3996062992125986590, -2.355643044619422533 ) ) ;
#47778 = CARTESIAN_POINT ( 'NONE',  ( -0.1588297147722000369, -0.2491186766705763000, 0.1541304905092664712 ) ) ;
#47779 = CARTESIAN_POINT ( 'NONE',  ( -0.1771653543307080136, -0.4536011799217367080, 0.2665933059059888421 ) ) ;
#47780 = CARTESIAN_POINT ( 'NONE',  ( -0.2362204724409442680, -0.1870078740157480879, -0.4822834645669291653 ) ) ;
#47781 = CARTESIAN_POINT ( 'NONE',  ( 1.076115485564305141, -0.6046776061558807314, 0.2411417322834647770 ) ) ;
#47782 = CARTESIAN_POINT ( 'NONE',  ( 0.3949938075777409963, 2.418639510665530743E-17, -2.084645669291338876 ) ) ;
#47783 = CARTESIAN_POINT ( 'NONE',  ( 0.01968503937007957949, -0.4536011799217368745, -0.2665933059059886201 ) ) ;
#47784 = CARTESIAN_POINT ( 'NONE',  ( -1.043307086614172041, -0.5400638737290844871, 0.3530559997133364547 ) ) ;
#47785 = CARTESIAN_POINT ( 'NONE',  ( 1.082677165354331228, -0.5400638737290844871, 0.3530559997133364547 ) ) ;
#47786 = CARTESIAN_POINT ( 'NONE',  ( -0.1265901696524986964, -0.4724409448818899238, -1.961942257217847763 ) ) ;
#47787 = CARTESIAN_POINT ( 'NONE',  ( 0.1265901696524989184, 0.4724409448818898127, -2.747375328083989210 ) ) ;
#47788 = ORIENTED_EDGE ( 'NONE', *, *, #4386, .T. ) ;
#47789 = EDGE_LOOP ( 'NONE', ( #19857, #82391, #71939, #12523 ) ) ;
#47790 = CARTESIAN_POINT ( 'NONE',  ( 1.003937007874016185, 0.1660481256975883668, -0.3530559997133364547 ) ) ;
#47791 = CARTESIAN_POINT ( 'NONE',  ( 1.587926509186352142, -0.004921259842519576551, 0.3153832671262227771 ) ) ;
#47793 = CARTESIAN_POINT ( 'NONE',  ( -1.213910761154854745, -0.6692913385826771977, 0.1292274648535927661 ) ) ;
#47792 = CARTESIAN_POINT ( 'NONE',  ( -1.141732283464566011, 0.1771653543307087630, 0.000000000000000000 ) ) ;
#47794 = CARTESIAN_POINT ( 'NONE',  ( -9.594673741351310580E-17, 0.3917322834645669549, -2.284757587105299859 ) ) ;
#47795 = CARTESIAN_POINT ( 'NONE',  ( 1.191441481664479829, -2.398893483443748302E-16, 0.4281993546915529580 ) ) ;
#47796 = CARTESIAN_POINT ( 'NONE',  ( 1.318897637795276356, -0.5400638737290844871, 0.3530559997133364547 ) ) ;
#47797 = CARTESIAN_POINT ( 'NONE',  ( -1.561679790026246017, 0.05413385826771666132, 0.4176697321401328100 ) ) ;
#47798 = CARTESIAN_POINT ( 'NONE',  ( -0.05905511811023545637, -0.5400638737290845981, -0.3530559997133363437 ) ) ;
#47799 = CARTESIAN_POINT ( 'NONE',  ( -0.4330708661417315697, 0.2952755905511811885, 0.000000000000000000 ) ) ;
#47800 = CARTESIAN_POINT ( 'NONE',  ( -1.443569553805773564, 0.2306618581243847221, -0.2411417322834647770 ) ) ;
#47801 = CARTESIAN_POINT ( 'NONE',  ( 0.2867679344610365999, -0.2867679344610365444, -0.3405511811023621549 ) ) ;
#47802 = EDGE_CURVE ( 'NONE', #78367, #28560, #50443, .T. ) ;
#47803 = CARTESIAN_POINT ( 'NONE',  ( 0.006561679790026889343, -0.05778040916215522460, 0.4822834645669289988 ) ) ;
#47804 = CARTESIAN_POINT ( 'NONE',  ( 0.1958661417322834775, 0.3392501089628018884, -2.026246719160105236 ) ) ;
#47805 = CARTESIAN_POINT ( 'NONE',  ( -1.292650918635170010, 0.1771653543307087075, -0.09757992244046823083 ) ) ;
#47806 = EDGE_LOOP ( 'NONE', ( #7018, #82584, #49367, #65553 ) ) ;
#47807 = CARTESIAN_POINT ( 'NONE',  ( -0.1974969037888703871, -0.3420746716998661063, -2.270341207349081181 ) ) ;
#47808 = VERTEX_POINT ( 'NONE', #82459 ) ;
#47809 = CARTESIAN_POINT ( 'NONE',  ( 0.000000000000000000, 0.000000000000000000, -0.1937007874015747588 ) ) ;
#47810 = VECTOR ( 'NONE', #81800, 39.37007874015748143 ) ;
#47811 = CARTESIAN_POINT ( 'NONE',  ( -1.673228346456691717, 0.1660481256975883668, -0.3530559997133364547 ) ) ;
#47812 = CARTESIAN_POINT ( 'NONE',  ( 0.1998031496062994405, -0.3460692066303958092, -0.8792650918635170898 ) ) ;
#47813 = CARTESIAN_POINT ( 'NONE',  ( -1.515748031496062076, 0.1660481256975883668, -0.3530559997133364547 ) ) ;
#47814 = CARTESIAN_POINT ( 'NONE',  ( 1.016821367227983774, 1.537401574803149984, -0.4744094488188970171 ) ) ;
#47815 = CARTESIAN_POINT ( 'NONE',  ( 0.4265091863517068149, 0.2952755905511811885, 0.1292274648535926551 ) ) ;
#47816 = LINE ( 'NONE', #54961, #68686 ) ;
#47817 = CARTESIAN_POINT ( 'NONE',  ( -0.3917322834645671215, 0.1049643490035301469, 0.04002624671916000382 ) ) ;
#47818 = EDGE_CURVE ( 'NONE', #60402, #21709, #71068, .T. ) ;
#47819 = CARTESIAN_POINT ( 'NONE',  ( -0.4396325459317577122, -0.5511811023622048555, -0.09757992244046775898 ) ) ;
#47820 = CARTESIAN_POINT ( 'NONE',  ( -0.8792650918635160906, -0.004921259842519870586, -0.3153832671262229437 ) ) ;
#47821 = CARTESIAN_POINT ( 'NONE',  ( -1.108923884514435132, -0.05778040916215560624, -0.4822834645669293319 ) ) ;
#47822 = CARTESIAN_POINT ( 'NONE',  ( 0.5511811023622054106, -0.1870078740157480879, -0.4822834645669291653 ) ) ;
#47823 = CARTESIAN_POINT ( 'NONE',  ( -0.7086614173228339419, -0.1870078740157479769, 0.4822834645669291653 ) ) ;
#47824 = CARTESIAN_POINT ( 'NONE',  ( 0.5314960629921396951, 2.729373344522950440, -3.881211926161856507 ) ) ;
#47825 = ORIENTED_EDGE ( 'NONE', *, *, #62552, .F. ) ;
#47826 = CARTESIAN_POINT ( 'NONE',  ( -1.581364829396324945, -0.05778040916215560624, -0.4822834645669293319 ) ) ;
#47827 = DIRECTION ( 'NONE',  ( 1.000000000000000000, 0.000000000000000000, 0.000000000000000000 ) ) ;
#47828 = CARTESIAN_POINT ( 'NONE',  ( 0.4091458600556404646, -0.2362204724409448231, -1.364829396325459188 ) ) ;
#47829 = CARTESIAN_POINT ( 'NONE',  ( 1.877461585981321068, 1.092324130688948181, -0.1650676745531886869 ) ) ;
#47830 = CARTESIAN_POINT ( 'NONE',  ( -0.2867679344610364334, -0.2867679344610367109, -0.8385826771653541734 ) ) ;
#47831 = CARTESIAN_POINT ( 'NONE',  ( 0.3917322834645669549, 0.1049643490035304660, -2.571522309711285814 ) ) ;
#47832 = CARTESIAN_POINT ( 'NONE',  ( -0.8005249343832011588, 0.05413385826771626580, -0.4176697321401330321 ) ) ;
#47833 = CARTESIAN_POINT ( 'NONE',  ( 1.561679790026247350, 0.05413385826771626580, -0.4176697321401330321 ) ) ;
#47834 = CARTESIAN_POINT ( 'NONE',  ( -0.3460692066303960313, 0.1998031496062989965, -0.1030183727034120894 ) ) ;
#47836 = CARTESIAN_POINT ( 'NONE',  ( -0.6962418744208963561, -2.294479370626195693E-15, 0.3464511005275217603 ) ) ;
#47835 = CARTESIAN_POINT ( 'NONE',  ( -1.594488188976377563, -0.5400638737290844871, 0.3530559997133364547 ) ) ;
#47837 = CARTESIAN_POINT ( 'NONE',  ( -1.522309711286088607, 0.2306618581243847221, -0.2411417322834647770 ) ) ;
#47838 = CARTESIAN_POINT ( 'NONE',  ( -0.9120734908136475250, 0.2952755905511811885, 0.1292274648535926551 ) ) ;
#47839 = CARTESIAN_POINT ( 'NONE',  ( 0.3917322834645668994, -0.1049643490035303134, -0.03410141912629739008 ) ) ;
#47840 = CARTESIAN_POINT ( 'NONE',  ( 0.5314960629921264834, 0.07958543189024071263, -0.2665933059059888421 ) ) ;
#47841 = CARTESIAN_POINT ( 'NONE',  ( 0.3392501089628018329, 0.1958661417322835607, -0.2158792650918636147 ) ) ;
#47842 = CARTESIAN_POINT ( 'NONE',  ( 0.1771653543307093182, -0.4536011799217368745, -0.2665933059059886201 ) ) ;
#47843 = CARTESIAN_POINT ( 'NONE',  ( 1.010498687664042716, -0.004921259842519870586, -0.3153832671262229437 ) ) ;
#47844 = CARTESIAN_POINT ( 'NONE',  ( 0.9317585301837276734, -0.4281496062992124485, 0.4176697321401328655 ) ) ;
#47845 = CARTESIAN_POINT ( 'NONE',  ( -0.1246719160104980823, -0.5511811023622048555, -0.09757992244046775898 ) ) ;
#47846 = CARTESIAN_POINT ( 'NONE',  ( -0.1958661417322836718, 0.3392501089628017219, -1.737532808398950079 ) ) ;
#47847 = CARTESIAN_POINT ( 'NONE',  ( 1.561679790026247350, -0.4281496062992124485, 0.4176697321401328655 ) ) ;
#47848 = CARTESIAN_POINT ( 'NONE',  ( -1.076115485564303809, -0.5023911411419708095, -0.1820866141732282451 ) ) ;
#47849 = VECTOR ( 'NONE', #12978, 39.37007874015748143 ) ;
#47850 = CARTESIAN_POINT ( 'NONE',  ( -0.2362204724409451284, 0.4091458600556402425, -0.5623359580052492701 ) ) ;
#47851 = VECTOR ( 'NONE', #75394, 39.37007874015748143 ) ;
#47852 = CARTESIAN_POINT ( 'NONE',  ( -0.8923884514435688198, -0.5023911411419708095, 0.1820866141732285504 ) ) ;
#47853 = CARTESIAN_POINT ( 'NONE',  ( 0.03280839895013198948, -0.6692913385826773087, -0.1292274648535924053 ) ) ;
#47854 = CARTESIAN_POINT ( 'NONE',  ( 0.5314960629921264834, 0.07958543189024071263, -0.2665933059059888421 ) ) ;
#47855 = CARTESIAN_POINT ( 'NONE',  ( -0.3018372703412066094, -0.004921259842519576551, 0.3153832671262227771 ) ) ;
#47856 = CARTESIAN_POINT ( 'NONE',  ( -0.5577427821522301654, -0.3162353388693405765, 0.4822834645669290543 ) ) ;
#47857 = DIRECTION ( 'NONE',  ( -3.096699300667737957E-16, 1.000000000000000000, -0.000000000000000000 ) ) ;
#47858 = CARTESIAN_POINT ( 'NONE',  ( 0.000000000000000000, 2.165354330708661568, 0.000000000000000000 ) ) ;
#47859 = CARTESIAN_POINT ( 'NONE',  ( 0.2952755905511819101, 0.1660481256975883668, -0.3530559997133364547 ) ) ;
#47860 = CARTESIAN_POINT ( 'NONE',  ( 0.1070741851644054776, -0.3996062992125984925, -1.736876640419947604 ) ) ;
#47861 = CARTESIAN_POINT ( 'NONE',  ( 1.384514435695538337, -0.6692913385826771977, 0.1292274648535927661 ) ) ;
#47862 = CARTESIAN_POINT ( 'NONE',  ( -0.1443569553805768291, -0.004921259842519576551, 0.3153832671262227771 ) ) ;
#47863 = VECTOR ( 'NONE', #217, 39.37007874015748143 ) ;
#47864 = CARTESIAN_POINT ( 'NONE',  ( -0.2362204724409442680, -0.1870078740157480879, -0.4822834645669291653 ) ) ;
#47865 = CARTESIAN_POINT ( 'NONE',  ( -1.476377952755905110, 0.1660481256975885056, 0.3530559997133364547 ) ) ;
#47866 = CARTESIAN_POINT ( 'NONE',  ( -1.587926509186350810, -0.004921259842519870586, -0.3153832671262229437 ) ) ;
#47867 = CARTESIAN_POINT ( 'NONE',  ( 1.450131233595801428, -0.6692913385826773087, -0.1292274648535924053 ) ) ;
#47868 = CARTESIAN_POINT ( 'NONE',  ( -0.6364829396325453192, -0.2845877964562159024, 0.3641732283464567677 ) ) ;
#47869 = CARTESIAN_POINT ( 'NONE',  ( -0.2925321140481930149, -0.2925321140481933480, -0.1358267716535433156 ) ) ;
#47870 = CARTESIAN_POINT ( 'NONE',  ( -9.787531504996567848E-17, 0.3996062992125986035, -0.4724409448818898127 ) ) ;
#47871 = CARTESIAN_POINT ( 'NONE',  ( -0.1049643490035302301, -0.3917322834645671770, -2.746082307907824038 ) ) ;
#47872 = CARTESIAN_POINT ( 'NONE',  ( 1.515748031496063408, 0.07958543189024085140, 0.2665933059059887866 ) ) ;
#47873 = CARTESIAN_POINT ( 'NONE',  ( 1.240157480314961314, -0.4536011799217367080, 0.2665933059059888421 ) ) ;
#47874 = LINE ( 'NONE', #73578, #40106 ) ;
#47875 = CARTESIAN_POINT ( 'NONE',  ( 0.7939632545931766261, -0.05778040916215522460, 0.4822834645669289988 ) ) ;
#47876 = CARTESIAN_POINT ( 'NONE',  ( -9.674558042662122972E-17, 0.3949938075777409963, -1.021653543307086798 ) ) ;
#47877 = CARTESIAN_POINT ( 'NONE',  ( 1.259842519685040019, -0.1870078740157480601, -0.3641732283464567677 ) ) ;
#47878 = CARTESIAN_POINT ( 'NONE',  ( -0.05249343832020911260, 0.2306618581243848609, 0.2411417322834645549 ) ) ;
#47879 = CARTESIAN_POINT ( 'NONE',  ( -0.4068241469816264999, -0.4281496062992124485, 0.4176697321401328655 ) ) ;
#47880 = CARTESIAN_POINT ( 'NONE',  ( -2.543486866223389153, 2.716535433070866645, -0.5314960629921260393 ) ) ;
#47881 = CARTESIAN_POINT ( 'NONE',  ( -0.4724409448818899238, 0.1265901696524986686, -0.8202099737532806412 ) ) ;
#47882 = CARTESIAN_POINT ( 'NONE',  ( -0.2925321140481932369, 0.2925321140481931814, -2.066929133858267598 ) ) ;
#47883 = CARTESIAN_POINT ( 'NONE',  ( 0.1509186351706042484, -0.2845877964562159024, 0.3641732283464567677 ) ) ;
#47884 = VERTEX_POINT ( 'NONE', #52100 ) ;
#47885 = CARTESIAN_POINT ( 'NONE',  ( 0.3917322834645670104, 0.1049643490035304660, -0.4363710218185846146 ) ) ;
#47886 = ORIENTED_EDGE ( 'NONE', *, *, #8937, .T. ) ;
#47887 = CARTESIAN_POINT ( 'NONE',  ( -0.3149606299212590610, -0.1870078740157479769, 0.4822834645669291653 ) ) ;
#47888 = CARTESIAN_POINT ( 'NONE',  ( 1.043307086614173818, -0.5400638737290845981, -0.3530559997133363437 ) ) ;
#47889 = CARTESIAN_POINT ( 'NONE',  ( 0.3937007874015754361, -0.1870078740157479769, 0.4822834645669291653 ) ) ;
#47890 = CARTESIAN_POINT ( 'NONE',  ( -0.4199475065616791736, -0.5023911411419708095, 0.1820866141732285504 ) ) ;
#47891 = CARTESIAN_POINT ( 'NONE',  ( 0.9776902887139113929, -0.6692913385826773087, -0.1292274648535924053 ) ) ;
#47892 = CARTESIAN_POINT ( 'NONE',  ( -0.7742782152230962556, -0.4281496062992127816, -0.4176697321401328100 ) ) ;
#47893 = CARTESIAN_POINT ( 'NONE',  ( -0.5839895013123351797, 0.2952755905511810774, -0.1292274648535930714 ) ) ;
#47894 = CARTESIAN_POINT ( 'NONE',  ( -0.7152230971128602510, -0.05778040916215560624, -0.4822834645669293319 ) ) ;
#47895 = CARTESIAN_POINT ( 'NONE',  ( 1.325459317585302665, 0.05413385826771626580, -0.4176697321401330321 ) ) ;
#47896 = CARTESIAN_POINT ( 'NONE',  ( 0.8136482939632553313, 0.2306618581243848609, 0.2411417322834645549 ) ) ;
#47897 = CARTESIAN_POINT ( 'NONE',  ( 0.8530183727034128527, -0.4281496062992124485, 0.4176697321401328655 ) ) ;
#47898 = CARTESIAN_POINT ( 'NONE',  ( 0.3917322834645669549, 0.1049643490035304660, -0.4317585301837270628 ) ) ;
#47899 = CARTESIAN_POINT ( 'NONE',  ( 0.1509186351706045259, -0.08942795157528024563, -0.3641732283464568787 ) ) ;
#47900 = ORIENTED_EDGE ( 'NONE', *, *, #29559, .T. ) ;
#47901 = CARTESIAN_POINT ( 'NONE',  ( 0.3949938075777409963, 2.418639510665530435E-17, -1.062992125984251857 ) ) ;
#47902 = VECTOR ( 'NONE', #83139, 39.37007874015748143 ) ;
#47903 = ORIENTED_EDGE ( 'NONE', *, *, #6316, .F. ) ;
#47904 = CARTESIAN_POINT ( 'NONE',  ( -1.043307086614172707, 0.07958543189024071263, -0.2665933059059888421 ) ) ;
#47905 = CIRCLE ( 'NONE', #33143, 2.362204724409449064 ) ;
#47906 = CIRCLE ( 'NONE', #22398, 1.289370078740159409 ) ;
#47907 = CARTESIAN_POINT ( 'NONE',  ( -0.2690288713910754526, -0.6692913385826771977, 0.1292274648535927661 ) ) ;
#47908 = CARTESIAN_POINT ( 'NONE',  ( 1.141392835773558767, 1.405664282898583473, 1.141392835773562764 ) ) ;
#47909 = CARTESIAN_POINT ( 'NONE',  ( -0.3149606299212590610, -0.1870078740157479769, 0.4822834645669291653 ) ) ;
#47910 = CARTESIAN_POINT ( 'NONE',  ( -0.5839895013123351797, 0.2952755905511810774, -0.1292274648535930714 ) ) ;
#47911 = CARTESIAN_POINT ( 'NONE',  ( -1.227034120734907141, -0.6692913385826773087, -0.1292274648535924053 ) ) ;
#47912 = CARTESIAN_POINT ( 'NONE',  ( -1.286089238845143479, -0.6046776061558807314, 0.2411417322834647770 ) ) ;
#47913 = CARTESIAN_POINT ( 'NONE',  ( 0.8136482939632553313, -0.5023911411419708095, -0.1820866141732282451 ) ) ;
#47914 = DIRECTION ( 'NONE',  ( 0.000000000000000000, 0.000000000000000000, 1.000000000000000000 ) ) ;
#47915 = CARTESIAN_POINT ( 'NONE',  ( -0.4724409448818898682, -8.678599364036362592E-17, -0.5885826771653542844 ) ) ;
#47916 = CARTESIAN_POINT ( 'NONE',  ( 0.5774278215223103139, -0.5023911411419708095, -0.1820866141732282451 ) ) ;
#47917 = CARTESIAN_POINT ( 'NONE',  ( 0.2099737532808405305, -0.6046776061558807314, 0.2411417322834647770 ) ) ;
#47918 = CARTESIAN_POINT ( 'NONE',  ( 0.1443569553805781891, 0.05413385826771626580, -0.4176697321401330321 ) ) ;
#47919 = ORIENTED_EDGE ( 'NONE', *, *, #83070, .F. ) ;
#47920 = CARTESIAN_POINT ( 'NONE',  ( 0.1070741851644053527, 0.3996062992125986590, -1.883202099737532276 ) ) ;
#47921 = CARTESIAN_POINT ( 'NONE',  ( -1.614173228346457378, 0.9921945702958913094, 0.1372047244094476981 ) ) ;
#47922 = VERTEX_POINT ( 'NONE', #12168 ) ;
#47923 = CARTESIAN_POINT ( 'NONE',  ( -0.2925321140481932369, 0.2925321140481931259, -1.356299212598425230 ) ) ;
#47924 = CARTESIAN_POINT ( 'NONE',  ( 0.3996062992125984925, 0.1070741851644054637, -0.6738845144356955252 ) ) ;
#47925 = CARTESIAN_POINT ( 'NONE',  ( -0.6167979002624665030, -0.004921259842519576551, 0.3153832671262227771 ) ) ;
#47926 = CARTESIAN_POINT ( 'NONE',  ( -1.010498687664041384, -0.4281496062992127816, -0.4176697321401328100 ) ) ;
#47927 = CARTESIAN_POINT ( 'NONE',  ( -0.1265901696524986964, -0.4724409448818899238, 0.08530183727034119923 ) ) ;
#47928 =( BOUNDED_CURVE ( )  B_SPLINE_CURVE ( 2, ( #65085, #7423, #1123, #9503, #10752, #36005, #3189, #74730, #49450, #62084, #28438, #67174, #29680 ),
 .UNSPECIFIED., .F., .F. ) 
 B_SPLINE_CURVE_WITH_KNOTS ( ( 3, 2, 2, 2, 2, 2, 3 ),
 ( 0.1278765491802554000, 0.1287878787878787845, 0.1325757575757575690, 0.1363636363636363535, 0.1401515151515151381, 0.1439393939393939503, 0.1448507235470174181 ),
 .UNSPECIFIED. ) 
 CURVE ( )  GEOMETRIC_REPRESENTATION_ITEM ( )  RATIONAL_B_SPLINE_CURVE ( ( 0.9875488213027527884, 0.9918020599134683701, 1.000000000000000000, 0.9659258262890683122, 1.000000000000000000, 0.9659258262890683122, 1.000000000000000000, 0.9659258262890683122, 1.000000000000000000, 0.9659258262890683122, 1.000000000000000000, 0.9918020599134675930, 0.9875488213027519002 ) ) 
 REPRESENTATION_ITEM ( '' )  );
#47929 = CARTESIAN_POINT ( 'NONE',  ( -0.3917322834645669549, -0.1049643490035306603, -2.492782152230970993 ) ) ;
#47930 = CARTESIAN_POINT ( 'NONE',  ( 1.548556430446194954, 0.2306618581243847221, -0.2411417322834647770 ) ) ;
#47931 = CARTESIAN_POINT ( 'NONE',  ( 0.9383202099737536495, -0.3162353388693405765, 0.4822834645669290543 ) ) ;
#47932 = VECTOR ( 'NONE', #41827, 39.37007874015748143 ) ;
#47933 = CARTESIAN_POINT ( 'NONE',  ( 0.3477690288713918276, -0.6692913385826773087, -0.1292274648535924053 ) ) ;
#47934 = CARTESIAN_POINT ( 'NONE',  ( -0.6102362204724400829, -0.4536011799217368745, -0.2665933059059886201 ) ) ;
#47935 = CARTESIAN_POINT ( 'NONE',  ( 0.1377952755905518800, -0.5400638737290844871, 0.3530559997133364547 ) ) ;
#47936 = CARTESIAN_POINT ( 'NONE',  ( 0.4724409448818896462, 0.1265901696524990294, -1.776246719160104570 ) ) ;
#47937 = CARTESIAN_POINT ( 'NONE',  ( -0.07217847769028787330, -0.08942795157527998196, 0.3641732283464567121 ) ) ;
#47938 = CARTESIAN_POINT ( 'NONE',  ( -0.3740157480314953431, -0.5400638737290845981, -0.3530559997133363437 ) ) ;
#47939 = CARTESIAN_POINT ( 'NONE',  ( 0.1974969037888704704, 0.3420746716998660508, -1.638451443569553634 ) ) ;
#47940 = CARTESIAN_POINT ( 'NONE',  ( -1.437007874015747477, -0.5400638737290844871, 0.3530559997133364547 ) ) ;
#47941 = CARTESIAN_POINT ( 'NONE',  ( 0.1837270341207354329, 0.1283753931104748280, 0.1820866141732283561 ) ) ;
#47942 = CARTESIAN_POINT ( 'NONE',  ( 1.496062992125985147, -0.1870078740157479769, 0.3641732283464567677 ) ) ;
#47944 = ADVANCED_FACE ( 'NONE', ( #57586 ), #64954, .F. ) ;
#47943 = CARTESIAN_POINT ( 'NONE',  ( -1.253280839895012377, -0.05778040916215522460, 0.4822834645669289988 ) ) ;
#47945 = CARTESIAN_POINT ( 'NONE',  ( -0.7939632545931750718, -0.08942795157528024563, -0.3641732283464568787 ) ) ;
#47946 = CARTESIAN_POINT ( 'NONE',  ( 1.141392835773559211, 0.3937007874015747699, 0.9435581901042713326 ) ) ;
#47947 = CARTESIAN_POINT ( 'NONE',  ( -1.167979002624671470, -0.4281496062992127816, -0.4176697321401328100 ) ) ;
#47948 = CARTESIAN_POINT ( 'NONE',  ( -0.01312335958005186876, 0.05413385826771626580, -0.4176697321401330321 ) ) ;
#47949 = CARTESIAN_POINT ( 'NONE',  ( 0.3460692066303958092, 0.1998031496062993018, -2.412729658792650778 ) ) ;
#47950 = CARTESIAN_POINT ( 'NONE',  ( 0.3917322834645668994, -0.1049643490035303134, -2.396306143535746447 ) ) ;
#47951 = CARTESIAN_POINT ( 'NONE',  ( -1.243977641345850094, 2.305458150815133500, 0.5876520854053413068 ) ) ;
#47952 = CARTESIAN_POINT ( 'NONE',  ( 0.4133858267716541968, 0.07958543189024085140, 0.2665933059059887866 ) ) ;
#47953 = CARTESIAN_POINT ( 'NONE',  ( 1.089238845144357537, -0.4281496062992124485, 0.4176697321401328655 ) ) ;
#47954 = CARTESIAN_POINT ( 'NONE',  ( -1.332020997375327642, -0.2845877964562161244, -0.3641732283464567121 ) ) ;
#47955 = CARTESIAN_POINT ( 'NONE',  ( 1.181102362204725198, -0.1870078740157479769, 0.4822834645669291653 ) ) ;
#47956 = CARTESIAN_POINT ( 'NONE',  ( -1.515748031496062076, 0.07958543189024071263, -0.2665933059059888421 ) ) ;
#47957 = CARTESIAN_POINT ( 'NONE',  ( -0.6627296587926503335, -0.6692913385826771977, 0.1292274648535927661 ) ) ;
#47958 = CARTESIAN_POINT ( 'NONE',  ( 0.2690288713910767848, 0.1771653543307087630, 0.09757992244046791164 ) ) ;
#47959 = CARTESIAN_POINT ( 'NONE',  ( -0.4091458600556402980, -0.2362204724409451284, -0.8398950131233595684 ) ) ;
#47960 = CARTESIAN_POINT ( 'NONE',  ( 0.4724409448818904789, -0.1870078740157479769, 0.3641732283464567677 ) ) ;
#47961 = AXIS2_PLACEMENT_3D ( 'NONE', #70125, #63812, #74091 ) ;
#47962 = CARTESIAN_POINT ( 'NONE',  ( -0.1837270341207340729, 0.2306618581243847221, -0.2411417322834647770 ) ) ;
#47963 = EDGE_CURVE ( 'NONE', #7865, #65743, #77809, .T. ) ;
#47964 = CARTESIAN_POINT ( 'NONE',  ( 4.893765752498283308E-17, -0.3996062992125985480, -0.3129921259842520231 ) ) ;
#47965 = CARTESIAN_POINT ( 'NONE',  ( -1.154855643044618851, -0.6046776061558809534, -0.2411417322834644161 ) ) ;
#47966 = VECTOR ( 'NONE', #74359, 39.37007874015748143 ) ;
#47967 = CARTESIAN_POINT ( 'NONE',  ( 0.3392501089628018884, -0.1958661417322834220, -1.764435695538057791 ) ) ;
#47968 = CARTESIAN_POINT ( 'NONE',  ( 1.115485564304462551, -0.004921259842519576551, 0.3153832671262227771 ) ) ;
#47970 = COLOUR_RGB ( '', 0.09019608, 0.27058824, 0.51372549) ;
#47969 = CARTESIAN_POINT ( 'NONE',  ( -0.1181102362204717315, -0.6692913385826771977, 8.415575281601705876E-17 ) ) ;
#47971 = CIRCLE ( 'NONE', #23762, 0.5118110236220471121 ) ;
#47972 = CARTESIAN_POINT ( 'NONE',  ( -0.3083989501312330295, -0.3162353388693409650, -0.4822834645669289433 ) ) ;
#47973 = CARTESIAN_POINT ( 'NONE',  ( -0.5643044619422565855, -0.3690944881889763329, 0.3153832671262228327 ) ) ;
#47974 = DIRECTION ( 'NONE',  ( 0.000000000000000000, 0.000000000000000000, -1.000000000000000000 ) ) ;
#47975 = CARTESIAN_POINT ( 'NONE',  ( -0.5314960629921250401, 0.07958543189024085140, 0.2665933059059887866 ) ) ;
#47976 = CARTESIAN_POINT ( 'NONE',  ( 0.2559055118110243332, 0.1660481256975885056, 0.3530559997133364547 ) ) ;
#47977 = CARTESIAN_POINT ( 'NONE',  ( -0.6233595800524928121, -0.08942795157527998196, 0.3641732283464567121 ) ) ;
#47978 = CARTESIAN_POINT ( 'NONE',  ( 0.1998031496062994128, -0.3460692066303957537, -0.7985564304461942875 ) ) ;
#47979 = CARTESIAN_POINT ( 'NONE',  ( -1.010498687664041384, 0.05413385826771666132, 0.4176697321401328100 ) ) ;
#47980 = CARTESIAN_POINT ( 'NONE',  ( -3.886287458032462006, 1.724409448818897905, 0.6299212598425196763 ) ) ;
#47981 = ORIENTED_EDGE ( 'NONE', *, *, #54784, .F. ) ;
#47982 = CARTESIAN_POINT ( 'NONE',  ( -1.272965879265091305, -0.3690944881889763329, 0.3153832671262228327 ) ) ;
#47983 = CARTESIAN_POINT ( 'NONE',  ( -0.2559055118110230564, 0.1660481256975883668, -0.3530559997133364547 ) ) ;
#47984 = ADVANCED_FACE ( 'NONE', ( #18485 ), #63093, .F. ) ;
#47985 = CARTESIAN_POINT ( 'NONE',  ( -1.719160104986876103, 0.05413385826771666132, 0.4176697321401328100 ) ) ;
#47986 = CARTESIAN_POINT ( 'NONE',  ( -1.194225721784776262, -0.4281496062992124485, 0.4176697321401328655 ) ) ;
#47987 = CARTESIAN_POINT ( 'NONE',  ( 0.5314960629920851831, 2.755905511811024056, 3.900966923095595451 ) ) ;
#47988 = CARTESIAN_POINT ( 'NONE',  ( 1.272965879265092637, -0.4281496062992127816, -0.4176697321401328100 ) ) ;
#47989 = CARTESIAN_POINT ( 'NONE',  ( 0.8595800524934390507, -0.3162353388693405765, 0.4822834645669290543 ) ) ;
#47990 = CARTESIAN_POINT ( 'NONE',  ( 1.013613127888309595, -4.408777212815537393E-16, -0.4445507791589063395 ) ) ;
#47991 = CARTESIAN_POINT ( 'NONE',  ( 1.473278426072732961, 0.2335363939278403966, 0.2780995266831706725 ) ) ;
#47992 = CARTESIAN_POINT ( 'NONE',  ( 1.555118110236221041, -0.4536011799217367080, 0.2665933059059888421 ) ) ;
#47993 = CARTESIAN_POINT ( 'NONE',  ( -0.3996062992125986035, -0.1070741851644056997, -0.3608923884514435576 ) ) ;
#47994 = ORIENTED_EDGE ( 'NONE', *, *, #80559, .T. ) ;
#47995 = CARTESIAN_POINT ( 'NONE',  ( -0.5314960629921250401, 0.07958543189024085140, 0.2665933059059887866 ) ) ;
#47996 = CARTESIAN_POINT ( 'NONE',  ( -0.2867679344610364334, -0.2867679344610367109, -2.413385826771653253 ) ) ;
#47997 = VERTEX_POINT ( 'NONE', #63501 ) ;
#47998 = CARTESIAN_POINT ( 'NONE',  ( 0.7414698162729663755, -0.6692913385826773087, -0.1292274648535924053 ) ) ;
#47999 = CARTESIAN_POINT ( 'NONE',  ( -0.4133858267716528645, 0.1660481256975883668, -0.3530559997133364547 ) ) ;
#48000 = CARTESIAN_POINT ( 'NONE',  ( -1.181102362204723644, -0.1870078740157479769, 0.4822834645669291653 ) ) ;
#48001 = CARTESIAN_POINT ( 'NONE',  ( 1.318897637795276356, -0.5400638737290844871, 0.3530559997133364547 ) ) ;
#48002 = CARTESIAN_POINT ( 'NONE',  ( -1.102362204724408601, -0.1870078740157480601, -0.3641732283464567677 ) ) ;
#48003 = CARTESIAN_POINT ( 'NONE',  ( -0.1265901696524986964, -0.4724409448818899238, -2.038713910761154491 ) ) ;
#48004 = CARTESIAN_POINT ( 'NONE',  ( 0.2296587926509192634, -0.3162353388693405765, 0.4822834645669290543 ) ) ;
#48005 = CARTESIAN_POINT ( 'NONE',  ( -0.8727034120734901146, -0.3162353388693405765, 0.4822834645669290543 ) ) ;
#48006 = CARTESIAN_POINT ( 'NONE',  ( -9.594673741351310580E-17, 0.3917322834645669549, -1.654836327262780182 ) ) ;
#48007 = CARTESIAN_POINT ( 'NONE',  ( -1.141732283464566011, 0.2952755905511811885, 0.000000000000000000 ) ) ;
#48008 = CARTESIAN_POINT ( 'NONE',  ( 0.2516118885077293643, 1.134065313995062718, -2.808863443762336765 ) ) ;
#48009 = CARTESIAN_POINT ( 'NONE',  ( 0.8333333333333340365, -0.6692913385826771977, 0.1292274648535927661 ) ) ;
#48010 = CARTESIAN_POINT ( 'NONE',  ( 1.417322834645670104, -0.1870078740157480601, -0.3641732283464567677 ) ) ;
#48011 = ORIENTED_EDGE ( 'NONE', *, *, #75818, .F. ) ;
#48012 = CARTESIAN_POINT ( 'NONE',  ( -0.2867679344610365444, -0.2867679344610367664, -2.732958948327771420 ) ) ;
#48013 = CARTESIAN_POINT ( 'NONE',  ( -0.4396325459317577122, -0.6692913385826773087, -0.1292274648535924053 ) ) ;
#48014 = ORIENTED_EDGE ( 'NONE', *, *, #35272, .F. ) ;
#48015 = CARTESIAN_POINT ( 'NONE',  ( 0.5118110236220478892, 0.1771653543307087630, 0.000000000000000000 ) ) ;
#48016 = CARTESIAN_POINT ( 'NONE',  ( -1.115485564304461219, -0.4281496062992124485, 0.4176697321401328655 ) ) ;
#48017 = CARTESIAN_POINT ( 'NONE',  ( 0.9514435695538062676, -0.05778040916215522460, 0.4822834645669289988 ) ) ;
#48018 = CARTESIAN_POINT ( 'NONE',  ( 1.036745406824147508, -0.4281496062992127816, -0.4176697321401328100 ) ) ;
#48019 = CARTESIAN_POINT ( 'NONE',  ( -0.2690288713910754526, 0.2952755905511810774, -0.1292274648535930714 ) ) ;
#48020 = CARTESIAN_POINT ( 'NONE',  ( 0.3917322834645670659, -0.1049643490035303273, -1.368129552002311788 ) ) ;
#48021 = CARTESIAN_POINT ( 'NONE',  ( -0.5971128608923877978, -0.6692913385826773087, -0.1292274648535924053 ) ) ;
#48022 = CARTESIAN_POINT ( 'NONE',  ( -0.3917322834645669549, -0.1049643490035306603, -2.177821522309711266 ) ) ;
#48023 = CARTESIAN_POINT ( 'NONE',  ( -1.423884514435694859, -0.3162353388693405765, 0.4822834645669290543 ) ) ;
#48024 = CARTESIAN_POINT ( 'NONE',  ( -0.7020997375328074108, -0.05778040916215522460, 0.4822834645669289988 ) ) ;
#48025 = CARTESIAN_POINT ( 'NONE',  ( -0.3280839895013117347, -0.004921259842519870586, -0.3153832671262229437 ) ) ;
#48026 = CARTESIAN_POINT ( 'NONE',  ( 1.338582677165355062, -0.1870078740157479769, 0.4822834645669291653 ) ) ;
#48027 = CARTESIAN_POINT ( 'NONE',  ( 1.627296587926509996, -0.6046776061558807314, 0.2411417322834647770 ) ) ;
#48028 = CARTESIAN_POINT ( 'NONE',  ( -1.108923884514435132, -0.3162353388693405765, 0.4822834645669290543 ) ) ;
#48029 = CARTESIAN_POINT ( 'NONE',  ( 0.1998031496062992463, 0.3460692066303959202, 0.09383202099737532331 ) ) ;
#48030 = CARTESIAN_POINT ( 'NONE',  ( 0.7020997375328090762, -0.05778040916215560624, -0.4822834645669293319 ) ) ;
#48031 = CARTESIAN_POINT ( 'NONE',  ( 0.2925321140481932369, 0.2925321140481932369, -1.870078740157480546 ) ) ;
#48032 = CARTESIAN_POINT ( 'NONE',  ( 1.594488188976378673, 0.1660481256975885056, 0.3530559997133364547 ) ) ;
#48033 = VECTOR ( 'NONE', #40399, 39.37007874015748143 ) ;
#48034 = CARTESIAN_POINT ( 'NONE',  ( 0.006561679790026889343, -0.3162353388693409650, -0.4822834645669289433 ) ) ;
#48035 = CARTESIAN_POINT ( 'NONE',  ( -1.141732283464566011, 0.1771653543307087630, 0.000000000000000000 ) ) ;
#48036 = CARTESIAN_POINT ( 'NONE',  ( 0.4002624671916016896, -0.08942795157527998196, 0.3641732283464567121 ) ) ;
#48037 = CARTESIAN_POINT ( 'NONE',  ( 0.4724409448818896462, 0.1265901696524990294, -0.6738845144356955252 ) ) ;
#48038 = CARTESIAN_POINT ( 'NONE',  ( 1.364829396325460076, 0.1283753931104748280, 0.1820866141732283561 ) ) ;
#48039 = CARTESIAN_POINT ( 'NONE',  ( 0.7480314960629927956, -0.6692913385826771977, 8.415575281601705876E-17 ) ) ;
#48040 = CARTESIAN_POINT ( 'NONE',  ( 0.1058382717557499880, 0.3949938075777409408, -0.7001312335958006505 ) ) ;
#48041 = PRODUCT_DEFINITION_SHAPE ( 'NONE', 'NONE',  #83314 ) ;
#48042 = CARTESIAN_POINT ( 'NONE',  ( -0.2427821522309703550, -0.05778040916215560624, -0.4822834645669293319 ) ) ;
#48043 = DIRECTION ( 'NONE',  ( 1.047444401652940007E-14, 0.000000000000000000, -1.000000000000000000 ) ) ;
#48044 = CARTESIAN_POINT ( 'NONE',  ( 1.450131233595801428, 0.1771653543307087630, 0.09757992244046791164 ) ) ;
#48045 = CARTESIAN_POINT ( 'NONE',  ( -0.5380577427821514602, -0.4281496062992127816, -0.4176697321401328100 ) ) ;
#48046 = CARTESIAN_POINT ( 'NONE',  ( 0.2891555358219910499, -0.2891555358219909944, -0.6476377952755905110 ) ) ;
#48047 = CARTESIAN_POINT ( 'NONE',  ( 1.443569553805774897, -0.6046776061558809534, -0.2411417322834644161 ) ) ;
#48048 = CARTESIAN_POINT ( 'NONE',  ( -0.01968503937007793844, -0.5400638737290844871, 0.3530559997133364547 ) ) ;
#48049 = CARTESIAN_POINT ( 'NONE',  ( 0.4068241469816281097, -0.004921259842519576551, 0.3153832671262227771 ) ) ;
#48050 = DIRECTION ( 'NONE',  ( -0.000000000000000000, -1.000000000000000000, -0.000000000000000000 ) ) ;
#48051 = CARTESIAN_POINT ( 'NONE',  ( 0.03937007874015833325, -0.5511811023622047445, 6.969142054262312111E-17 ) ) ;
#48052 = CARTESIAN_POINT ( 'NONE',  ( -1.489501312335957062, -0.05778040916215522460, 0.4822834645669289988 ) ) ;
#48053 = CARTESIAN_POINT ( 'NONE',  ( -0.1998031496062991630, -0.3460692066303959202, -1.244750656167979086 ) ) ;
#48054 = CARTESIAN_POINT ( 'NONE',  ( 0.8595800524934390507, -0.3162353388693405765, 0.4822834645669290543 ) ) ;
#48055 = CARTESIAN_POINT ( 'NONE',  ( -0.1958661417322836718, 0.3392501089628017219, -0.9501312335958004285 ) ) ;
#48056 = CARTESIAN_POINT ( 'NONE',  ( 1.666666666666667185, -0.004921259842519576551, 0.3153832671262227771 ) ) ;
#48057 = CARTESIAN_POINT ( 'NONE',  ( -1.291027602697912169, 0.000000000000000000, 0.5830028338522510456 ) ) ;
#48058 = CARTESIAN_POINT ( 'NONE',  ( 0.02624671916010564918, 0.1283753931104748280, 0.1820866141732283561 ) ) ;
#48059 = CARTESIAN_POINT ( 'NONE',  ( 0.07217847769028949700, -0.3162353388693405765, 0.4822834645669290543 ) ) ;
#48060 = CARTESIAN_POINT ( 'NONE',  ( 1.437007874015748810, -0.4536011799217368745, -0.2665933059059886201 ) ) ;
#48061 = CARTESIAN_POINT ( 'NONE',  ( -1.443569553805773564, -0.5023911411419708095, 0.1820866141732285504 ) ) ;
#48062 = CARTESIAN_POINT ( 'NONE',  ( -1.548556430446193399, 0.2306618581243848609, 0.2411417322834645549 ) ) ;
#48063 = CARTESIAN_POINT ( 'NONE',  ( 0.3543307086614181922, -0.6692913385826771977, 8.415575281601705876E-17 ) ) ;
#48064 = CARTESIAN_POINT ( 'NONE',  ( 1.095800524934383846, -0.05778040916215560624, -0.4822834645669293319 ) ) ;
#48065 = DIRECTION ( 'NONE',  ( 0.000000000000000000, 0.000000000000000000, 1.000000000000000000 ) ) ;
#48066 = CARTESIAN_POINT ( 'NONE',  ( 0.5118110236220478892, 0.2952755905511811885, 0.000000000000000000 ) ) ;
#48067 = CARTESIAN_POINT ( 'NONE',  ( 1.240157480314961314, 0.1660481256975883668, -0.3530559997133364547 ) ) ;
#48068 = CARTESIAN_POINT ( 'NONE',  ( 1.017060367454068803, -0.3162353388693405765, 0.4822834645669290543 ) ) ;
#48069 = CARTESIAN_POINT ( 'NONE',  ( 0.3458507752293908943, -0.3458507752293908943, -0.3326771653543306728 ) ) ;
#48070 = CARTESIAN_POINT ( 'NONE',  ( 0.9055118110236227702, 0.1771653543307087630, 0.000000000000000000 ) ) ;
#48071 = CARTESIAN_POINT ( 'NONE',  ( 1.469816272965879911, -0.6046776061558807314, 0.2411417322834647770 ) ) ;
#48072 = CARTESIAN_POINT ( 'NONE',  ( -0.9908136482939626788, 0.1771653543307087630, 0.09757992244046791164 ) ) ;
#48073 = CARTESIAN_POINT ( 'NONE',  ( 0.3805774278215230400, -0.004921259842519870586, -0.3153832671262229437 ) ) ;
#48074 = CARTESIAN_POINT ( 'NONE',  ( 0.1181102362204730916, 0.2952755905511811885, 0.000000000000000000 ) ) ;
#48075 = CARTESIAN_POINT ( 'NONE',  ( 0.6364829396325465405, -0.05778040916215522460, 0.4822834645669289988 ) ) ;
#48076 = CARTESIAN_POINT ( 'NONE',  ( -0.4199475065616791736, -0.6046776061558807314, 0.2411417322834647770 ) ) ;
#48077 = CARTESIAN_POINT ( 'NONE',  ( 0.1246719160104994284, -0.5511811023622046335, 0.09757992244046803654 ) ) ;
#48078 = CARTESIAN_POINT ( 'NONE',  ( 0.7414698162729663755, -0.6692913385826773087, -0.1292274648535924053 ) ) ;
#48079 = CARTESIAN_POINT ( 'NONE',  ( -1.220472440944878834, 0.8346805926620878280, -0.5309055118110234117 ) ) ;
#48080 = CARTESIAN_POINT ( 'NONE',  ( -0.8661417322834640276, -0.1870078740157480879, -0.4822834645669291653 ) ) ;
#48082 = CARTESIAN_POINT ( 'NONE',  ( 0.000000000000000000, 2.755905511811024056, 0.000000000000000000 ) ) ;
#48081 = CARTESIAN_POINT ( 'NONE',  ( 1.586688153636164111, 1.522296263979924902, 0.1275903502784767052 ) ) ;
#48083 = FACE_OUTER_BOUND ( 'NONE', #18628, .T. ) ;
#48084 = VECTOR ( 'NONE', #66521, 39.37007874015748854 ) ;
#48085 = CARTESIAN_POINT ( 'NONE',  ( -0.8661417322834640276, -0.1870078740157479769, 0.4822834645669291653 ) ) ;
#48086 = CARTESIAN_POINT ( 'NONE',  ( -0.6561679790026240244, -0.6046776061558807314, 0.2411417322834647770 ) ) ;
#48087 = EDGE_CURVE ( 'NONE', #71224, #21828, #67860, .T. ) ;
#48088 = CARTESIAN_POINT ( 'NONE',  ( -0.3458507752293906723, -0.3458507752293910609, 0.09842519685039372024 ) ) ;
#48089 = CARTESIAN_POINT ( 'NONE',  ( -0.3949938075777411628, 0.1058382717557497937, -2.237532808398950301 ) ) ;
#48090 = ORIENTED_EDGE ( 'NONE', *, *, #79779, .T. ) ;
#48091 = CARTESIAN_POINT ( 'NONE',  ( 0.6233595800524942554, -0.08942795157528024563, -0.3641732283464568787 ) ) ;
#48092 = CARTESIAN_POINT ( 'NONE',  ( -9.594673741351313045E-17, 0.3917322834645670104, -0.9370078740157480324 ) ) ;
#48093 = CARTESIAN_POINT ( 'NONE',  ( 1.207349081364829990, -0.6046776061558809534, -0.2411417322834644161 ) ) ;
#48094 = DIRECTION ( 'NONE',  ( 1.000000000000000000, 0.000000000000000000, 3.455050906509825972E-15 ) ) ;
#48095 = EDGE_CURVE ( 'NONE', #32357, #24500, #17975, .T. ) ;
#48096 = CARTESIAN_POINT ( 'NONE',  ( -1.443569553805773564, -0.5023911411419708095, 0.1820866141732285504 ) ) ;
#48097 = CARTESIAN_POINT ( 'NONE',  ( 1.443569553805774897, -0.6046776061558809534, -0.2411417322834644161 ) ) ;
#48098 = CARTESIAN_POINT ( 'NONE',  ( -1.614173228346456268, -0.6692913385826771977, 8.415575281601705876E-17 ) ) ;
#48099 = CARTESIAN_POINT ( 'NONE',  ( 0.2821522309711292364, 0.2952755905511810774, -0.1292274648535930714 ) ) ;
#48100 = CARTESIAN_POINT ( 'NONE',  ( -0.3392501089628018329, -0.1958661417322836440, -0.2900069309373210502 ) ) ;
#48101 = B_SPLINE_CURVE_WITH_KNOTS ( 'NONE', 3,
 ( #37809, #11750, #62248, #31077 ),
 .UNSPECIFIED., .F., .F.,
 ( 4, 4 ),
 ( 7.561484326770510175E-18, 0.0007402370886711638707 ),
 .UNSPECIFIED. ) ;
#48102 = CARTESIAN_POINT ( 'NONE',  ( -0.04593175853018302557, 0.2952755905511811885, 0.1292274648535926551 ) ) ;
#48104 = CARTESIAN_POINT ( 'NONE',  ( -0.8923884514435688198, 0.1283753931104746893, -0.1820866141732285504 ) ) ;
#48103 = SHAPE_REPRESENTATION ( 'Reversible Hardened Steel Jaws', ( #22098 ), #14119 ) ;
#48105 = CARTESIAN_POINT ( 'NONE',  ( 1.003937007874016185, 0.1660481256975883668, -0.3530559997133364547 ) ) ;
#48106 = CARTESIAN_POINT ( 'NONE',  ( -0.04593175853018302557, -0.6692913385826773087, -0.1292274648535924053 ) ) ;
#48107 = CARTESIAN_POINT ( 'NONE',  ( -0.4724409448818899238, 0.1265901696524986964, -0.03280839895013123314 ) ) ;
#48108 = CARTESIAN_POINT ( 'NONE',  ( 0.4091458600556403535, 0.2362204724409449896, -1.076115485564304475 ) ) ;
#48109 = CARTESIAN_POINT ( 'NONE',  ( 0.1049643490035303967, 0.3917322834645670659, -1.722460260663728926 ) ) ;
#48110 = CARTESIAN_POINT ( 'NONE',  ( 0.6496062992125991586, -0.5400638737290845981, -0.3530559997133363437 ) ) ;
#48111 = CARTESIAN_POINT ( 'NONE',  ( 0.06561679790026316017, 0.05413385826771626580, -0.4176697321401330321 ) ) ;
#48112 = CARTESIAN_POINT ( 'NONE',  ( -1.141732283464566011, 0.2952755905511811885, 0.000000000000000000 ) ) ;
#48113 = CARTESIAN_POINT ( 'NONE',  ( 1.187664041994751285, -0.3162353388693409650, -0.4822834645669289433 ) ) ;
#48114 = CARTESIAN_POINT ( 'NONE',  ( 0.6036745406824154392, 0.2306618581243847221, -0.2411417322834647770 ) ) ;
#48115 = CARTESIAN_POINT ( 'NONE',  ( -0.3917322834645669549, -0.1049643490035306603, -0.9179790026246721357 ) ) ;
#48116 = CARTESIAN_POINT ( 'NONE',  ( -0.4330708661417315697, 0.2952755905511811885, 0.000000000000000000 ) ) ;
#48117 = CARTESIAN_POINT ( 'NONE',  ( 0.6692913385826778638, -0.6692913385826771977, 8.415575281601705876E-17 ) ) ;
#48118 = CARTESIAN_POINT ( 'NONE',  ( -0.05249343832020911260, 0.2306618581243848609, 0.2411417322834645549 ) ) ;
#48119 = CARTESIAN_POINT ( 'NONE',  ( 0.7874015748031503170, -0.1870078740157480601, -0.3641732283464567677 ) ) ;
#48120 = CARTESIAN_POINT ( 'NONE',  ( -1.312335958005248715, -0.6046776061558809534, -0.2411417322834644161 ) ) ;
#48121 = CARTESIAN_POINT ( 'NONE',  ( -0.03416814150274047335, 1.063911309852950682, -2.873163370116321946 ) ) ;
#48122 = CARTESIAN_POINT ( 'NONE',  ( 0.3083989501312343062, -0.3162353388693405765, 0.4822834645669290543 ) ) ;
#48123 = CARTESIAN_POINT ( 'NONE',  ( -0.03443470937339727228, 0.2755905511811023723, -1.417921404050779710 ) ) ;
#48124 = EDGE_CURVE ( 'NONE', #32589, #13567, #4483, .T. ) ;
#48125 = CARTESIAN_POINT ( 'NONE',  ( -0.3392501089628019995, 0.1958661417322832277, -2.538057742782152015 ) ) ;
#48126 = VERTEX_POINT ( 'NONE', #7088 ) ;
#48127 = ORIENTED_EDGE ( 'NONE', *, *, #79898, .T. ) ;
#48128 = CARTESIAN_POINT ( 'NONE',  ( 1.332020997375329197, -0.3162353388693405765, 0.4822834645669290543 ) ) ;
#48129 = CARTESIAN_POINT ( 'NONE',  ( 0.7283464566929140904, -0.4536011799217368745, -0.2665933059059886201 ) ) ;
#48130 = DIRECTION ( 'NONE',  ( -1.000000000000000000, -8.805702923740138355E-17, 0.000000000000000000 ) ) ;
#48131 = CARTESIAN_POINT ( 'NONE',  ( 0.4724409448818899238, -0.1265901696524985298, -0.03083989501312338691 ) ) ;
#48132 = CARTESIAN_POINT ( 'NONE',  ( -1.313877454013331780, 0.2755905511811023723, 0.6792347910202041206 ) ) ;
#48133 = CARTESIAN_POINT ( 'NONE',  ( 0.1049643490035304938, -0.3917322834645669549, -1.429790026246719359 ) ) ;
#48134 = ADVANCED_FACE ( 'NONE', ( #64331 ), #82351, .T. ) ;
#48135 = CARTESIAN_POINT ( 'NONE',  ( -0.1070741851644056997, 0.3996062992125984925, -2.445538057742782101 ) ) ;
#48136 = CARTESIAN_POINT ( 'NONE',  ( -0.7808398950131222316, -0.3162353388693409650, -0.4822834645669289433 ) ) ;
#48137 = CARTESIAN_POINT ( 'NONE',  ( -0.7480314960629914633, 0.2952755905511811885, 0.000000000000000000 ) ) ;
#48138 = CARTESIAN_POINT ( 'NONE',  ( 0.7611548556430451917, -0.6046776061558807314, 0.2411417322834647770 ) ) ;
#48139 = ORIENTED_EDGE ( 'NONE', *, *, #49631, .T. ) ;
#48140 = CARTESIAN_POINT ( 'NONE',  ( 1.528871391076116026, -0.6692913385826773087, -0.1292274648535924053 ) ) ;
#48141 = CARTESIAN_POINT ( 'NONE',  ( 1.646981627296588035, -0.2845877964562159024, 0.3641732283464567677 ) ) ;
#48142 = APPLICATION_PROTOCOL_DEFINITION ( 'draft international standard', 'automotive_design', 1998, #75624 ) ;
#48143 = CARTESIAN_POINT ( 'NONE',  ( 0.000000000000000000, 2.755905511811024056, 0.000000000000000000 ) ) ;
#48144 = CARTESIAN_POINT ( 'NONE',  ( 0.3911666210184634451, 0.1216921365961784601, -1.934761428466221123 ) ) ;
#48145 = CARTESIAN_POINT ( 'NONE',  ( -1.279527559055116948, 0.07958543189024071263, -0.2665933059059888421 ) ) ;
#48146 = ADVANCED_FACE ( 'NONE', ( #17893 ), #50674, .F. ) ;
#48147 = CARTESIAN_POINT ( 'NONE',  ( 0.1049643490035303689, 0.3917322834645670104, 0.01443569553805778768 ) ) ;
#48148 = CARTESIAN_POINT ( 'NONE',  ( 0.2296587926509192634, -0.3162353388693405765, 0.4822834645669290543 ) ) ;
#48149 = CIRCLE ( 'NONE', #52159, 0.5120078740157480990 ) ;
#48151 = LINE ( 'NONE', #73846, #66805 ) ;
#48150 = CARTESIAN_POINT ( 'NONE',  ( 1.679790026246720025, 0.2306618581243848609, 0.2411417322834645549 ) ) ;
#48152 = CARTESIAN_POINT ( 'NONE',  ( -1.003937007874015297, -0.4536011799217368745, -0.2665933059059886201 ) ) ;
#48153 = CARTESIAN_POINT ( 'NONE',  ( 0.2755905511811031494, 0.2952755905511811885, 0.000000000000000000 ) ) ;
#48154 = CARTESIAN_POINT ( 'NONE',  ( 1.148293963254593653, 0.1771653543307087075, -0.09757992244046823083 ) ) ;
#48155 = CARTESIAN_POINT ( 'NONE',  ( 0.3917322834645668994, -0.1049643490035303134, -1.136463623850706650 ) ) ;
#48156 = CARTESIAN_POINT ( 'NONE',  ( -1.161417322834644716, -0.4536011799217368745, -0.2665933059059886201 ) ) ;
#48157 = CARTESIAN_POINT ( 'NONE',  ( 1.391076115485564868, 0.2306618581243847221, -0.2411417322834647770 ) ) ;
#48158 = CARTESIAN_POINT ( 'NONE',  ( 0.3120460330268322036, 1.650912851539013682, 0.02472967731811865147 ) ) ;
#48159 = CARTESIAN_POINT ( 'NONE',  ( -0.05905511811023545637, -0.5400638737290845981, -0.3530559997133363437 ) ) ;
#48160 = CARTESIAN_POINT ( 'NONE',  ( -1.253280839895012377, -0.2845877964562161244, -0.3641732283464567121 ) ) ;
#48161 = CARTESIAN_POINT ( 'NONE',  ( -0.4790026246719154557, -0.2845877964562159024, 0.3641732283464567677 ) ) ;
#48162 = CARTESIAN_POINT ( 'NONE',  ( -0.8595800524934373854, -0.3162353388693409650, -0.4822834645669289433 ) ) ;
#48163 = CARTESIAN_POINT ( 'NONE',  ( -1.371391076115484609, -0.5511811023622046335, 0.09757992244046803654 ) ) ;
#48164 = CARTESIAN_POINT ( 'NONE',  ( -0.3392501089628019995, 0.1958661417322831999, -0.3379458249681908666 ) ) ;
#48165 = CARTESIAN_POINT ( 'NONE',  ( 0.4133858267716541968, -0.5400638737290845981, -0.3530559997133363437 ) ) ;
#48166 = DIRECTION ( 'NONE',  ( -0.000000000000000000, 1.000000000000000000, -0.000000000000000000 ) ) ;
#48167 = CARTESIAN_POINT ( 'NONE',  ( -0.4091458600556405756, 0.2362204724409446288, -1.520341207349081181 ) ) ;
#48168 = CARTESIAN_POINT ( 'NONE',  ( -1.062992125984250968, 0.2952755905511811885, 0.000000000000000000 ) ) ;
#48169 = CARTESIAN_POINT ( 'NONE',  ( -0.4133858267716528645, 0.07958543189024071263, -0.2665933059059888421 ) ) ;
#48170 = CARTESIAN_POINT ( 'NONE',  ( 0.7981007675632553200, -1.206088964116209378E-16, 0.4118477457932991359 ) ) ;
#48171 = CARTESIAN_POINT ( 'NONE',  ( -0.04593175853018302557, 0.2952755905511811885, 0.1292274648535926551 ) ) ;
#48172 = CARTESIAN_POINT ( 'NONE',  ( 0.3018372703412079971, -0.004921259842519870586, -0.3153832671262229437 ) ) ;
#48173 = CARTESIAN_POINT ( 'NONE',  ( -0.5577427821522301654, -0.08942795157528024563, -0.3641732283464568787 ) ) ;
#48174 = CARTESIAN_POINT ( 'NONE',  ( -1.620734908136482577, -0.6692913385826773087, -0.1292274648535924053 ) ) ;
#48175 = CARTESIAN_POINT ( 'NONE',  ( -1.371391076115484831, 0.2952755905511810774, -0.1292274648535930714 ) ) ;
#48176 = CARTESIAN_POINT ( 'NONE',  ( 1.338582677165355062, -0.1870078740157479769, 0.4822834645669291653 ) ) ;
#48177 = CARTESIAN_POINT ( 'NONE',  ( 0.4477177017962634675, 1.379801381128189064, 2.114025566600534312 ) ) ;
#48178 = CARTESIAN_POINT ( 'NONE',  ( 0.9448818897637802916, -0.1870078740157480601, -0.3641732283464567677 ) ) ;
#48179 = CARTESIAN_POINT ( 'NONE',  ( 0.8202099737532814183, -0.6692913385826773087, -0.1292274648535924053 ) ) ;
#48180 = CARTESIAN_POINT ( 'NONE',  ( -0.01000891935578489267, 8.471767977567108961E-16, -0.4445507791589058955 ) ) ;
#48181 = CARTESIAN_POINT ( 'NONE',  ( 1.574803149606299746, -0.1870078740157479769, 0.3641732283464567677 ) ) ;
#48182 = ORIENTED_EDGE ( 'NONE', *, *, #42744, .F. ) ;
#48183 = CARTESIAN_POINT ( 'NONE',  ( -1.305774278215222184, 0.2952755905511811885, 0.1292274648535926551 ) ) ;
#48184 = CARTESIAN_POINT ( 'NONE',  ( -0.8792650918635160906, -0.4281496062992124485, 0.4176697321401328655 ) ) ;
#48185 = CARTESIAN_POINT ( 'NONE',  ( 0.2755905511811031494, -0.6692913385826771977, 8.415575281601705876E-17 ) ) ;
#48186 = CARTESIAN_POINT ( 'NONE',  ( -1.358267716535432434, 0.07958543189024071263, -0.2665933059059888421 ) ) ;
#48187 = CARTESIAN_POINT ( 'NONE',  ( 0.1998031496062994128, -0.3460692066303957537, -2.058398950131233640 ) ) ;
#48188 = CARTESIAN_POINT ( 'NONE',  ( 1.541994750656168645, -0.5511811023622046335, 0.09757992244046803654 ) ) ;
#48189 = CARTESIAN_POINT ( 'NONE',  ( 0.2427821522309719648, -0.05778040916215522460, 0.4822834645669289988 ) ) ;
#48190 = CARTESIAN_POINT ( 'NONE',  ( 0.7742782152230978099, -0.4281496062992124485, 0.4176697321401328655 ) ) ;
#48192 = EDGE_CURVE ( 'NONE', #33111, #31856, #47714, .T. ) ;
#48191 = LINE ( 'NONE', #24064, #11690 ) ;
#48193 = CARTESIAN_POINT ( 'NONE',  ( 0.3996062992125986035, 0.1070741851644054776, -1.856955380577427928 ) ) ;
#48194 = CARTESIAN_POINT ( 'NONE',  ( 0.1974969037888706369, -0.3420746716998659953, -0.8792650918635170898 ) ) ;
#48195 = CARTESIAN_POINT ( 'NONE',  ( 0.3996062992125986035, 0.1070741851644054776, -2.644356955380577912 ) ) ;
#48196 = CARTESIAN_POINT ( 'NONE',  ( -2.516666444179625373, 2.742784451071572427, 0.5314960629921260393 ) ) ;
#48197 = APPLICATION_CONTEXT ( 'automotive_design' ) ;
#48198 = CARTESIAN_POINT ( 'NONE',  ( -0.2867679344610366554, 0.2867679344610365444, -0.3267716535433070058 ) ) ;
#48199 = CARTESIAN_POINT ( 'NONE',  ( 0.04593175853018440641, 0.1771653543307087075, -0.09757992244046823083 ) ) ;
#48200 = CARTESIAN_POINT ( 'NONE',  ( -0.2821522309711278487, 0.2952755905511811885, 0.1292274648535926551 ) ) ;
#48201 = CARTESIAN_POINT ( 'NONE',  ( 0.9251968503937015864, -0.5400638737290844871, 0.3530559997133364547 ) ) ;
#48202 = CARTESIAN_POINT ( 'NONE',  ( 0.1974969037888704704, 0.3420746716998660508, -2.268372703412073754 ) ) ;
#48203 = CARTESIAN_POINT ( 'NONE',  ( -0.05249343832020911260, 0.1283753931104748280, 0.1820866141732283561 ) ) ;
#48204 = CARTESIAN_POINT ( 'NONE',  ( -1.017060367454067249, -0.05778040916215522460, 0.4822834645669289988 ) ) ;
#48205 = CARTESIAN_POINT ( 'NONE',  ( 1.141732283464567566, 0.2952755905511811885, 0.000000000000000000 ) ) ;
#48206 = CARTESIAN_POINT ( 'NONE',  ( 0.3458507752293908943, -0.3458507752293908943, -2.460629921259842146 ) ) ;
#48207 = CARTESIAN_POINT ( 'NONE',  ( -0.3460692066303960868, 0.1998031496062990242, -1.916010498687664043 ) ) ;
#48208 = CARTESIAN_POINT ( 'NONE',  ( -1.559171609364246924, 0.3937007874015748254, 0.2406134192599649890 ) ) ;
#48209 = ORIENTED_EDGE ( 'NONE', *, *, #49907, .T. ) ;
#48210 = ORIENTED_EDGE ( 'NONE', *, *, #82633, .F. ) ;
#48211 = CARTESIAN_POINT ( 'NONE',  ( 0.8727034120734912248, -0.3162353388693409650, -0.4822834645669289433 ) ) ;
#48212 = CARTESIAN_POINT ( 'NONE',  ( -1.712598425196849572, 0.1660481256975885056, 0.3530559997133364547 ) ) ;
#48214 = CARTESIAN_POINT ( 'NONE',  ( -1.456692913385826182, 0.2952755905511811885, 0.000000000000000000 ) ) ;
#48213 = CARTESIAN_POINT ( 'NONE',  ( -1.332020997375327642, -0.08942795157527998196, 0.3641732283464567121 ) ) ;
#48215 = CARTESIAN_POINT ( 'NONE',  ( 0.1958661417322836162, -0.3392501089628018329, -2.691581734086927469 ) ) ;
#48216 = DIRECTION ( 'NONE',  ( 0.000000000000000000, 1.000000000000000000, 0.000000000000000000 ) ) ;
#48217 = CARTESIAN_POINT ( 'NONE',  ( 1.227034120734908917, 0.2952755905511810774, -0.1292274648535930714 ) ) ;
#48218 = CARTESIAN_POINT ( 'NONE',  ( -0.2362204724409447953, -0.4091458600556404646, -2.427821522309711266 ) ) ;
#48219 = CARTESIAN_POINT ( 'NONE',  ( 5.463695987328526437E-16, -0.1870078740157479769, 0.4822834645669291653 ) ) ;
#48220 = CARTESIAN_POINT ( 'NONE',  ( -0.7283464566929126471, 0.1660481256975883668, -0.3530559997133364547 ) ) ;
#48221 = CARTESIAN_POINT ( 'NONE',  ( -1.594488188976377119, 0.1660481256975883668, -0.3530559997133364547 ) ) ;
#48222 = CARTESIAN_POINT ( 'NONE',  ( -0.1958661417322836718, 0.3392501089628017219, -0.09776902887139117537 ) ) ;
#48223 = CARTESIAN_POINT ( 'NONE',  ( 0.09842519685039434474, -0.5400638737290845981, -0.3530559997133363437 ) ) ;
#48224 = CARTESIAN_POINT ( 'NONE',  ( 0.3392501089628018884, -0.1958661417322834220, -2.301837270341207553 ) ) ;
#48225 = CARTESIAN_POINT ( 'NONE',  ( -1.240157480314959759, -0.4536011799217368745, -0.2665933059059886201 ) ) ;
#48226 = ORIENTED_EDGE ( 'NONE', *, *, #5997, .T. ) ;
#48227 = CARTESIAN_POINT ( 'NONE',  ( 0.3420746716998660508, -0.1974969037888703871, -2.152230971128608950 ) ) ;
#48228 = ORIENTED_EDGE ( 'NONE', *, *, #55825, .F. ) ;
#48229 = CARTESIAN_POINT ( 'NONE',  ( -1.736178228450298011, 1.299212598425196985, 0.4102808022082834460 ) ) ;
#48230 = CARTESIAN_POINT ( 'NONE',  ( -1.377952755905511140, 0.2952755905511811885, 0.000000000000000000 ) ) ;
#48231 = CARTESIAN_POINT ( 'NONE',  ( -0.1998031496062991907, -0.3460692066303959757, -1.167979002624671914 ) ) ;
#48232 = FACE_OUTER_BOUND ( 'NONE', #13549, .T. ) ;
#48233 = CARTESIAN_POINT ( 'NONE',  ( -1.574803149606298636, -0.1870078740157479769, 0.4822834645669291653 ) ) ;
#48234 = FACE_OUTER_BOUND ( 'NONE', #40346, .T. ) ;
#48235 = CARTESIAN_POINT ( 'NONE',  ( 0.4724409448818898682, 0.000000000000000000, -2.755905511811024056 ) ) ;
#48236 = CARTESIAN_POINT ( 'NONE',  ( 0.1049643490035304938, -0.3917322834645669549, -0.1699475065616798397 ) ) ;
#48237 = CARTESIAN_POINT ( 'NONE',  ( -0.2034120734908128059, 0.1771653543307087630, 0.09757992244046791164 ) ) ;
#48238 = CARTESIAN_POINT ( 'NONE',  ( -0.6758530183727028406, -0.5511811023622048555, -0.09757992244046775898 ) ) ;
#48239 = CARTESIAN_POINT ( 'NONE',  ( -1.397637795275589623, -0.5400638737290845981, -0.3530559997133363437 ) ) ;
#48240 = CARTESIAN_POINT ( 'NONE',  ( 0.5839895013123367340, -0.6692913385826773087, -0.1292274648535924053 ) ) ;
#48241 = CARTESIAN_POINT ( 'NONE',  ( -1.450131233595799651, 0.2952755905511810774, -0.1292274648535930714 ) ) ;
#48242 = CARTESIAN_POINT ( 'NONE',  ( 0.1049643490035304938, -0.3917322834645669549, 0.08005249343832024356 ) ) ;
#48243 = ORIENTED_EDGE ( 'NONE', *, *, #79898, .F. ) ;
#48244 = CARTESIAN_POINT ( 'NONE',  ( -1.364829396325458521, -0.6046776061558807314, 0.2411417322834647770 ) ) ;
#48245 = CYLINDRICAL_SURFACE ( 'NONE', #82377, 3.543307086614173151 ) ;
#48246 = CARTESIAN_POINT ( 'NONE',  ( 0.3458507752293908943, -0.3458507752293908943, -1.515748031496062742 ) ) ;
#48247 = CARTESIAN_POINT ( 'NONE',  ( 1.850381573804679158, 1.062979042929935058, -0.007789085821702718300 ) ) ;
#48248 = CARTESIAN_POINT ( 'NONE',  ( 4.797336870675656522E-17, -0.3917322834645670104, -0.7007874015748030150 ) ) ;
#48249 = CARTESIAN_POINT ( 'NONE',  ( 0.4768139191967274981, 1.559564387633094018, -0.5050868514466849701 ) ) ;
#48250 = CARTESIAN_POINT ( 'NONE',  ( -0.8858267716535425107, -0.5400638737290844871, 0.3530559997133364547 ) ) ;
#48251 = CARTESIAN_POINT ( 'NONE',  ( 1.450131233595801428, -0.6692913385826773087, -0.1292274648535924053 ) ) ;
#48253 = CARTESIAN_POINT ( 'NONE',  ( -0.4724409448818896462, -0.1265901696524993070, -1.935695538057742526 ) ) ;
#48252 = DIRECTION ( 'NONE',  ( 0.000000000000000000, -1.000000000000000000, -0.000000000000000000 ) ) ;
#48254 = CARTESIAN_POINT ( 'NONE',  ( -1.312335958005248715, -0.6046776061558809534, -0.2411417322834644161 ) ) ;
#48255 = CARTESIAN_POINT ( 'NONE',  ( -0.7742782152230965886, 0.05413385826771666132, 0.4176697321401328100 ) ) ;
#48256 = CARTESIAN_POINT ( 'NONE',  ( -0.1958661417322834497, -0.3392501089628018884, 0.01183033940388633805 ) ) ;
#48257 = CARTESIAN_POINT ( 'NONE',  ( -0.1640419947506555343, -0.2845877964562159024, 0.3641732283464567677 ) ) ;
#48258 = CARTESIAN_POINT ( 'NONE',  ( -0.1958661417322836718, 0.3392501089628017219, -0.5702099737532808632 ) ) ;
#48259 = CARTESIAN_POINT ( 'NONE',  ( -0.2690288713910754526, -0.5511811023622046335, 0.09757992244046803654 ) ) ;
#48260 = CARTESIAN_POINT ( 'NONE',  ( 1.017060367454068581, -0.08942795157528024563, -0.3641732283464568787 ) ) ;
#48261 = CARTESIAN_POINT ( 'NONE',  ( 0.8398950131233602345, 0.2306618581243847221, -0.2411417322834647770 ) ) ;
#48262 = CARTESIAN_POINT ( 'NONE',  ( -0.3018372703412066094, -0.3690944881889765550, -0.3153832671262227771 ) ) ;
#48263 = CARTESIAN_POINT ( 'NONE',  ( -0.3392501089628017219, -0.1958661417322836718, -2.249343832020997525 ) ) ;
#48264 = CARTESIAN_POINT ( 'NONE',  ( -1.496062992125983815, -0.1870078740157479769, 0.4822834645669291653 ) ) ;
#48265 = CARTESIAN_POINT ( 'NONE',  ( -1.286089238845143479, 0.1283753931104746893, -0.1820866141732285504 ) ) ;
#48266 = CARTESIAN_POINT ( 'NONE',  ( 0.4724409448818897572, -0.1265901696524988906, -0.1883202099737532054 ) ) ;
#48267 = CARTESIAN_POINT ( 'NONE',  ( 0.2165354330708668673, 0.1660481256975883668, -0.3530559997133364547 ) ) ;
#48268 = CARTESIAN_POINT ( 'NONE',  ( -0.2887139107611542133, -0.6046776061558809534, -0.2411417322834644161 ) ) ;
#48269 = CARTESIAN_POINT ( 'NONE',  ( 1.568241469816273659, -0.08942795157528024563, -0.3641732283464568787 ) ) ;
#48270 = CARTESIAN_POINT ( 'NONE',  ( 0.6955380577427828781, -0.004921259842519870586, -0.3153832671262229437 ) ) ;
#48271 = CARTESIAN_POINT ( 'NONE',  ( -0.1509186351706028884, -0.08942795157527998196, 0.3641732283464567121 ) ) ;
#48272 = CARTESIAN_POINT ( 'NONE',  ( -0.6167979002624665030, -0.4281496062992127816, -0.4176697321401328100 ) ) ;
#48273 = DIRECTION ( 'NONE',  ( -1.000000000000000000, 0.000000000000000000, 0.000000000000000000 ) ) ;
#48274 = CARTESIAN_POINT ( 'NONE',  ( -0.4724409448818882584, 0.1265901696525017217, -1.999343832020997525 ) ) ;
#48275 = CARTESIAN_POINT ( 'NONE',  ( 8.195543980992789655E-16, -0.1870078740157480879, -0.4822834645669291653 ) ) ;
#48276 = CARTESIAN_POINT ( 'NONE',  ( 0.3460692066303958092, 0.1998031496062993018, -1.467847769028871596 ) ) ;
#48277 = CARTESIAN_POINT ( 'NONE',  ( 1.502624671916010790, -0.3162353388693409650, -0.4822834645669289433 ) ) ;
#48278 = CARTESIAN_POINT ( 'NONE',  ( -0.1115485564304456306, 0.1771653543307087075, -0.09757992244046823083 ) ) ;
#48279 = CARTESIAN_POINT ( 'NONE',  ( -0.07874015748031421014, -0.1870078740157480879, -0.4822834645669291653 ) ) ;
#48280 = CARTESIAN_POINT ( 'NONE',  ( -1.469816272965878357, 0.2306618581243848609, 0.2411417322834645549 ) ) ;
#48281 = CARTESIAN_POINT ( 'NONE',  ( -1.456692913385826182, 0.1771653543307087630, 0.000000000000000000 ) ) ;
#48282 = CARTESIAN_POINT ( 'NONE',  ( 1.430446194225722500, -0.4281496062992127816, -0.4176697321401328100 ) ) ;
#48283 =( BOUNDED_CURVE ( )  B_SPLINE_CURVE ( 1, ( #62352, #4690 ),
 .UNSPECIFIED., .F., .F. ) 
 B_SPLINE_CURVE_WITH_KNOTS ( ( 2, 2 ),
 ( 1.738108305489988542E-18, 0.001850000000000003118 ),
 .UNSPECIFIED. ) 
 CURVE ( )  GEOMETRIC_REPRESENTATION_ITEM ( )  RATIONAL_B_SPLINE_CURVE ( ( 0.9911642120908008557, 0.9911642120908008557 ) ) 
 REPRESENTATION_ITEM ( '' )  );
#48284 = CARTESIAN_POINT ( 'NONE',  ( -1.515748031496062076, -0.5400638737290844871, 0.3530559997133364547 ) ) ;
#48285 = CARTESIAN_POINT ( 'NONE',  ( -0.6561679790026240244, -0.5023911411419708095, 0.1820866141732285504 ) ) ;
#48287 = EDGE_CURVE ( 'NONE', #81066, #64662, #57002, .T. ) ;
#48286 = CARTESIAN_POINT ( 'NONE',  ( 0.3996062992125985480, 2.446882876249141654E-17, -0.3523622047244094335 ) ) ;
#48288 = CARTESIAN_POINT ( 'NONE',  ( -0.2925321140481932924, 0.2925321140481931814, -0.6496062992125984925 ) ) ;
#48289 = CARTESIAN_POINT ( 'NONE',  ( -0.3949938075777411628, 0.1058382717557497937, 0.1246719160104986374 ) ) ;
#48290 = CARTESIAN_POINT ( 'NONE',  ( 1.496062992125985147, -0.1870078740157479769, 0.3641732283464567677 ) ) ;
#48291 = CARTESIAN_POINT ( 'NONE',  ( 1.076115485564305141, -0.5023911411419708095, 0.1820866141732285504 ) ) ;
#48292 = CARTESIAN_POINT ( 'NONE',  ( -1.587926509186350810, -0.4281496062992124485, 0.4176697321401328655 ) ) ;
#48293 = CARTESIAN_POINT ( 'NONE',  ( 0.8595800524934390507, -0.05778040916215560624, -0.4822834645669293319 ) ) ;
#48294 = CARTESIAN_POINT ( 'NONE',  ( -0.1058382717557497660, -0.3949938075777411073, -1.093832020997375309 ) ) ;
#48295 = CARTESIAN_POINT ( 'NONE',  ( 1.036745406824147731, -0.004921259842519576551, 0.3153832671262227771 ) ) ;
#48296 = CARTESIAN_POINT ( 'NONE',  ( -0.006561679790025524116, -0.05778040916215560624, -0.4822834645669293319 ) ) ;
#48297 = CARTESIAN_POINT ( 'NONE',  ( -1.010498687664041384, 0.05413385826771666132, 0.4176697321401328100 ) ) ;
#48298 = CARTESIAN_POINT ( 'NONE',  ( -3.908320185825790993, 1.553415232435839677, 0.4744094488188969616 ) ) ;
#48299 = CARTESIAN_POINT ( 'NONE',  ( -0.4724409448818899238, 0.1265901696524986686, -1.135170603674540590 ) ) ;
#48300 = CARTESIAN_POINT ( 'NONE',  ( 0.3996062992125985480, 0.1070741851644054637, -2.171916010498687211 ) ) ;
#48301 = CARTESIAN_POINT ( 'NONE',  ( 0.3280839895013130669, -0.004921259842519576551, 0.3153832671262227771 ) ) ;
#48302 = ORIENTED_EDGE ( 'NONE', *, *, #67409, .T. ) ;
#48303 = CARTESIAN_POINT ( 'NONE',  ( 4.797336870675656522E-17, -0.3917322834645670659, -0.2329589483277709483 ) ) ;
#48304 = ORIENTED_EDGE ( 'NONE', *, *, #42584, .T. ) ;
#48305 = CARTESIAN_POINT ( 'NONE',  ( -0.3543307086614165824, -0.6692913385826771977, 8.415575281601705876E-17 ) ) ;
#48306 = CARTESIAN_POINT ( 'NONE',  ( -0.1640419947506553400, -0.05778040916215560624, -0.4822834645669293319 ) ) ;
#48307 = CARTESIAN_POINT ( 'NONE',  ( -0.3280839895013117347, -0.004921259842519870586, -0.3153832671262229437 ) ) ;
#48308 = CARTESIAN_POINT ( 'NONE',  ( 0.8070866141732289112, -0.5400638737290845981, -0.3530559997133363437 ) ) ;
#48309 = CARTESIAN_POINT ( 'NONE',  ( -0.8530183727034112984, 0.05413385826771666132, 0.4176697321401328100 ) ) ;
#48310 = CARTESIAN_POINT ( 'NONE',  ( -0.3871391076115479057, -0.3162353388693409650, -0.4822834645669289433 ) ) ;
#48311 = CARTESIAN_POINT ( 'NONE',  ( 1.082677165354331228, -0.5400638737290844871, 0.3530559997133364547 ) ) ;
#48312 = CARTESIAN_POINT ( 'NONE',  ( 0.9383202099737536495, -0.3162353388693405765, 0.4822834645669290543 ) ) ;
#48313 = CARTESIAN_POINT ( 'NONE',  ( 0.6955380577427828781, -0.4281496062992124485, 0.4176697321401328655 ) ) ;
#48314 = CARTESIAN_POINT ( 'NONE',  ( -0.3392501089628017219, -0.1958661417322836718, -1.146981627296587813 ) ) ;
#48315 = CARTESIAN_POINT ( 'NONE',  ( -0.1837270341207340729, 0.1283753931104746893, -0.1820866141732285504 ) ) ;
#48316 = ORIENTED_EDGE ( 'NONE', *, *, #405, .T. ) ;
#48317 = CARTESIAN_POINT ( 'NONE',  ( -0.3420746716998659953, -0.1974969037888706647, -1.154855643044619518 ) ) ;
#48318 = VERTEX_POINT ( 'NONE', #8161 ) ;
#48319 = CARTESIAN_POINT ( 'NONE',  ( -0.7480314960629914633, 0.1771653543307087630, 0.000000000000000000 ) ) ;
#48320 = CARTESIAN_POINT ( 'NONE',  ( -0.6627296587926501115, 0.2952755905511810774, -0.1292274648535930714 ) ) ;
#48321 = CARTESIAN_POINT ( 'NONE',  ( -0.5314960629921373636, 2.755905511811024056, 3.264097702071371288 ) ) ;
#48322 = CARTESIAN_POINT ( 'NONE',  ( -0.5380577427821514602, -0.4281496062992127816, -0.4176697321401328100 ) ) ;
#48323 = CARTESIAN_POINT ( 'NONE',  ( -0.2099737532808391705, -0.6046776061558809534, -0.2411417322834644161 ) ) ;
#48324 = CARTESIAN_POINT ( 'NONE',  ( -1.253280839895012377, -0.3162353388693409650, -0.4822834645669289433 ) ) ;
#48325 = CARTESIAN_POINT ( 'NONE',  ( -1.397637795275589623, 0.1660481256975885056, 0.3530559997133364547 ) ) ;
#48326 = CARTESIAN_POINT ( 'NONE',  ( 0.9448818897637802916, -0.1870078740157480601, -0.3641732283464567677 ) ) ;
#48327 = CARTESIAN_POINT ( 'NONE',  ( -1.646051170424378096, 0.8346805926620876059, 0.5309055118110233007 ) ) ;
#48328 = CARTESIAN_POINT ( 'NONE',  ( 0.2397245358942217408, 0.1724005034516534474, 5.660736073501680288 ) ) ;
#48329 = CARTESIAN_POINT ( 'NONE',  ( 0.5511811023622054106, -0.1870078740157480601, -0.3641732283464567677 ) ) ;
#48330 = CARTESIAN_POINT ( 'NONE',  ( 0.08530183727034192087, -0.05778040916215522460, 0.4822834645669289988 ) ) ;
#48331 = CARTESIAN_POINT ( 'NONE',  ( 0.2952755905511819101, 0.1660481256975883668, -0.3530559997133364547 ) ) ;
#48332 = ORIENTED_EDGE ( 'NONE', *, *, #15774, .T. ) ;
#48333 = CARTESIAN_POINT ( 'NONE',  ( 0.1070741851644053527, 0.3996062992125986590, -1.725721784776903078 ) ) ;
#48334 = CARTESIAN_POINT ( 'NONE',  ( -0.6986524979670485358, -2.191421614605370878E-15, 0.4445507791589071167 ) ) ;
#48335 = EDGE_LOOP ( 'NONE', ( #37283, #70255, #20169, #15952 ) ) ;
#48336 = CARTESIAN_POINT ( 'NONE',  ( -0.3996062992125986590, 0.1070741851644051723, -1.211942257217847541 ) ) ;
#48337 = CARTESIAN_POINT ( 'NONE',  ( 1.568241469816273437, -0.3162353388693405765, 0.4822834645669290543 ) ) ;
#48338 = CARTESIAN_POINT ( 'NONE',  ( -0.5446194225721777693, -0.2845877964562161244, -0.3641732283464567121 ) ) ;
#48339 = CARTESIAN_POINT ( 'NONE',  ( -1.148293963254592542, -0.6692913385826773087, -0.1292274648535924053 ) ) ;
#48340 = CARTESIAN_POINT ( 'NONE',  ( 0.4091458600556404646, -0.2362204724409448231, -0.2624671916010498651 ) ) ;
#48341 = CARTESIAN_POINT ( 'NONE',  ( -9.594673741351313045E-17, 0.3917322834645670104, -2.604330708661416693 ) ) ;
#48342 = CARTESIAN_POINT ( 'NONE',  ( -1.509186351706035767, -0.3690944881889763329, 0.3153832671262228327 ) ) ;
#48343 = CARTESIAN_POINT ( 'NONE',  ( 0.3937007874015754361, -0.1870078740157480879, -0.4822834645669291653 ) ) ;
#48344 = CARTESIAN_POINT ( 'NONE',  ( 0.6889763779527566800, -0.5400638737290844871, 0.3530559997133364547 ) ) ;
#48345 = CARTESIAN_POINT ( 'NONE',  ( -0.6692913385826764205, 0.1771653543307087630, 0.000000000000000000 ) ) ;
#48346 = CARTESIAN_POINT ( 'NONE',  ( -0.01312335958005186876, -0.4281496062992124485, 0.4176697321401328655 ) ) ;
#48347 = CARTESIAN_POINT ( 'NONE',  ( -0.1265901696524986964, -0.4724409448818899238, -2.196194225721784576 ) ) ;
#48348 = CARTESIAN_POINT ( 'NONE',  ( -0.3018372703412066094, -0.3690944881889765550, -0.3153832671262227771 ) ) ;
#48349 = CARTESIAN_POINT ( 'NONE',  ( -0.4265091863517051496, 0.2952755905511810774, -0.1292274648535930714 ) ) ;
#48350 = CARTESIAN_POINT ( 'NONE',  ( 0.3949938075777409963, 2.418639510665530743E-17, -1.927165354330708569 ) ) ;
#48351 = CARTESIAN_POINT ( 'NONE',  ( 1.614173228346457378, 0.1771653543307087630, 0.000000000000000000 ) ) ;
#48352 = CARTESIAN_POINT ( 'NONE',  ( -0.08530183727034056085, -0.08942795157528024563, -0.3641732283464568787 ) ) ;
#48353 = CARTESIAN_POINT ( 'NONE',  ( 1.266404199475066328, -0.2845877964562161244, -0.3641732283464567121 ) ) ;
#48354 = CARTESIAN_POINT ( 'NONE',  ( -1.299212598425196097, -0.6692913385826771977, 8.415575281601705876E-17 ) ) ;
#48355 = CARTESIAN_POINT ( 'NONE',  ( -0.6102362204724400829, -0.4536011799217368745, -0.2665933059059886201 ) ) ;
#48356 = CARTESIAN_POINT ( 'NONE',  ( 0.000000000000000000, 1.724409448818897461, -2.362204724409448620 ) ) ;
#48357 = CARTESIAN_POINT ( 'NONE',  ( -1.233595800524933894, 0.2306618581243848609, 0.2411417322834645549 ) ) ;
#48358 = CARTESIAN_POINT ( 'NONE',  ( -0.4396325459317577122, -0.6692913385826773087, -0.1292274648535924053 ) ) ;
#48359 = CARTESIAN_POINT ( 'NONE',  ( 0.4855643044619430415, -0.4281496062992127816, -0.4176697321401328100 ) ) ;
#48360 = CARTESIAN_POINT ( 'NONE',  ( 0.1958661417322834497, 0.3392501089628018329, -2.586594857446507412 ) ) ;
#48361 = CARTESIAN_POINT ( 'NONE',  ( 0.5314960629920855162, 2.740199102106095186, 3.870235431238107981 ) ) ;
#48362 = CARTESIAN_POINT ( 'NONE',  ( 0.2493438320209980519, -0.004921259842519576551, 0.3153832671262227771 ) ) ;
#48363 = CARTESIAN_POINT ( 'NONE',  ( 0.9251968503937015864, -0.5400638737290844871, 0.3530559997133364547 ) ) ;
#48364 = CARTESIAN_POINT ( 'NONE',  ( -1.227034120734907585, 0.1771653543307087630, 0.09757992244046791164 ) ) ;
#48365 = CARTESIAN_POINT ( 'NONE',  ( 1.246719160104987623, 0.05413385826771626580, -0.4176697321401330321 ) ) ;
#48366 = CARTESIAN_POINT ( 'NONE',  ( -1.443569553805773564, -0.5023911411419708095, 0.1820866141732285504 ) ) ;
#48367 = CARTESIAN_POINT ( 'NONE',  ( -1.456692913385826182, -0.6692913385826771977, 8.415575281601705876E-17 ) ) ;
#48368 = CARTESIAN_POINT ( 'NONE',  ( -0.9317585301837263412, 0.05413385826771666132, 0.4176697321401328100 ) ) ;
#48369 = CARTESIAN_POINT ( 'NONE',  ( 0.1049868766404206816, 0.1283753931104748280, 0.1820866141732283561 ) ) ;
#48370 = CARTESIAN_POINT ( 'NONE',  ( 0.5314960629921325896, 2.755905511811024056, -1.895394334970790018 ) ) ;
#48371 = CARTESIAN_POINT ( 'NONE',  ( 0.7217847769028878924, -0.3690944881889765550, -0.3153832671262227771 ) ) ;
#48372 = CARTESIAN_POINT ( 'NONE',  ( -0.1771653543307080136, 0.1660481256975883668, -0.3530559997133364547 ) ) ;
#48373 = CARTESIAN_POINT ( 'NONE',  ( -0.3996062992125984925, -0.1070741851644056858, -0.1227034120734908362 ) ) ;
#48374 = EDGE_CURVE ( 'NONE', #32076, #35211, #34618, .T. ) ;
#48375 = CARTESIAN_POINT ( 'NONE',  ( -0.9908136482939626788, -0.6692913385826773087, -0.1292274648535924053 ) ) ;
#48376 = CARTESIAN_POINT ( 'NONE',  ( 4.797336870675656522E-17, -0.3917322834645670104, -1.895669291338582640 ) ) ;
#48377 = CARTESIAN_POINT ( 'NONE',  ( 1.240157480314961314, -0.4536011799217367080, 0.2665933059059888421 ) ) ;
#48378 = CARTESIAN_POINT ( 'NONE',  ( 0.05905511811023709395, -0.5400638737290844871, 0.3530559997133364547 ) ) ;
#48379 = CARTESIAN_POINT ( 'NONE',  ( -0.1771653543307080136, 0.1660481256975883668, -0.3530559997133364547 ) ) ;
#48380 = CARTESIAN_POINT ( 'NONE',  ( -0.4724409448818890911, -0.1870078740157480601, -0.3641732283464567677 ) ) ;
#48381 = CARTESIAN_POINT ( 'NONE',  ( 1.220472440944882386, 0.2952755905511811885, 0.000000000000000000 ) ) ;
#48382 = CARTESIAN_POINT ( 'NONE',  ( -0.6692913385826764205, 0.1771653543307087630, 0.000000000000000000 ) ) ;
#48383 = CARTESIAN_POINT ( 'NONE',  ( 0.5708661417322842269, 0.1660481256975885056, 0.3530559997133364547 ) ) ;
#48384 = CARTESIAN_POINT ( 'NONE',  ( -1.194225721784776262, -0.004921259842519870586, -0.3153832671262229437 ) ) ;
#48385 = CARTESIAN_POINT ( 'NONE',  ( -0.1998031496062991630, -0.3460692066303959202, -1.087270341207349000 ) ) ;
#48386 = CARTESIAN_POINT ( 'NONE',  ( -1.108923884514435132, -0.05778040916215560624, -0.4822834645669293319 ) ) ;
#48387 = CARTESIAN_POINT ( 'NONE',  ( -3.224202737261815166, 2.716535433070866645, 0.5314960629921260393 ) ) ;
#48388 = VERTEX_POINT ( 'NONE', #1024 ) ;
#48389 = CARTESIAN_POINT ( 'NONE',  ( -1.528871391076114250, 0.1771653543307087075, -0.09757992244046823083 ) ) ;
#48390 = CARTESIAN_POINT ( 'NONE',  ( -0.3412073490813641308, -0.6046776061558807314, 0.2411417322834647770 ) ) ;
#48391 = CARTESIAN_POINT ( 'NONE',  ( 0.2540590912309962368, 1.136744334959988389, -1.491123965641447002 ) ) ;
#48392 = CARTESIAN_POINT ( 'NONE',  ( -1.115485564304461219, 0.05413385826771626580, -0.4176697321401330321 ) ) ;
#48393 = CARTESIAN_POINT ( 'NONE',  ( -0.1958661417322834220, -0.3392501089628018884, -1.725065616797900381 ) ) ;
#48394 = CARTESIAN_POINT ( 'NONE',  ( -0.1265901696524986964, -0.4724409448818899238, -2.119422572178477626 ) ) ;
#48395 = CARTESIAN_POINT ( 'NONE',  ( 1.299212598425197429, -0.6692913385826771977, 8.415575281601705876E-17 ) ) ;
#48396 = CARTESIAN_POINT ( 'NONE',  ( 0.3805774278215230400, -0.4281496062992124485, 0.4176697321401328655 ) ) ;
#48397 = CARTESIAN_POINT ( 'NONE',  ( -3.900966923095589678, 2.559055118110236560, -0.5314960629921260393 ) ) ;
#48398 = CARTESIAN_POINT ( 'NONE',  ( -9.787531504996566615E-17, 0.3996062992125985480, -2.596456692913385655 ) ) ;
#48399 = CARTESIAN_POINT ( 'NONE',  ( -1.568241469816272105, -0.05778040916215522460, 0.4822834645669289988 ) ) ;
#48400 = CARTESIAN_POINT ( 'NONE',  ( -0.3460692066303960868, 0.1998031496062990242, -0.4986876640419947715 ) ) ;
#48401 = ORIENTED_EDGE ( 'NONE', *, *, #21258, .T. ) ;
#48402 = CARTESIAN_POINT ( 'NONE',  ( -1.056430446194224881, -0.5511811023622046335, 0.09757992244046803654 ) ) ;
#48403 = CARTESIAN_POINT ( 'NONE',  ( 0.2867679344610365999, -0.2867679344610365444, -2.295275590551181022 ) ) ;
#48404 = ORIENTED_EDGE ( 'NONE', *, *, #17250, .F. ) ;
#48405 = CARTESIAN_POINT ( 'NONE',  ( 0.6233595800524939223, -0.3162353388693405765, 0.4822834645669290543 ) ) ;
#48406 = CARTESIAN_POINT ( 'NONE',  ( -0.2624671916010490880, 0.2306618581243847221, -0.2411417322834647770 ) ) ;
#48407 = CARTESIAN_POINT ( 'NONE',  ( -1.233595800524933894, -0.6046776061558809534, -0.2411417322834644161 ) ) ;
#48408 = CARTESIAN_POINT ( 'NONE',  ( 1.213910761154856299, 0.2952755905511811885, 0.1292274648535926551 ) ) ;
#48409 = CARTESIAN_POINT ( 'NONE',  ( -1.095800524934382292, -0.2845877964562161244, -0.3641732283464567121 ) ) ;
#48410 = CARTESIAN_POINT ( 'NONE',  ( -0.4744094488188832504, 1.537401574803149984, -3.937007874015763687 ) ) ;
#48411 = CARTESIAN_POINT ( 'NONE',  ( 0.3346456692913393205, -0.5400638737290845981, -0.3530559997133363437 ) ) ;
#48412 = CARTESIAN_POINT ( 'NONE',  ( -0.7349081364829387342, -0.6046776061558807314, 0.2411417322834647770 ) ) ;
#48413 = CARTESIAN_POINT ( 'NONE',  ( 0.2867679344610365999, -0.2867679344610365999, -1.753261524113173708 ) ) ;
#48414 = CARTESIAN_POINT ( 'NONE',  ( -1.423884514435694859, -0.05778040916215560624, -0.4822834645669293319 ) ) ;
#48415 = B_SPLINE_CURVE_WITH_KNOTS ( 'NONE', 3,
 ( #27424, #72473, #77536, #45935 ),
 .UNSPECIFIED., .F., .F.,
 ( 4, 4 ),
 ( 0.1331161126011571050, 0.1345277053022634894 ),
 .UNSPECIFIED. ) ;
#48416 = CARTESIAN_POINT ( 'NONE',  ( 0.3335738234991732498, 1.199759523613724843, -2.750612009938800284 ) ) ;
#48417 =( BOUNDED_CURVE ( )  B_SPLINE_CURVE ( 2, ( #1800, #32109, #25784, #77994, #19481, #27045, #13187, #14022, #554, #46814, #78416, #45975, #8119 ),
 .UNSPECIFIED., .F., .F. ) 
 B_SPLINE_CURVE_WITH_KNOTS ( ( 3, 2, 2, 2, 2, 2, 3 ),
 ( 0.2649423569342326812, 0.2651515151515151381, 0.2689393939393939226, 0.2727272727272727071, 0.2765151515151514916, 0.2803030303030302761, 0.2805121885203127330 ),
 .UNSPECIFIED. ) 
 CURVE ( )  GEOMETRIC_REPRESENTATION_ITEM ( )  RATIONAL_B_SPLINE_CURVE ( ( 0.9964447847208428577, 0.9981185001348096275, 1.000000000000000000, 0.9659258262890683122, 1.000000000000000000, 0.9659258262890683122, 1.000000000000000000, 0.9659258262890683122, 1.000000000000000000, 0.9659258262890683122, 1.000000000000000000, 0.9981185001348097385, 0.9964447847208430797 ) ) 
 REPRESENTATION_ITEM ( '' )  );
#48418 = CARTESIAN_POINT ( 'NONE',  ( 0.7939632545931766261, -0.3162353388693409650, -0.4822834645669289433 ) ) ;
#48419 = CARTESIAN_POINT ( 'NONE',  ( 1.089238845144357759, -0.004921259842519870586, -0.3153832671262229437 ) ) ;
#48420 = ORIENTED_EDGE ( 'NONE', *, *, #39780, .T. ) ;
#48421 = CARTESIAN_POINT ( 'NONE',  ( -9.674558042662121740E-17, 0.3949938075777409963, 0.1574803149606298636 ) ) ;
#48422 = CARTESIAN_POINT ( 'NONE',  ( -0.5446194225721777693, -0.05778040916215522460, 0.4822834645669289988 ) ) ;
#48423 = VERTEX_POINT ( 'NONE', #33826 ) ;
#48424 = CARTESIAN_POINT ( 'NONE',  ( 0.4461942257217855201, -0.5023911411419708095, 0.1820866141732285504 ) ) ;
#48425 = CARTESIAN_POINT ( 'NONE',  ( -1.528871391076114250, 0.2952755905511810774, -0.1292274648535930714 ) ) ;
#48426 = CARTESIAN_POINT ( 'NONE',  ( 0.9580052493438326877, 0.05413385826771666132, 0.4176697321401328100 ) ) ;
#48427 = CARTESIAN_POINT ( 'NONE',  ( 0.9514435695538062676, -0.05778040916215522460, 0.4822834645669289988 ) ) ;
#48428 = CARTESIAN_POINT ( 'NONE',  ( -0.3674540682414692561, -0.6046776061558809534, -0.2411417322834644161 ) ) ;
#48429 = VECTOR ( 'NONE', #60686, 39.37007874015748143 ) ;
#48430 = CARTESIAN_POINT ( 'NONE',  ( 0.3392501089628018329, 0.1958661417322835607, -1.387814591372390272 ) ) ;
#48431 = CARTESIAN_POINT ( 'NONE',  ( -0.6758530183727028406, 0.2952755905511811885, 0.1292274648535926551 ) ) ;
#48432 = CARTESIAN_POINT ( 'NONE',  ( -0.2867679344610364334, -0.2867679344610367109, -2.348425196850393970 ) ) ;
#48433 = CARTESIAN_POINT ( 'NONE',  ( -1.410761154855642463, -0.05778040916215522460, 0.4822834645669289988 ) ) ;
#48434 = CARTESIAN_POINT ( 'NONE',  ( -0.9580052493438311334, 0.05413385826771626580, -0.4176697321401330321 ) ) ;
#48435 = CARTESIAN_POINT ( 'NONE',  ( 1.187664041994751285, -0.05778040916215522460, 0.4822834645669289988 ) ) ;
#48436 = CARTESIAN_POINT ( 'NONE',  ( 1.653543307086614789, -0.1870078740157479769, 0.4822834645669291653 ) ) ;
#48437 = CARTESIAN_POINT ( 'NONE',  ( -0.7611548556430438595, 0.2306618581243848609, 0.2411417322834645549 ) ) ;
#48438 = CARTESIAN_POINT ( 'NONE',  ( -0.5314960629921371416, 2.755905511811024056, 3.184294706754628557 ) ) ;
#48439 = CARTESIAN_POINT ( 'NONE',  ( 0.1640419947506569498, -0.05778040916215522460, 0.4822834645669289988 ) ) ;
#48440 = CARTESIAN_POINT ( 'NONE',  ( -0.3996062992125986035, -7.340648628747425578E-17, -1.771653543307086576 ) ) ;
#48441 = CARTESIAN_POINT ( 'NONE',  ( -0.3477690288713902178, 0.2952755905511810774, -0.1292274648535930714 ) ) ;
#48442 = CARTESIAN_POINT ( 'NONE',  ( -1.443569553805773564, 0.1283753931104746893, -0.1820866141732285504 ) ) ;
#48443 = CARTESIAN_POINT ( 'NONE',  ( 0.4199475065616805614, 0.1283753931104748280, 0.1820866141732283561 ) ) ;
#48444 = CARTESIAN_POINT ( 'NONE',  ( 1.305774278215223960, 0.2952755905511810774, -0.1292274648535930714 ) ) ;
#48445 = CARTESIAN_POINT ( 'NONE',  ( -0.4091458600556405756, 0.2362204724409446288, -0.7329396325459317518 ) ) ;
#48446 = CARTESIAN_POINT ( 'NONE',  ( 1.358267716535433323, 0.07958543189024085140, 0.2665933059059887866 ) ) ;
#48447 = CARTESIAN_POINT ( 'NONE',  ( 0.8005249343832027131, 0.05413385826771666132, 0.4176697321401328100 ) ) ;
#48448 = CARTESIAN_POINT ( 'NONE',  ( -0.1974969037888704149, -0.3420746716998661063, -0.4573490813648294906 ) ) ;
#48449 = CARTESIAN_POINT ( 'NONE',  ( -0.5577427821522301654, -0.05778040916215560624, -0.4822834645669293319 ) ) ;
#48450 = DIRECTION ( 'NONE',  ( 1.000000000000000000, -0.000000000000000000, -0.000000000000000000 ) ) ;
#48451 = CARTESIAN_POINT ( 'NONE',  ( 1.469816272965879911, 0.1283753931104746893, -0.1820866141732285504 ) ) ;
#48452 = CARTESIAN_POINT ( 'NONE',  ( -0.6824146981627291497, -0.6046776061558809534, -0.2411417322834644161 ) ) ;
#48453 = CARTESIAN_POINT ( 'NONE',  ( 0.3420746716998660508, 0.1974969037888705814, -0.6804461942257220564 ) ) ;
#48454 = CARTESIAN_POINT ( 'NONE',  ( 1.450131233595801428, -0.6692913385826773087, -0.1292274648535924053 ) ) ;
#48455 = CARTESIAN_POINT ( 'NONE',  ( 0.05905511811023681640, 0.1660481256975883668, -0.3530559997133364547 ) ) ;
#48456 = CARTESIAN_POINT ( 'NONE',  ( 0.3674540682414705883, -0.5023911411419708095, 0.1820866141732285504 ) ) ;
#48457 = FACE_OUTER_BOUND ( 'NONE', #82313, .T. ) ;
#48458 = CARTESIAN_POINT ( 'NONE',  ( -0.1246719160104980823, -0.5511811023622048555, -0.09757992244046775898 ) ) ;
#48459 = CARTESIAN_POINT ( 'NONE',  ( 0.7874015748031503170, -0.1870078740157479769, 0.3641732283464567677 ) ) ;
#48460 = CARTESIAN_POINT ( 'NONE',  ( -1.496062992125983815, -0.1870078740157479769, 0.4822834645669291653 ) ) ;
#48461 = CARTESIAN_POINT ( 'NONE',  ( -0.1070741851644056997, 0.3996062992125984925, -1.500656167979002253 ) ) ;
#48462 = CARTESIAN_POINT ( 'NONE',  ( 0.8530183727034128527, -0.4281496062992124485, 0.4176697321401328655 ) ) ;
#48463 = CARTESIAN_POINT ( 'NONE',  ( 0.3917322834645670104, -0.1049643490035303411, -1.048556430446194287 ) ) ;
#48464 = CARTESIAN_POINT ( 'NONE',  ( 1.587926509186352586, -0.3690944881889765550, -0.3153832671262227771 ) ) ;
#48465 = CARTESIAN_POINT ( 'NONE',  ( 1.895394334970792016, 2.755905511811024056, -0.5314960629921260393 ) ) ;
#48466 = CARTESIAN_POINT ( 'NONE',  ( -0.1771653543307080136, -0.4536011799217367080, 0.2665933059059888421 ) ) ;
#48467 = CARTESIAN_POINT ( 'NONE',  ( 0.1377952755905518800, 0.1660481256975883668, -0.3530559997133364547 ) ) ;
#48468 = CARTESIAN_POINT ( 'NONE',  ( 1.345144356955381593, -0.08942795157527998196, 0.3641732283464567121 ) ) ;
#48469 = CARTESIAN_POINT ( 'NONE',  ( -1.259842519685038686, -0.1870078740157479769, 0.3641732283464567677 ) ) ;
#48470 = CARTESIAN_POINT ( 'NONE',  ( -1.456692913385826182, -0.6692913385826771977, 8.415575281601705876E-17 ) ) ;
#48471 = CARTESIAN_POINT ( 'NONE',  ( 0.4986876640419954376, -0.6046776061558809534, -0.2411417322834644161 ) ) ;
#48472 = CARTESIAN_POINT ( 'NONE',  ( 1.030183727034121421, -0.05778040916215522460, 0.4822834645669289988 ) ) ;
#48473 = CARTESIAN_POINT ( 'NONE',  ( -0.005475238697255037888, 1.062992125984248304, -1.631265707957251010 ) ) ;
#48474 = CARTESIAN_POINT ( 'NONE',  ( 0.3215223097112867578, -0.05778040916215522460, 0.4822834645669289988 ) ) ;
#48475 = CARTESIAN_POINT ( 'NONE',  ( 1.122047244094488860, -0.5400638737290845981, -0.3530559997133363437 ) ) ;
#48476 = B_SPLINE_CURVE_WITH_KNOTS ( 'NONE', 3,
 ( #2387, #66783, #59610, #1965 ),
 .UNSPECIFIED., .F., .F.,
 ( 4, 4 ),
 ( 3.210432057656183116E-07, 0.001287787053612127848 ),
 .UNSPECIFIED. ) ;
#48477 = CARTESIAN_POINT ( 'NONE',  ( 1.135170603674541256, -0.6692913385826773087, -0.1292274648535924053 ) ) ;
#48478 = FACE_OUTER_BOUND ( 'NONE', #5225, .T. ) ;
#48479 = CARTESIAN_POINT ( 'NONE',  ( 0.7414698162729663755, 0.1771653543307087630, 0.09757992244046791164 ) ) ;
#48480 = CARTESIAN_POINT ( 'NONE',  ( -1.581364829396324945, -0.08942795157528024563, -0.3641732283464568787 ) ) ;
#48481 = CARTESIAN_POINT ( 'NONE',  ( 0.04593175853018440641, 0.1771653543307087075, -0.09757992244046823083 ) ) ;
#48482 = CARTESIAN_POINT ( 'NONE',  ( 0.3083989501312343062, -0.05778040916215560624, -0.4822834645669293319 ) ) ;
#48483 = CARTESIAN_POINT ( 'NONE',  ( 0.7152230971128614723, -0.3162353388693409650, -0.4822834645669289433 ) ) ;
#48484 = CARTESIAN_POINT ( 'NONE',  ( -0.4068241469816264999, -0.4281496062992124485, 0.4176697321401328655 ) ) ;
#48485 = CARTESIAN_POINT ( 'NONE',  ( -0.3149606299212590610, -0.1870078740157479769, 0.3641732283464567677 ) ) ;
#48486 = CIRCLE ( 'NONE', #71332, 3.937007874015748143 ) ;
#48487 = CARTESIAN_POINT ( 'NONE',  ( 0.6692913385826777528, 0.2952755905511811885, 0.000000000000000000 ) ) ;
#48488 = CARTESIAN_POINT ( 'NONE',  ( 0.7742782152230979209, -0.004921259842519870586, -0.3153832671262229437 ) ) ;
#48489 = CARTESIAN_POINT ( 'NONE',  ( -1.650841896953458843, 1.144577896360981395, 0.2660319121884003879 ) ) ;
#48491 = DIRECTION ( 'NONE',  ( -0.000000000000000000, -1.000000000000000000, -0.000000000000000000 ) ) ;
#48490 = DIRECTION ( 'NONE',  ( 0.7071067811865524577, 0.000000000000000000, 0.7071067811865425767 ) ) ;
#48492 = LINE ( 'NONE', #47669, #19338 ) ;
#48493 = CARTESIAN_POINT ( 'NONE',  ( -1.213910761154854745, -0.6692913385826771977, 0.1292274648535927661 ) ) ;
#48494 = CARTESIAN_POINT ( 'NONE',  ( -0.2821522309711278487, 0.2952755905511811885, 0.1292274648535926551 ) ) ;
#48495 = CARTESIAN_POINT ( 'NONE',  ( 0.1265901696524990294, -0.4724409448818896462, -0.08530183727034119923 ) ) ;
#48496 = CARTESIAN_POINT ( 'NONE',  ( -0.1058382717557497937, -0.3949938075777411628, -2.434383202099737353 ) ) ;
#48497 = ORIENTED_EDGE ( 'NONE', *, *, #50925, .T. ) ;
#48498 = CARTESIAN_POINT ( 'NONE',  ( 0.5971128608923891301, 0.1771653543307087075, -0.09757992244046823083 ) ) ;
#48499 = CARTESIAN_POINT ( 'NONE',  ( 0.1958661417322834775, 0.3392501089628018884, -1.081364829396325389 ) ) ;
#48500 = CARTESIAN_POINT ( 'NONE',  ( 1.076115485564305141, -0.6046776061558807314, 0.2411417322834647770 ) ) ;
#48501 = CARTESIAN_POINT ( 'NONE',  ( -0.3458507752293906723, -0.3458507752293910609, -2.421259842519684735 ) ) ;
#48502 = CARTESIAN_POINT ( 'NONE',  ( 3.898413161119330450, 2.697625129285034173, -0.5314960629921259283 ) ) ;
#48504 = CONICAL_SURFACE ( 'NONE', #41778, 2.401574803149606918, 0.6981317007977250189 ) ;
#48503 = CARTESIAN_POINT ( 'NONE',  ( -1.338582677165353729, -0.1870078740157480601, -0.3641732283464567677 ) ) ;
#48505 = CARTESIAN_POINT ( 'NONE',  ( 1.568241469816273659, -0.05778040916215560624, -0.4822834645669293319 ) ) ;
#48506 = EDGE_CURVE ( 'NONE', #50475, #56091, #59792, .T. ) ;
#48507 = CARTESIAN_POINT ( 'NONE',  ( 1.227034120734908917, -0.5511811023622046335, 0.09757992244046803654 ) ) ;
#48508 = CARTESIAN_POINT ( 'NONE',  ( 0.5774278215223104249, 0.2306618581243848609, 0.2411417322834645549 ) ) ;
#48509 = CARTESIAN_POINT ( 'NONE',  ( -9.594673741351310580E-17, 0.3917322834645669549, -0.3949938075777409963 ) ) ;
#48510 = CARTESIAN_POINT ( 'NONE',  ( -0.1902887139107604098, 0.2952755905511810774, -0.1292274648535930714 ) ) ;
#48511 = CARTESIAN_POINT ( 'NONE',  ( -0.9120734908136475250, 0.1771653543307087630, 0.09757992244046791164 ) ) ;
#48512 = CARTESIAN_POINT ( 'NONE',  ( 0.3477690288713918276, 0.2952755905511811885, 0.1292274648535926551 ) ) ;
#48514 = ADVANCED_FACE ( 'NONE', ( #7320 ), #79293, .F. ) ;
#48513 = CARTESIAN_POINT ( 'NONE',  ( -0.1312335958005241554, 0.2306618581243848609, 0.2411417322834645549 ) ) ;
#48515 = CARTESIAN_POINT ( 'NONE',  ( 0.4422585667712756741, 1.709808357580390625, 3.912093821574601282 ) ) ;
#48516 = CARTESIAN_POINT ( 'NONE',  ( 0.1998031496062994405, -0.3460692066303958092, -2.926509186351706315 ) ) ;
#48517 = CARTESIAN_POINT ( 'NONE',  ( 0.2867679344610366554, -0.2867679344610365999, -1.512486507382889256 ) ) ;
#48518 = CARTESIAN_POINT ( 'NONE',  ( 0.7283464566929143125, 0.1660481256975885056, 0.3530559997133364547 ) ) ;
#48519 = CARTESIAN_POINT ( 'NONE',  ( -0.006561679790025524116, -0.3162353388693405765, 0.4822834645669290543 ) ) ;
#48520 = CARTESIAN_POINT ( 'NONE',  ( -1.030183727034119867, -0.3162353388693405765, 0.4822834645669290543 ) ) ;
#48521 = CARTESIAN_POINT ( 'NONE',  ( 0.9448818897637802916, -0.1870078740157479769, 0.4822834645669291653 ) ) ;
#48522 = CARTESIAN_POINT ( 'NONE',  ( 0.4330708661417329575, 0.2952755905511811885, 0.000000000000000000 ) ) ;
#48523 = CARTESIAN_POINT ( 'NONE',  ( 4.797336870675656522E-17, -0.3917322834645670104, -0.9507874015748032370 ) ) ;
#48524 = CARTESIAN_POINT ( 'NONE',  ( -0.5183727034120726440, -0.6692913385826773087, -0.1292274648535924053 ) ) ;
#48525 = CARTESIAN_POINT ( 'NONE',  ( 0.1443569553805781891, 0.05413385826771626580, -0.4176697321401330321 ) ) ;
#48526 = CARTESIAN_POINT ( 'NONE',  ( -0.6496062992125976043, 0.1660481256975883668, -0.3530559997133364547 ) ) ;
#48527 = CARTESIAN_POINT ( 'NONE',  ( 0.5774278215223104249, 0.1283753931104748280, 0.1820866141732283561 ) ) ;
#48528 = DIRECTION ( 'NONE',  ( -0.000000000000000000, 1.000000000000000000, -0.000000000000000000 ) ) ;
#48529 = CARTESIAN_POINT ( 'NONE',  ( -0.3635331417845649726, 1.231226750417221183, -2.723475981305045313 ) ) ;
#48530 = CARTESIAN_POINT ( 'NONE',  ( 0.3871391076115492380, -0.05778040916215560624, -0.4822834645669293319 ) ) ;
#48531 = CARTESIAN_POINT ( 'NONE',  ( -0.1265901696524986964, -0.4724409448818899238, -0.9363517060367454459 ) ) ;
#48532 = CARTESIAN_POINT ( 'NONE',  ( 0.2867679344610365999, -0.2867679344610365444, -2.295275590551181022 ) ) ;
#48533 = ORIENTED_EDGE ( 'NONE', *, *, #27901, .T. ) ;
#48534 = EDGE_CURVE ( 'NONE', #1757, #75163, #10819, .T. ) ;
#48535 = ORIENTED_EDGE ( 'NONE', *, *, #24322, .F. ) ;
#48536 = CARTESIAN_POINT ( 'NONE',  ( 0.6299212598425204535, -0.1870078740157480879, -0.4822834645669291653 ) ) ;
#48537 = CARTESIAN_POINT ( 'NONE',  ( 0.6955380577427828781, -0.004921259842519870586, -0.3153832671262229437 ) ) ;
#48539 = CARTESIAN_POINT ( 'NONE',  ( -3.250800425606660049, 2.742781087017835961, -0.5314960629921260393 ) ) ;
#48538 = CARTESIAN_POINT ( 'NONE',  ( 0.000000000000000000, 2.755905511811024056, 0.000000000000000000 ) ) ;
#48540 = CARTESIAN_POINT ( 'NONE',  ( 4.797336870675656522E-17, -0.3917322834645670104, -0.9507874015748032370 ) ) ;
#48541 = EDGE_CURVE ( 'NONE', #9951, #9892, #44786, .T. ) ;
#48542 = FACE_BOUND ( 'NONE', #22741, .T. ) ;
#48543 = SURFACE_STYLE_USAGE ( .BOTH. , #15760 ) ;
#48544 = CARTESIAN_POINT ( 'NONE',  ( -0.3392501089628019995, 0.1958661417322832277, -1.528215223097112885 ) ) ;
#48546 = CARTESIAN_POINT ( 'NONE',  ( 0.2925321140481932369, -0.2925321140481931814, -2.222440944881889813 ) ) ;
#48545 = PRODUCT_RELATED_PRODUCT_CATEGORY ( 'part', '', ( #38538 ) ) ;
#48547 = CARTESIAN_POINT ( 'NONE',  ( 0.8595800524934390507, -0.05778040916215560624, -0.4822834645669293319 ) ) ;
#48548 = CARTESIAN_POINT ( 'NONE',  ( -0.6758530183727028406, 0.2952755905511811885, 0.1292274648535926551 ) ) ;
#48549 = CARTESIAN_POINT ( 'NONE',  ( -0.5839895013123351797, 0.2952755905511810774, -0.1292274648535930714 ) ) ;
#48550 = CARTESIAN_POINT ( 'NONE',  ( 0.5314960629921264834, 0.1660481256975883668, -0.3530559997133364547 ) ) ;
#48551 = AXIS2_PLACEMENT_3D ( 'NONE', #19230, #49976, #23901 ) ;
#48552 = CARTESIAN_POINT ( 'NONE',  ( 1.515748031496063186, -0.5400638737290845981, -0.3530559997133363437 ) ) ;
#48553 = CARTESIAN_POINT ( 'NONE',  ( 1.220472440944882164, 0.2066929133858268208, 4.479895975645240118E-15 ) ) ;
#48554 = CONTEXT_DEPENDENT_SHAPE_REPRESENTATION ( #43872, #78249 ) ;
#48555 = CARTESIAN_POINT ( 'NONE',  ( 1.122047244094488860, -0.4536011799217368745, -0.2665933059059886201 ) ) ;
#48556 = CARTESIAN_POINT ( 'NONE',  ( 0.2925321140481931814, 0.2925321140481931814, -1.946850393700787496 ) ) ;
#48557 = CARTESIAN_POINT ( 'NONE',  ( -1.128608923884513837, 0.1283753931104746893, -0.1820866141732285504 ) ) ;
#48558 = CARTESIAN_POINT ( 'NONE',  ( 0.1958661417322836440, -0.3392501089628017219, 0.07349081364829400387 ) ) ;
#48559 = CARTESIAN_POINT ( 'NONE',  ( -0.006561679790025524116, -0.05778040916215560624, -0.4822834645669293319 ) ) ;
#48561 = FACE_OUTER_BOUND ( 'NONE', #42025, .T. ) ;
#48560 = DIRECTION ( 'NONE',  ( 0.000000000000000000, 0.000000000000000000, 1.000000000000000000 ) ) ;
#48562 = CARTESIAN_POINT ( 'NONE',  ( -1.272965879265091305, -0.3690944881889763329, 0.3153832671262228327 ) ) ;
#48563 = CARTESIAN_POINT ( 'NONE',  ( 0.3740157480314966754, -0.5400638737290844871, 0.3530559997133364547 ) ) ;
#48564 = CARTESIAN_POINT ( 'NONE',  ( 1.135170603674541256, 0.1771653543307087630, 0.09757992244046791164 ) ) ;
#48565 = CARTESIAN_POINT ( 'NONE',  ( -0.1958661417322836440, 0.3392501089628016664, -1.195518741960943210 ) ) ;
#48566 = CARTESIAN_POINT ( 'NONE',  ( -1.082677165354329896, 0.07958543189024085140, 0.2665933059059887866 ) ) ;
#48567 = CARTESIAN_POINT ( 'NONE',  ( 1.305774278215223960, -0.6692913385826771977, 0.1292274648535927661 ) ) ;
#48568 = CARTESIAN_POINT ( 'NONE',  ( 2.586150256253534785, 1.653403552777528596, -0.4602852883866567768 ) ) ;
#48569 = CARTESIAN_POINT ( 'NONE',  ( -0.2559055118110230564, 0.1660481256975883668, -0.3530559997133364547 ) ) ;
#48570 = CARTESIAN_POINT ( 'NONE',  ( -1.272965879265091305, -0.004921259842519870586, -0.3153832671262229437 ) ) ;
#48571 = CIRCLE ( 'NONE', #71407, 0.5118110236220471121 ) ;
#48572 = CARTESIAN_POINT ( 'NONE',  ( -0.5249343832020990641, -0.6046776061558809534, -0.2411417322834644161 ) ) ;
#48573 = CARTESIAN_POINT ( 'NONE',  ( -1.456692913385826182, 0.1771653543307087630, 0.000000000000000000 ) ) ;
#48574 = CARTESIAN_POINT ( 'NONE',  ( 0.2867679344610366554, -0.2867679344610365999, -0.4101243026584795448 ) ) ;
#48575 = CARTESIAN_POINT ( 'NONE',  ( 0.3805774278215230400, 0.05413385826771626580, -0.4176697321401330321 ) ) ;
#48576 = DIRECTION ( 'NONE',  ( -3.096699300667737957E-16, 1.000000000000000000, -0.000000000000000000 ) ) ;
#48577 = CARTESIAN_POINT ( 'NONE',  ( 1.286089238845145033, 0.2306618581243848609, 0.2411417322834645549 ) ) ;
#48578 = CARTESIAN_POINT ( 'NONE',  ( -1.157146581871515012E-16, 0.4724409448818898682, -2.124015748031495843 ) ) ;
#48579 = CARTESIAN_POINT ( 'NONE',  ( -1.135170603674539924, -0.6692913385826771977, 0.1292274648535927661 ) ) ;
#48580 = CARTESIAN_POINT ( 'NONE',  ( -0.4002624671916004129, -0.08942795157528024563, -0.3641732283464568787 ) ) ;
#48581 = CARTESIAN_POINT ( 'NONE',  ( -0.5052493438320202479, 0.2066929133858267098, -0.1054918080437494132 ) ) ;
#48582 = CARTESIAN_POINT ( 'NONE',  ( -0.1706036745406816491, 0.05413385826771626580, -0.4176697321401330321 ) ) ;
#48583 = CARTESIAN_POINT ( 'NONE',  ( 0.2493438320209980519, -0.004921259842519576551, 0.3153832671262227771 ) ) ;
#48584 = CARTESIAN_POINT ( 'NONE',  ( -1.076115485564303809, 0.1283753931104748280, 0.1820866141732283561 ) ) ;
#48585 = CARTESIAN_POINT ( 'NONE',  ( -1.410761154855642463, -0.05778040916215522460, 0.4822834645669289988 ) ) ;
#48586 = CARTESIAN_POINT ( 'NONE',  ( -1.456692913385826182, -0.6692913385826771977, 8.415575281601705876E-17 ) ) ;
#48587 = CARTESIAN_POINT ( 'NONE',  ( 1.292650918635171564, -0.6692913385826773087, -0.1292274648535924053 ) ) ;
#48588 = LINE ( 'NONE', #68386, #43397 ) ;
#48589 = CARTESIAN_POINT ( 'NONE',  ( 0.3412073490813655186, -0.5023911411419708095, -0.1820866141732282451 ) ) ;
#48590 = CARTESIAN_POINT ( 'NONE',  ( 1.023622047244095334, -0.1870078740157479769, 0.4822834645669291653 ) ) ;
#48591 = CYLINDRICAL_SURFACE ( 'NONE', #59538, 0.4724409448818898682 ) ;
#48592 = CARTESIAN_POINT ( 'NONE',  ( 1.430446194225722500, -0.004921259842519576551, 0.3153832671262227771 ) ) ;
#48593 = ORIENTED_EDGE ( 'NONE', *, *, #7888, .T. ) ;
#48594 = CARTESIAN_POINT ( 'NONE',  ( -1.167979002624671470, 0.05413385826771666132, 0.4176697321401328100 ) ) ;
#48595 = EDGE_CURVE ( 'NONE', #50169, #64186, #48844, .T. ) ;
#48596 = CARTESIAN_POINT ( 'NONE',  ( -0.7808398950131222316, -0.3162353388693409650, -0.4822834645669289433 ) ) ;
#48597 = CARTESIAN_POINT ( 'NONE',  ( 0.2559055118110243332, -0.5400638737290845981, -0.3530559997133363437 ) ) ;
#48598 = CARTESIAN_POINT ( 'NONE',  ( -9.787531504996567848E-17, 0.3996062992125986035, -1.920830620545185230E-17 ) ) ;
#48599 = CARTESIAN_POINT ( 'NONE',  ( 0.3996062992125984925, 0.1070741851644054637, -2.091207349081364963 ) ) ;
#48600 = CARTESIAN_POINT ( 'NONE',  ( 0.8136482939632553313, 0.2306618581243848609, 0.2411417322834645549 ) ) ;
#48601 = CARTESIAN_POINT ( 'NONE',  ( 1.528871391076116026, -0.5511811023622048555, -0.09757992244046775898 ) ) ;
#48602 = CARTESIAN_POINT ( 'NONE',  ( 0.07217847769028949700, -0.3162353388693405765, 0.4822834645669290543 ) ) ;
#48603 = CARTESIAN_POINT ( 'NONE',  ( 0.6167979002624678353, -0.4281496062992124485, 0.4176697321401328655 ) ) ;
#48604 = B_SPLINE_CURVE_WITH_KNOTS ( 'NONE', 3,
 ( #70259, #58465, #6705, #32374, #45409, #63538, #76181, #7124, #82903, #58038, #77421, #63950, #44568, #19755, #20174, #828, #13869, #24810, #76589, #45824, #12614, #71523, #63127, #6287, #5465, #31962, #31127, #57623, #47494, #28563, #60137, #65216, #28147, #9214, #46669, #73186, #79105, #40366, #47078, #65643, #7555, #7973, #21424, #33636, #1248, #26897, #54219, #53803, #2488, #14711, #78265, #34887, #39528, #33226, #2067, #52556, #34471, #20596, #72769, #59299 ),
 .UNSPECIFIED., .F., .F.,
 ( 4, 2, 2, 2, 2, 2, 2, 2, 2, 2, 2, 2, 2, 2, 2, 2, 2, 2, 2, 2, 2, 2, 2, 2, 2, 2, 2, 2, 2, 4 ),
 ( 0.01323639539072392866, 0.01388181161316760608, 0.01452722783561128175, 0.01581806028049860535, 0.01710889272538592895, 0.01839972517027324908, 0.02098139006004787199, 0.02356305494982249837, 0.02485388739470980463, 0.02614471983959711088, 0.02743555228448441713, 0.02872638472937171991, 0.03130804961914634282, 0.03259888206403365601, 0.03388971450892096227, 0.03453513073136461886, 0.03518054695380826852, 0.03647137939869557477, 0.03776221184358288796, 0.03905304428847020115, 0.04034387673335750740, 0.04163470917824481365, 0.04421637406801944697, 0.04679803895779408723, 0.04937970384756872749, 0.05067053629245604762, 0.05196136873734337469, 0.05325220118223069482, 0.05389761740467436529, 0.05454303362711803577 ),
 .UNSPECIFIED. ) ;
#48605 = CARTESIAN_POINT ( 'NONE',  ( -0.2925321140481932924, 0.2925321140481931814, -1.594488188976378229 ) ) ;
#48606 = CARTESIAN_POINT ( 'NONE',  ( -0.1058382717557497937, -0.3949938075777411628, -1.017060367454068359 ) ) ;
#48607 = CARTESIAN_POINT ( 'NONE',  ( -0.1070741851644051862, -0.3996062992125987146, -2.276902887139107268 ) ) ;
#48608 = CARTESIAN_POINT ( 'NONE',  ( 0.2362204724409449064, 0.4091458600556404646, -0.6167979002624671692 ) ) ;
#48609 = CARTESIAN_POINT ( 'NONE',  ( -0.1049643490035301885, -0.3917322834645671215, -0.06430446194225716838 ) ) ;
#48610 = CARTESIAN_POINT ( 'NONE',  ( -0.03937007874015669567, -0.5511811023622047445, 6.969142054262312111E-17 ) ) ;
#48611 = CIRCLE ( 'NONE', #24393, 2.559055118110236560 ) ;
#48612 = CARTESIAN_POINT ( 'NONE',  ( -0.3477690288713905509, -0.6692913385826771977, 0.1292274648535927661 ) ) ;
#48613 = CARTESIAN_POINT ( 'NONE',  ( 0.6824146981627303710, 0.2306618581243847221, -0.2411417322834647770 ) ) ;
#48614 = CARTESIAN_POINT ( 'NONE',  ( 0.3949938075777409408, -0.1058382717557499186, -2.078083989501312345 ) ) ;
#48615 = CARTESIAN_POINT ( 'NONE',  ( 0.1246719160104994284, 0.1771653543307087075, -0.09757992244046823083 ) ) ;
#48616 = CARTESIAN_POINT ( 'NONE',  ( -1.227034120734907141, -0.6692913385826773087, -0.1292274648535924053 ) ) ;
#48617 = CARTESIAN_POINT ( 'NONE',  ( 1.220472440944882386, -0.6692913385826771977, 8.415575281601705876E-17 ) ) ;
#48618 = CARTESIAN_POINT ( 'NONE',  ( -0.4724409448818899238, 0.1265901696524986686, -2.237532808398950301 ) ) ;
#48619 = CARTESIAN_POINT ( 'NONE',  ( -0.2925321140481930704, -0.2925321140481933480, -1.948818897637795144 ) ) ;
#48620 = CARTESIAN_POINT ( 'NONE',  ( -0.7426113562969628434, 2.209901789876557832, 0.5309055118110236338 ) ) ;
#48621 = VERTEX_POINT ( 'NONE', #77620 ) ;
#48622 = CARTESIAN_POINT ( 'NONE',  ( 0.8595800524934390507, -0.05778040916215560624, -0.4822834645669293319 ) ) ;
#48623 = CARTESIAN_POINT ( 'NONE',  ( 1.286089238845145033, 0.1283753931104748280, 0.1820866141732283561 ) ) ;
#48625 = CARTESIAN_POINT ( 'NONE',  ( 1.482939632545932307, 0.05413385826771626580, -0.4176697321401330321 ) ) ;
#48624 = CARTESIAN_POINT ( 'NONE',  ( 1.640419947506562393, -0.4281496062992124485, 0.4176697321401328655 ) ) ;
#48626 = CARTESIAN_POINT ( 'NONE',  ( 0.2867679344610365999, -0.2867679344610365999, -2.698143413876953556 ) ) ;
#48627 = PLANE ( 'NONE',  #70581 ) ;
#48628 = CARTESIAN_POINT ( 'NONE',  ( 1.115485564304462551, -0.4281496062992127816, -0.4176697321401328100 ) ) ;
#48629 = CARTESIAN_POINT ( 'NONE',  ( -1.692913385826770645, 0.2952755905511811885, 0.000000000000000000 ) ) ;
#48630 = CARTESIAN_POINT ( 'NONE',  ( -0.5971128608923877978, 0.2952755905511811885, 0.1292274648535926551 ) ) ;
#48631 = CARTESIAN_POINT ( 'NONE',  ( -0.6889763779527552368, -0.5400638737290845981, -0.3530559997133363437 ) ) ;
#48632 = CARTESIAN_POINT ( 'NONE',  ( 1.410761154855643795, -0.3162353388693405765, 0.4822834645669290543 ) ) ;
#48633 = CARTESIAN_POINT ( 'NONE',  ( -0.1049643490035302024, -0.3917322834645671215, -0.1568241469816273603 ) ) ;
#48634 = CARTESIAN_POINT ( 'NONE',  ( 0.1771653543307093182, 0.1660481256975885056, 0.3530559997133364547 ) ) ;
#48635 = CARTESIAN_POINT ( 'NONE',  ( -0.1049643490035302024, -0.3917322834645671215, -2.111548556430446144 ) ) ;
#48636 = EDGE_CURVE ( 'NONE', #29791, #35196, #10339, .T. ) ;
#48637 = CARTESIAN_POINT ( 'NONE',  ( -1.469816272965878357, 0.1283753931104748280, 0.1820866141732283561 ) ) ;
#48638 = ORIENTED_EDGE ( 'NONE', *, *, #28964, .T. ) ;
#48639 = CARTESIAN_POINT ( 'NONE',  ( 0.1058382717557500713, -0.3949938075777409408, -2.604986876640420501 ) ) ;
#48640 = EDGE_LOOP ( 'NONE', ( #63649, #14997 ) ) ;
#48641 = CARTESIAN_POINT ( 'NONE',  ( 3.937007874015748143, 2.755905511811024056, 0.5314960629921260393 ) ) ;
#48642 = CARTESIAN_POINT ( 'NONE',  ( -1.502624671916009680, -0.05778040916215560624, -0.4822834645669293319 ) ) ;
#48643 = CARTESIAN_POINT ( 'NONE',  ( 0.3460692066303959202, 0.1998031496062993295, -1.076115485564304475 ) ) ;
#48644 = CARTESIAN_POINT ( 'NONE',  ( 1.673228346456693494, 0.07958543189024085140, 0.2665933059059887866 ) ) ;
#48645 = CARTESIAN_POINT ( 'NONE',  ( 0.4091458600556404646, -0.2362204724409448231, -0.8116797900262466836 ) ) ;
#48646 = CARTESIAN_POINT ( 'NONE',  ( 0.4052866537519773660, 0.02791078216816386681, 0.4328096321851896966 ) ) ;
#48647 = CARTESIAN_POINT ( 'NONE',  ( 0.005815251566305920140, -0.3972027188793976760, -2.755905511808609099 ) ) ;
#48648 = CARTESIAN_POINT ( 'NONE',  ( 0.1958661417322834775, 0.3392501089628018884, 0.08595800524934374409 ) ) ;
#48649 = CARTESIAN_POINT ( 'NONE',  ( -0.2755905511811015396, -0.5511811023622047445, 6.969142054262312111E-17 ) ) ;
#48650 = CARTESIAN_POINT ( 'NONE',  ( -1.089238845144356427, -0.004921259842519576551, 0.3153832671262227771 ) ) ;
#48651 = CARTESIAN_POINT ( 'NONE',  ( -1.049868766404198794, -0.6046776061558807314, 0.2411417322834647770 ) ) ;
#48652 = CARTESIAN_POINT ( 'NONE',  ( 0.3477690288713918276, 0.2952755905511811885, 0.1292274648535926551 ) ) ;
#48653 = CARTESIAN_POINT ( 'NONE',  ( -1.482939632545930975, 0.05413385826771666132, 0.4176697321401328100 ) ) ;
#48654 = CARTESIAN_POINT ( 'NONE',  ( 0.3392501089628018329, 0.1958661417322835607, 0.03412073490813653104 ) ) ;
#48655 = ORIENTED_EDGE ( 'NONE', *, *, #42359, .T. ) ;
#48656 = CARTESIAN_POINT ( 'NONE',  ( -1.345144356955379816, -0.3162353388693405765, 0.4822834645669290543 ) ) ;
#48657 = CARTESIAN_POINT ( 'NONE',  ( -1.595398199321655275, 2.115458727241839476, -0.1559797534342494962 ) ) ;
#48658 = CARTESIAN_POINT ( 'NONE',  ( 0.4091458600556404646, -0.2362204724409448231, -1.679790026246719137 ) ) ;
#48659 = CARTESIAN_POINT ( 'NONE',  ( -1.157146581871515012E-16, 0.4724409448818898682, 0.000000000000000000 ) ) ;
#48660 = CARTESIAN_POINT ( 'NONE',  ( -0.3917322834645671215, 0.1049643490035301469, -0.8123359580052491591 ) ) ;
#48661 = CARTESIAN_POINT ( 'NONE',  ( -0.1049643490035301885, -0.3917322834645671215, -2.676509186351705871 ) ) ;
#48662 = CARTESIAN_POINT ( 'NONE',  ( -0.6167979002624665030, -0.4281496062992127816, -0.4176697321401328100 ) ) ;
#48663 = CARTESIAN_POINT ( 'NONE',  ( 1.318897637795276356, -0.5400638737290844871, 0.3530559997133364547 ) ) ;
#48665 = DIRECTION ( 'NONE',  ( 0.000000000000000000, 0.000000000000000000, -1.000000000000000000 ) ) ;
#48664 = DIRECTION ( 'NONE',  ( -1.000000000000000000, -0.000000000000000000, -0.000000000000000000 ) ) ;
#48666 = EDGE_CURVE ( 'NONE', #64697, #51414, #27340, .T. ) ;
#48667 = CARTESIAN_POINT ( 'NONE',  ( 0.1674892343164159914, -2.191421614605370878E-15, 0.4445507791589071167 ) ) ;
#48668 = CARTESIAN_POINT ( 'NONE',  ( -0.9055118110236215490, 0.2952755905511811885, 0.000000000000000000 ) ) ;
#48669 = CARTESIAN_POINT ( 'NONE',  ( -0.1958661417322834497, -0.3392501089628018884, -0.1456499755567436105 ) ) ;
#48670 = CARTESIAN_POINT ( 'NONE',  ( 0.1049868766404206816, -0.5023911411419708095, -0.1820866141732282451 ) ) ;
#48671 = CARTESIAN_POINT ( 'NONE',  ( 0.1049643490035304799, -0.3917322834645669549, -0.4849081364829397334 ) ) ;
#48672 = EDGE_CURVE ( 'NONE', #10674, #82069, #58261, .T. ) ;
#48673 = CARTESIAN_POINT ( 'NONE',  ( -0.09186351706036663400, -0.3690944881889763329, 0.3153832671262228327 ) ) ;
#48674 = CARTESIAN_POINT ( 'NONE',  ( 0.7545931758530188826, -0.5511811023622046335, 0.09757992244046803654 ) ) ;
#48675 = CARTESIAN_POINT ( 'NONE',  ( 0.5643044619422579178, -0.4281496062992127816, -0.4176697321401328100 ) ) ;
#48676 = AXIS2_PLACEMENT_3D ( 'NONE', #32003, #76626, #69890 ) ;
#48677 = CARTESIAN_POINT ( 'NONE',  ( -0.2165354330708654795, 0.07958543189024085140, 0.2665933059059887866 ) ) ;
#48678 = CARTESIAN_POINT ( 'NONE',  ( -0.3917322834645670104, -7.196005306013484475E-17, -2.393700787401574992 ) ) ;
#48679 = CARTESIAN_POINT ( 'NONE',  ( -1.620734908136482577, 0.2952755905511811885, 0.1292274648535926551 ) ) ;
#48680 = CARTESIAN_POINT ( 'NONE',  ( -0.8464566929133852113, 0.1660481256975885056, 0.3530559997133364547 ) ) ;
#48681 = CARTESIAN_POINT ( 'NONE',  ( -0.4724409448818898682, -8.678599364036362592E-17, -0.7460629921259841479 ) ) ;
#48682 = CARTESIAN_POINT ( 'NONE',  ( 0.05249343832021075018, 0.2306618581243847221, -0.2411417322834647770 ) ) ;
#48683 = CARTESIAN_POINT ( 'NONE',  ( -0.4921259842519677963, 0.1660481256975883668, -0.3530559997133364547 ) ) ;
#48684 = CARTESIAN_POINT ( 'NONE',  ( -0.4724409448818898682, -8.678599364036362592E-17, -0.6692913385826770867 ) ) ;
#48685 = CARTESIAN_POINT ( 'NONE',  ( 0.006561679790026889343, -0.08942795157527998196, 0.3641732283464567121 ) ) ;
#48686 = CARTESIAN_POINT ( 'NONE',  ( -0.2296587926509179312, -0.3162353388693409650, -0.4822834645669289433 ) ) ;
#48687 = CARTESIAN_POINT ( 'NONE',  ( -0.6299212598425188991, -0.1870078740157480879, -0.4822834645669291653 ) ) ;
#48688 = CARTESIAN_POINT ( 'NONE',  ( 1.604771003085129433, 0.7270283685441701893, -0.1466069496707750053 ) ) ;
#48689 = CARTESIAN_POINT ( 'NONE',  ( -1.012922870834580324, 5.991678263669262536E-15, 0.4118484887281945728 ) ) ;
#48690 = CARTESIAN_POINT ( 'NONE',  ( 0.1049868766404206816, 0.2306618581243848609, 0.2411417322834645549 ) ) ;
#48691 = CARTESIAN_POINT ( 'NONE',  ( -0.1070741851644051862, -0.3996062992125986590, -2.038713910761154491 ) ) ;
#48692 = CARTESIAN_POINT ( 'NONE',  ( 1.574803149606299746, -0.1870078740157479769, 0.4822834645669291653 ) ) ;
#48693 = CARTESIAN_POINT ( 'NONE',  ( -0.4461942257217840213, 0.1283753931104748280, 0.1820866141732283561 ) ) ;
#48694 = CARTESIAN_POINT ( 'NONE',  ( -0.5511811023622041894, -0.1870078740157480879, -0.4822834645669291653 ) ) ;
#48695 = CARTESIAN_POINT ( 'NONE',  ( 1.640419947506562393, -0.4281496062992124485, 0.4176697321401328655 ) ) ;
#48696 = CARTESIAN_POINT ( 'NONE',  ( 1.305774278215223960, -0.6692913385826771977, 0.1292274648535927661 ) ) ;
#48697 = CARTESIAN_POINT ( 'NONE',  ( -1.482939632545930975, 0.05413385826771666132, 0.4176697321401328100 ) ) ;
#48698 = CARTESIAN_POINT ( 'NONE',  ( -0.6692913385826764205, -0.5511811023622047445, 6.969142054262312111E-17 ) ) ;
#48699 = CARTESIAN_POINT ( 'NONE',  ( -0.3996062992125986035, 0.1070741851644051584, -0.1095800524934383430 ) ) ;
#48700 = CARTESIAN_POINT ( 'NONE',  ( 0.3460692066303959757, -0.1998031496062991907, -0.4199475065616797842 ) ) ;
#48701 = CARTESIAN_POINT ( 'NONE',  ( 0.1974969037888706369, -0.3420746716998659953, 0.06561679790026241077 ) ) ;
#48702 = CARTESIAN_POINT ( 'NONE',  ( 1.384514435695538559, 0.1771653543307087075, -0.09757992244046823083 ) ) ;
#48703 = CARTESIAN_POINT ( 'NONE',  ( 1.318897637795276356, 0.07958543189024071263, -0.2665933059059888421 ) ) ;
#48704 = CARTESIAN_POINT ( 'NONE',  ( 0.8858267716535438430, -0.5400638737290845981, -0.3530559997133363437 ) ) ;
#48705 = CARTESIAN_POINT ( 'NONE',  ( 0.4330708661417329020, 0.2066929133858268208, 0.000000000000000000 ) ) ;
#48706 = B_SPLINE_CURVE_WITH_KNOTS ( 'NONE', 3,
 ( #4594, #12572, #37416, #82455, #63088, #43705, #76551, #23953, #25595, #25184, #31088, #24363, #51258, #75315, #17662, #68990, #24770, #62678, #38230, #11339, #36999, #82862, #63907, #50439, #69408, #6243, #56755, #5020, #76960, #36579, #19288, #30688, #82050, #50033, #76140, #18481, #44123, #71064, #27272, #13408, #19710, #21383, #77804, #39063, #53356, #70637, #59672, #65601, #20557 ),
 .UNSPECIFIED., .F., .F.,
 ( 4, 2, 2, 2, 2, 2, 2, 2, 2, 2, 2, 2, 2, 1, 2, 2, 2, 2, 2, 2, 2, 2, 2, 2, 4 ),
 ( 0.004857456657547474382, 0.007214810972081309864, 0.008393488129348227605, 0.009572165286615145346, 0.01192951960114899991, 0.01310819675841591939, 0.01428687391568283019, 0.01546555107294974273, 0.01664422823021665526, 0.01900158254475048034, 0.02135893685928430541, 0.02371629117381813048, 0.02489496833108504129, 0.02607364548835195209, 0.02725232264561886983, 0.02843099980288578063, 0.03078835411741961264, 0.03196703127468653038, 0.03314570843195344119, 0.03550306274648727667, 0.03668173990375418747, 0.03786041706102111215, 0.04021777137555496151, 0.04139644853282188619, 0.04257512569008879699 ),
 .UNSPECIFIED. ) ;
#48707 = CARTESIAN_POINT ( 'NONE',  ( 0.7414698162729663755, -0.6692913385826773087, -0.1292274648535924053 ) ) ;
#48708 = CARTESIAN_POINT ( 'NONE',  ( 0.3949938075777409408, -0.1058382717557499186, -0.9757217847769031893 ) ) ;
#48709 = CARTESIAN_POINT ( 'NONE',  ( 1.141732283464567788, -0.5511811023622047445, 6.969142054262312111E-17 ) ) ;
#48710 = CARTESIAN_POINT ( 'NONE',  ( 0.1837270341207357105, -0.6046776061558809534, -0.2411417322834644161 ) ) ;
#48711 = CARTESIAN_POINT ( 'NONE',  ( -0.9448818897637790704, -0.1870078740157480879, -0.4822834645669291653 ) ) ;
#48712 = CARTESIAN_POINT ( 'NONE',  ( 1.233595800524935227, 0.2306618581243847221, -0.2411417322834647770 ) ) ;
#48713 = CARTESIAN_POINT ( 'NONE',  ( -0.4724409448818899238, 0.1265901696524986686, -0.9776902887139107268 ) ) ;
#48714 = CARTESIAN_POINT ( 'NONE',  ( 0.3460692066303959757, -0.1998031496062991907, -2.467191601049868677 ) ) ;
#48715 = CARTESIAN_POINT ( 'NONE',  ( 0.2296587926509192634, -0.08942795157528024563, -0.3641732283464568787 ) ) ;
#48716 = ORIENTED_EDGE ( 'NONE', *, *, #815, .F. ) ;
#48717 = CARTESIAN_POINT ( 'NONE',  ( -0.2867679344610367109, 0.2867679344610365444, -0.8038250900600545368 ) ) ;
#48718 = VERTEX_POINT ( 'NONE', #3917 ) ;
#48719 = AXIS2_PLACEMENT_3D ( 'NONE', #78074, #39333, #65860 ) ;
#48720 = CARTESIAN_POINT ( 'NONE',  ( -0.6824146981627291497, -0.6046776061558809534, -0.2411417322834644161 ) ) ;
#48721 = CARTESIAN_POINT ( 'NONE',  ( -0.4002624671916004129, -0.3162353388693405765, 0.4822834645669290543 ) ) ;
#48722 = CARTESIAN_POINT ( 'NONE',  ( -0.3871391076115476282, -0.05778040916215522460, 0.4822834645669289988 ) ) ;
#48723 = CARTESIAN_POINT ( 'NONE',  ( 0.7545931758530189937, 0.2952755905511810774, -0.1292274648535930714 ) ) ;
#48724 = CARTESIAN_POINT ( 'NONE',  ( -0.8989501312335946848, -0.6692913385826771977, 0.1292274648535927661 ) ) ;
#48725 = CARTESIAN_POINT ( 'NONE',  ( -0.4790026246719154557, -0.3162353388693405765, 0.4822834645669290543 ) ) ;
#48726 = CARTESIAN_POINT ( 'NONE',  ( 1.181102362204724976, -0.1870078740157480879, -0.4822834645669291653 ) ) ;
#48727 = CARTESIAN_POINT ( 'NONE',  ( 0.4199475065616803948, -0.6046776061558809534, -0.2411417322834644161 ) ) ;
#48728 = CARTESIAN_POINT ( 'NONE',  ( 0.6299212598425204535, -0.1870078740157480879, -0.4822834645669291653 ) ) ;
#48729 = CARTESIAN_POINT ( 'NONE',  ( -0.3392501089628017219, -0.1958661417322836718, -0.8320209973753279753 ) ) ;
#48730 = CARTESIAN_POINT ( 'NONE',  ( -0.5839895013123351797, -0.5511811023622046335, 0.09757992244046803654 ) ) ;
#48731 = ORIENTED_EDGE ( 'NONE', *, *, #58543, .F. ) ;
#48732 = CARTESIAN_POINT ( 'NONE',  ( -0.3420746716998661618, 0.1974969037888702206, -1.443569553805774230 ) ) ;
#48733 = ORIENTED_EDGE ( 'NONE', *, *, #19980, .T. ) ;
#48734 = CARTESIAN_POINT ( 'NONE',  ( -0.7611548556430438595, 0.1283753931104748280, 0.1820866141732283561 ) ) ;
#48735 = CARTESIAN_POINT ( 'NONE',  ( -0.3346456692913377662, 0.1660481256975883668, -0.3530559997133364547 ) ) ;
#48736 = CARTESIAN_POINT ( 'NONE',  ( -9.787531504996567848E-17, 0.3996062992125986035, 0.1574803149606299191 ) ) ;
#48737 = CARTESIAN_POINT ( 'NONE',  ( -0.6889763779527552368, -0.5400638737290845981, -0.3530559997133363437 ) ) ;
#48738 = CARTESIAN_POINT ( 'NONE',  ( -1.030183727034119867, -0.05778040916215560624, -0.4822834645669293319 ) ) ;
#48739 = CARTESIAN_POINT ( 'NONE',  ( -1.312335958005248715, 0.2306618581243848609, 0.2411417322834645549 ) ) ;
#48740 = CARTESIAN_POINT ( 'NONE',  ( -1.338582677165353729, -0.1870078740157480879, -0.4822834645669291653 ) ) ;
#48741 = CARTESIAN_POINT ( 'NONE',  ( 0.7545931758530189937, 0.1771653543307087075, -0.09757992244046823083 ) ) ;
#48742 = CARTESIAN_POINT ( 'NONE',  ( 0.2362204724409449064, 0.4091458600556404646, -0.3786089238845143923 ) ) ;
#48743 = CARTESIAN_POINT ( 'NONE',  ( -0.1265901696524986964, -0.4724409448818899238, -0.6213910761154856077 ) ) ;
#48744 = CARTESIAN_POINT ( 'NONE',  ( 0.4921259842519691285, 0.07958543189024085140, 0.2665933059059887866 ) ) ;
#48745 = CARTESIAN_POINT ( 'NONE',  ( 0.1377952755905518800, 0.1660481256975883668, -0.3530559997133364547 ) ) ;
#48746 = CARTESIAN_POINT ( 'NONE',  ( 0.1181102362204730916, 0.2952755905511811885, 0.000000000000000000 ) ) ;
#48747 = ORIENTED_EDGE ( 'NONE', *, *, #27995, .F. ) ;
#48748 = CARTESIAN_POINT ( 'NONE',  ( 0.2925321140481932369, -0.2925321140481932369, -1.830708661417322913 ) ) ;
#48749 = CARTESIAN_POINT ( 'NONE',  ( 0.5314960629920993940, 2.716535433070866645, 2.543486866223394482 ) ) ;
#48750 = ORIENTED_EDGE ( 'NONE', *, *, #67228, .T. ) ;
#48751 = CARTESIAN_POINT ( 'NONE',  ( -0.1070741851644056997, 0.3996062992125984925, -1.028215223097112663 ) ) ;
#48752 = CARTESIAN_POINT ( 'NONE',  ( 1.607611548556431069, 0.2952755905511811885, 0.1292274648535926551 ) ) ;
#48753 = CARTESIAN_POINT ( 'NONE',  ( -0.5577427821522301654, -0.08942795157528024563, -0.3641732283464568787 ) ) ;
#48754 = CARTESIAN_POINT ( 'NONE',  ( -1.030183727034119867, -0.05778040916215560624, -0.4822834645669293319 ) ) ;
#48755 = CARTESIAN_POINT ( 'NONE',  ( 0.4091458600556404646, -0.2362204724409448231, -0.4199475065616797842 ) ) ;
#48756 = LINE ( 'NONE', #1367, #35745 ) ;
#48757 = CARTESIAN_POINT ( 'NONE',  ( -0.3917322834645670104, -7.196005306013484475E-17, -2.328740157480315265 ) ) ;
#48758 = CARTESIAN_POINT ( 'NONE',  ( -1.417322834645668772, -0.1870078740157480601, -0.3641732283464567677 ) ) ;
#48759 = CARTESIAN_POINT ( 'NONE',  ( 0.6233595800524939223, -0.3162353388693405765, 0.4822834645669290543 ) ) ;
#48760 = CARTESIAN_POINT ( 'NONE',  ( 0.4921259842519691285, -0.5400638737290845981, -0.3530559997133363437 ) ) ;
#48761 = CARTESIAN_POINT ( 'NONE',  ( -0.5774278215223089816, -0.5023911411419708095, 0.1820866141732285504 ) ) ;
#48762 = CARTESIAN_POINT ( 'NONE',  ( 0.1115485564304467270, -0.6692913385826773087, -0.1292274648535924053 ) ) ;
#48763 = CARTESIAN_POINT ( 'NONE',  ( 0.4091458600556404646, -0.2362204724409448231, -2.386482939632545985 ) ) ;
#48764 = CARTESIAN_POINT ( 'NONE',  ( -0.2493438320209966919, 0.05413385826771626580, -0.4176697321401330321 ) ) ;
#48765 = EDGE_CURVE ( 'NONE', #63914, #39649, #80833, .T. ) ;
#48766 = CARTESIAN_POINT ( 'NONE',  ( 0.1058382717557500852, -0.3949938075777408852, -1.894356955380577245 ) ) ;
#48767 = CARTESIAN_POINT ( 'NONE',  ( 1.404199475065617264, -0.3690944881889763329, 0.3153832671262228327 ) ) ;
#48768 = CARTESIAN_POINT ( 'NONE',  ( 0.07874015748031558404, -0.1870078740157480601, -0.3641732283464567677 ) ) ;
#48769 = CARTESIAN_POINT ( 'NONE',  ( 1.312335958005250269, -0.5023911411419708095, 0.1820866141732285504 ) ) ;
#48770 = CARTESIAN_POINT ( 'NONE',  ( -1.082677165354329896, 0.1660481256975885056, 0.3530559997133364547 ) ) ;
#48771 = CARTESIAN_POINT ( 'NONE',  ( -1.338582677165353729, -0.1870078740157479769, 0.3641732283464567677 ) ) ;
#48772 = CARTESIAN_POINT ( 'NONE',  ( -3.210901149692899637, 2.729659893098101087, -0.5314960629921260393 ) ) ;
#48773 = CARTESIAN_POINT ( 'NONE',  ( -0.9776902887139098386, -0.6692913385826771977, 0.1292274648535927661 ) ) ;
#48774 = CARTESIAN_POINT ( 'NONE',  ( -0.3740157480314953431, 0.1660481256975885056, 0.3530559997133364547 ) ) ;
#48775 = CARTESIAN_POINT ( 'NONE',  ( 0.1968503937007881344, -0.6692913385826771977, 8.415575281601705876E-17 ) ) ;
#48776 = CARTESIAN_POINT ( 'NONE',  ( 0.1958661417322836162, -0.3392501089628018329, -2.534101419126297827 ) ) ;
#48777 = CARTESIAN_POINT ( 'NONE',  ( 1.090866038711136632, -3.876714527516387216E-16, -0.3791475997938230647 ) ) ;
#48778 = CARTESIAN_POINT ( 'NONE',  ( 0.1574803149606306130, -0.1870078740157480601, -0.3641732283464567677 ) ) ;
#48779 = CARTESIAN_POINT ( 'NONE',  ( 0.8530183727034126306, 0.05413385826771626580, -0.4176697321401330321 ) ) ;
#48780 = CARTESIAN_POINT ( 'NONE',  ( -1.496062992125983815, -0.1870078740157480601, -0.3641732283464567677 ) ) ;
#48781 =( BOUNDED_CURVE ( )  B_SPLINE_CURVE ( 2, ( #33287, #78324, #39159, #14358, #8441, #8853, #19816, #77481, #45465, #71163, #59356, #46727, #40015 ),
 .UNSPECIFIED., .F., .F. ) 
 B_SPLINE_CURVE_WITH_KNOTS ( ( 3, 2, 2, 2, 2, 2, 3 ),
 ( 0.3103969023887781509, 0.3106060606060606077, 0.3143939393939393923, 0.3181818181818181768, 0.3219696969696969613, 0.3257575757575757458, 0.3259667339748582027 ),
 .UNSPECIFIED. ) 
 CURVE ( )  GEOMETRIC_REPRESENTATION_ITEM ( )  RATIONAL_B_SPLINE_CURVE ( ( 0.9964447847208428577, 0.9981185001348096275, 1.000000000000000000, 0.9659258262890683122, 1.000000000000000000, 0.9659258262890683122, 1.000000000000000000, 0.9659258262890683122, 1.000000000000000000, 0.9659258262890683122, 1.000000000000000000, 0.9981185001348097385, 0.9964447847208430797 ) ) 
 REPRESENTATION_ITEM ( '' )  );
#48782 = CARTESIAN_POINT ( 'NONE',  ( 0.8333333333333340365, -0.6692913385826771977, 0.1292274648535927661 ) ) ;
#48783 = CARTESIAN_POINT ( 'NONE',  ( -1.410761154855642463, -0.08942795157527998196, 0.3641732283464567121 ) ) ;
#48784 = AXIS2_PLACEMENT_3D ( 'NONE', #19987, #14929, #51949 ) ;
#48785 = CARTESIAN_POINT ( 'NONE',  ( -1.423884514435694859, -0.3162353388693405765, 0.4822834645669290543 ) ) ;
#48786 = CARTESIAN_POINT ( 'NONE',  ( -1.043307086614172707, 0.1660481256975883668, -0.3530559997133364547 ) ) ;
#48787 = CARTESIAN_POINT ( 'NONE',  ( -0.2821522309711278487, -0.5511811023622048555, -0.09757992244046775898 ) ) ;
#48788 = DIRECTION ( 'NONE',  ( -0.000000000000000000, -0.000000000000000000, -1.000000000000000000 ) ) ;
#48789 = CARTESIAN_POINT ( 'NONE',  ( 0.7545931758530188826, -0.5511811023622046335, 0.09757992244046803654 ) ) ;
#48790 = CARTESIAN_POINT ( 'NONE',  ( -0.1574803149606292529, -0.1870078740157480879, -0.4822834645669291653 ) ) ;
#48791 = CARTESIAN_POINT ( 'NONE',  ( -0.1070741851644056997, 0.3996062992125984925, -0.3982939632545932085 ) ) ;
#48792 = CARTESIAN_POINT ( 'NONE',  ( -0.9580052493438311334, -0.4281496062992124485, 0.4176697321401328655 ) ) ;
#48793 = CARTESIAN_POINT ( 'NONE',  ( 0.3917322834645669549, 0.1049643490035304660, -1.941601049868766582 ) ) ;
#48794 = CARTESIAN_POINT ( 'NONE',  ( 0.8530183727034126306, -0.004921259842519870586, -0.3153832671262229437 ) ) ;
#48795 = CARTESIAN_POINT ( 'NONE',  ( -0.1443569553805765515, -0.4281496062992127816, -0.4176697321401328100 ) ) ;
#48796 = CARTESIAN_POINT ( 'NONE',  ( -0.1312335958005241554, -0.6046776061558809534, -0.2411417322834644161 ) ) ;
#48797 = CARTESIAN_POINT ( 'NONE',  ( -0.4002624671916004129, -0.2845877964562159024, 0.3641732283464567677 ) ) ;
#48798 = CARTESIAN_POINT ( 'NONE',  ( 1.141392835773559211, 0.3937007874015748254, 1.141392835773562764 ) ) ;
#48799 = CARTESIAN_POINT ( 'NONE',  ( -0.4593175853018364174, -0.3690944881889765550, -0.3153832671262227771 ) ) ;
#48800 = CARTESIAN_POINT ( 'NONE',  ( 0.2034120734908144990, -0.6692913385826771977, 0.1292274648535927661 ) ) ;
#48801 = CARTESIAN_POINT ( 'NONE',  ( -1.364829396325458521, 0.1283753931104746893, -0.1820866141732285504 ) ) ;
#48802 = CARTESIAN_POINT ( 'NONE',  ( -0.3996062992125986590, 0.1070741851644051723, -1.369422572178477404 ) ) ;
#48803 = CARTESIAN_POINT ( 'NONE',  ( 1.607611548556431069, 0.2952755905511811885, 0.1292274648535926551 ) ) ;
#48804 = CARTESIAN_POINT ( 'NONE',  ( -0.1265901696524993347, 0.4724409448818896462, -2.211286089238845065 ) ) ;
#48805 = ORIENTED_EDGE ( 'NONE', *, *, #51403, .T. ) ;
#48806 = CARTESIAN_POINT ( 'NONE',  ( -1.614173228346456268, -0.5511811023622047445, 6.969142054262312111E-17 ) ) ;
#48807 = CARTESIAN_POINT ( 'NONE',  ( -0.3608923884514428360, -0.6692913385826773087, -0.1292274648535924053 ) ) ;
#48808 = CARTESIAN_POINT ( 'NONE',  ( -1.089238845144356427, -0.4281496062992127816, -0.4176697321401328100 ) ) ;
#48809 = CARTESIAN_POINT ( 'NONE',  ( 4.797336870675656522E-17, -0.3917322834645670104, -1.738188976377952777 ) ) ;
#48810 = CARTESIAN_POINT ( 'NONE',  ( 0.3458507752293908943, -0.3458507752293908943, -2.145669291338582418 ) ) ;
#48811 = CARTESIAN_POINT ( 'NONE',  ( 1.509186351706037543, 0.05413385826771666132, 0.4176697321401328100 ) ) ;
#48812 = CARTESIAN_POINT ( 'NONE',  ( 0.2559055118110243332, 0.1660481256975885056, 0.3530559997133364547 ) ) ;
#48813 = CARTESIAN_POINT ( 'NONE',  ( 0.06192927228921586008, -0.3917322834645669549, -2.751902906291787687 ) ) ;
#48814 = CARTESIAN_POINT ( 'NONE',  ( 0.1070741851644053527, 0.3996062992125985480, -2.432414698162729483 ) ) ;
#48815 = CARTESIAN_POINT ( 'NONE',  ( -1.594488188976377563, -0.5400638737290844871, 0.3530559997133364547 ) ) ;
#48816 = CARTESIAN_POINT ( 'NONE',  ( 0.2925321140481932369, -0.2925321140481932369, -0.8858267716535430658 ) ) ;
#48817 = ORIENTED_EDGE ( 'NONE', *, *, #37615, .F. ) ;
#48818 = CARTESIAN_POINT ( 'NONE',  ( -0.7874015748031489847, -0.1870078740157480601, -0.3641732283464567677 ) ) ;
#48819 = CARTESIAN_POINT ( 'NONE',  ( 0.3917322834645670104, -0.1049643490035303411, -2.623359580052493367 ) ) ;
#48820 = ORIENTED_EDGE ( 'NONE', *, *, #58440, .F. ) ;
#48821 = CARTESIAN_POINT ( 'NONE',  ( 0.6758530183727039509, 0.2952755905511810774, -0.1292274648535930714 ) ) ;
#48822 = CARTESIAN_POINT ( 'NONE',  ( -0.1837270341207343505, -0.6046776061558807314, 0.2411417322834647770 ) ) ;
#48823 = CARTESIAN_POINT ( 'NONE',  ( -1.108923884514435132, -0.05778040916215560624, -0.4822834645669293319 ) ) ;
#48824 = CARTESIAN_POINT ( 'NONE',  ( 1.056430446194226658, 0.2952755905511811885, 0.1292274648535926551 ) ) ;
#48825 = CARTESIAN_POINT ( 'NONE',  ( -1.181102362204723644, -0.1870078740157479769, 0.3641732283464567677 ) ) ;
#48826 = CARTESIAN_POINT ( 'NONE',  ( 6.372542394380578105E-15, 1.062992125984252523, -1.629220936382730134 ) ) ;
#48827 = CARTESIAN_POINT ( 'NONE',  ( 0.1640419947506569498, -0.3162353388693409650, -0.4822834645669289433 ) ) ;
#48828 = CARTESIAN_POINT ( 'NONE',  ( -0.9120734908136475250, -0.6692913385826773087, -0.1292274648535924053 ) ) ;
#48829 = CARTESIAN_POINT ( 'NONE',  ( -0.3392501089628019439, 0.1958661417322832554, -1.366122416501625469 ) ) ;
#48830 = CARTESIAN_POINT ( 'NONE',  ( 1.601049868766404982, 0.2306618581243848609, 0.2411417322834645549 ) ) ;
#48831 = CARTESIAN_POINT ( 'NONE',  ( -0.7426113562972000981, 2.362204724409448620, -0.5309055118110235227 ) ) ;
#48832 = CARTESIAN_POINT ( 'NONE',  ( 0.9580052493438327987, -0.4281496062992127816, -0.4176697321401328100 ) ) ;
#48833 = CARTESIAN_POINT ( 'NONE',  ( -0.3917322834645671215, 0.1049643490035301469, -2.637139107611548461 ) ) ;
#48834 = CARTESIAN_POINT ( 'NONE',  ( 1.345144356955381593, -0.08942795157527998196, 0.3641732283464567121 ) ) ;
#48835 = VERTEX_POINT ( 'NONE', #29168 ) ;
#48836 = CARTESIAN_POINT ( 'NONE',  ( 0.3917322834645670659, 2.398668435337828261E-17, -2.792014066438007092 ) ) ;
#48837 = CARTESIAN_POINT ( 'NONE',  ( -0.6167979002624665030, -0.4281496062992127816, -0.4176697321401328100 ) ) ;
#48838 = VERTEX_POINT ( 'NONE', #53999 ) ;
#48839 = CARTESIAN_POINT ( 'NONE',  ( 0.2362204724409456558, -0.1870078740157480601, -0.3641732283464567677 ) ) ;
#48840 = CARTESIAN_POINT ( 'NONE',  ( -1.456692913385826182, -0.6692913385826771977, 8.415575281601705876E-17 ) ) ;
#48841 = CARTESIAN_POINT ( 'NONE',  ( 0.6233595800524939223, -0.3162353388693405765, 0.4822834645669290543 ) ) ;
#48842 = CARTESIAN_POINT ( 'NONE',  ( 0.7414698162729663755, -0.6692913385826773087, -0.1292274648535924053 ) ) ;
#48843 = CARTESIAN_POINT ( 'NONE',  ( -0.07874015748031421014, -0.1870078740157480879, -0.4822834645669291653 ) ) ;
#48844 = CIRCLE ( 'NONE', #23311, 0.3149606299212597271 ) ;
#48845 = CARTESIAN_POINT ( 'NONE',  ( 0.3392501089628018329, 0.1958661417322835607, -1.230334276411760186 ) ) ;
#48846 = CARTESIAN_POINT ( 'NONE',  ( -0.9514435695538050464, -0.05778040916215560624, -0.4822834645669293319 ) ) ;
#48847 = CARTESIAN_POINT ( 'NONE',  ( 0.1049643490035303689, 0.3917322834645670104, -2.440288713910760521 ) ) ;
#48848 = CARTESIAN_POINT ( 'NONE',  ( -1.633858267716534529, -0.5400638737290845981, -0.3530559997133363437 ) ) ;
#48849 = CARTESIAN_POINT ( 'NONE',  ( -1.122047244094487306, 0.1660481256975883668, -0.3530559997133364547 ) ) ;
#48850 = CARTESIAN_POINT ( 'NONE',  ( 1.358267716535433323, 0.1660481256975885056, 0.3530559997133364547 ) ) ;
#48851 = CARTESIAN_POINT ( 'NONE',  ( 1.076115485564305141, 0.2306618581243847221, -0.2411417322834647770 ) ) ;
#48852 = CARTESIAN_POINT ( 'NONE',  ( -0.3996062992125987146, 0.1070741851644051862, -0.3477690288713909950 ) ) ;
#48853 = CARTESIAN_POINT ( 'NONE',  ( -1.062992125984250968, 0.2952755905511811885, 0.000000000000000000 ) ) ;
#48854 = CARTESIAN_POINT ( 'NONE',  ( -0.1998031496062991630, -0.3460692066303959202, 0.1725721784776902690 ) ) ;
#48855 = CARTESIAN_POINT ( 'NONE',  ( 0.4396325459317590445, -0.6692913385826771977, 0.1292274648535927661 ) ) ;
#48856 = CARTESIAN_POINT ( 'NONE',  ( -0.3996062992125986035, -0.1070741851644056997, -2.250656167979002920 ) ) ;
#48857 = EDGE_CURVE ( 'NONE', #25753, #35562, #65661, .T. ) ;
#48858 = CARTESIAN_POINT ( 'NONE',  ( -0.4527559055118102749, -0.5400638737290845981, -0.3530559997133363437 ) ) ;
#48859 = CARTESIAN_POINT ( 'NONE',  ( 1.653543307086614789, -0.1870078740157479769, 0.4822834645669291653 ) ) ;
#48860 = CARTESIAN_POINT ( 'NONE',  ( 0.5708661417322842269, 0.07958543189024085140, 0.2665933059059887866 ) ) ;
#48861 = CARTESIAN_POINT ( 'NONE',  ( 1.338582677165355062, -0.1870078740157480879, -0.4822834645669291653 ) ) ;
#48862 = CARTESIAN_POINT ( 'NONE',  ( -0.4724409448818895907, -0.1265901696524993070, -0.9101049868766404316 ) ) ;
#48863 = CARTESIAN_POINT ( 'NONE',  ( 0.8595800524934390507, -0.2845877964562159024, 0.3641732283464567677 ) ) ;
#48864 = CARTESIAN_POINT ( 'NONE',  ( 0.8136482939632553313, 0.2306618581243848609, 0.2411417322834645549 ) ) ;
#48865 = ADVANCED_FACE ( 'NONE', ( #61984 ), #80127, .F. ) ;
#48866 = CARTESIAN_POINT ( 'NONE',  ( -0.2891555358219909388, -0.2891555358219912164, -0.6082677165354331006 ) ) ;
#48867 = CARTESIAN_POINT ( 'NONE',  ( -0.9973753280839886548, -0.6046776061558809534, -0.2411417322834644161 ) ) ;
#48868 = CARTESIAN_POINT ( 'NONE',  ( -1.603475055217291612, 2.157339783260149080, 0.04573490813648253134 ) ) ;
#48869 = CARTESIAN_POINT ( 'NONE',  ( 1.200787401574803681, -0.4536011799217368745, -0.2665933059059886201 ) ) ;
#48870 = CARTESIAN_POINT ( 'NONE',  ( -0.7874015748031489847, -0.1870078740157479769, 0.4822834645669291653 ) ) ;
#48871 = CARTESIAN_POINT ( 'NONE',  ( 0.05905511811023681640, 0.1660481256975883668, -0.3530559997133364547 ) ) ;
#48872 = CARTESIAN_POINT ( 'NONE',  ( 0.4678109194727930187, 1.617842475621884768, -1.019880138406202175 ) ) ;
#48873 = CARTESIAN_POINT ( 'NONE',  ( -0.08530183727034056085, -0.05778040916215560624, -0.4822834645669293319 ) ) ;
#48874 = CARTESIAN_POINT ( 'NONE',  ( 0.6889763779527566800, -0.4536011799217367080, 0.2665933059059888421 ) ) ;
#48875 = CARTESIAN_POINT ( 'NONE',  ( -0.1265901696524986964, -0.4724409448818899238, -0.1489501312335957672 ) ) ;
#48876 = CARTESIAN_POINT ( 'NONE',  ( 0.1509186351706045259, -0.08942795157528024563, -0.3641732283464568787 ) ) ;
#48877 = CARTESIAN_POINT ( 'NONE',  ( 0.8595800524934390507, -0.08942795157528024563, -0.3641732283464568787 ) ) ;
#48878 = DIRECTION ( 'NONE',  ( 0.8050726085550603539, 2.493067783899206833E-16, -0.5931762764594944448 ) ) ;
#48879 = CARTESIAN_POINT ( 'NONE',  ( 0.3996062992125984925, 0.1070741851644054637, -1.933727034120735100 ) ) ;
#48880 = CARTESIAN_POINT ( 'NONE',  ( 0.4855643044619430415, -0.4281496062992127816, -0.4176697321401328100 ) ) ;
#48881 = CARTESIAN_POINT ( 'NONE',  ( -0.3917322834645670104, -7.196005306013484475E-17, -0.9763779527559053317 ) ) ;
#48882 = CARTESIAN_POINT ( 'NONE',  ( 1.430446194225722500, -0.3690944881889765550, -0.3153832671262227771 ) ) ;
#48883 = CARTESIAN_POINT ( 'NONE',  ( -0.3089825338611873473, 0.2417350488526503194, 6.867566722516314874E-18 ) ) ;
#48884 = CARTESIAN_POINT ( 'NONE',  ( 0.1115485564304467270, -0.5511811023622048555, -0.09757992244046775898 ) ) ;
#48885 = CARTESIAN_POINT ( 'NONE',  ( 0.006561679790026889343, -0.3162353388693409650, -0.4822834645669289433 ) ) ;
#48886 = CARTESIAN_POINT ( 'NONE',  ( 1.246719160104987623, -0.004921259842519870586, -0.3153832671262229437 ) ) ;
#48887 = CARTESIAN_POINT ( 'NONE',  ( -1.397637795275589623, 0.07958543189024085140, 0.2665933059059887866 ) ) ;
#48888 = CARTESIAN_POINT ( 'NONE',  ( -1.443569553805773564, -0.6046776061558807314, 0.2411417322834647770 ) ) ;
#48889 = CARTESIAN_POINT ( 'NONE',  ( 0.3149606299212606708, -0.1870078740157480879, -0.4822834645669291653 ) ) ;
#48890 = CARTESIAN_POINT ( 'NONE',  ( 1.049868766404200349, 0.2306618581243848609, 0.2411417322834645549 ) ) ;
#48891 = CARTESIAN_POINT ( 'NONE',  ( 1.604771003085129433, 1.320215725944020813, -0.1466069496707750330 ) ) ;
#48892 = CARTESIAN_POINT ( 'NONE',  ( 0.3412073490813655186, 0.2306618581243848609, 0.2411417322834645549 ) ) ;
#48893 = CARTESIAN_POINT ( 'NONE',  ( 1.200787401574803681, 0.1660481256975885056, 0.3530559997133364547 ) ) ;
#48894 = CARTESIAN_POINT ( 'NONE',  ( 0.9251968503937015864, 0.1660481256975883668, -0.3530559997133364547 ) ) ;
#48895 = CARTESIAN_POINT ( 'NONE',  ( -1.614173228346457378, 1.330640075373402897, -0.1372047244094477536 ) ) ;
#48896 = CARTESIAN_POINT ( 'NONE',  ( 0.8005249343832028242, -0.3690944881889765550, -0.3153832671262227771 ) ) ;
#48897 = CARTESIAN_POINT ( 'NONE',  ( -1.561679790026246017, -0.3690944881889765550, -0.3153832671262227771 ) ) ;
#48898 = CARTESIAN_POINT ( 'NONE',  ( -0.05249343832020938322, -0.5023911411419708095, -0.1820866141732282451 ) ) ;
#48899 = AXIS2_PLACEMENT_3D ( 'NONE', #59888, #46422, #14051 ) ;
#48900 = CARTESIAN_POINT ( 'NONE',  ( -0.09842519685039295696, -0.5400638737290844871, 0.3530559997133364547 ) ) ;
#48901 = CARTESIAN_POINT ( 'NONE',  ( 0.8923884514435701520, -0.6046776061558809534, -0.2411417322834644161 ) ) ;
#48902 = CARTESIAN_POINT ( 'NONE',  ( -0.2690288713910754526, -0.6692913385826771977, 0.1292274648535927661 ) ) ;
#48903 = CARTESIAN_POINT ( 'NONE',  ( -0.3917322834645670659, -7.196005306013484475E-17, -2.083352649115172373 ) ) ;
#48904 = CARTESIAN_POINT ( 'NONE',  ( -0.1049868766404193215, 0.1283753931104746893, -0.1820866141732285504 ) ) ;
#48905 = CARTESIAN_POINT ( 'NONE',  ( 0.9120734908136489683, -0.6692913385826771977, 0.1292274648535927661 ) ) ;
#48906 = CARTESIAN_POINT ( 'NONE',  ( 0.9580052493438327987, -0.3690944881889765550, -0.3153832671262227771 ) ) ;
#48907 =( BOUNDED_SURFACE ( )  B_SPLINE_SURFACE ( 3, 2, ( 
 ( #13089, #58516, #46720, #77473, #58941, #51770, #13924, #72412, #78317, #77051, #14761, #8025, #59349, #6753, #7176, #40417, #38742, #13497, #40008, #71995, #33280, #27363, #77896, #39153, #20647, #26109, #39581, #46301, #58088, #19810, #1299, #32847, #65270, #6340, #33688, #19384, #32012, #1708, #57672, #453, #879, #34, #52192, #20227, #25687, #51348, #26948, #45036, #45875, #71573, #52611, #2540, #16007, #80403, #47131, #48373, #28616, #29026, #9678, #72822, #8846, #28198, #54693, #15172, #41654, #22715, #35760, #74073, #40828, #53857, #61011, #16419, #61427, #8434, #42065, #66098, #34522, #79156, #9268, #15590, #41248, #67760, #3776, #22303, #47964, #10095, #73666, #66514, #66935, #29440, #79990, #35349, #2951, #23123, #34104, #55099, #80807, #48791, #79569, #53448, #67345, #60189, #74489, #16836, #59765, #2119, #21885, #3362, #27785, #21473, #47549, #73240, #34939, #60602, #54274, #76133, #76545, #4183, #61842, #81217, #49615, #44117, #17252, #36992, #82856, #4588, #62672, #81637, #17655, #43697, #5012, #30682, #18064, #36168, #11754, #82448, #63490, #23947, #12158, #5824, #25176, #69809, #37410, #24357, #36573, #29845, #55509, #75309, #55923, #50845, #31496, #42471, #75724, #11332, #23533, #56343, #57156, #82044, #63082, #49202, #37814, #50026, #68173, #69402, #5420, #10515, #68574, #74903, #42880, #10916, #62251, #31082, #56749, #18474, #30259, #24764, #43287, #68984, #50432, #19704, #33588, #20550, #77372, #51669, #76954, #18873, #354, #1201, #38642, #25589, #13824, #14248, #58843, #52088, #775, #32328, #19282, #13402, #57989, #77798, #26437, #32749, #64320, #45362, #6237, #59253, #26011, #39483, #71058, #44522, #20130, #52926, #52510, #58416, #39056, #12566, #64740, #33175, #7078, #1610, #46202, #44933, #27266, #45778, #65170, #70630, #70210, #51252, #6654, #26851, #78218, #65594, #63900, #71476, #7506, #83266, #71897, #39906, #12987, #38224, #7927, #57574, #31913, #2021, #60912, #46622, #8339, #14664, #66836, #47032, #3263, #60090, #53351, #34005, #9170, #54172, #79060, #15072, #21378, #67658, #48276, #66000, #40730, #35660, #53757, #22616, #41964, #72726, #79886, #66414, #40321, #27686, #41558, #28102, #73565, #34841, #59667, #79468, #78640, #15909, #72317, #9995, #20963, #29342, #73974, #61323, #8750, #34423, #16320, #73141, #67247, #2444, #3678, #15490, #21785, #60503, #2852, #47446, #41147, #28515, #22204, #47860, #9578, #35248, #28924, #54592, #80302, #75212, #18379, #55413, #4495, #55824, #69713, #56650, #30162, #81532, #29750, #55003, #36479, #37311, #74805, #61745, #49929, #50337, #11653, #4910, #36895, #68480, #81120, #49519, #10818, #30581, #62571, #68885, #17152, #23852, #42373, #12057, #62154, #75627, #17556, #80710, #56247, #5723, #5324, #11235, #43189, #48691, #81943, #69304, #24256, #37714, #82350, #23436, #63388, #17965, #43602, #49101, #23025, #4082, #42785, #62985, #30982, #44020, #16732, #24669, #76034, #36074, #74388, #68071, #10416, #14145, #65060, #70112, #64222, #38125, #13721, #82751, #44417, #50747, #19597, #83166, #39375, #12882, #6137, #12463, #45260, #6974, #31812, #51152, #57472, #20446, #1098, #18774, #76846, #71792, #6556, #58736, #78113, #25486, #32643, #19180, #76446, #63799, #77694, #32228, #26327, #70956, #44829, #57886, #31394, #51989, #25073, #13301, #70526, #253, #26749, #38953, #673, #51565, #39797, #57059, #46099, #65492, #38542, #25904, #77268, #64637, #58307, #7397, #20024, #52404, #45675, #71371, #33066, #2343, #9477, #40218, #60403, #15386, #8236, #52826, #2753, #35151, #27164, #1510, #20863, #78957, #54073, #14566, #66312, #41463, #59566, #8651, #53242, #46931, #21685, #34322, #40630, #79366, #59153, #47348, #9072, #47764, #21275, #79788, #73462, #67148, #22104, #73037, #27999, #33902, #78538, #46513, #72623 ),
 ( #65900, #72214, #7824, #33491, #14971, #15814, #1922, #27585, #41048, #59984, #53658, #66733, #34743, #28413, #14432, #1377, #58169, #32506, #57751, #83029, #64498, #65353, #19465, #6421, #77977, #78397, #39663, #32931, #64921, #13170, #113, #77559, #38820, #58596, #7259, #13582, #45115, #538, #70390, #40084, #6836, #20307, #26191, #25352, #965, #33769, #33358, #39236, #51852, #76713, #19893, #14006, #45540, #51014, #20729, #71238, #45957, #38404, #52689, #26619, #46380, #52273, #71654, #72073, #25768, #32090, #19046, #44693, #12745, #7691, #59021, #27028, #64084, #65771, #8103, #51429, #77132, #70823, #74153, #61092, #34606, #8929, #34184, #59430, #40913, #41728, #79236, #66180, #54357, #54777, #16083, #9345, #41332, #72902, #59848, #53939, #15254, #35016, #67012, #73324, #21551, #60271, #46799, #16500, #66594, #80069, #2621, #1785, #60680, #10178, #9755, #15670, #28277, #53106, #79651, #73747, #21968, #42144, #3443, #2200, #67839, #3029, #22386, #27868, #27445, #8517, #47212, #67422, #35427, #22793, #21144, #47630, #28695, #40499, #29107, #48046, #53528, #78815, #80480, #14839, #48453, #72490, #61341, #61761, #11253, #55840, #56263, #67263, #41573, #60929, #29359, #23867, #80318, #16750, #62587, #67675, #42389, #3694, #80727, #23452, #68088, #10433, #81136, #15926, #74823, #62170, #43205, #55018, #75228, #68900, #4929, #49534, #17167, #4099, #16338, #9596, #35264, #23041, #35676, #30597, #3279, #22220, #81549, #17572, #22633, #48708, #36911, #28943, #74406, #30178, #4509, #49117, #47876, #36090, #29767, #10835, #41981, #55428, #36494, #54609, #73580, #42801, #68495, #48294, #73991, #10011, #44037, #44848, #63001, #31830, #70546, #51584, #6575, #30999, #69729, #76867, #64240, #77286, #24274, #32246, #81959, #50353, #11671, #25093, #31412, #57076, #271, #19617, #38145, #63817, #12901, #6156, #82367, #82770, #45279, #12481, #51171, #18792, #38972, #49945, #70974, #13319, #64655, #12074, #69320, #57491, #5340, #57906, #6993, #32661, #75643, #76051, #83183, #25505, #17982, #24686, #50765, #37732, #19199, #43619, #25926, #37328, #56667, #18395, #63405, #5741, #76466, #44437, #70130, #38560, #20465, #78556, #14163, #33507, #59584, #20881, #52845, #33919, #52007, #27603, #14990, #79384, #39819, #28016, #21703, #15407, #60005, #53263, #40235, #52422, #20042, #45693, #65508, #71812, #66756, #47366, #9090, #8255, #27181, #39395, #46533, #73057, #46118, #78974, #7840, #65918, #41067, #46948, #66331, #58328, #71390, #59169, #1527, #65079, #8669, #21295, #7417, #690, #34340, #13739, #72233, #2360, #53676, #77712, #14582, #33087, #1941, #26767, #26346, #72640, #58754, #1116, #40647, #78132, #35170, #54509, #9497, #23773, #4417, #22123, #80223, #75138, #9910, #62079, #81456, #60831, #35999, #3183, #79807, #67167, #81045, #67578, #29674, #48614, #47782, #35582, #34762, #55336, #2773, #49444, #60422, #68811, #30086, #29264, #23358, #73484, #55748, #54928, #17483, #74308, #16655, #43114, #28847, #41482, #28433, #54092, #15834, #67992, #49029, #10747, #22539, #80635, #48202, #73897, #61245, #3599, #16237, #36404, #22946, #42295, #41885, #10337, #61669, #17074, #4010, #74725, #42711, #68407, #51073, #44344, #76369, #24593, #69224, #5650, #50261, #70035, #18702, #24995, #56574, #69635, #81869, #25826, #75959, #6062, #18296, #36815, #12389, #45173, #44752, #50669, #43941, #4825, #11981, #25410, #37635, #77188, #12806, #11572, #51485, #38046, #31733, #37231, #62491, #17889, #82275, #76772, #62909, #30504, #43526, #63311, #19104, #70448, #57806, #56166, #31316, #56981, #75550, #38460, #57398, #5243, #19520, #64146, #49850, #82678, #6480, #32149, #24181, #63722, #30907, #83088, #172, #11157, #52327, #45598, #26249, #59073, #46435, #71292, #7315, #13639, #59901, #40551, #58226, #32984, #27919 ),
 ( #20363, #70879, #8156, #38878, #34240, #13228, #21605, #66232, #65408, #33821, #51908, #8570, #7746, #2254, #27084, #1428, #53578, #39293, #77615, #64556, #6894, #32564, #20780, #59487, #46849, #19948, #33411, #79287, #64979, #46014, #71709, #593, #72544, #14063, #39717, #58652, #1019, #78033, #53158, #26672, #52747, #65823, #78454, #27501, #72126, #14484, #40138, #1841, #78870, #21195, #14891, #54832, #61145, #9396, #22441, #34661, #61979, #60733, #42199, #3085, #72955, #22848, #81355, #80942, #3497, #54411, #40969, #80122, #61569, #73799, #29981, #48927, #47682, #4316, #29163, #67895, #28332, #67475, #10648, #73377, #48100, #16136, #55644, #74627, #41782, #9809, #22022, #47265, #28749, #29573, #67064, #53994, #10233, #42611, #3912, #80537, #48509, #35481, #15727, #74209, #16555, #35900, #55235, #23257, #35067, #16971, #60324, #15306, #68311, #36303, #66651, #8987, #2673, #79706, #41382, #37537, #30809, #17385, #56474, #37948, #50160, #6379, #25311, #24080, #38364, #5553, #18604, #49750, #49339, #30395, #69120, #5962, #31632, #70350, #68710, #11469, #82177, #4721, #57292, #44247, #56061, #32051, #82990, #62384, #24493, #50975, #76673, #43016, #11885, #11051, #63213, #75450, #19005, #5144, #81770, #17788, #31217, #82578, #43423, #37126, #62810, #12705, #44654, #36709, #75856, #64040, #18198, #57711, #23667, #43833, #24897, #69535, #56885, #50566, #69936, #76270, #12292, #63625, #75039, #32889, #74, #20690, #51387, #46761, #25727, #34146, #78778, #77937, #46341, #38781, #53067, #20267, #21103, #39624, #13967, #72454, #26150, #6795, #77092, #19424, #45076, #33322, #72035, #59391, #1339, #45917, #71615, #58984, #70779, #52653, #40049, #14803, #39196, #40461, #66139, #8477, #1749, #78359, #65313, #77516, #13130, #64458, #7218, #13540, #32466, #58128, #495, #26990, #52234, #51811, #7652, #19851, #71197, #14391, #45500, #65735, #64879, #8068, #58558, #924, #27406, #26581, #33730, #34977, #48829, #40873, #66974, #67801, #42104, #3404, #15213, #74113, #29478, #9307, #34565, #59807, #41289, #10138, #79612, #66555, #54738, #55137, #16459, #9718, #41691, #73284, #60230, #54316, #15632, #35389, #67384, #73705, #21929, #60641, #47173, #74530, #2991, #80443, #28657, #2162, #61054, #10552, #35802, #16045, #80027, #53488, #22346, #61469, #48006, #42513, #3817, #2580, #16876, #29067, #22753, #28239, #27828, #8888, #47590, #80848, #23160, #68216, #21514, #48413, #79198, #53899, #72864, #57920, #42918, #20055, #70988, #74945, #70143, #13332, #7007, #29884, #25519, #55547, #51184, #4626, #45292, #18806, #10953, #17290, #76882, #12916, #36610, #55963, #62289, #26360, #32675, #23571, #51598, #68613, #19631, #83197, #284, #64254, #30297, #81676, #23987, #25939, #49654, #70560, #77300, #58341, #38985, #76479, #44451, #32259, #64668, #703, #61879, #52020, #36210, #12495, #49242, #63831, #38158, #6169, #77726, #45708, #19213, #44861, #71404, #38573, #31844, #57506, #4220, #6588, #81256, #33932, #54104, #13752, #60434, #2785, #79820, #27194, #1129, #21307, #78145, #79396, #28445, #66769, #47794, #7853, #27614, #78987, #22136, #14175, #72245, #52858, #53277, #39409, #47379, #65092, #58766, #33100, #52435, #20894, #15419, #71825, #8267, #7430, #59182, #59597, #78568, #14594, #15002, #1952, #46960, #72652, #26779, #66344, #53688, #34775, #46547, #9102, #20477, #46131, #41080, #8682, #40659, #33519, #39833, #65522, #40247, #65930, #1539, #34352, #60018, #2373, #28030, #21715, #73070, #4841, #61257, #42721, #35594, #81055, #36830, #62090, #60844, #56178, #49456, #43126, #48215, #48626, #62503, #54522, #80647, #81467, #55761, #17084, #23785, #24193, #74736, #68417, #9923, #23371, #68824, #29686, #4022, #11169, #16251, #80237, #73498, #15846, #35183, #49039, #10757, #75150, #22553, #10350, #30516 ),
 ( #36417, #73911, #41898, #3611, #4432, #67592, #30098, #17495, #81881, #41495, #29277, #54941, #67181, #9510, #3196, #28860, #22960, #74321, #16668, #42307, #68005, #36011, #61681, #55349, #70891, #6073, #31747, #12818, #57409, #50273, #50682, #19531, #63734, #19115, #70046, #6906, #49862, #13241, #38890, #32578, #63323, #37246, #83102, #30919, #32162, #64569, #45188, #606, #43952, #25421, #51086, #58240, #75970, #25009, #5661, #76783, #75562, #185, #17902, #11586, #69238, #5255, #56993, #51497, #24604, #44355, #43539, #11992, #12400, #31328, #76380, #44764, #38057, #70461, #38475, #62922, #64159, #6492, #56585, #82690, #82286, #18311, #69648, #77202, #57818, #25838, #37646, #18714, #13652, #33425, #39730, #34675, #72968, #60338, #59500, #78468, #7328, #20793, #40984, #27515, #53171, #46028, #1853, #40563, #32996, #8582, #72142, #72556, #78886, #58666, #52340, #71722, #14903, #1031, #21207, #66244, #79300, #34254, #26685, #14078, #46862, #59915, #21618, #51923, #2270, #26262, #78047, #39305, #52760, #59086, #1441, #27933, #47278, #65835, #8168, #53591, #33833, #20376, #27098, #15319, #40151, #66664, #46449, #9003, #77628, #19960, #45611, #71305, #65426, #64992, #7759, #14498, #68324, #49355, #55658, #36723, #80135, #16568, #67909, #11065, #3098, #61159, #41797, #42213, #75052, #36317, #2686, #47696, #22036, #41396, #9824, #4329, #60746, #80550, #43029, #48115, #22862, #67488, #3510, #3927, #48523, #74223, #61582, #79719, #55249, #42627, #23681, #35494, #81368, #17399, #68724, #29995, #80956, #10245, #22456, #73391, #15742, #29179, #16150, #28346, #54007, #67078, #35916, #54846, #9410, #29586, #35080, #73813, #23271, #48940, #74642, #28762, #16984, #54425, #10662, #61992, #32065, #37140, #37553, #51405, #43437, #69551, #70364, #44669, #5977, #12719, #13146, #31648, #38379, #62399, #63639, #57306, #82191, #12306, #76687, #69134, #64055, #24912, #25325, #83004, #11486, #5160, #24508, #50989, #62825, #37963, #19021, #57726, #6395, #30824, #50175, #89, #25742, #77107, #4738, #19439, #30411, #56489, #75464, #5567, #11899, #63227, #45090, #70794, #18618, #44261, #56079, #69952, #75870, #31232, #81784, #76287, #24095, #82593, #49764, #17803, #18213, #43848, #56899, #50580, #26166, #46357, #19867, #21118, #2177, #8494, #72880, #32906, #52667, #20705, #47188, #39211, #13982, #77953, #78374, #27844, #72469, #38797, #513, #58144, #77532, #45931, #40477, #13555, #33337, #79213, #938, #58998, #20282, #39638, #40062, #1354, #27005, #14408, #32481, #8082, #78794, #59822, #71630, #34161, #53505, #21529, #66155, #33745, #72051, #58573, #51827, #45516, #65329, #52248, #64473, #6810, #71212, #65749, #7666, #64896, #59406, #7233, #26596, #1763, #27420, #53081, #46778, #14818, #2596, #81272, #74548, #68234, #73299, #73722, #4236, #79628, #22363, #23177, #80865, #28254, #34992, #55564, #16061, #42532, #61895, #41304, #16476, #15648, #60248, #47605, #61487, #48022, #10155, #29084, #53915, #41708, #15229, #35821, #66570, #29900, #40888, #49259, #10569, #9735, #3835, #21946, #36226, #35406, #23588, #54754, #80460, #8904, #66990, #9322, #34580, #60657, #3006, #48432, #29495, #16893, #28673, #61070, #54334, #80044, #67400, #74131, #3421, #55154, #22769, #42123, #67818, #48847, #56397, #57208, #11388, #81692, #69860, #70266, #31551, #24816, #56801, #5065, #49671, #69455, #30734, #50483, #82500, #5472, #37045, #50079, #62305, #6293, #82095, #12211, #24409, #17307, #76187, #25643, #25230, #31134, #75775, #68629, #18116, #5878, #43749, #57629, #76595, #75361, #31968, #18524, #37869, #17709, #42935, #24003, #62727, #82909, #50895, #38280, #36628, #11805, #37460, #55981, #18925, #63544, #43337, #42331, #44574, #30313, #63133, #12621, #63956, #10969, #44167, #4642, #74961, #69038, #59306, #32804, #26066 ) ),
 .UNSPECIFIED., .F., .F., .F. ) 
 B_SPLINE_SURFACE_WITH_KNOTS ( ( 4, 4 ),
 ( 3, 2, 2, 2, 2, 2, 2, 2, 2, 2, 2, 2, 2, 2, 2, 2, 2, 2, 2, 2, 2, 2, 2, 2, 2, 2, 2, 2, 2, 2, 2, 2, 2, 2, 2, 2, 2, 2, 2, 2, 2, 2, 2, 2, 2, 2, 2, 2, 2, 2, 2, 2, 2, 2, 2, 2, 2, 2, 2, 2, 2, 2, 2, 2, 2, 2, 2, 2, 2, 2, 2, 2, 2, 2, 2, 2, 2, 2, 2, 2, 2, 2, 2, 2, 2, 2, 2, 2, 2, 2, 2, 2, 2, 2, 2, 2, 2, 2, 2, 2, 2, 2, 2, 2, 2, 2, 2, 2, 2, 2, 2, 2, 2, 2, 2, 2, 2, 2, 2, 2, 2, 2, 2, 2, 2, 2, 2, 2, 2, 2, 2, 2, 2, 2, 2, 2, 2, 2, 2, 2, 2, 2, 2, 2, 2, 2, 2, 2, 2, 2, 2, 2, 2, 2, 2, 2, 2, 2, 2, 2, 2, 2, 2, 2, 2, 2, 2, 2, 2, 2, 2, 2, 2, 2, 2, 2, 2, 2, 2, 2, 2, 2, 2, 2, 2, 2, 2, 2, 2, 2, 2, 2, 2, 2, 2, 2, 2, 2, 2, 2, 2, 2, 2, 2, 2, 2, 2, 2, 2, 2, 2, 2, 2, 2, 2, 2, 2, 2, 2, 2, 2, 2, 2, 2, 2, 2, 2, 2, 2, 2, 2, 2, 2, 2, 2, 2, 2, 3 ),
 ( 0.000000000000000000, 1.000000000000000000 ),
 ( 0.000000000000000000, 0.004166666666666666609, 0.008333333333333333218, 0.01250000000000000069, 0.01666666666666666644, 0.02083333333333333218, 0.02500000000000000139, 0.02916666666666666713, 0.03333333333333333287, 0.03749999999999999861, 0.04166666666666666435, 0.04583333333333333010, 0.05000000000000000278, 0.05416666666666666852, 0.05833333333333333426, 0.06250000000000000000, 0.06666666666666666574, 0.07083333333333333148, 0.07499999999999999722, 0.07916666666666666297, 0.08333333333333332871, 0.08749999999999999445, 0.09166666666666666019, 0.09583333333333333981, 0.1000000000000000056, 0.1041666666666666713, 0.1083333333333333370, 0.1125000000000000028, 0.1166666666666666685, 0.1208333333333333343, 0.1250000000000000000, 0.1291666666666666796, 0.1333333333333333315, 0.1375000000000000111, 0.1416666666666666630, 0.1458333333333333426, 0.1499999999999999944, 0.1541666666666666741, 0.1583333333333333259, 0.1625000000000000056, 0.1666666666666666574, 0.1708333333333333370, 0.1749999999999999889, 0.1791666666666666685, 0.1833333333333333204, 0.1875000000000000000, 0.1916666666666666796, 0.1958333333333333315, 0.2000000000000000111, 0.2041666666666666630, 0.2083333333333333426, 0.2124999999999999944, 0.2166666666666666741, 0.2208333333333333259, 0.2250000000000000056, 0.2291666666666666574, 0.2333333333333333370, 0.2374999999999999889, 0.2416666666666666685, 0.2458333333333333204, 0.2500000000000000000, 0.2541666666666666519, 0.2583333333333333592, 0.2625000000000000111, 0.2666666666666666630, 0.2708333333333333148, 0.2750000000000000222, 0.2791666666666666741, 0.2833333333333333259, 0.2874999999999999778, 0.2916666666666666852, 0.2958333333333333370, 0.2999999999999999889, 0.3041666666666666408, 0.3083333333333333481, 0.3125000000000000000, 0.3166666666666666519, 0.3208333333333333592, 0.3250000000000000111, 0.3291666666666666630, 0.3333333333333333148, 0.3375000000000000222, 0.3416666666666666741, 0.3458333333333333259, 0.3499999999999999778, 0.3541666666666666852, 0.3583333333333333370, 0.3624999999999999889, 0.3666666666666666408, 0.3708333333333333481, 0.3750000000000000000, 0.3791666666666666519, 0.3833333333333333592, 0.3875000000000000111, 0.3916666666666666630, 0.3958333333333333148, 0.4000000000000000222, 0.4041666666666666741, 0.4083333333333333259, 0.4124999999999999778, 0.4166666666666666852, 0.4208333333333333370, 0.4249999999999999889, 0.4291666666666666408, 0.4333333333333333481, 0.4375000000000000000, 0.4416666666666666519, 0.4458333333333333592, 0.4500000000000000111, 0.4541666666666666630, 0.4583333333333333148, 0.4625000000000000222, 0.4666666666666666741, 0.4708333333333333259, 0.4749999999999999778, 0.4791666666666666852, 0.4833333333333333370, 0.4874999999999999889, 0.4916666666666666408, 0.4958333333333333481, 0.5000000000000000000, 0.5041666666666666519, 0.5083333333333333037, 0.5124999999999999556, 0.5166666666666667185, 0.5208333333333333703, 0.5250000000000000222, 0.5291666666666666741, 0.5333333333333333259, 0.5374999999999999778, 0.5416666666666666297, 0.5458333333333332815, 0.5500000000000000444, 0.5541666666666666963, 0.5583333333333333481, 0.5625000000000000000, 0.5666666666666666519, 0.5708333333333333037, 0.5749999999999999556, 0.5791666666666667185, 0.5833333333333333703, 0.5875000000000000222, 0.5916666666666666741, 0.5958333333333333259, 0.5999999999999999778, 0.6041666666666666297, 0.6083333333333332815, 0.6125000000000000444, 0.6166666666666666963, 0.6208333333333333481, 0.6250000000000000000, 0.6291666666666666519, 0.6333333333333333037, 0.6374999999999999556, 0.6416666666666667185, 0.6458333333333333703, 0.6500000000000000222, 0.6541666666666666741, 0.6583333333333333259, 0.6624999999999999778, 0.6666666666666666297, 0.6708333333333332815, 0.6750000000000000444, 0.6791666666666666963, 0.6833333333333333481, 0.6875000000000000000, 0.6916666666666666519, 0.6958333333333333037, 0.6999999999999999556, 0.7041666666666667185, 0.7083333333333333703, 0.7125000000000000222, 0.7166666666666666741, 0.7208333333333333259, 0.7249999999999999778, 0.7291666666666666297, 0.7333333333333332815, 0.7375000000000000444, 0.7416666666666666963, 0.7458333333333333481, 0.7500000000000000000, 0.7541666666666666519, 0.7583333333333333037, 0.7624999999999999556, 0.7666666666666667185, 0.7708333333333333703, 0.7750000000000000222, 0.7791666666666666741, 0.7833333333333333259, 0.7874999999999999778, 0.7916666666666666297, 0.7958333333333332815, 0.8000000000000000444, 0.8041666666666666963, 0.8083333333333333481, 0.8125000000000000000, 0.8166666666666666519, 0.8208333333333333037, 0.8249999999999999556, 0.8291666666666667185, 0.8333333333333333703, 0.8375000000000000222, 0.8416666666666666741, 0.8458333333333333259, 0.8499999999999999778, 0.8541666666666666297, 0.8583333333333332815, 0.8625000000000000444, 0.8666666666666666963, 0.8708333333333333481, 0.8750000000000000000, 0.8791666666666666519, 0.8833333333333333037, 0.8874999999999999556, 0.8916666666666667185, 0.8958333333333333703, 0.9000000000000000222, 0.9041666666666666741, 0.9083333333333333259, 0.9124999999999999778, 0.9166666666666666297, 0.9208333333333332815, 0.9250000000000000444, 0.9291666666666666963, 0.9333333333333333481, 0.9375000000000000000, 0.9416666666666666519, 0.9458333333333333037, 0.9499999999999999556, 0.9541666666666667185, 0.9583333333333333703, 0.9625000000000000222, 0.9666666666666666741, 0.9708333333333333259, 0.9749999999999999778, 0.9791666666666666297, 0.9833333333333332815, 0.9875000000000000444 ),
 .UNSPECIFIED. ) 
 GEOMETRIC_REPRESENTATION_ITEM ( )  RATIONAL_B_SPLINE_SURFACE ( (
 ( 1.000000000000000000, 0.9659258262890683122, 1.000000000000000000, 0.9659258262890683122, 1.000000000000000000, 0.9659258262890683122, 1.000000000000000000, 0.9659258262890683122, 1.000000000000000000, 0.9659258262890683122, 1.000000000000000000, 0.9659258262890683122, 1.000000000000000000, 0.9659258262890683122, 1.000000000000000000, 0.9659258262890683122, 1.000000000000000000, 0.9659258262890683122, 1.000000000000000000, 0.9659258262890683122, 1.000000000000000000, 0.9659258262890683122, 1.000000000000000000, 0.9659258262890683122, 1.000000000000000000, 0.9659258262890683122, 1.000000000000000000, 0.9659258262890683122, 1.000000000000000000, 0.9659258262890683122, 1.000000000000000000, 0.9659258262890683122, 1.000000000000000000, 0.9659258262890683122, 1.000000000000000000, 0.9659258262890683122, 1.000000000000000000, 0.9659258262890683122, 1.000000000000000000, 0.9659258262890683122, 1.000000000000000000, 0.9659258262890683122, 1.000000000000000000, 0.9659258262890683122, 1.000000000000000000, 0.9659258262890683122, 1.000000000000000000, 0.9659258262890683122, 1.000000000000000000, 0.9659258262890683122, 1.000000000000000000, 0.9659258262890683122, 1.000000000000000000, 0.9659258262890683122, 1.000000000000000000, 0.9659258262890683122, 1.000000000000000000, 0.9659258262890683122, 1.000000000000000000, 0.9659258262890683122, 1.000000000000000000, 0.9659258262890683122, 1.000000000000000000, 0.9659258262890683122, 1.000000000000000000, 0.9659258262890683122, 1.000000000000000000, 0.9659258262890683122, 1.000000000000000000, 0.9659258262890683122, 1.000000000000000000, 0.9659258262890683122, 1.000000000000000000, 0.9659258262890683122, 1.000000000000000000, 0.9659258262890683122, 1.000000000000000000, 0.9659258262890683122, 1.000000000000000000, 0.9659258262890683122, 1.000000000000000000, 0.9659258262890683122, 1.000000000000000000, 0.9659258262890683122, 1.000000000000000000, 0.9659258262890683122, 1.000000000000000000, 0.9659258262890683122, 1.000000000000000000, 0.9659258262890683122, 1.000000000000000000, 0.9659258262890683122, 1.000000000000000000, 0.9659258262890683122, 1.000000000000000000, 0.9659258262890683122, 1.000000000000000000, 0.9659258262890683122, 1.000000000000000000, 0.9659258262890683122, 1.000000000000000000, 0.9659258262890683122, 1.000000000000000000, 0.9659258262890683122, 1.000000000000000000, 0.9659258262890683122, 1.000000000000000000, 0.9659258262890683122, 1.000000000000000000, 0.9659258262890683122, 1.000000000000000000, 0.9659258262890683122, 1.000000000000000000, 0.9659258262890683122, 1.000000000000000000, 0.9659258262890683122, 1.000000000000000000, 0.9659258262890683122, 1.000000000000000000, 0.9659258262890683122, 1.000000000000000000, 0.9659258262890683122, 1.000000000000000000, 0.9659258262890683122, 1.000000000000000000, 0.9659258262890683122, 1.000000000000000000, 0.9659258262890683122, 1.000000000000000000, 0.9659258262890683122, 1.000000000000000000, 0.9659258262890683122, 1.000000000000000000, 0.9659258262890683122, 1.000000000000000000, 0.9659258262890683122, 1.000000000000000000, 0.9659258262890683122, 1.000000000000000000, 0.9659258262890683122, 1.000000000000000000, 0.9659258262890683122, 1.000000000000000000, 0.9659258262890683122, 1.000000000000000000, 0.9659258262890683122, 1.000000000000000000, 0.9659258262890683122, 1.000000000000000000, 0.9659258262890683122, 1.000000000000000000, 0.9659258262890683122, 1.000000000000000000, 0.9659258262890683122, 1.000000000000000000, 0.9659258262890683122, 1.000000000000000000, 0.9659258262890683122, 1.000000000000000000, 0.9659258262890683122, 1.000000000000000000, 0.9659258262890683122, 1.000000000000000000, 0.9659258262890683122, 1.000000000000000000, 0.9659258262890683122, 1.000000000000000000, 0.9659258262890683122, 1.000000000000000000, 0.9659258262890683122, 1.000000000000000000, 0.9659258262890683122, 1.000000000000000000, 0.9659258262890683122, 1.000000000000000000, 0.9659258262890683122, 1.000000000000000000, 0.9659258262890683122, 1.000000000000000000, 0.9659258262890683122, 1.000000000000000000, 0.9659258262890683122, 1.000000000000000000, 0.9659258262890683122, 1.000000000000000000, 0.9659258262890683122, 1.000000000000000000, 0.9659258262890683122, 1.000000000000000000, 0.9659258262890683122, 1.000000000000000000, 0.9659258262890683122, 1.000000000000000000, 0.9659258262890683122, 1.000000000000000000, 0.9659258262890683122, 1.000000000000000000, 0.9659258262890683122, 1.000000000000000000, 0.9659258262890683122, 1.000000000000000000, 0.9659258262890683122, 1.000000000000000000, 0.9659258262890683122, 1.000000000000000000, 0.9659258262890683122, 1.000000000000000000, 0.9659258262890683122, 1.000000000000000000, 0.9659258262890683122, 1.000000000000000000, 0.9659258262890683122, 1.000000000000000000, 0.9659258262890683122, 1.000000000000000000, 0.9659258262890683122, 1.000000000000000000, 0.9659258262890683122, 1.000000000000000000, 0.9659258262890683122, 1.000000000000000000, 0.9659258262890683122, 1.000000000000000000, 0.9659258262890683122, 1.000000000000000000, 0.9659258262890683122, 1.000000000000000000, 0.9659258262890683122, 1.000000000000000000, 0.9659258262890683122, 1.000000000000000000, 0.9659258262890683122, 1.000000000000000000, 0.9659258262890683122, 1.000000000000000000, 0.9659258262890683122, 1.000000000000000000, 0.9659258262890683122, 1.000000000000000000, 0.9659258262890683122, 1.000000000000000000, 0.9659258262890683122, 1.000000000000000000, 0.9659258262890683122, 1.000000000000000000, 0.9659258262890683122, 1.000000000000000000, 0.9659258262890683122, 1.000000000000000000, 0.9659258262890683122, 1.000000000000000000, 0.9659258262890683122, 1.000000000000000000, 0.9659258262890683122, 1.000000000000000000, 0.9659258262890683122, 1.000000000000000000, 0.9659258262890683122, 1.000000000000000000, 0.9659258262890683122, 1.000000000000000000, 0.9659258262890683122, 1.000000000000000000, 0.9659258262890683122, 1.000000000000000000, 0.9659258262890683122, 1.000000000000000000, 0.9659258262890683122, 1.000000000000000000, 0.9659258262890683122, 1.000000000000000000, 0.9659258262890683122, 1.000000000000000000, 0.9659258262890683122, 1.000000000000000000, 0.9659258262890683122, 1.000000000000000000, 0.9659258262890683122, 1.000000000000000000, 0.9659258262890683122, 1.000000000000000000, 0.9659258262890683122, 1.000000000000000000, 0.9659258262890683122, 1.000000000000000000, 0.9659258262890683122, 1.000000000000000000, 0.9659258262890683122, 1.000000000000000000, 0.9659258262890683122, 1.000000000000000000, 0.9659258262890683122, 1.000000000000000000, 0.9659258262890683122, 1.000000000000000000, 0.9659258262890683122, 1.000000000000000000, 0.9659258262890683122, 1.000000000000000000, 0.9659258262890683122, 1.000000000000000000, 0.9659258262890683122, 1.000000000000000000, 0.9659258262890683122, 1.000000000000000000, 0.9659258262890683122, 1.000000000000000000, 0.9659258262890683122, 1.000000000000000000, 0.9659258262890683122, 1.000000000000000000, 0.9659258262890683122, 1.000000000000000000, 0.9659258262890683122, 1.000000000000000000, 0.9659258262890683122, 1.000000000000000000, 0.9659258262890683122, 1.000000000000000000, 0.9659258262890683122, 1.000000000000000000, 0.9659258262890683122, 1.000000000000000000, 0.9659258262890683122, 1.000000000000000000, 0.9659258262890683122, 1.000000000000000000, 0.9659258262890683122, 1.000000000000000000, 0.9659258262890683122, 1.000000000000000000, 0.9659258262890683122, 1.000000000000000000, 0.9659258262890683122, 1.000000000000000000, 0.9659258262890683122, 1.000000000000000000, 0.9659258262890683122, 1.000000000000000000, 0.9659258262890683122, 1.000000000000000000, 0.9659258262890683122, 1.000000000000000000, 0.9659258262890683122, 1.000000000000000000, 0.9659258262890683122, 1.000000000000000000, 0.9659258262890683122, 1.000000000000000000, 0.9659258262890683122, 1.000000000000000000, 0.9659258262890683122, 1.000000000000000000, 0.9659258262890683122, 1.000000000000000000, 0.9659258262890683122, 1.000000000000000000, 0.9659258262890683122, 1.000000000000000000, 0.9659258262890683122, 1.000000000000000000, 0.9659258262890683122, 1.000000000000000000, 0.9659258262890683122, 1.000000000000000000, 0.9659258262890683122, 1.000000000000000000, 0.9659258262890683122, 1.000000000000000000, 0.9659258262890683122, 1.000000000000000000, 0.9659258262890683122, 1.000000000000000000, 0.9659258262890683122, 1.000000000000000000, 0.9659258262890683122, 1.000000000000000000, 0.9659258262890683122, 1.000000000000000000, 0.9659258262890683122, 1.000000000000000000, 0.9659258262890683122, 1.000000000000000000, 0.9659258262890683122, 1.000000000000000000, 0.9659258262890683122, 1.000000000000000000, 0.9659258262890683122, 1.000000000000000000, 0.9659258262890683122, 1.000000000000000000, 0.9659258262890683122, 1.000000000000000000, 0.9659258262890683122, 1.000000000000000000, 0.9659258262890683122, 1.000000000000000000, 0.9659258262890683122, 1.000000000000000000, 0.9659258262890683122, 1.000000000000000000, 0.9659258262890683122, 1.000000000000000000, 0.9659258262890683122, 1.000000000000000000, 0.9659258262890683122, 1.000000000000000000, 0.9659258262890683122, 1.000000000000000000, 0.9659258262890683122, 1.000000000000000000, 0.9659258262890683122, 1.000000000000000000, 0.9659258262890683122, 1.000000000000000000, 0.9659258262890683122, 1.000000000000000000, 0.9659258262890683122, 1.000000000000000000, 0.9659258262890683122, 1.000000000000000000, 0.9659258262890683122, 1.000000000000000000, 0.9659258262890683122, 1.000000000000000000, 0.9659258262890683122, 1.000000000000000000, 0.9659258262890683122, 1.000000000000000000, 0.9659258262890683122, 1.000000000000000000, 0.9659258262890683122, 1.000000000000000000, 0.9659258262890683122, 1.000000000000000000, 0.9659258262890683122, 1.000000000000000000, 0.9659258262890683122, 1.000000000000000000, 0.9659258262890683122, 1.000000000000000000, 0.9659258262890683122, 1.000000000000000000, 0.9659258262890683122, 1.000000000000000000, 0.9659258262890683122, 1.000000000000000000, 0.9659258262890683122, 1.000000000000000000, 0.9659258262890683122, 1.000000000000000000, 0.9659258262890683122, 1.000000000000000000, 0.9659258262890683122, 1.000000000000000000, 0.9659258262890683122, 1.000000000000000000, 0.9659258262890683122, 1.000000000000000000, 0.9659258262890683122, 1.000000000000000000, 0.9659258262890683122, 1.000000000000000000, 0.9659258262890683122, 1.000000000000000000, 0.9659258262890683122, 1.000000000000000000, 0.9659258262890683122, 1.000000000000000000, 0.9659258262890683122, 1.000000000000000000, 0.9659258262890683122, 1.000000000000000000, 0.9659258262890683122, 1.000000000000000000),
 ( 0.8047378541243631611, 0.7773170766911672303, 0.8047378541243631611, 0.7773170766911672303, 0.8047378541243631611, 0.7773170766911672303, 0.8047378541243631611, 0.7773170766911672303, 0.8047378541243631611, 0.7773170766911672303, 0.8047378541243631611, 0.7773170766911672303, 0.8047378541243631611, 0.7773170766911672303, 0.8047378541243631611, 0.7773170766911672303, 0.8047378541243631611, 0.7773170766911672303, 0.8047378541243631611, 0.7773170766911672303, 0.8047378541243631611, 0.7773170766911672303, 0.8047378541243631611, 0.7773170766911672303, 0.8047378541243631611, 0.7773170766911672303, 0.8047378541243631611, 0.7773170766911672303, 0.8047378541243631611, 0.7773170766911672303, 0.8047378541243631611, 0.7773170766911672303, 0.8047378541243631611, 0.7773170766911672303, 0.8047378541243631611, 0.7773170766911672303, 0.8047378541243631611, 0.7773170766911672303, 0.8047378541243631611, 0.7773170766911672303, 0.8047378541243631611, 0.7773170766911672303, 0.8047378541243631611, 0.7773170766911672303, 0.8047378541243631611, 0.7773170766911672303, 0.8047378541243631611, 0.7773170766911672303, 0.8047378541243631611, 0.7773170766911672303, 0.8047378541243631611, 0.7773170766911672303, 0.8047378541243631611, 0.7773170766911672303, 0.8047378541243631611, 0.7773170766911672303, 0.8047378541243631611, 0.7773170766911672303, 0.8047378541243631611, 0.7773170766911672303, 0.8047378541243631611, 0.7773170766911672303, 0.8047378541243631611, 0.7773170766911672303, 0.8047378541243631611, 0.7773170766911672303, 0.8047378541243631611, 0.7773170766911672303, 0.8047378541243631611, 0.7773170766911672303, 0.8047378541243631611, 0.7773170766911672303, 0.8047378541243631611, 0.7773170766911672303, 0.8047378541243631611, 0.7773170766911672303, 0.8047378541243631611, 0.7773170766911672303, 0.8047378541243631611, 0.7773170766911672303, 0.8047378541243631611, 0.7773170766911672303, 0.8047378541243631611, 0.7773170766911672303, 0.8047378541243631611, 0.7773170766911672303, 0.8047378541243631611, 0.7773170766911672303, 0.8047378541243631611, 0.7773170766911672303, 0.8047378541243631611, 0.7773170766911672303, 0.8047378541243631611, 0.7773170766911672303, 0.8047378541243631611, 0.7773170766911672303, 0.8047378541243631611, 0.7773170766911672303, 0.8047378541243631611, 0.7773170766911672303, 0.8047378541243631611, 0.7773170766911672303, 0.8047378541243631611, 0.7773170766911672303, 0.8047378541243631611, 0.7773170766911672303, 0.8047378541243631611, 0.7773170766911672303, 0.8047378541243631611, 0.7773170766911672303, 0.8047378541243631611, 0.7773170766911672303, 0.8047378541243631611, 0.7773170766911672303, 0.8047378541243631611, 0.7773170766911672303, 0.8047378541243631611, 0.7773170766911672303, 0.8047378541243631611, 0.7773170766911672303, 0.8047378541243631611, 0.7773170766911672303, 0.8047378541243631611, 0.7773170766911672303, 0.8047378541243631611, 0.7773170766911672303, 0.8047378541243631611, 0.7773170766911672303, 0.8047378541243631611, 0.7773170766911672303, 0.8047378541243631611, 0.7773170766911672303, 0.8047378541243631611, 0.7773170766911672303, 0.8047378541243631611, 0.7773170766911672303, 0.8047378541243631611, 0.7773170766911672303, 0.8047378541243631611, 0.7773170766911672303, 0.8047378541243631611, 0.7773170766911672303, 0.8047378541243631611, 0.7773170766911672303, 0.8047378541243631611, 0.7773170766911672303, 0.8047378541243631611, 0.7773170766911672303, 0.8047378541243631611, 0.7773170766911672303, 0.8047378541243631611, 0.7773170766911672303, 0.8047378541243631611, 0.7773170766911672303, 0.8047378541243631611, 0.7773170766911672303, 0.8047378541243631611, 0.7773170766911672303, 0.8047378541243631611, 0.7773170766911672303, 0.8047378541243631611, 0.7773170766911672303, 0.8047378541243631611, 0.7773170766911672303, 0.8047378541243631611, 0.7773170766911672303, 0.8047378541243631611, 0.7773170766911672303, 0.8047378541243631611, 0.7773170766911672303, 0.8047378541243631611, 0.7773170766911672303, 0.8047378541243631611, 0.7773170766911672303, 0.8047378541243631611, 0.7773170766911672303, 0.8047378541243631611, 0.7773170766911672303, 0.8047378541243631611, 0.7773170766911672303, 0.8047378541243631611, 0.7773170766911672303, 0.8047378541243631611, 0.7773170766911672303, 0.8047378541243631611, 0.7773170766911672303, 0.8047378541243631611, 0.7773170766911672303, 0.8047378541243631611, 0.7773170766911672303, 0.8047378541243631611, 0.7773170766911672303, 0.8047378541243631611, 0.7773170766911672303, 0.8047378541243631611, 0.7773170766911672303, 0.8047378541243631611, 0.7773170766911672303, 0.8047378541243631611, 0.7773170766911672303, 0.8047378541243631611, 0.7773170766911672303, 0.8047378541243631611, 0.7773170766911672303, 0.8047378541243631611, 0.7773170766911672303, 0.8047378541243631611, 0.7773170766911672303, 0.8047378541243631611, 0.7773170766911672303, 0.8047378541243631611, 0.7773170766911672303, 0.8047378541243631611, 0.7773170766911672303, 0.8047378541243631611, 0.7773170766911672303, 0.8047378541243631611, 0.7773170766911672303, 0.8047378541243631611, 0.7773170766911672303, 0.8047378541243631611, 0.7773170766911672303, 0.8047378541243631611, 0.7773170766911672303, 0.8047378541243631611, 0.7773170766911672303, 0.8047378541243631611, 0.7773170766911672303, 0.8047378541243631611, 0.7773170766911672303, 0.8047378541243631611, 0.7773170766911672303, 0.8047378541243631611, 0.7773170766911672303, 0.8047378541243631611, 0.7773170766911672303, 0.8047378541243631611, 0.7773170766911672303, 0.8047378541243631611, 0.7773170766911672303, 0.8047378541243631611, 0.7773170766911672303, 0.8047378541243631611, 0.7773170766911672303, 0.8047378541243631611, 0.7773170766911672303, 0.8047378541243631611, 0.7773170766911672303, 0.8047378541243631611, 0.7773170766911672303, 0.8047378541243631611, 0.7773170766911672303, 0.8047378541243631611, 0.7773170766911672303, 0.8047378541243631611, 0.7773170766911672303, 0.8047378541243631611, 0.7773170766911672303, 0.8047378541243631611, 0.7773170766911672303, 0.8047378541243631611, 0.7773170766911672303, 0.8047378541243631611, 0.7773170766911672303, 0.8047378541243631611, 0.7773170766911672303, 0.8047378541243631611, 0.7773170766911672303, 0.8047378541243631611, 0.7773170766911672303, 0.8047378541243631611, 0.7773170766911672303, 0.8047378541243631611, 0.7773170766911672303, 0.8047378541243631611, 0.7773170766911672303, 0.8047378541243631611, 0.7773170766911672303, 0.8047378541243631611, 0.7773170766911672303, 0.8047378541243631611, 0.7773170766911672303, 0.8047378541243631611, 0.7773170766911672303, 0.8047378541243631611, 0.7773170766911672303, 0.8047378541243631611, 0.7773170766911672303, 0.8047378541243631611, 0.7773170766911672303, 0.8047378541243631611, 0.7773170766911672303, 0.8047378541243631611, 0.7773170766911672303, 0.8047378541243631611, 0.7773170766911672303, 0.8047378541243631611, 0.7773170766911672303, 0.8047378541243631611, 0.7773170766911672303, 0.8047378541243631611, 0.7773170766911672303, 0.8047378541243631611, 0.7773170766911672303, 0.8047378541243631611, 0.7773170766911672303, 0.8047378541243631611, 0.7773170766911672303, 0.8047378541243631611, 0.7773170766911672303, 0.8047378541243631611, 0.7773170766911672303, 0.8047378541243631611, 0.7773170766911672303, 0.8047378541243631611, 0.7773170766911672303, 0.8047378541243631611, 0.7773170766911672303, 0.8047378541243631611, 0.7773170766911672303, 0.8047378541243631611, 0.7773170766911672303, 0.8047378541243631611, 0.7773170766911672303, 0.8047378541243631611, 0.7773170766911672303, 0.8047378541243631611, 0.7773170766911672303, 0.8047378541243631611, 0.7773170766911672303, 0.8047378541243631611, 0.7773170766911672303, 0.8047378541243631611, 0.7773170766911672303, 0.8047378541243631611, 0.7773170766911672303, 0.8047378541243631611, 0.7773170766911672303, 0.8047378541243631611, 0.7773170766911672303, 0.8047378541243631611, 0.7773170766911672303, 0.8047378541243631611, 0.7773170766911672303, 0.8047378541243631611, 0.7773170766911672303, 0.8047378541243631611, 0.7773170766911672303, 0.8047378541243631611, 0.7773170766911672303, 0.8047378541243631611, 0.7773170766911672303, 0.8047378541243631611, 0.7773170766911672303, 0.8047378541243631611, 0.7773170766911672303, 0.8047378541243631611, 0.7773170766911672303, 0.8047378541243631611, 0.7773170766911672303, 0.8047378541243631611, 0.7773170766911672303, 0.8047378541243631611, 0.7773170766911672303, 0.8047378541243631611, 0.7773170766911672303, 0.8047378541243631611, 0.7773170766911672303, 0.8047378541243631611, 0.7773170766911672303, 0.8047378541243631611, 0.7773170766911672303, 0.8047378541243631611, 0.7773170766911672303, 0.8047378541243631611, 0.7773170766911672303, 0.8047378541243631611, 0.7773170766911672303, 0.8047378541243631611, 0.7773170766911672303, 0.8047378541243631611, 0.7773170766911672303, 0.8047378541243631611, 0.7773170766911672303, 0.8047378541243631611, 0.7773170766911672303, 0.8047378541243631611, 0.7773170766911672303, 0.8047378541243631611, 0.7773170766911672303, 0.8047378541243631611, 0.7773170766911672303, 0.8047378541243631611, 0.7773170766911672303, 0.8047378541243631611, 0.7773170766911672303, 0.8047378541243631611, 0.7773170766911672303, 0.8047378541243631611, 0.7773170766911672303, 0.8047378541243631611, 0.7773170766911672303, 0.8047378541243631611, 0.7773170766911672303, 0.8047378541243631611, 0.7773170766911672303, 0.8047378541243631611, 0.7773170766911672303, 0.8047378541243631611, 0.7773170766911672303, 0.8047378541243631611, 0.7773170766911672303, 0.8047378541243631611, 0.7773170766911672303, 0.8047378541243631611, 0.7773170766911672303, 0.8047378541243631611, 0.7773170766911672303, 0.8047378541243631611, 0.7773170766911672303, 0.8047378541243631611, 0.7773170766911672303, 0.8047378541243631611, 0.7773170766911672303, 0.8047378541243631611, 0.7773170766911672303, 0.8047378541243631611, 0.7773170766911672303, 0.8047378541243631611, 0.7773170766911672303, 0.8047378541243631611, 0.7773170766911672303, 0.8047378541243631611, 0.7773170766911672303, 0.8047378541243631611, 0.7773170766911672303, 0.8047378541243631611, 0.7773170766911672303, 0.8047378541243631611, 0.7773170766911672303, 0.8047378541243631611, 0.7773170766911672303, 0.8047378541243631611, 0.7773170766911672303, 0.8047378541243631611, 0.7773170766911672303, 0.8047378541243631611, 0.7773170766911672303, 0.8047378541243631611, 0.7773170766911672303, 0.8047378541243631611, 0.7773170766911672303, 0.8047378541243631611, 0.7773170766911672303, 0.8047378541243631611, 0.7773170766911672303, 0.8047378541243631611, 0.7773170766911672303, 0.8047378541243631611, 0.7773170766911672303, 0.8047378541243631611, 0.7773170766911672303, 0.8047378541243631611, 0.7773170766911672303, 0.8047378541243631611, 0.7773170766911672303, 0.8047378541243631611, 0.7773170766911672303, 0.8047378541243631611, 0.7773170766911672303, 0.8047378541243631611, 0.7773170766911672303, 0.8047378541243631611, 0.7773170766911672303, 0.8047378541243631611),
 ( 0.8047378541243631611, 0.7773170766911672303, 0.8047378541243631611, 0.7773170766911672303, 0.8047378541243631611, 0.7773170766911672303, 0.8047378541243631611, 0.7773170766911672303, 0.8047378541243631611, 0.7773170766911672303, 0.8047378541243631611, 0.7773170766911672303, 0.8047378541243631611, 0.7773170766911672303, 0.8047378541243631611, 0.7773170766911672303, 0.8047378541243631611, 0.7773170766911672303, 0.8047378541243631611, 0.7773170766911672303, 0.8047378541243631611, 0.7773170766911672303, 0.8047378541243631611, 0.7773170766911672303, 0.8047378541243631611, 0.7773170766911672303, 0.8047378541243631611, 0.7773170766911672303, 0.8047378541243631611, 0.7773170766911672303, 0.8047378541243631611, 0.7773170766911672303, 0.8047378541243631611, 0.7773170766911672303, 0.8047378541243631611, 0.7773170766911672303, 0.8047378541243631611, 0.7773170766911672303, 0.8047378541243631611, 0.7773170766911672303, 0.8047378541243631611, 0.7773170766911672303, 0.8047378541243631611, 0.7773170766911672303, 0.8047378541243631611, 0.7773170766911672303, 0.8047378541243631611, 0.7773170766911672303, 0.8047378541243631611, 0.7773170766911672303, 0.8047378541243631611, 0.7773170766911672303, 0.8047378541243631611, 0.7773170766911672303, 0.8047378541243631611, 0.7773170766911672303, 0.8047378541243631611, 0.7773170766911672303, 0.8047378541243631611, 0.7773170766911672303, 0.8047378541243631611, 0.7773170766911672303, 0.8047378541243631611, 0.7773170766911672303, 0.8047378541243631611, 0.7773170766911672303, 0.8047378541243631611, 0.7773170766911672303, 0.8047378541243631611, 0.7773170766911672303, 0.8047378541243631611, 0.7773170766911672303, 0.8047378541243631611, 0.7773170766911672303, 0.8047378541243631611, 0.7773170766911672303, 0.8047378541243631611, 0.7773170766911672303, 0.8047378541243631611, 0.7773170766911672303, 0.8047378541243631611, 0.7773170766911672303, 0.8047378541243631611, 0.7773170766911672303, 0.8047378541243631611, 0.7773170766911672303, 0.8047378541243631611, 0.7773170766911672303, 0.8047378541243631611, 0.7773170766911672303, 0.8047378541243631611, 0.7773170766911672303, 0.8047378541243631611, 0.7773170766911672303, 0.8047378541243631611, 0.7773170766911672303, 0.8047378541243631611, 0.7773170766911672303, 0.8047378541243631611, 0.7773170766911672303, 0.8047378541243631611, 0.7773170766911672303, 0.8047378541243631611, 0.7773170766911672303, 0.8047378541243631611, 0.7773170766911672303, 0.8047378541243631611, 0.7773170766911672303, 0.8047378541243631611, 0.7773170766911672303, 0.8047378541243631611, 0.7773170766911672303, 0.8047378541243631611, 0.7773170766911672303, 0.8047378541243631611, 0.7773170766911672303, 0.8047378541243631611, 0.7773170766911672303, 0.8047378541243631611, 0.7773170766911672303, 0.8047378541243631611, 0.7773170766911672303, 0.8047378541243631611, 0.7773170766911672303, 0.8047378541243631611, 0.7773170766911672303, 0.8047378541243631611, 0.7773170766911672303, 0.8047378541243631611, 0.7773170766911672303, 0.8047378541243631611, 0.7773170766911672303, 0.8047378541243631611, 0.7773170766911672303, 0.8047378541243631611, 0.7773170766911672303, 0.8047378541243631611, 0.7773170766911672303, 0.8047378541243631611, 0.7773170766911672303, 0.8047378541243631611, 0.7773170766911672303, 0.8047378541243631611, 0.7773170766911672303, 0.8047378541243631611, 0.7773170766911672303, 0.8047378541243631611, 0.7773170766911672303, 0.8047378541243631611, 0.7773170766911672303, 0.8047378541243631611, 0.7773170766911672303, 0.8047378541243631611, 0.7773170766911672303, 0.8047378541243631611, 0.7773170766911672303, 0.8047378541243631611, 0.7773170766911672303, 0.8047378541243631611, 0.7773170766911672303, 0.8047378541243631611, 0.7773170766911672303, 0.8047378541243631611, 0.7773170766911672303, 0.8047378541243631611, 0.7773170766911672303, 0.8047378541243631611, 0.7773170766911672303, 0.8047378541243631611, 0.7773170766911672303, 0.8047378541243631611, 0.7773170766911672303, 0.8047378541243631611, 0.7773170766911672303, 0.8047378541243631611, 0.7773170766911672303, 0.8047378541243631611, 0.7773170766911672303, 0.8047378541243631611, 0.7773170766911672303, 0.8047378541243631611, 0.7773170766911672303, 0.8047378541243631611, 0.7773170766911672303, 0.8047378541243631611, 0.7773170766911672303, 0.8047378541243631611, 0.7773170766911672303, 0.8047378541243631611, 0.7773170766911672303, 0.8047378541243631611, 0.7773170766911672303, 0.8047378541243631611, 0.7773170766911672303, 0.8047378541243631611, 0.7773170766911672303, 0.8047378541243631611, 0.7773170766911672303, 0.8047378541243631611, 0.7773170766911672303, 0.8047378541243631611, 0.7773170766911672303, 0.8047378541243631611, 0.7773170766911672303, 0.8047378541243631611, 0.7773170766911672303, 0.8047378541243631611, 0.7773170766911672303, 0.8047378541243631611, 0.7773170766911672303, 0.8047378541243631611, 0.7773170766911672303, 0.8047378541243631611, 0.7773170766911672303, 0.8047378541243631611, 0.7773170766911672303, 0.8047378541243631611, 0.7773170766911672303, 0.8047378541243631611, 0.7773170766911672303, 0.8047378541243631611, 0.7773170766911672303, 0.8047378541243631611, 0.7773170766911672303, 0.8047378541243631611, 0.7773170766911672303, 0.8047378541243631611, 0.7773170766911672303, 0.8047378541243631611, 0.7773170766911672303, 0.8047378541243631611, 0.7773170766911672303, 0.8047378541243631611, 0.7773170766911672303, 0.8047378541243631611, 0.7773170766911672303, 0.8047378541243631611, 0.7773170766911672303, 0.8047378541243631611, 0.7773170766911672303, 0.8047378541243631611, 0.7773170766911672303, 0.8047378541243631611, 0.7773170766911672303, 0.8047378541243631611, 0.7773170766911672303, 0.8047378541243631611, 0.7773170766911672303, 0.8047378541243631611, 0.7773170766911672303, 0.8047378541243631611, 0.7773170766911672303, 0.8047378541243631611, 0.7773170766911672303, 0.8047378541243631611, 0.7773170766911672303, 0.8047378541243631611, 0.7773170766911672303, 0.8047378541243631611, 0.7773170766911672303, 0.8047378541243631611, 0.7773170766911672303, 0.8047378541243631611, 0.7773170766911672303, 0.8047378541243631611, 0.7773170766911672303, 0.8047378541243631611, 0.7773170766911672303, 0.8047378541243631611, 0.7773170766911672303, 0.8047378541243631611, 0.7773170766911672303, 0.8047378541243631611, 0.7773170766911672303, 0.8047378541243631611, 0.7773170766911672303, 0.8047378541243631611, 0.7773170766911672303, 0.8047378541243631611, 0.7773170766911672303, 0.8047378541243631611, 0.7773170766911672303, 0.8047378541243631611, 0.7773170766911672303, 0.8047378541243631611, 0.7773170766911672303, 0.8047378541243631611, 0.7773170766911672303, 0.8047378541243631611, 0.7773170766911672303, 0.8047378541243631611, 0.7773170766911672303, 0.8047378541243631611, 0.7773170766911672303, 0.8047378541243631611, 0.7773170766911672303, 0.8047378541243631611, 0.7773170766911672303, 0.8047378541243631611, 0.7773170766911672303, 0.8047378541243631611, 0.7773170766911672303, 0.8047378541243631611, 0.7773170766911672303, 0.8047378541243631611, 0.7773170766911672303, 0.8047378541243631611, 0.7773170766911672303, 0.8047378541243631611, 0.7773170766911672303, 0.8047378541243631611, 0.7773170766911672303, 0.8047378541243631611, 0.7773170766911672303, 0.8047378541243631611, 0.7773170766911672303, 0.8047378541243631611, 0.7773170766911672303, 0.8047378541243631611, 0.7773170766911672303, 0.8047378541243631611, 0.7773170766911672303, 0.8047378541243631611, 0.7773170766911672303, 0.8047378541243631611, 0.7773170766911672303, 0.8047378541243631611, 0.7773170766911672303, 0.8047378541243631611, 0.7773170766911672303, 0.8047378541243631611, 0.7773170766911672303, 0.8047378541243631611, 0.7773170766911672303, 0.8047378541243631611, 0.7773170766911672303, 0.8047378541243631611, 0.7773170766911672303, 0.8047378541243631611, 0.7773170766911672303, 0.8047378541243631611, 0.7773170766911672303, 0.8047378541243631611, 0.7773170766911672303, 0.8047378541243631611, 0.7773170766911672303, 0.8047378541243631611, 0.7773170766911672303, 0.8047378541243631611, 0.7773170766911672303, 0.8047378541243631611, 0.7773170766911672303, 0.8047378541243631611, 0.7773170766911672303, 0.8047378541243631611, 0.7773170766911672303, 0.8047378541243631611, 0.7773170766911672303, 0.8047378541243631611, 0.7773170766911672303, 0.8047378541243631611, 0.7773170766911672303, 0.8047378541243631611, 0.7773170766911672303, 0.8047378541243631611, 0.7773170766911672303, 0.8047378541243631611, 0.7773170766911672303, 0.8047378541243631611, 0.7773170766911672303, 0.8047378541243631611, 0.7773170766911672303, 0.8047378541243631611, 0.7773170766911672303, 0.8047378541243631611, 0.7773170766911672303, 0.8047378541243631611, 0.7773170766911672303, 0.8047378541243631611, 0.7773170766911672303, 0.8047378541243631611, 0.7773170766911672303, 0.8047378541243631611, 0.7773170766911672303, 0.8047378541243631611, 0.7773170766911672303, 0.8047378541243631611, 0.7773170766911672303, 0.8047378541243631611, 0.7773170766911672303, 0.8047378541243631611, 0.7773170766911672303, 0.8047378541243631611, 0.7773170766911672303, 0.8047378541243631611, 0.7773170766911672303, 0.8047378541243631611, 0.7773170766911672303, 0.8047378541243631611, 0.7773170766911672303, 0.8047378541243631611, 0.7773170766911672303, 0.8047378541243631611, 0.7773170766911672303, 0.8047378541243631611, 0.7773170766911672303, 0.8047378541243631611, 0.7773170766911672303, 0.8047378541243631611, 0.7773170766911672303, 0.8047378541243631611, 0.7773170766911672303, 0.8047378541243631611, 0.7773170766911672303, 0.8047378541243631611, 0.7773170766911672303, 0.8047378541243631611, 0.7773170766911672303, 0.8047378541243631611, 0.7773170766911672303, 0.8047378541243631611, 0.7773170766911672303, 0.8047378541243631611, 0.7773170766911672303, 0.8047378541243631611, 0.7773170766911672303, 0.8047378541243631611, 0.7773170766911672303, 0.8047378541243631611, 0.7773170766911672303, 0.8047378541243631611, 0.7773170766911672303, 0.8047378541243631611, 0.7773170766911672303, 0.8047378541243631611, 0.7773170766911672303, 0.8047378541243631611, 0.7773170766911672303, 0.8047378541243631611, 0.7773170766911672303, 0.8047378541243631611, 0.7773170766911672303, 0.8047378541243631611, 0.7773170766911672303, 0.8047378541243631611, 0.7773170766911672303, 0.8047378541243631611, 0.7773170766911672303, 0.8047378541243631611, 0.7773170766911672303, 0.8047378541243631611, 0.7773170766911672303, 0.8047378541243631611, 0.7773170766911672303, 0.8047378541243631611, 0.7773170766911672303, 0.8047378541243631611, 0.7773170766911672303, 0.8047378541243631611, 0.7773170766911672303, 0.8047378541243631611, 0.7773170766911672303, 0.8047378541243631611, 0.7773170766911672303, 0.8047378541243631611, 0.7773170766911672303, 0.8047378541243631611, 0.7773170766911672303, 0.8047378541243631611, 0.7773170766911672303, 0.8047378541243631611, 0.7773170766911672303, 0.8047378541243631611, 0.7773170766911672303, 0.8047378541243631611),
 ( 1.000000000000000000, 0.9659258262890683122, 1.000000000000000000, 0.9659258262890683122, 1.000000000000000000, 0.9659258262890683122, 1.000000000000000000, 0.9659258262890683122, 1.000000000000000000, 0.9659258262890683122, 1.000000000000000000, 0.9659258262890683122, 1.000000000000000000, 0.9659258262890683122, 1.000000000000000000, 0.9659258262890683122, 1.000000000000000000, 0.9659258262890683122, 1.000000000000000000, 0.9659258262890683122, 1.000000000000000000, 0.9659258262890683122, 1.000000000000000000, 0.9659258262890683122, 1.000000000000000000, 0.9659258262890683122, 1.000000000000000000, 0.9659258262890683122, 1.000000000000000000, 0.9659258262890683122, 1.000000000000000000, 0.9659258262890683122, 1.000000000000000000, 0.9659258262890683122, 1.000000000000000000, 0.9659258262890683122, 1.000000000000000000, 0.9659258262890683122, 1.000000000000000000, 0.9659258262890683122, 1.000000000000000000, 0.9659258262890683122, 1.000000000000000000, 0.9659258262890683122, 1.000000000000000000, 0.9659258262890683122, 1.000000000000000000, 0.9659258262890683122, 1.000000000000000000, 0.9659258262890683122, 1.000000000000000000, 0.9659258262890683122, 1.000000000000000000, 0.9659258262890683122, 1.000000000000000000, 0.9659258262890683122, 1.000000000000000000, 0.9659258262890683122, 1.000000000000000000, 0.9659258262890683122, 1.000000000000000000, 0.9659258262890683122, 1.000000000000000000, 0.9659258262890683122, 1.000000000000000000, 0.9659258262890683122, 1.000000000000000000, 0.9659258262890683122, 1.000000000000000000, 0.9659258262890683122, 1.000000000000000000, 0.9659258262890683122, 1.000000000000000000, 0.9659258262890683122, 1.000000000000000000, 0.9659258262890683122, 1.000000000000000000, 0.9659258262890683122, 1.000000000000000000, 0.9659258262890683122, 1.000000000000000000, 0.9659258262890683122, 1.000000000000000000, 0.9659258262890683122, 1.000000000000000000, 0.9659258262890683122, 1.000000000000000000, 0.9659258262890683122, 1.000000000000000000, 0.9659258262890683122, 1.000000000000000000, 0.9659258262890683122, 1.000000000000000000, 0.9659258262890683122, 1.000000000000000000, 0.9659258262890683122, 1.000000000000000000, 0.9659258262890683122, 1.000000000000000000, 0.9659258262890683122, 1.000000000000000000, 0.9659258262890683122, 1.000000000000000000, 0.9659258262890683122, 1.000000000000000000, 0.9659258262890683122, 1.000000000000000000, 0.9659258262890683122, 1.000000000000000000, 0.9659258262890683122, 1.000000000000000000, 0.9659258262890683122, 1.000000000000000000, 0.9659258262890683122, 1.000000000000000000, 0.9659258262890683122, 1.000000000000000000, 0.9659258262890683122, 1.000000000000000000, 0.9659258262890683122, 1.000000000000000000, 0.9659258262890683122, 1.000000000000000000, 0.9659258262890683122, 1.000000000000000000, 0.9659258262890683122, 1.000000000000000000, 0.9659258262890683122, 1.000000000000000000, 0.9659258262890683122, 1.000000000000000000, 0.9659258262890683122, 1.000000000000000000, 0.9659258262890683122, 1.000000000000000000, 0.9659258262890683122, 1.000000000000000000, 0.9659258262890683122, 1.000000000000000000, 0.9659258262890683122, 1.000000000000000000, 0.9659258262890683122, 1.000000000000000000, 0.9659258262890683122, 1.000000000000000000, 0.9659258262890683122, 1.000000000000000000, 0.9659258262890683122, 1.000000000000000000, 0.9659258262890683122, 1.000000000000000000, 0.9659258262890683122, 1.000000000000000000, 0.9659258262890683122, 1.000000000000000000, 0.9659258262890683122, 1.000000000000000000, 0.9659258262890683122, 1.000000000000000000, 0.9659258262890683122, 1.000000000000000000, 0.9659258262890683122, 1.000000000000000000, 0.9659258262890683122, 1.000000000000000000, 0.9659258262890683122, 1.000000000000000000, 0.9659258262890683122, 1.000000000000000000, 0.9659258262890683122, 1.000000000000000000, 0.9659258262890683122, 1.000000000000000000, 0.9659258262890683122, 1.000000000000000000, 0.9659258262890683122, 1.000000000000000000, 0.9659258262890683122, 1.000000000000000000, 0.9659258262890683122, 1.000000000000000000, 0.9659258262890683122, 1.000000000000000000, 0.9659258262890683122, 1.000000000000000000, 0.9659258262890683122, 1.000000000000000000, 0.9659258262890683122, 1.000000000000000000, 0.9659258262890683122, 1.000000000000000000, 0.9659258262890683122, 1.000000000000000000, 0.9659258262890683122, 1.000000000000000000, 0.9659258262890683122, 1.000000000000000000, 0.9659258262890683122, 1.000000000000000000, 0.9659258262890683122, 1.000000000000000000, 0.9659258262890683122, 1.000000000000000000, 0.9659258262890683122, 1.000000000000000000, 0.9659258262890683122, 1.000000000000000000, 0.9659258262890683122, 1.000000000000000000, 0.9659258262890683122, 1.000000000000000000, 0.9659258262890683122, 1.000000000000000000, 0.9659258262890683122, 1.000000000000000000, 0.9659258262890683122, 1.000000000000000000, 0.9659258262890683122, 1.000000000000000000, 0.9659258262890683122, 1.000000000000000000, 0.9659258262890683122, 1.000000000000000000, 0.9659258262890683122, 1.000000000000000000, 0.9659258262890683122, 1.000000000000000000, 0.9659258262890683122, 1.000000000000000000, 0.9659258262890683122, 1.000000000000000000, 0.9659258262890683122, 1.000000000000000000, 0.9659258262890683122, 1.000000000000000000, 0.9659258262890683122, 1.000000000000000000, 0.9659258262890683122, 1.000000000000000000, 0.9659258262890683122, 1.000000000000000000, 0.9659258262890683122, 1.000000000000000000, 0.9659258262890683122, 1.000000000000000000, 0.9659258262890683122, 1.000000000000000000, 0.9659258262890683122, 1.000000000000000000, 0.9659258262890683122, 1.000000000000000000, 0.9659258262890683122, 1.000000000000000000, 0.9659258262890683122, 1.000000000000000000, 0.9659258262890683122, 1.000000000000000000, 0.9659258262890683122, 1.000000000000000000, 0.9659258262890683122, 1.000000000000000000, 0.9659258262890683122, 1.000000000000000000, 0.9659258262890683122, 1.000000000000000000, 0.9659258262890683122, 1.000000000000000000, 0.9659258262890683122, 1.000000000000000000, 0.9659258262890683122, 1.000000000000000000, 0.9659258262890683122, 1.000000000000000000, 0.9659258262890683122, 1.000000000000000000, 0.9659258262890683122, 1.000000000000000000, 0.9659258262890683122, 1.000000000000000000, 0.9659258262890683122, 1.000000000000000000, 0.9659258262890683122, 1.000000000000000000, 0.9659258262890683122, 1.000000000000000000, 0.9659258262890683122, 1.000000000000000000, 0.9659258262890683122, 1.000000000000000000, 0.9659258262890683122, 1.000000000000000000, 0.9659258262890683122, 1.000000000000000000, 0.9659258262890683122, 1.000000000000000000, 0.9659258262890683122, 1.000000000000000000, 0.9659258262890683122, 1.000000000000000000, 0.9659258262890683122, 1.000000000000000000, 0.9659258262890683122, 1.000000000000000000, 0.9659258262890683122, 1.000000000000000000, 0.9659258262890683122, 1.000000000000000000, 0.9659258262890683122, 1.000000000000000000, 0.9659258262890683122, 1.000000000000000000, 0.9659258262890683122, 1.000000000000000000, 0.9659258262890683122, 1.000000000000000000, 0.9659258262890683122, 1.000000000000000000, 0.9659258262890683122, 1.000000000000000000, 0.9659258262890683122, 1.000000000000000000, 0.9659258262890683122, 1.000000000000000000, 0.9659258262890683122, 1.000000000000000000, 0.9659258262890683122, 1.000000000000000000, 0.9659258262890683122, 1.000000000000000000, 0.9659258262890683122, 1.000000000000000000, 0.9659258262890683122, 1.000000000000000000, 0.9659258262890683122, 1.000000000000000000, 0.9659258262890683122, 1.000000000000000000, 0.9659258262890683122, 1.000000000000000000, 0.9659258262890683122, 1.000000000000000000, 0.9659258262890683122, 1.000000000000000000, 0.9659258262890683122, 1.000000000000000000, 0.9659258262890683122, 1.000000000000000000, 0.9659258262890683122, 1.000000000000000000, 0.9659258262890683122, 1.000000000000000000, 0.9659258262890683122, 1.000000000000000000, 0.9659258262890683122, 1.000000000000000000, 0.9659258262890683122, 1.000000000000000000, 0.9659258262890683122, 1.000000000000000000, 0.9659258262890683122, 1.000000000000000000, 0.9659258262890683122, 1.000000000000000000, 0.9659258262890683122, 1.000000000000000000, 0.9659258262890683122, 1.000000000000000000, 0.9659258262890683122, 1.000000000000000000, 0.9659258262890683122, 1.000000000000000000, 0.9659258262890683122, 1.000000000000000000, 0.9659258262890683122, 1.000000000000000000, 0.9659258262890683122, 1.000000000000000000, 0.9659258262890683122, 1.000000000000000000, 0.9659258262890683122, 1.000000000000000000, 0.9659258262890683122, 1.000000000000000000, 0.9659258262890683122, 1.000000000000000000, 0.9659258262890683122, 1.000000000000000000, 0.9659258262890683122, 1.000000000000000000, 0.9659258262890683122, 1.000000000000000000, 0.9659258262890683122, 1.000000000000000000, 0.9659258262890683122, 1.000000000000000000, 0.9659258262890683122, 1.000000000000000000, 0.9659258262890683122, 1.000000000000000000, 0.9659258262890683122, 1.000000000000000000, 0.9659258262890683122, 1.000000000000000000, 0.9659258262890683122, 1.000000000000000000, 0.9659258262890683122, 1.000000000000000000, 0.9659258262890683122, 1.000000000000000000, 0.9659258262890683122, 1.000000000000000000, 0.9659258262890683122, 1.000000000000000000, 0.9659258262890683122, 1.000000000000000000, 0.9659258262890683122, 1.000000000000000000, 0.9659258262890683122, 1.000000000000000000, 0.9659258262890683122, 1.000000000000000000, 0.9659258262890683122, 1.000000000000000000, 0.9659258262890683122, 1.000000000000000000, 0.9659258262890683122, 1.000000000000000000, 0.9659258262890683122, 1.000000000000000000, 0.9659258262890683122, 1.000000000000000000, 0.9659258262890683122, 1.000000000000000000, 0.9659258262890683122, 1.000000000000000000, 0.9659258262890683122, 1.000000000000000000, 0.9659258262890683122, 1.000000000000000000, 0.9659258262890683122, 1.000000000000000000, 0.9659258262890683122, 1.000000000000000000, 0.9659258262890683122, 1.000000000000000000, 0.9659258262890683122, 1.000000000000000000, 0.9659258262890683122, 1.000000000000000000, 0.9659258262890683122, 1.000000000000000000, 0.9659258262890683122, 1.000000000000000000, 0.9659258262890683122, 1.000000000000000000, 0.9659258262890683122, 1.000000000000000000, 0.9659258262890683122, 1.000000000000000000, 0.9659258262890683122, 1.000000000000000000, 0.9659258262890683122, 1.000000000000000000, 0.9659258262890683122, 1.000000000000000000, 0.9659258262890683122, 1.000000000000000000, 0.9659258262890683122, 1.000000000000000000, 0.9659258262890683122, 1.000000000000000000, 0.9659258262890683122, 1.000000000000000000, 0.9659258262890683122, 1.000000000000000000) ) ) 
 REPRESENTATION_ITEM ( '' )  SURFACE ( )  );
#48908 = CARTESIAN_POINT ( 'NONE',  ( -0.3249695492770445782, -2.567464376874931580E-15, -0.4445507791589072832 ) ) ;
#48910 = DIRECTION ( 'NONE',  ( 0.000000000000000000, 0.000000000000000000, 1.000000000000000000 ) ) ;
#48909 = CARTESIAN_POINT ( 'NONE',  ( 1.614173228346456712, 1.496062992125984481, 0.1372047244094478646 ) ) ;
#48911 = CARTESIAN_POINT ( 'NONE',  ( -1.193875086542979913, 0.004960608223780448196, -0.3437734562760181856 ) ) ;
#48912 = CARTESIAN_POINT ( 'NONE',  ( -1.174540682414697335, -0.05778040916215522460, 0.4822834645669289988 ) ) ;
#48913 = CARTESIAN_POINT ( 'NONE',  ( -0.3215223097112853146, -0.3162353388693405765, 0.4822834645669290543 ) ) ;
#48914 = CARTESIAN_POINT ( 'NONE',  ( 0.2925321140481932369, -0.2925321140481932369, -2.933070866141732402 ) ) ;
#48915 = CARTESIAN_POINT ( 'NONE',  ( -0.2891555358219908833, -0.2891555358219912164, -2.263779527559055094 ) ) ;
#48916 = ORIENTED_EDGE ( 'NONE', *, *, #38141, .T. ) ;
#48917 = CARTESIAN_POINT ( 'NONE',  ( 0.3412073490813655186, -0.5023911411419708095, -0.1820866141732282451 ) ) ;
#48918 = CARTESIAN_POINT ( 'NONE',  ( -0.1958661417322836718, 0.3392501089628017219, -0.7926509186351704539 ) ) ;
#48919 = CARTESIAN_POINT ( 'NONE',  ( 1.154855643044620184, 0.2306618581243847221, -0.2411417322834647770 ) ) ;
#48920 = EDGE_CURVE ( 'NONE', #50394, #44445, #49640, .T. ) ;
#48921 = CARTESIAN_POINT ( 'NONE',  ( -0.4091458600556405756, 0.2362204724409446288, -2.545931758530183497 ) ) ;
#48922 = CARTESIAN_POINT ( 'NONE',  ( 0.9645669291338588858, 0.1660481256975885056, 0.3530559997133364547 ) ) ;
#48923 = FILL_AREA_STYLE_COLOUR ( '', #31917 ) ;
#48924 = CARTESIAN_POINT ( 'NONE',  ( 1.509186351706037543, 0.05413385826771666132, 0.4176697321401328100 ) ) ;
#48925 = CARTESIAN_POINT ( 'NONE',  ( 1.266404199475066328, -0.08942795157527998196, 0.3641732283464567121 ) ) ;
#48926 = CARTESIAN_POINT ( 'NONE',  ( 0.2165354330708668673, -0.5400638737290844871, 0.3530559997133364547 ) ) ;
#48927 = CARTESIAN_POINT ( 'NONE',  ( 0.1049643490035303689, 0.3917322834645668994, -0.2309518128270847681 ) ) ;
#48928 = CARTESIAN_POINT ( 'NONE',  ( -0.01312335958005186876, 0.05413385826771626580, -0.4176697321401330321 ) ) ;
#48929 = CARTESIAN_POINT ( 'NONE',  ( -0.8267716535433065062, -0.5511811023622047445, 6.969142054262312111E-17 ) ) ;
#48930 = CARTESIAN_POINT ( 'NONE',  ( 0.4921259842519691285, 0.1660481256975885056, 0.3530559997133364547 ) ) ;
#48931 = CARTESIAN_POINT ( 'NONE',  ( -0.2559055118110230564, 0.1660481256975883668, -0.3530559997133364547 ) ) ;
#48932 = CARTESIAN_POINT ( 'NONE',  ( 0.4711511276547932781, 1.601562584932245237, 3.908719782672964715 ) ) ;
#48933 = CARTESIAN_POINT ( 'NONE',  ( -0.1998031496062994683, 0.3460692066303958092, -2.847769028871391050 ) ) ;
#48934 = CARTESIAN_POINT ( 'NONE',  ( -9.594673741351313045E-17, 0.3917322834645670659, -1.729021940453755013 ) ) ;
#48935 = CARTESIAN_POINT ( 'NONE',  ( 0.6889763779527566800, -0.5400638737290844871, 0.3530559997133364547 ) ) ;
#48936 = CARTESIAN_POINT ( 'NONE',  ( -0.2165354330708654795, -0.5400638737290845981, -0.3530559997133363437 ) ) ;
#48937 = CARTESIAN_POINT ( 'NONE',  ( -1.430446194225720724, 0.05413385826771626580, -0.4176697321401330321 ) ) ;
#48938 = CARTESIAN_POINT ( 'NONE',  ( 1.023622047244095112, -0.1870078740157480879, -0.4822834645669291653 ) ) ;
#48939 = CARTESIAN_POINT ( 'NONE',  ( 0.5511811023622055217, -0.1870078740157479769, 0.4822834645669291653 ) ) ;
#48940 = CARTESIAN_POINT ( 'NONE',  ( 0.3917322834645670104, -0.1049643490035303411, -1.141076115485564202 ) ) ;
#48941 = CARTESIAN_POINT ( 'NONE',  ( -0.2099737532808391705, -0.6046776061558809534, -0.2411417322834644161 ) ) ;
#48942 = CARTESIAN_POINT ( 'NONE',  ( 0.2165354330708668673, -0.5400638737290844871, 0.3530559997133364547 ) ) ;
#48943 = CARTESIAN_POINT ( 'NONE',  ( -0.6102362204724400829, -0.5400638737290845981, -0.3530559997133363437 ) ) ;
#48944 = AXIS2_PLACEMENT_3D ( 'NONE', #7200, #82563, #64023 ) ;
#48945 = CARTESIAN_POINT ( 'NONE',  ( 0.1509186351706045259, -0.08942795157528024563, -0.3641732283464568787 ) ) ;
#48946 = CARTESIAN_POINT ( 'NONE',  ( -1.620734908136482577, -0.6692913385826773087, -0.1292274648535924053 ) ) ;
#48947 = CARTESIAN_POINT ( 'NONE',  ( -0.1807872349014755242, 1.098494004316918460, -2.841285918040845626 ) ) ;
#48948 = CARTESIAN_POINT ( 'NONE',  ( 0.2690288713910767848, -0.6692913385826773087, -0.1292274648535924053 ) ) ;
#48949 = DIRECTION ( 'NONE',  ( 0.000000000000000000, 0.000000000000000000, 1.000000000000000000 ) ) ;
#48950 = CARTESIAN_POINT ( 'NONE',  ( -1.515748031496062076, -0.5400638737290844871, 0.3530559997133364547 ) ) ;
#48951 = CARTESIAN_POINT ( 'NONE',  ( -0.1958661417322836718, 0.3392501089628017219, -2.367454068241469756 ) ) ;
#48952 = ORIENTED_EDGE ( 'NONE', *, *, #20829, .T. ) ;
#48953 = ORIENTED_EDGE ( 'NONE', *, *, #16637, .T. ) ;
#48954 = CARTESIAN_POINT ( 'NONE',  ( 0.7874015748031503170, -0.1870078740157480879, -0.4822834645669291653 ) ) ;
#48955 = CARTESIAN_POINT ( 'NONE',  ( 0.1115485564304467270, -0.5511811023622048555, -0.09757992244046775898 ) ) ;
#48957 = DIRECTION ( 'NONE',  ( 0.000000000000000000, 0.000000000000000000, -1.000000000000000000 ) ) ;
#48956 = CARTESIAN_POINT ( 'NONE',  ( 1.673228346456693494, 0.07958543189024085140, 0.2665933059059887866 ) ) ;
#48958 = CARTESIAN_POINT ( 'NONE',  ( 0.1049643490035303689, 0.3917322834645670104, -0.8654855643044619962 ) ) ;
#48959 = CARTESIAN_POINT ( 'NONE',  ( 0.4091458600556404646, -0.2362204724409448231, -0.02427821522309711946 ) ) ;
#48960 = DIRECTION ( 'NONE',  ( -1.000000000000000000, -0.000000000000000000, -0.000000000000000000 ) ) ;
#48961 = AXIS2_PLACEMENT_3D ( 'NONE', #25316, #11890, #55651 ) ;
#48962 = CARTESIAN_POINT ( 'NONE',  ( 0.3996062992125985480, 2.446882876249141654E-17, -2.242125984251968518 ) ) ;
#48963 = CARTESIAN_POINT ( 'NONE',  ( 0.7611548556430451917, -0.6046776061558807314, 0.2411417322834647770 ) ) ;
#48964 = CARTESIAN_POINT ( 'NONE',  ( -0.7086614173228339419, -0.1870078740157479769, 0.4822834645669291653 ) ) ;
#48965 = CARTESIAN_POINT ( 'NONE',  ( -0.7545931758530177724, 0.2952755905511811885, 0.1292274648535926551 ) ) ;
#48966 = CARTESIAN_POINT ( 'NONE',  ( 0.8333333333333340365, 0.2952755905511810774, -0.1292274648535930714 ) ) ;
#48967 = CARTESIAN_POINT ( 'NONE',  ( 1.227034120734908917, -0.6692913385826771977, 0.1292274648535927661 ) ) ;
#48968 = CARTESIAN_POINT ( 'NONE',  ( -1.170763242744969235, -1.094630224652485432E-15, 0.4281993546915541238 ) ) ;
#48969 = SHAPE_DEFINITION_REPRESENTATION ( #54067, #27201 ) ;
#48970 = CARTESIAN_POINT ( 'NONE',  ( 1.207349081364829990, 0.1283753931104748280, 0.1820866141732283561 ) ) ;
#48971 = CARTESIAN_POINT ( 'NONE',  ( 0.3996062992125984925, 0.1070741851644054499, -2.091207349081364963 ) ) ;
#48972 = CARTESIAN_POINT ( 'NONE',  ( -1.502624671916009680, -0.2845877964562159024, 0.3641732283464567677 ) ) ;
#48973 = FACE_OUTER_BOUND ( 'NONE', #62889, .T. ) ;
#48974 = CARTESIAN_POINT ( 'NONE',  ( 0.1115485564304470323, 0.2952755905511811885, 0.1292274648535926551 ) ) ;
#48976 = CARTESIAN_POINT ( 'NONE',  ( -2.118110236220477116, 0.000000000000000000, 0.4498537592782676509 ) ) ;
#48975 = CARTESIAN_POINT ( 'NONE',  ( 1.345144356955381593, -0.05778040916215522460, 0.4822834645669289988 ) ) ;
#48977 = CARTESIAN_POINT ( 'NONE',  ( -1.338582677165353729, -0.1870078740157480601, -0.3641732283464567677 ) ) ;
#48978 = CARTESIAN_POINT ( 'NONE',  ( 0.3083989501312343062, -0.05778040916215560624, -0.4822834645669293319 ) ) ;
#48979 = CARTESIAN_POINT ( 'NONE',  ( 1.397637795275591177, -0.4536011799217367080, 0.2665933059059888421 ) ) ;
#48980 = CARTESIAN_POINT ( 'NONE',  ( -0.3917322834645670659, 0.1049643490035301607, -1.530164411252281420 ) ) ;
#48981 = CARTESIAN_POINT ( 'NONE',  ( -1.391076115485563758, 0.1283753931104748280, 0.1820866141732283561 ) ) ;
#48982 = CARTESIAN_POINT ( 'NONE',  ( 1.535433070866142558, 0.2952755905511811885, 0.000000000000000000 ) ) ;
#48983 = CARTESIAN_POINT ( 'NONE',  ( 2.594411373832371304, 1.668416680336019864, -0.4562095852119716355 ) ) ;
#48984 = CARTESIAN_POINT ( 'NONE',  ( 0.03937007874015806264, 0.1771653543307087630, 0.000000000000000000 ) ) ;
#48985 = CARTESIAN_POINT ( 'NONE',  ( -0.08530183727034056085, -0.05778040916215560624, -0.4822834645669293319 ) ) ;
#48986 = CARTESIAN_POINT ( 'NONE',  ( -1.233595800524933894, -0.5023911411419708095, -0.1820866141732282451 ) ) ;
#48987 = EDGE_CURVE ( 'NONE', #65960, #69752, #39676, .T. ) ;
#48988 = CARTESIAN_POINT ( 'NONE',  ( -0.7742782152230965886, 0.05413385826771666132, 0.4176697321401328100 ) ) ;
#48989 = CARTESIAN_POINT ( 'NONE',  ( 1.522309711286089939, 0.2306618581243848609, 0.2411417322834645549 ) ) ;
#48990 = CARTESIAN_POINT ( 'NONE',  ( -0.1958661417322833942, -0.3392501089628018884, -0.6922765336296082817 ) ) ;
#48991 = DIRECTION ( 'NONE',  ( 1.000000000000000000, 0.000000000000000000, -0.000000000000000000 ) ) ;
#48992 = CARTESIAN_POINT ( 'NONE',  ( 1.213910761154856299, -0.6692913385826773087, -0.1292274648535924053 ) ) ;
#48993 = CARTESIAN_POINT ( 'NONE',  ( -0.2362204724409451284, 0.4091458600556402425, -2.137139107611548905 ) ) ;
#48994 = CARTESIAN_POINT ( 'NONE',  ( -1.003937007874015297, -0.5400638737290845981, -0.3530559997133363437 ) ) ;
#48995 = CARTESIAN_POINT ( 'NONE',  ( -1.115485564304461219, -0.004921259842519870586, -0.3153832671262229437 ) ) ;
#48996 = CARTESIAN_POINT ( 'NONE',  ( -0.5774278215223089816, 0.1283753931104746893, -0.1820866141732285504 ) ) ;
#48997 = CARTESIAN_POINT ( 'NONE',  ( 0.7977407017645454790, -9.595573933774993207E-16, 0.4281989832122458095 ) ) ;
#48998 = CARTESIAN_POINT ( 'NONE',  ( 0.1246719160104994284, 0.2952755905511810774, -0.1292274648535930714 ) ) ;
#48999 = CARTESIAN_POINT ( 'NONE',  ( -0.05905511811023545637, 0.07958543189024085140, 0.2665933059059887866 ) ) ;
#49000 = CARTESIAN_POINT ( 'NONE',  ( -1.266404199475064773, -0.2845877964562159024, 0.3641732283464567677 ) ) ;
#49001 = CARTESIAN_POINT ( 'NONE',  ( -1.587926509186350810, -0.4281496062992124485, 0.4176697321401328655 ) ) ;
#49002 = CARTESIAN_POINT ( 'NONE',  ( 1.489501312335958172, -0.08942795157528024563, -0.3641732283464568787 ) ) ;
#49003 = CARTESIAN_POINT ( 'NONE',  ( 1.259842519685040019, -0.1870078740157480879, -0.4822834645669291653 ) ) ;
#49004 = CARTESIAN_POINT ( 'NONE',  ( 0.4567729623170501685, 1.408376684009862378, 2.131114924183266091 ) ) ;
#49005 = CARTESIAN_POINT ( 'NONE',  ( 0.5708661417322842269, 0.07958543189024085140, 0.2665933059059887866 ) ) ;
#49006 = CARTESIAN_POINT ( 'NONE',  ( 1.010498687664042716, -0.4281496062992124485, 0.4176697321401328655 ) ) ;
#49007 = CARTESIAN_POINT ( 'NONE',  ( 0.8530183727034126306, -0.004921259842519870586, -0.3153832671262229437 ) ) ;
#49008 = VERTEX_POINT ( 'NONE', #16560 ) ;
#49009 = EDGE_CURVE ( 'NONE', #17299, #57855, #32740, .T. ) ;
#49010 = CARTESIAN_POINT ( 'NONE',  ( -1.076115485564303809, -0.6046776061558809534, -0.2411417322834644161 ) ) ;
#49011 = ADVANCED_FACE ( 'NONE', ( #75044 ), #43021, .T. ) ;
#49012 = CARTESIAN_POINT ( 'NONE',  ( -0.7545931758530176614, -0.6692913385826773087, -0.1292274648535924053 ) ) ;
#49013 = CARTESIAN_POINT ( 'NONE',  ( -0.2099737532808391705, -0.6046776061558809534, -0.2411417322834644161 ) ) ;
#49014 = CARTESIAN_POINT ( 'NONE',  ( -0.6575345472713096662, 1.929133858267489954, 0.5309055118110236338 ) ) ;
#49015 = CARTESIAN_POINT ( 'NONE',  ( -0.1070741851644051862, -0.3996062992125986590, -2.038713910761154491 ) ) ;
#49016 = CARTESIAN_POINT ( 'NONE',  ( 0.7874015748031503170, -0.1870078740157479769, 0.4822834645669291653 ) ) ;
#49017 = CARTESIAN_POINT ( 'NONE',  ( 1.581364829396326277, -0.08942795157527998196, 0.3641732283464567121 ) ) ;
#49018 = CARTESIAN_POINT ( 'NONE',  ( 0.2099737532808405305, -0.6046776061558807314, 0.2411417322834647770 ) ) ;
#49019 = CARTESIAN_POINT ( 'NONE',  ( 0.9448818897637802916, -0.1870078740157479769, 0.4822834645669291653 ) ) ;
#49020 = CARTESIAN_POINT ( 'NONE',  ( -0.3996062992125986035, -7.340648628747425578E-17, -1.771653543307086576 ) ) ;
#49021 = AXIS2_PLACEMENT_3D ( 'NONE', #9530, #36436, #68843 ) ;
#49022 = CARTESIAN_POINT ( 'NONE',  ( 0.1974969037888706369, -0.3420746716998659953, -1.036745406824147064 ) ) ;
#49023 = CARTESIAN_POINT ( 'NONE',  ( -0.2925321140481930704, -0.2925321140481933480, -2.578740157480315265 ) ) ;
#49024 = CARTESIAN_POINT ( 'NONE',  ( 0.000000000000000000, 0.03937007874015751446, 2.362204724409448620 ) ) ;
#49025 = CARTESIAN_POINT ( 'NONE',  ( 0.3392501089628018884, -0.1958661417322834220, -0.4120734908136482466 ) ) ;
#49026 = CARTESIAN_POINT ( 'NONE',  ( -0.3937007874015740483, -0.1870078740157480601, -0.3641732283464567677 ) ) ;
#49027 = CARTESIAN_POINT ( 'NONE',  ( -0.5905511811023615998, 0.2952755905511811885, 0.000000000000000000 ) ) ;
#49028 = CARTESIAN_POINT ( 'NONE',  ( 0.3018372703412079971, -0.4281496062992124485, 0.4176697321401328655 ) ) ;
#49029 = CARTESIAN_POINT ( 'NONE',  ( 0.3949938075777409963, 2.418639510665530743E-17, -2.242125984251968518 ) ) ;
#49030 = CARTESIAN_POINT ( 'NONE',  ( 1.581364829396326277, -0.05778040916215522460, 0.4822834645669289988 ) ) ;
#49031 = CARTESIAN_POINT ( 'NONE',  ( 0.9973753280839902091, 0.2306618581243847221, -0.2411417322834647770 ) ) ;
#49032 = CARTESIAN_POINT ( 'NONE',  ( -0.3458507752293909498, 0.3458507752293907833, -2.381889763779527325 ) ) ;
#49033 = CARTESIAN_POINT ( 'NONE',  ( -0.2925321140481930704, -0.2925321140481933480, -1.633858267716534973 ) ) ;
#49034 = CARTESIAN_POINT ( 'NONE',  ( 0.4849061582275019378, 1.967896864084105024, 0.4921425059946345493 ) ) ;
#49035 = CARTESIAN_POINT ( 'NONE',  ( 1.154855643044620184, 0.2306618581243847221, -0.2411417322834647770 ) ) ;
#49036 = CARTESIAN_POINT ( 'NONE',  ( 1.089238845144357537, -0.3690944881889763329, 0.3153832671262228327 ) ) ;
#49038 = CARTESIAN_POINT ( 'NONE',  ( -1.509186351706035767, -0.4281496062992124485, 0.4176697321401328655 ) ) ;
#49037 = CARTESIAN_POINT ( 'NONE',  ( -1.450131233595799651, 0.1771653543307087075, -0.09757992244046823083 ) ) ;
#49039 = CARTESIAN_POINT ( 'NONE',  ( 0.1049643490035304522, -0.3917322834645668994, -2.842500369257531023 ) ) ;
#49040 = CARTESIAN_POINT ( 'NONE',  ( -1.614173228346457378, 2.094556775020298023, 0.1372047244094476981 ) ) ;
#49041 = CARTESIAN_POINT ( 'NONE',  ( 0.8005249343832028242, -0.4281496062992127816, -0.4176697321401328100 ) ) ;
#49042 = CARTESIAN_POINT ( 'NONE',  ( 1.364829396325460076, 0.1283753931104748280, 0.1820866141732283561 ) ) ;
#49043 = CARTESIAN_POINT ( 'NONE',  ( -0.5511811023622041894, -0.1870078740157480879, -0.4822834645669291653 ) ) ;
#49044 = CARTESIAN_POINT ( 'NONE',  ( -0.4133858267716528645, 0.1660481256975883668, -0.3530559997133364547 ) ) ;
#49045 = CARTESIAN_POINT ( 'NONE',  ( 1.502624671916010790, -0.3162353388693409650, -0.4822834645669289433 ) ) ;
#49046 = CARTESIAN_POINT ( 'NONE',  ( -0.1049643490035307020, 0.3917322834645669549, -0.09120734908136493568 ) ) ;
#49047 = CARTESIAN_POINT ( 'NONE',  ( 0.3083989501312343062, -0.3162353388693405765, 0.4822834645669290543 ) ) ;
#49048 = CARTESIAN_POINT ( 'NONE',  ( 0.1049643490035304938, -0.3917322834645669549, -2.439632545931758045 ) ) ;
#49049 = CARTESIAN_POINT ( 'NONE',  ( 1.627296587926509996, -0.6046776061558807314, 0.2411417322834647770 ) ) ;
#49050 = ORIENTED_EDGE ( 'NONE', *, *, #35952, .T. ) ;
#49051 = CARTESIAN_POINT ( 'NONE',  ( -0.3420746716998661618, 0.1974969037888702206, -2.703412073490814027 ) ) ;
#49052 = ORIENTED_EDGE ( 'NONE', *, *, #27675, .F. ) ;
#49053 = DIRECTION ( 'NONE',  ( -0.2810846377148243924, -0.6785983445458325658, -0.6785983445458596552 ) ) ;
#49054 = CARTESIAN_POINT ( 'NONE',  ( -1.482939632545930975, -0.4281496062992127816, -0.4176697321401328100 ) ) ;
#49055 = CARTESIAN_POINT ( 'NONE',  ( -0.1070741851644051862, -0.3996062992125987146, -1.017060367454067915 ) ) ;
#49056 = CARTESIAN_POINT ( 'NONE',  ( 0.4889872687189470435, 1.535433070866141225, 0.4915354330708653907 ) ) ;
#49057 = PLANE ( 'NONE',  #46425 ) ;
#49058 = FACE_OUTER_BOUND ( 'NONE', #20142, .T. ) ;
#49059 = CARTESIAN_POINT ( 'NONE',  ( 0.5314960629921323676, 2.742788190551039396, -1.827151662668102361 ) ) ;
#49060 = CARTESIAN_POINT ( 'NONE',  ( 0.3917322834645670104, -0.1049643490035303411, -0.5111548556430445256 ) ) ;
#49061 = CARTESIAN_POINT ( 'NONE',  ( -0.1377952755905504645, -0.4536011799217368745, -0.2665933059059886201 ) ) ;
#49062 = CARTESIAN_POINT ( 'NONE',  ( -1.017060367454067249, -0.2845877964562161244, -0.3641732283464567121 ) ) ;
#49063 = PRODUCT_DEFINITION_FORMATION_WITH_SPECIFIED_SOURCE ( 'ANY', '', #25763, .NOT_KNOWN. ) ;
#49064 = CARTESIAN_POINT ( 'NONE',  ( -1.515748031496062076, -0.5400638737290844871, 0.3530559997133364547 ) ) ;
#49065 = CARTESIAN_POINT ( 'NONE',  ( 0.4133858267716541968, -0.5400638737290845981, -0.3530559997133363437 ) ) ;
#49066 = CARTESIAN_POINT ( 'NONE',  ( -1.541994750656167090, -0.6692913385826773087, -0.1292274648535924053 ) ) ;
#49067 = CARTESIAN_POINT ( 'NONE',  ( -0.1049643490035307020, 0.3917322834645669549, -0.1561679790026246351 ) ) ;
#49068 = VERTEX_POINT ( 'NONE', #30813 ) ;
#49069 = CARTESIAN_POINT ( 'NONE',  ( 1.541994750656168645, -0.6692913385826771977, 0.1292274648535927661 ) ) ;
#49070 = DIRECTION ( 'NONE',  ( 1.000000000000000000, 0.000000000000000000, 0.000000000000000000 ) ) ;
#49071 = CARTESIAN_POINT ( 'NONE',  ( -0.4091458600556402980, -0.2362204724409451284, -1.784776902887138972 ) ) ;
#49072 = CARTESIAN_POINT ( 'NONE',  ( 0.1133856558944469489, 0.2726377952755905665, 0.1574803149606299191 ) ) ;
#49073 = DIRECTION ( 'NONE',  ( 0.000000000000000000, -1.000000000000000000, 0.000000000000000000 ) ) ;
#49074 = CARTESIAN_POINT ( 'NONE',  ( -0.9448818897637790704, -0.1870078740157480879, -0.4822834645669291653 ) ) ;
#49075 = CARTESIAN_POINT ( 'NONE',  ( 1.371391076115485941, 0.2952755905511811885, 0.1292274648535926551 ) ) ;
#49076 = CARTESIAN_POINT ( 'NONE',  ( 0.6423408027444581503, 0.000000000000000000, 0.3464511005275205946 ) ) ;
#49077 = CARTESIAN_POINT ( 'NONE',  ( 1.574803149606299746, -0.1870078740157480879, -0.4822834645669291653 ) ) ;
#49078 = CARTESIAN_POINT ( 'NONE',  ( -0.7349081364829390672, 0.2306618581243847221, -0.2411417322834647770 ) ) ;
#49079 = AXIS2_PLACEMENT_3D ( 'NONE', #56916, #36336, #29605 ) ;
#49080 = CARTESIAN_POINT ( 'NONE',  ( 0.2867679344610365999, 0.2867679344610365999, -0.5327890831682923212 ) ) ;
#49081 = CARTESIAN_POINT ( 'NONE',  ( -0.02624671916010428221, -0.5023911411419708095, 0.1820866141732285504 ) ) ;
#49082 = CARTESIAN_POINT ( 'NONE',  ( 0.2867679344610366554, 0.2867679344610366554, -0.2224409448818898127 ) ) ;
#49083 = CARTESIAN_POINT ( 'NONE',  ( 0.08530183727034192087, -0.08942795157527998196, 0.3641732283464567121 ) ) ;
#49084 = CARTESIAN_POINT ( 'NONE',  ( 0.5577427821522314977, -0.2845877964562161244, -0.3641732283464567121 ) ) ;
#49085 = CARTESIAN_POINT ( 'NONE',  ( 0.4593175853018379162, -0.4281496062992124485, 0.4176697321401328655 ) ) ;
#49086 = CARTESIAN_POINT ( 'NONE',  ( -0.2624671916010490880, -0.5023911411419708095, 0.1820866141732285504 ) ) ;
#49087 = CARTESIAN_POINT ( 'NONE',  ( 0.2867679344610365999, -0.2867679344610365444, -2.137795275590551380 ) ) ;
#49088 = CARTESIAN_POINT ( 'NONE',  ( 1.482939632545932307, 0.05413385826771626580, -0.4176697321401330321 ) ) ;
#49089 = CARTESIAN_POINT ( 'NONE',  ( -1.194225721784776262, -0.4281496062992124485, 0.4176697321401328655 ) ) ;
#49090 = CARTESIAN_POINT ( 'NONE',  ( -0.4724409448818899238, 0.1265901696524986686, -0.7395013123359580609 ) ) ;
#49091 = CARTESIAN_POINT ( 'NONE',  ( -0.1049868766404193215, 0.2306618581243847221, -0.2411417322834647770 ) ) ;
#49092 = CARTESIAN_POINT ( 'NONE',  ( -0.5971128608923877978, -0.6692913385826773087, -0.1292274648535924053 ) ) ;
#49093 = CARTESIAN_POINT ( 'NONE',  ( 1.509186351706037543, -0.004921259842519576551, 0.3153832671262227771 ) ) ;
#49094 = CARTESIAN_POINT ( 'NONE',  ( 0.2690288713910767848, -0.5511811023622048555, -0.09757992244046775898 ) ) ;
#49095 = CARTESIAN_POINT ( 'NONE',  ( -0.3477690288713905509, -0.6692913385826771977, 0.1292274648535927661 ) ) ;
#49096 = CARTESIAN_POINT ( 'NONE',  ( -0.7545931758530176614, -0.6692913385826773087, -0.1292274648535924053 ) ) ;
#49097 = CARTESIAN_POINT ( 'NONE',  ( -3.890406373195415490, 2.716724272663529227, 0.5314960629921260393 ) ) ;
#49098 = CARTESIAN_POINT ( 'NONE',  ( 1.515748031496063408, 0.07958543189024085140, 0.2665933059059887866 ) ) ;
#49099 = CARTESIAN_POINT ( 'NONE',  ( 0.1837270341207357105, -0.6046776061558809534, -0.2411417322834644161 ) ) ;
#49100 = ORIENTED_EDGE ( 'NONE', *, *, #59684, .T. ) ;
#49101 = CARTESIAN_POINT ( 'NONE',  ( 0.2925321140481932369, 0.2925321140481932369, -2.104330708661417138 ) ) ;
#49102 = CARTESIAN_POINT ( 'NONE',  ( 1.318897637795276356, 0.1660481256975883668, -0.3530559997133364547 ) ) ;
#49103 = CARTESIAN_POINT ( 'NONE',  ( -0.5971128608923877978, 0.1771653543307087630, 0.09757992244046791164 ) ) ;
#49104 = CARTESIAN_POINT ( 'NONE',  ( -0.7742782152230965886, 0.05413385826771666132, 0.4176697321401328100 ) ) ;
#49105 = CARTESIAN_POINT ( 'NONE',  ( 1.233595800524935227, 0.2306618581243847221, -0.2411417322834647770 ) ) ;
#49106 = CARTESIAN_POINT ( 'NONE',  ( 0.7414698162729663755, 0.2952755905511811885, 0.1292274648535926551 ) ) ;
#49107 = CARTESIAN_POINT ( 'NONE',  ( -0.3149606299212458493, 2.165354330708661568, -3.937007874015763242 ) ) ;
#49108 = CARTESIAN_POINT ( 'NONE',  ( -1.148293963254592542, -0.5511811023622048555, -0.09757992244046775898 ) ) ;
#49109 = CARTESIAN_POINT ( 'NONE',  ( 0.2925321140481931814, 0.2925321140481931814, -0.05708661417322837689 ) ) ;
#49110 = CARTESIAN_POINT ( 'NONE',  ( 0.2925321140481932369, 0.2925321140481932369, -0.6102362204724409711 ) ) ;
#49111 = CARTESIAN_POINT ( 'NONE',  ( -0.2891555358219911054, 0.2891555358219909388, 0.1377952755905511306 ) ) ;
#49112 = EDGE_CURVE ( 'NONE', #6101, #78909, #32055, .T. ) ;
#49113 = DIRECTION ( 'NONE',  ( 9.929802617766460227E-17, -0.7071067811865515695, -0.7071067811865434649 ) ) ;
#49114 = CARTESIAN_POINT ( 'NONE',  ( 1.030183727034121421, -0.2845877964562161244, -0.3641732283464567121 ) ) ;
#49115 = CARTESIAN_POINT ( 'NONE',  ( 0.3740157480314966754, 0.1660481256975883668, -0.3530559997133364547 ) ) ;
#49116 = CARTESIAN_POINT ( 'NONE',  ( -1.548556430446193399, 0.2306618581243848609, 0.2411417322834645549 ) ) ;
#49117 = CARTESIAN_POINT ( 'NONE',  ( 0.1058382717557499880, 0.3949938075777409408, -1.015091863517060489 ) ) ;
#49118 = CARTESIAN_POINT ( 'NONE',  ( 1.003937007874016407, -0.4536011799217367080, 0.2665933059059888421 ) ) ;
#49119 = CARTESIAN_POINT ( 'NONE',  ( -0.1049868766404193215, -0.6046776061558807314, 0.2411417322834647770 ) ) ;
#49120 = CARTESIAN_POINT ( 'NONE',  ( -0.7808398950131222316, -0.3162353388693409650, -0.4822834645669289433 ) ) ;
#49121 = CARTESIAN_POINT ( 'NONE',  ( 1.220472440944882608, 0.2952755905511811885, 0.000000000000000000 ) ) ;
#49122 = CARTESIAN_POINT ( 'NONE',  ( 0.4724409448818897572, -0.1265901696524988906, -1.213910761154855189 ) ) ;
#49123 = CARTESIAN_POINT ( 'NONE',  ( -0.1998031496062994683, 0.3460692066303958092, -2.217847769028871596 ) ) ;
#49124 = CONICAL_SURFACE ( 'NONE', #73312, 0.09842519685039351207, 1.029744258676651647 ) ;
#49125 = CARTESIAN_POINT ( 'NONE',  ( -0.2165354330708654795, -0.4536011799217368745, -0.2665933059059886201 ) ) ;
#49126 = EDGE_CURVE ( 'NONE', #64347, #16662, #25639, .T. ) ;
#49127 = ORIENTED_EDGE ( 'NONE', *, *, #65114, .F. ) ;
#49128 = CARTESIAN_POINT ( 'NONE',  ( 0.3392501089628018329, 0.1958661417322835607, -0.7578933315298707063 ) ) ;
#49129 = ORIENTED_EDGE ( 'NONE', *, *, #70912, .F. ) ;
#49130 = CARTESIAN_POINT ( 'NONE',  ( -1.017060367454067249, -0.3162353388693409650, -0.4822834645669289433 ) ) ;
#49131 = CARTESIAN_POINT ( 'NONE',  ( -0.09842519685039295696, -0.5400638737290844871, 0.3530559997133364547 ) ) ;
#49132 = CARTESIAN_POINT ( 'NONE',  ( -0.1246719160104980823, -0.6692913385826773087, -0.1292274648535924053 ) ) ;
#49133 = CARTESIAN_POINT ( 'NONE',  ( 0.8398950131233602345, -0.6046776061558807314, 0.2411417322834647770 ) ) ;
#49134 = EDGE_CURVE ( 'NONE', #34868, #26979, #12709, .T. ) ;
#49135 = CARTESIAN_POINT ( 'NONE',  ( -0.5708661417322825615, -0.5400638737290844871, 0.3530559997133364547 ) ) ;
#49136 = CARTESIAN_POINT ( 'NONE',  ( -1.246719160104985846, -0.4281496062992127816, -0.4176697321401328100 ) ) ;
#49137 = CARTESIAN_POINT ( 'NONE',  ( -0.2362204724409442680, -0.1870078740157480879, -0.4822834645669291653 ) ) ;
#49138 = CARTESIAN_POINT ( 'NONE',  ( 0.9251968503937015864, -0.5400638737290844871, 0.3530559997133364547 ) ) ;
#49139 = CARTESIAN_POINT ( 'NONE',  ( 0.5446194225721792126, -0.05778040916215560624, -0.4822834645669293319 ) ) ;
#49140 = CARTESIAN_POINT ( 'NONE',  ( 0.2867679344610365999, -0.2867679344610365444, -1.192913385826771755 ) ) ;
#49141 = CARTESIAN_POINT ( 'NONE',  ( -0.2559055118110227234, -0.4536011799217367080, 0.2665933059059888421 ) ) ;
#49142 = ORIENTED_EDGE ( 'NONE', *, *, #28554, .T. ) ;
#49143 = CARTESIAN_POINT ( 'NONE',  ( -0.1058382717557497937, -0.3949938075777411628, -1.646981627296588035 ) ) ;
#49144 = VERTEX_POINT ( 'NONE', #18202 ) ;
#49145 = CARTESIAN_POINT ( 'NONE',  ( -1.240157480314959759, 0.07958543189024085140, 0.2665933059059887866 ) ) ;
#49146 = CARTESIAN_POINT ( 'NONE',  ( -0.6299212598425188991, -0.1870078740157480879, -0.4822834645669291653 ) ) ;
#49147 = CARTESIAN_POINT ( 'NONE',  ( -1.191111281560509383, -2.567464376874931580E-15, -0.4445507791589072832 ) ) ;
#49148 = CARTESIAN_POINT ( 'NONE',  ( -0.8005249343832013809, -0.4281496062992124485, 0.4176697321401328655 ) ) ;
#49149 = CARTESIAN_POINT ( 'NONE',  ( -0.9973753280839886548, -0.6046776061558809534, -0.2411417322834644161 ) ) ;
#49150 = CARTESIAN_POINT ( 'NONE',  ( -1.358267716535432434, -0.5400638737290844871, 0.3530559997133364547 ) ) ;
#49151 = DIRECTION ( 'NONE',  ( -0.000000000000000000, -1.000000000000000000, -0.000000000000000000 ) ) ;
#49152 = B_SPLINE_CURVE_WITH_KNOTS ( 'NONE', 3,
 ( #25603, #51266, #13415, #44130 ),
 .UNSPECIFIED., .F., .F.,
 ( 4, 4 ),
 ( 1.999999999910059834E-07, 0.006970199999999934261 ),
 .UNSPECIFIED. ) ;
#49153 = CARTESIAN_POINT ( 'NONE',  ( 0.7349081364829403995, 0.1283753931104748280, 0.1820866141732283561 ) ) ;
#49154 = CARTESIAN_POINT ( 'NONE',  ( -0.3458507752293909498, 0.3458507752293908388, -0.4114173228346456046 ) ) ;
#49155 = CARTESIAN_POINT ( 'NONE',  ( -0.2867679344610365999, 0.2867679344610364889, 0.2106299212598424508 ) ) ;
#49156 = CARTESIAN_POINT ( 'NONE',  ( 0.09842519685039434474, -0.4536011799217368745, -0.2665933059059886201 ) ) ;
#49157 = CARTESIAN_POINT ( 'NONE',  ( -0.4461942257217840213, -0.6046776061558809534, -0.2411417322834644161 ) ) ;
#49158 = CARTESIAN_POINT ( 'NONE',  ( -0.04593175853018302557, 0.2952755905511811885, 0.1292274648535926551 ) ) ;
#49159 = EDGE_LOOP ( 'NONE', ( #65722, #2151, #65449, #19221, #56910, #26156, #44678, #67500, #32668, #7939, #6505, #72025, #69026, #24709, #34551, #30955, #31760, #53497, #63534, #10768, #77811, #54449, #20389, #1947, #18800, #21727, #29872, #67372, #5562, #15811, #3109, #65126, #6267, #20088, #2079, #56622, #1739, #75334, #36428, #75274, #12462, #9195, #4033, #22247, #19329, #68000, #28574, #78681, #60838, #2485, #7548, #15199, #41047, #59592, #51526, #6686, #33943, #36601, #44080, #83279, #64906, #58018, #8675, #20023, #4552, #47491, #79527, #10345, #33858 ) ) ;
#49160 = CARTESIAN_POINT ( 'NONE',  ( -0.1070741851644051862, -0.3996062992125987146, -1.961942257217847763 ) ) ;
#49161 = CARTESIAN_POINT ( 'NONE',  ( -0.5643044619422565855, 0.009842519685039144428, -0.3409548833797004797 ) ) ;
#49162 = ORIENTED_EDGE ( 'NONE', *, *, #80402, .F. ) ;
#49163 = CARTESIAN_POINT ( 'NONE',  ( -0.3460692066303960313, 0.1998031496062989965, -1.520341207349081181 ) ) ;
#49164 = CARTESIAN_POINT ( 'NONE',  ( -0.4724409448818898682, -8.678599364036362592E-17, -2.401574803149606474 ) ) ;
#49165 = CARTESIAN_POINT ( 'NONE',  ( -0.6430446194225716283, -0.3690944881889763329, 0.3153832671262228327 ) ) ;
#49166 = CARTESIAN_POINT ( 'NONE',  ( -0.8398950131233589023, -0.6046776061558809534, -0.2411417322834644161 ) ) ;
#49167 = CARTESIAN_POINT ( 'NONE',  ( 0.4724409448818897572, -0.1265901696524988906, -0.5839895013123358458 ) ) ;
#49168 = EDGE_CURVE ( 'NONE', #3211, #21404, #66340, .T. ) ;
#49169 = CARTESIAN_POINT ( 'NONE',  ( -0.2893911920035082685, 1.160213065395012899, 3.926441900275995600 ) ) ;
#49170 = CARTESIAN_POINT ( 'NONE',  ( 0.2867679344610365999, -0.2867679344610365444, -2.387795275590551380 ) ) ;
#49171 = CARTESIAN_POINT ( 'NONE',  ( 1.292650918635171564, -0.6692913385826773087, -0.1292274648535924053 ) ) ;
#49172 = CARTESIAN_POINT ( 'NONE',  ( 0.3412073490813655186, 0.2306618581243848609, 0.2411417322834645549 ) ) ;
#49173 = CARTESIAN_POINT ( 'NONE',  ( 0.5971128608923891301, 0.2952755905511810774, -0.1292274648535930714 ) ) ;
#49174 = CARTESIAN_POINT ( 'NONE',  ( -0.8595800524934373854, -0.08942795157527998196, 0.3641732283464567121 ) ) ;
#49175 = AXIS2_PLACEMENT_3D ( 'NONE', #55593, #48878, #74578 ) ;
#49176 = CARTESIAN_POINT ( 'NONE',  ( -0.2755905511811018171, 0.2952755905511811885, 0.000000000000000000 ) ) ;
#49177 = CARTESIAN_POINT ( 'NONE',  ( -0.4724409448818898682, -8.678599364036362592E-17, -2.163385826771653697 ) ) ;
#49178 = CARTESIAN_POINT ( 'NONE',  ( -0.3346456692913377662, -0.5400638737290844871, 0.3530559997133364547 ) ) ;
#49179 = ADVANCED_FACE ( 'NONE', ( #78 ), #79816, .T. ) ;
#49180 = CARTESIAN_POINT ( 'NONE',  ( 0.2891555358219910499, 0.2891555358219910499, -2.419291338582677753 ) ) ;
#49181 = CARTESIAN_POINT ( 'NONE',  ( 1.154855643044620184, 0.1283753931104746893, -0.1820866141732285504 ) ) ;
#49182 = CARTESIAN_POINT ( 'NONE',  ( -0.2887139107611542133, 0.1283753931104748280, 0.1820866141732283561 ) ) ;
#49183 = CARTESIAN_POINT ( 'NONE',  ( 1.318897637795276356, -0.4536011799217367080, 0.2665933059059888421 ) ) ;
#49184 = CARTESIAN_POINT ( 'NONE',  ( -1.732283464566928277, -0.1870078740157479769, 0.4822834645669291653 ) ) ;
#49185 = CARTESIAN_POINT ( 'NONE',  ( -1.200787401574802349, -0.4536011799217367080, 0.2665933059059888421 ) ) ;
#49186 = FACE_OUTER_BOUND ( 'NONE', #50746, .T. ) ;
#49187 = CARTESIAN_POINT ( 'NONE',  ( -1.299212598425196097, -0.6692913385826771977, 8.415575281601705876E-17 ) ) ;
#49188 = CARTESIAN_POINT ( 'NONE',  ( -0.3871391076115476282, -0.05778040916215522460, 0.4822834645669289988 ) ) ;
#49189 = EDGE_CURVE ( 'NONE', #25849, #21435, #59593, .T. ) ;
#49190 = VECTOR ( 'NONE', #81384, 39.37007874015748143 ) ;
#49191 = CARTESIAN_POINT ( 'NONE',  ( -2.019766021329723937, 1.253539720428408888, 0.3811758253793102735 ) ) ;
#49192 = CARTESIAN_POINT ( 'NONE',  ( 0.1312335958005257930, 0.1283753931104746893, -0.1820866141732285504 ) ) ;
#49193 = CARTESIAN_POINT ( 'NONE',  ( -1.469816272965878357, -0.5023911411419708095, -0.1820866141732282451 ) ) ;
#49194 = CARTESIAN_POINT ( 'NONE',  ( 0.9055118110236227702, 0.2952755905511811885, 0.000000000000000000 ) ) ;
#49195 = CARTESIAN_POINT ( 'NONE',  ( -1.673228346456691717, 0.07958543189024071263, -0.2665933059059888421 ) ) ;
#49196 = CARTESIAN_POINT ( 'NONE',  ( 1.404199475065617264, -0.3690944881889763329, 0.3153832671262228327 ) ) ;
#49197 = CARTESIAN_POINT ( 'NONE',  ( -0.8267716535433065062, -0.6692913385826771977, 8.415575281601705876E-17 ) ) ;
#49198 = CARTESIAN_POINT ( 'NONE',  ( -0.4724409448818890911, -0.1870078740157480601, -0.3641732283464567677 ) ) ;
#49199 = CARTESIAN_POINT ( 'NONE',  ( 5.785732909357575061E-17, -0.4724409448818898682, -2.755905511811023612 ) ) ;
#49200 = CARTESIAN_POINT ( 'NONE',  ( 0.1837270341207354329, 0.1283753931104748280, 0.1820866141732283561 ) ) ;
#49201 = CARTESIAN_POINT ( 'NONE',  ( 0.09186351706036827158, 0.05413385826771666132, 0.4176697321401328100 ) ) ;
#49202 = CARTESIAN_POINT ( 'NONE',  ( 0.2925321140481932369, -0.2925321140481931814, -0.8051181102362205966 ) ) ;
#49203 = CARTESIAN_POINT ( 'NONE',  ( 0.1958661417322834775, 0.3392501089628018884, -1.961286089238845287 ) ) ;
#49204 = CARTESIAN_POINT ( 'NONE',  ( 0.5577427821522314977, -0.2845877964562161244, -0.3641732283464567121 ) ) ;
#49205 = CARTESIAN_POINT ( 'NONE',  ( 0.09842519685039434474, 0.1660481256975885056, 0.3530559997133364547 ) ) ;
#49206 = CARTESIAN_POINT ( 'NONE',  ( -0.7677165354330699465, -0.5400638737290845981, -0.3530559997133363437 ) ) ;
#49207 = CARTESIAN_POINT ( 'NONE',  ( -0.7939632545931750718, -0.08942795157528024563, -0.3641732283464568787 ) ) ;
#49208 = CARTESIAN_POINT ( 'NONE',  ( 0.9973753280839902091, 0.1539470093639521697, -0.1968503937007875793 ) ) ;
#49209 = CARTESIAN_POINT ( 'NONE',  ( -0.2887139107611542133, -0.5023911411419708095, -0.1820866141732282451 ) ) ;
#49210 = CARTESIAN_POINT ( 'NONE',  ( -0.06561679790026180015, 0.05413385826771666132, 0.4176697321401328100 ) ) ;
#49211 = CARTESIAN_POINT ( 'NONE',  ( -1.325459317585300889, -0.3690944881889765550, -0.3153832671262227771 ) ) ;
#49212 = CARTESIAN_POINT ( 'NONE',  ( -0.1070741851644051862, -0.3996062992125986590, -1.408792650918635259 ) ) ;
#49213 = CARTESIAN_POINT ( 'NONE',  ( -1.640419947506561060, 0.05413385826771666132, 0.4176697321401328100 ) ) ;
#49214 = CARTESIAN_POINT ( 'NONE',  ( 0.2087913723976025926, 0.2087913723976026203, 0.1248231986745541033 ) ) ;
#49215 = ORIENTED_EDGE ( 'NONE', *, *, #5901, .F. ) ;
#49216 = CARTESIAN_POINT ( 'NONE',  ( -1.541994750656167090, 0.1771653543307087630, 0.09757992244046791164 ) ) ;
#49217 = CARTESIAN_POINT ( 'NONE',  ( -0.3215223097112853146, -0.3162353388693405765, 0.4822834645669290543 ) ) ;
#49218 = CARTESIAN_POINT ( 'NONE',  ( -0.9973753280839886548, 0.2306618581243848609, 0.2411417322834645549 ) ) ;
#49219 = CARTESIAN_POINT ( 'NONE',  ( -0.3392501089628019995, 0.1958661417322832277, -1.685695538057742970 ) ) ;
#49220 = FACE_OUTER_BOUND ( 'NONE', #21421, .T. ) ;
#49221 = CARTESIAN_POINT ( 'NONE',  ( 1.207349081364829990, 0.2306618581243848609, 0.2411417322834645549 ) ) ;
#49222 = CARTESIAN_POINT ( 'NONE',  ( 0.4265091863517067594, 0.2952755905511811885, 0.1292274648535926551 ) ) ;
#49223 = CARTESIAN_POINT ( 'NONE',  ( 1.141392835773559211, 0.2755905511811023723, 1.141392835773562764 ) ) ;
#49224 = VECTOR ( 'NONE', #58277, 39.37007874015748143 ) ;
#49226 = CIRCLE ( 'NONE', #76159, 2.362204724409449064 ) ;
#49225 = CARTESIAN_POINT ( 'NONE',  ( 0.1070741851644054637, -0.3996062992125984925, -2.366797900262467280 ) ) ;
#49227 = CARTESIAN_POINT ( 'NONE',  ( -1.732283464566928277, -0.1870078740157479769, 0.4822834645669291653 ) ) ;
#49228 = EDGE_CURVE ( 'NONE', #40163, #65284, #38080, .T. ) ;
#49229 = CARTESIAN_POINT ( 'NONE',  ( 0.3996062992125986035, 0.1070741851644054776, -0.7545931758530182165 ) ) ;
#49230 = ORIENTED_EDGE ( 'NONE', *, *, #76425, .F. ) ;
#49231 = CARTESIAN_POINT ( 'NONE',  ( -0.7677165354330699465, -0.4536011799217368745, -0.2665933059059886201 ) ) ;
#49232 = CARTESIAN_POINT ( 'NONE',  ( 0.2867679344610365999, -0.2867679344610365444, -2.452755905511811108 ) ) ;
#49233 = ORIENTED_EDGE ( 'NONE', *, *, #31679, .F. ) ;
#49234 = CARTESIAN_POINT ( 'NONE',  ( 0.3018372703412079971, -0.4281496062992124485, 0.4176697321401328655 ) ) ;
#49235 = CARTESIAN_POINT ( 'NONE',  ( -0.4396325459317579898, 0.2952755905511811885, 0.1292274648535926551 ) ) ;
#49236 = CARTESIAN_POINT ( 'NONE',  ( -1.161417322834644716, 0.1660481256975885056, 0.3530559997133364547 ) ) ;
#49237 = CARTESIAN_POINT ( 'NONE',  ( 0.8792650918635177559, 0.05413385826771666132, 0.4176697321401328100 ) ) ;
#49238 = CARTESIAN_POINT ( 'NONE',  ( -1.417322834645668772, -0.1870078740157480601, -0.3641732283464567677 ) ) ;
#49239 = CARTESIAN_POINT ( 'NONE',  ( 1.092343761084409559, 1.535433070866141447, 0.6033564923654649581 ) ) ;
#49240 = CARTESIAN_POINT ( 'NONE',  ( -0.01968503937007793844, 0.1660481256975883668, -0.3530559997133364547 ) ) ;
#49241 = CARTESIAN_POINT ( 'NONE',  ( -1.207349081364828436, -0.6046776061558807314, 0.2411417322834647770 ) ) ;
#49242 = CARTESIAN_POINT ( 'NONE',  ( 0.3392501089628018329, 0.1958661417322835052, -2.101030552984564981 ) ) ;
#49243 = CARTESIAN_POINT ( 'NONE',  ( -1.587926509186350810, 0.05413385826771626580, -0.4176697321401330321 ) ) ;
#49244 = CARTESIAN_POINT ( 'NONE',  ( 1.348312163386739426, 0.2755905511811023723, 0.7386866130305692613 ) ) ;
#49245 = CARTESIAN_POINT ( 'NONE',  ( -0.3917322834645670104, -7.196005306013484475E-17, -2.643700787401574548 ) ) ;
#49246 = CARTESIAN_POINT ( 'NONE',  ( 0.8923884514435703741, 0.1283753931104748280, 0.1820866141732283561 ) ) ;
#49247 = ORIENTED_EDGE ( 'NONE', *, *, #82686, .T. ) ;
#49248 = CARTESIAN_POINT ( 'NONE',  ( 0.2891555358219910499, 0.2891555358219910499, -0.1377952755905512694 ) ) ;
#49249 = CARTESIAN_POINT ( 'NONE',  ( -0.9842519685039360366, 0.2952755905511811885, 0.000000000000000000 ) ) ;
#49250 = ORIENTED_EDGE ( 'NONE', *, *, #67975, .F. ) ;
#49252 = VECTOR ( 'NONE', #15456, 39.37007874015748143 ) ;
#49251 = CARTESIAN_POINT ( 'NONE',  ( 0.01312335958005323398, -0.004921259842519576551, 0.3153832671262227771 ) ) ;
#49253 = CARTESIAN_POINT ( 'NONE',  ( -1.469816272965878357, -0.6046776061558809534, -0.2411417322834644161 ) ) ;
#49254 = CARTESIAN_POINT ( 'NONE',  ( 0.7349081364829402885, -0.6046776061558809534, -0.2411417322834644161 ) ) ;
#49255 = CARTESIAN_POINT ( 'NONE',  ( 0.3543307086614179147, 0.2952755905511811885, 0.000000000000000000 ) ) ;
#49256 = CARTESIAN_POINT ( 'NONE',  ( -0.2624671916010490880, 0.2306618581243847221, -0.2411417322834647770 ) ) ;
#49257 = CARTESIAN_POINT ( 'NONE',  ( -9.594673741351313045E-17, 0.3917322834645670659, -1.099100680611235559 ) ) ;
#49258 = CARTESIAN_POINT ( 'NONE',  ( -0.9908136482939626788, 0.2952755905511811885, 0.1292274648535926551 ) ) ;
#49259 = CARTESIAN_POINT ( 'NONE',  ( 0.3917322834645670104, -0.1049643490035303411, -2.243438320209974357 ) ) ;
#49260 = CARTESIAN_POINT ( 'NONE',  ( 1.496062992125984703, -0.1870078740157480601, -0.3641732283464567677 ) ) ;
#49261 = CARTESIAN_POINT ( 'NONE',  ( -1.030183727034119867, -0.3162353388693405765, 0.4822834645669290543 ) ) ;
#49262 = CARTESIAN_POINT ( 'NONE',  ( 0.8923884514435703741, 0.2306618581243848609, 0.2411417322834645549 ) ) ;
#49263 = CARTESIAN_POINT ( 'NONE',  ( 1.332020997375329197, -0.3162353388693405765, 0.4822834645669290543 ) ) ;
#49264 = CARTESIAN_POINT ( 'NONE',  ( 0.1070741851644053527, 0.3996062992125986590, -0.4658792650918635592 ) ) ;
#49265 = CARTESIAN_POINT ( 'NONE',  ( -0.8005249343832013809, -0.4281496062992124485, 0.4176697321401328655 ) ) ;
#49266 = CARTESIAN_POINT ( 'NONE',  ( 4.893765752498283308E-17, -0.3996062992125985480, -0.3129921259842520231 ) ) ;
#49267 = CARTESIAN_POINT ( 'NONE',  ( 0.2296587926509192634, -0.05778040916215560624, -0.4822834645669293319 ) ) ;
#49268 = CARTESIAN_POINT ( 'NONE',  ( -9.787531504996567848E-17, 0.3996062992125986035, -2.362204724409448620 ) ) ;
#49269 = CARTESIAN_POINT ( 'NONE',  ( -0.7020997375328074108, -0.05778040916215522460, 0.4822834645669289988 ) ) ;
#49270 = CARTESIAN_POINT ( 'NONE',  ( -1.653543307086613234, -0.1870078740157479769, 0.3641732283464567677 ) ) ;
#49271 = CARTESIAN_POINT ( 'NONE',  ( 0.6955380577427828781, -0.3690944881889763329, 0.3153832671262228327 ) ) ;
#49272 = CARTESIAN_POINT ( 'NONE',  ( 1.515748031496063186, -0.5400638737290845981, -0.3530559997133363437 ) ) ;
#49273 = CARTESIAN_POINT ( 'NONE',  ( 0.2362204724409449064, 0.4091458600556404646, -1.166010498687663821 ) ) ;
#49274 = CARTESIAN_POINT ( 'NONE',  ( 0.8333333333333340365, -0.5511811023622046335, 0.09757992244046803654 ) ) ;
#49275 = CARTESIAN_POINT ( 'NONE',  ( 0.9776902887139113929, 0.2952755905511811885, 0.1292274648535926551 ) ) ;
#49276 = CARTESIAN_POINT ( 'NONE',  ( -0.3420746716998660508, -0.1974969037888706924, -0.6017060367454067915 ) ) ;
#49277 = CARTESIAN_POINT ( 'NONE',  ( -0.8333333333333323711, -0.6692913385826773087, -0.1292274648535924053 ) ) ;
#49278 = DIRECTION ( 'NONE',  ( 0.000000000000000000, -1.000000000000000000, 1.734723475976808327E-16 ) ) ;
#49279 = CARTESIAN_POINT ( 'NONE',  ( 0.9120734908136489683, -0.5511811023622046335, 0.09757992244046803654 ) ) ;
#49280 = CARTESIAN_POINT ( 'NONE',  ( -0.5052493438320203589, -0.6692913385826771977, 0.1292274648535927661 ) ) ;
#49281 = CARTESIAN_POINT ( 'NONE',  ( -0.06561679790026180015, -0.4281496062992127816, -0.4176697321401328100 ) ) ;
#49282 = CARTESIAN_POINT ( 'NONE',  ( 0.1447075906223747321, 0.004960608223779807216, -0.3437734562760184631 ) ) ;
#49283 = CARTESIAN_POINT ( 'NONE',  ( 0.1377952755905518800, -0.5400638737290844871, 0.3530559997133364547 ) ) ;
#49284 = CARTESIAN_POINT ( 'NONE',  ( 0.2952755905511819101, 0.07958543189024071263, -0.2665933059059888421 ) ) ;
#49285 = CARTESIAN_POINT ( 'NONE',  ( -2.800975763476014180, 1.142877263639032748, -0.2639061591569959453 ) ) ;
#49286 = CARTESIAN_POINT ( 'NONE',  ( -0.09842519685039295696, -0.4536011799217367080, 0.2665933059059888421 ) ) ;
#49287 = CARTESIAN_POINT ( 'NONE',  ( 0.6036745406824153282, -0.5023911411419708095, 0.1820866141732285504 ) ) ;
#49288 = CARTESIAN_POINT ( 'NONE',  ( 0.000000000000000000, 2.677165354330708791, 0.000000000000000000 ) ) ;
#49289 = CARTESIAN_POINT ( 'NONE',  ( 0.3460692066303958092, 0.1998031496062993018, -1.625328083989501460 ) ) ;
#49290 = CARTESIAN_POINT ( 'NONE',  ( 0.5380577427821529035, -0.4281496062992124485, 0.4176697321401328655 ) ) ;
#49291 = AXIS2_PLACEMENT_3D ( 'NONE', #35530, #43063, #61192 ) ;
#49292 = CARTESIAN_POINT ( 'NONE',  ( 0.2867679344610365999, 0.2867679344610365999, -1.704724409448818978 ) ) ;
#49293 = AXIS2_PLACEMENT_3D ( 'NONE', #25821, #52322, #78028 ) ;
#49294 = LINE ( 'NONE', #22399, #60054 ) ;
#49295 = CARTESIAN_POINT ( 'NONE',  ( -0.1123167701215806169, -0.3758920641862485978, -1.519619016692322133E-17 ) ) ;
#49296 = CARTESIAN_POINT ( 'NONE',  ( -0.2952755905511804668, 0.07958543189024085140, 0.2665933059059887866 ) ) ;
#49297 = CARTESIAN_POINT ( 'NONE',  ( -0.4790026246719152336, -0.05778040916215560624, -0.4822834645669293319 ) ) ;
#49298 = CARTESIAN_POINT ( 'NONE',  ( 1.128608923884515169, -0.5023911411419708095, -0.1820866141732282451 ) ) ;
#49299 = CARTESIAN_POINT ( 'NONE',  ( -1.706036745406823485, 0.1283753931104748280, 0.1820866141732283561 ) ) ;
#49300 = CARTESIAN_POINT ( 'NONE',  ( -1.391076115485563758, 0.2306618581243848609, 0.2411417322834645549 ) ) ;
#49301 = CARTESIAN_POINT ( 'NONE',  ( -0.03280839895013062252, 0.2952755905511810774, -0.1292274648535930714 ) ) ;
#49302 = CARTESIAN_POINT ( 'NONE',  ( 0.9842519685039378130, -0.6692913385826771977, 8.415575281601705876E-17 ) ) ;
#49303 = CARTESIAN_POINT ( 'NONE',  ( 0.2887997841774525010, 1.160717306711469110, -1.939402670811599450 ) ) ;
#49304 = CARTESIAN_POINT ( 'NONE',  ( 0.2624671916010504757, -0.6046776061558809534, -0.2411417322834644161 ) ) ;
#49305 = CARTESIAN_POINT ( 'NONE',  ( 1.469816272965879911, -0.6046776061558807314, 0.2411417322834647770 ) ) ;
#49306 = CARTESIAN_POINT ( 'NONE',  ( 0.3543307086614181922, -0.6692913385826771977, 8.415575281601705876E-17 ) ) ;
#49307 = DIRECTION ( 'NONE',  ( 0.000000000000000000, 0.000000000000000000, 1.000000000000000000 ) ) ;
#49308 = CARTESIAN_POINT ( 'NONE',  ( 0.9580052493438327987, -0.3690944881889765550, -0.3153832671262227771 ) ) ;
#49309 = CARTESIAN_POINT ( 'NONE',  ( 1.633858267716535639, -0.5400638737290844871, 0.3530559997133364547 ) ) ;
#49310 = CARTESIAN_POINT ( 'NONE',  ( 0.2034120734908142214, 0.1771653543307087075, -0.09757992244046823083 ) ) ;
#49311 = CARTESIAN_POINT ( 'NONE',  ( -0.1574803149606292529, -0.1870078740157480879, -0.4822834645669291653 ) ) ;
#49312 = CARTESIAN_POINT ( 'NONE',  ( 0.5708661417322841158, -0.5400638737290845981, -0.3530559997133363437 ) ) ;
#49313 = B_SPLINE_CURVE_WITH_KNOTS ( 'NONE', 3,
 ( #25869, #51531, #53201, #78499, #27126, #39335, #19563 ),
 .UNSPECIFIED., .F., .F.,
 ( 4, 3, 4 ),
 ( 1.561251128379126385E-17, 0.001246230184515585400, 0.002492489877932649832 ),
 .UNSPECIFIED. ) ;
#49314 = CARTESIAN_POINT ( 'NONE',  ( -0.4724409448818890911, -0.1870078740157480879, -0.4822834645669291653 ) ) ;
#49315 = CARTESIAN_POINT ( 'NONE',  ( -0.3392501089628017219, -0.1958661417322836995, -2.253956323655855076 ) ) ;
#49316 = CARTESIAN_POINT ( 'NONE',  ( -0.3740157480314953431, -0.4536011799217368745, -0.2665933059059886201 ) ) ;
#49317 = CARTESIAN_POINT ( 'NONE',  ( 0.6233595800524939223, -0.3162353388693405765, 0.4822834645669290543 ) ) ;
#49318 = CARTESIAN_POINT ( 'NONE',  ( 0.8333333333333340365, -0.5511811023622046335, 0.09757992244046803654 ) ) ;
#49319 = CARTESIAN_POINT ( 'NONE',  ( 0.2296587926509192634, -0.3162353388693405765, 0.4822834645669290543 ) ) ;
#49320 = DIRECTION ( 'NONE',  ( -0.000000000000000000, -1.000000000000000000, -0.000000000000000000 ) ) ;
#49322 = CARTESIAN_POINT ( 'NONE',  ( -0.03443470937339728616, 0.2755905511811023723, -1.537015892239756099 ) ) ;
#49321 = DIRECTION ( 'NONE',  ( 0.000000000000000000, -0.000000000000000000, -1.000000000000000000 ) ) ;
#49323 = CARTESIAN_POINT ( 'NONE',  ( -0.3917322834645671215, 0.1049643490035301469, -2.072178477690288734 ) ) ;
#49324 = CARTESIAN_POINT ( 'NONE',  ( -1.246719160104985846, -0.4281496062992127816, -0.4176697321401328100 ) ) ;
#49325 = CARTESIAN_POINT ( 'NONE',  ( -0.3083989501312330295, -0.05778040916215522460, 0.4822834645669289988 ) ) ;
#49326 = CARTESIAN_POINT ( 'NONE',  ( -0.2362204724409451284, 0.4091458600556402425, -0.4855643044619422644 ) ) ;
#49327 = CARTESIAN_POINT ( 'NONE',  ( 0.3949938075777409963, 2.418639510665530435E-17, -2.637795275590551380 ) ) ;
#49328 = VERTEX_POINT ( 'NONE', #50979 ) ;
#49329 = CARTESIAN_POINT ( 'NONE',  ( 0.2362204724409456558, -0.1870078740157479769, 0.3641732283464567677 ) ) ;
#49330 = CARTESIAN_POINT ( 'NONE',  ( -0.3917322834645669549, -0.1049643490035306603, -1.297900262467191590 ) ) ;
#49331 = EDGE_CURVE ( 'NONE', #65960, #19643, #5557, .T. ) ;
#49332 = CARTESIAN_POINT ( 'NONE',  ( 0.5643044619422579178, -0.4281496062992127816, -0.4176697321401328100 ) ) ;
#49333 = CARTESIAN_POINT ( 'NONE',  ( 5.785732909357575061E-17, -0.4724409448818898682, -2.440944881889763884 ) ) ;
#49334 = CARTESIAN_POINT ( 'NONE',  ( 2.130073781772665598, 0.01305114060239440966, 0.4563452811745986049 ) ) ;
#49335 = LINE ( 'NONE', #69531, #9053 ) ;
#49336 = FACE_OUTER_BOUND ( 'NONE', #43505, .T. ) ;
#49337 = CARTESIAN_POINT ( 'NONE',  ( 1.174540682414699111, -0.08942795157528024563, -0.3641732283464568787 ) ) ;
#49338 = CARTESIAN_POINT ( 'NONE',  ( 0.5577427821522316087, -0.05778040916215522460, 0.4822834645669289988 ) ) ;
#49339 = CARTESIAN_POINT ( 'NONE',  ( -0.3392501089628018329, -0.1958661417322836440, -0.6049675608585809439 ) ) ;
#49340 = CARTESIAN_POINT ( 'NONE',  ( -0.5314960629921250401, 0.1660481256975885056, 0.3530559997133364547 ) ) ;
#49341 = CARTESIAN_POINT ( 'NONE',  ( -1.030183727034119867, -0.08942795157528024563, -0.3641732283464568787 ) ) ;
#49342 = CARTESIAN_POINT ( 'NONE',  ( 0.2690288713910767848, -0.6692913385826773087, -0.1292274648535924053 ) ) ;
#49343 = CARTESIAN_POINT ( 'NONE',  ( -0.08530183727034056085, -0.05778040916215560624, -0.4822834645669293319 ) ) ;
#49344 = CARTESIAN_POINT ( 'NONE',  ( 0.5052493438320215802, 0.2952755905511811885, 0.1292274648535926551 ) ) ;
#49345 = VECTOR ( 'NONE', #1689, 39.37007874015748143 ) ;
#49346 = DIRECTION ( 'NONE',  ( -1.000000000000000000, -0.000000000000000000, -0.000000000000000000 ) ) ;
#49347 = CARTESIAN_POINT ( 'NONE',  ( -0.1958661417322836995, 0.3392501089628017219, -2.214586244915697222 ) ) ;
#49348 = CARTESIAN_POINT ( 'NONE',  ( 0.6299212598425204535, -0.1870078740157480879, -0.4822834645669291653 ) ) ;
#49349 = CIRCLE ( 'NONE', #69487, 3.267716535433071279 ) ;
#49350 = AXIS2_PLACEMENT_3D ( 'NONE', #55179, #24024, #4261 ) ;
#49351 = CARTESIAN_POINT ( 'NONE',  ( -0.1968503937007867743, -0.6692913385826771977, 8.415575281601705876E-17 ) ) ;
#49352 = CARTESIAN_POINT ( 'NONE',  ( -1.292650918635170010, 0.2952755905511810774, -0.1292274648535930714 ) ) ;
#49353 = CARTESIAN_POINT ( 'NONE',  ( 1.305774278215223960, 0.2952755905511810774, -0.1292274648535930714 ) ) ;
#49354 = CARTESIAN_POINT ( 'NONE',  ( 0.3477690288713918276, -0.6692913385826773087, -0.1292274648535924053 ) ) ;
#49355 = CARTESIAN_POINT ( 'NONE',  ( -0.2867679344610364334, -0.2867679344610367109, -0.7736220472440945573 ) ) ;
#49356 = CARTESIAN_POINT ( 'NONE',  ( -0.6692913385826764205, -0.6692913385826771977, 8.415575281601705876E-17 ) ) ;
#49357 = CARTESIAN_POINT ( 'NONE',  ( 0.07217847769028949700, -0.3162353388693405765, 0.4822834645669290543 ) ) ;
#49358 = CARTESIAN_POINT ( 'NONE',  ( -0.4855643044619415427, 0.05413385826771626580, -0.4176697321401330321 ) ) ;
#49359 = CARTESIAN_POINT ( 'NONE',  ( 0.4724409448818904789, -0.1870078740157480601, -0.3641732283464567677 ) ) ;
#49360 = CARTESIAN_POINT ( 'NONE',  ( 1.587926509186352586, -0.3690944881889765550, -0.3153832671262227771 ) ) ;
#49361 = CARTESIAN_POINT ( 'NONE',  ( -0.4741766535082717060, 1.520234135998521863, -2.554840505098090020 ) ) ;
#49362 = CARTESIAN_POINT ( 'NONE',  ( 0.2427821522309716595, -0.3162353388693409650, -0.4822834645669289433 ) ) ;
#49363 = FACE_OUTER_BOUND ( 'NONE', #47291, .T. ) ;
#49364 = CARTESIAN_POINT ( 'NONE',  ( -1.535433070866141225, -0.6692913385826771977, 8.415575281601705876E-17 ) ) ;
#49365 = CARTESIAN_POINT ( 'NONE',  ( 0.1049643490035304938, -0.3917322834645669549, -2.754593175853017328 ) ) ;
#49366 = VERTEX_POINT ( 'NONE', #82582 ) ;
#49367 = ORIENTED_EDGE ( 'NONE', *, *, #20837, .F. ) ;
#49368 = CARTESIAN_POINT ( 'NONE',  ( 0.5118110236220480003, -0.6692913385826771977, 8.415575281601705876E-17 ) ) ;
#49369 = CARTESIAN_POINT ( 'NONE',  ( 0.1312335958005255154, -0.5023911411419708095, 0.1820866141732285504 ) ) ;
#49371 = CARTESIAN_POINT ( 'NONE',  ( 0.000000000000000000, 0.000000000000000000, -2.755905511811024056 ) ) ;
#49370 = CARTESIAN_POINT ( 'NONE',  ( 0.5314960629921066104, 2.729664745829105232, 1.840814904541347774 ) ) ;
#49372 = CARTESIAN_POINT ( 'NONE',  ( 0.3917322834645670104, -0.1049643490035303411, -0.9835958005249345604 ) ) ;
#49373 = CARTESIAN_POINT ( 'NONE',  ( -0.2362204724409451284, 0.4091458600556402425, 0.2250656167979002698 ) ) ;
#49374 = PRESENTATION_STYLE_ASSIGNMENT (( #11917 ) ) ;
#49375 = CARTESIAN_POINT ( 'NONE',  ( -9.787531504996566615E-17, 0.3996062992125985480, -2.438976377952756014 ) ) ;
#49376 = CARTESIAN_POINT ( 'NONE',  ( 0.4396325459317590445, -0.6692913385826771977, 0.1292274648535927661 ) ) ;
#49377 = CARTESIAN_POINT ( 'NONE',  ( -0.9448818897637790704, -0.1870078740157480879, -0.4822834645669291653 ) ) ;
#49378 = CARTESIAN_POINT ( 'NONE',  ( -0.9186351706036736120, 0.2306618581243848609, 0.2411417322834645549 ) ) ;
#49379 = CARTESIAN_POINT ( 'NONE',  ( 0.6364829396325465405, -0.05778040916215522460, 0.4822834645669289988 ) ) ;
#49380 = CARTESIAN_POINT ( 'NONE',  ( 1.548556430446194954, -0.6046776061558807314, 0.2411417322834647770 ) ) ;
#49381 = CARTESIAN_POINT ( 'NONE',  ( 1.187664041994751285, -0.08942795157527998196, 0.3641732283464567121 ) ) ;
#49382 = ITEM_DEFINED_TRANSFORMATION ( 'NONE', 'NONE', #55784,  #22098 ) ;
#49383 = CARTESIAN_POINT ( 'NONE',  ( 1.266404199475066328, -0.2845877964562161244, -0.3641732283464567121 ) ) ;
#49384 = CARTESIAN_POINT ( 'NONE',  ( -0.7939632545931750718, -0.05778040916215560624, -0.4822834645669293319 ) ) ;
#49385 = CARTESIAN_POINT ( 'NONE',  ( 0.1998031496062992463, 0.3460692066303959202, -0.3786089238845143923 ) ) ;
#49386 = CARTESIAN_POINT ( 'NONE',  ( 1.456692913385827515, -0.6692913385826771977, 8.415575281601705876E-17 ) ) ;
#49387 = CARTESIAN_POINT ( 'NONE',  ( 0.1049643490035304938, -0.3917322834645669549, -0.2349081364829396223 ) ) ;
#49388 = CARTESIAN_POINT ( 'NONE',  ( -0.1837270341207340729, 0.2306618581243847221, -0.2411417322834647770 ) ) ;
#49389 = B_SPLINE_CURVE_WITH_KNOTS ( 'NONE', 3,
 ( #53045, #33708, #64857, #32867 ),
 .UNSPECIFIED., .F., .F.,
 ( 4, 4 ),
 ( 0.1237084911784920305, 0.1251516581501740388 ),
 .UNSPECIFIED. ) ;
#49391 = CARTESIAN_POINT ( 'NONE',  ( -3.912791665790199769, 1.724409448818897905, -0.4359958488159722534 ) ) ;
#49390 = CARTESIAN_POINT ( 'NONE',  ( 1.207349081364829990, 0.2306618581243848609, 0.2411417322834645549 ) ) ;
#49392 = CARTESIAN_POINT ( 'NONE',  ( -0.9973753280839886548, -0.5023911411419708095, -0.1820866141732282451 ) ) ;
#49393 = CARTESIAN_POINT ( 'NONE',  ( 0.5118110236220480003, -0.6692913385826771977, 8.415575281601705876E-17 ) ) ;
#49394 = CARTESIAN_POINT ( 'NONE',  ( 0.8530183727034126306, -0.004921259842519870586, -0.3153832671262229437 ) ) ;
#49395 = CARTESIAN_POINT ( 'NONE',  ( 0.3917322834645668994, -0.1049643490035303134, -1.451424253771966599 ) ) ;
#49396 = CARTESIAN_POINT ( 'NONE',  ( -1.371391076115484831, 0.1771653543307087075, -0.09757992244046823083 ) ) ;
#49397 = CARTESIAN_POINT ( 'NONE',  ( 1.502624671916010790, -0.05778040916215522460, 0.4822834645669289988 ) ) ;
#49398 = CYLINDRICAL_SURFACE ( 'NONE', #25004, 0.3129921259842520787 ) ;
#49399 = CARTESIAN_POINT ( 'NONE',  ( 0.03280839895013198948, 0.1771653543307087630, 0.09757992244046791164 ) ) ;
#49400 = CARTESIAN_POINT ( 'NONE',  ( -0.1968503937007867743, -0.6692913385826771977, 8.415575281601705876E-17 ) ) ;
#49401 = CARTESIAN_POINT ( 'NONE',  ( -1.430446194225720724, -0.004921259842519870586, -0.3153832671262229437 ) ) ;
#49402 = CARTESIAN_POINT ( 'NONE',  ( -0.5643044619422565855, 0.05413385826771626580, -0.4176697321401330321 ) ) ;
#49403 = CARTESIAN_POINT ( 'NONE',  ( 1.417322834645670104, -0.1870078740157480879, -0.4822834645669291653 ) ) ;
#49404 = CARTESIAN_POINT ( 'NONE',  ( 0.1049643490035304799, -0.3917322834645670104, -0.5544812580390570123 ) ) ;
#49405 = CARTESIAN_POINT ( 'NONE',  ( -0.8136482939632537770, 0.1283753931104746893, -0.1820866141732285504 ) ) ;
#49406 =( BOUNDED_SURFACE ( )  B_SPLINE_SURFACE ( 1, 2, ( 
 ( #34635, #72521, #21580, #40114, #60299, #8135, #2649, #27478, #53136, #78847, #14870, #40531, #66210, #47243, #72932, #15283, #40944, #66623, #65237, #46268, #6304, #26078, #77440, #20616, #12632, #20192, #32816, #31980, #82921, #18937, #78285, #76607, #51738, #50906, #19354, #13889, #70279, #6723, #52576, #57641, #32393, #51318, #70702, #13466, #58056, #4, #37881, #7143, #26505, #52158, #33247, #77021, #7574, #58908, #38291, #44585, #422, #71123, #63967, #25656, #45003, #1268, #26916, #25241, #13055, #58483, #45843, #19774, #64804, #38708, #39123, #64387, #57219, #45427, #848, #77863, #71542, #39548, #12224, #63556, #5890, #31562, #39976, #35317, #14317, #22684, #67313, #66480, #9236, #27332, #41624, #8815, #9648, #71963, #65665, #7992, #73208, #78705, #33656, #59319, #1675, #21852, #34908, #47931, #52992, #66067, #79539, #21029, #46689, #72789, #3330, #73635, #47100, #34491, #72382, #14732, #60157, #54242, #8403, #40384, #66905, #60980, #28586, #47516, #53825, #2088, #34070, #2509, #27753, #15558, #41217, #28168, #59734, #15139, #53417, #28994, #79126, #60571, #21443, #40795, #2922, #79959, #22272, #15977, #54660, #80371, #55478, #62641, #74877, #31053, #49998, #48759, #63053, #30232, #43258, #74458, #74040, #55068, #10486, #30652, #56316, #11726, #10063, #36140, #23505, #29409, #82014, #68955, #80776, #56722, #24328, #3745, #81188, #23092, #75695, #16387, #61396, #18036, #4152, #37382, #81606, #29817, #82419, #42441, #62223, #55894, #48343, #16805, #43670, #11305, #68141, #35726, #61812, #42034, #49172, #4561, #17221, #42853, #69373, #68546, #10887, #5391, #36547, #23922, #49588, #75283, #17626, #36964, #4985, #67728, #330, #61918, #37066, #10593, #80887, #68257, #83242, #68652, #30755, #49691, #23200, #10990, #35843, #57551, #3857, #25984, #61512, #71033, #32302, #30336, #25564, #74571, #6630, #56002, #57963, #29517, #55178, #48871, #62751, #42554, #16916, #36249, #4260, #69061, #51230, #12961, #29923, #55586, #43360, #81298, #23612, #36651, #51642, #38618, #62326, #81713, #49281, #74984, #24023, #19256, #17329, #42959, #76929, #77347, #44908, #11411, #17732, #4663, #75385, #5087, #70606, #64296, #19678, #45337, #58819, #71872, #751, #28075, #26827, #8312, #52485, #39030, #72292, #47423, #47006, #27242, #20524, #7055, #46176, #27659, #39882, #79441, #15047, #13798, #53733, #78614, #33979, #39456, #64714, #20104, #1176, #79034, #21353, #60064, #58390, #78193, #14222, #77772, #72700, #65569, #45754, #7903, #21760, #33564, #65975, #20938, #40703, #71450, #59226, #26412, #13377, #66387, #8725, #65143, #1587, #2418, #7480, #32723, #52065, #52901, #14638, #34396, #46596, #40294, #1996, #59640, #33150, #53325, #2828, #55389, #35638, #36050, #16708, #79863, #15887, #35225, #61723, #54149, #23002, #4060, #42762, #81095, #22180, #60889, #68047, #23412, #68458, #15465, #49078, #73114, #41536, #28489, #16297, #22594, #48255, #74779, #10796, #29320, #54981, #29727, #80689, #73544, #73951, #36456, #3657, #42349, #9967, #30138, #41123, #62130, #4470, #55800, #3239, #60477, #48668, #47838, #17130, #81507, #23829, #66814, #67223, #74365, #10394, #9147, #9555, #34819, #28903, #54566, #80281, #41940, #67636, #61299, #63364, #4884, #56626, #51128, #24233, #43995, #6533, #11626, #69689, #5300, #24645, #50723, #12032, #37689, #25048, #43166, #18750, #6114, #70500, #30959, #19154, #12858, #32203, #76822, #44394, #31369, #43578, #11211, #36870, #82326, #62962, #57860, #38516, #227, #82729, #12439, #50312, #70086, #5698, #62547, #76010, #49497, #38099, #17534, #64199, #75190, #68862, #44805, #57034, #63773, #30558, #56224, #76421, #81922, #49905, #75603, #17942, #31786, #69280, #37287, #25461, #18352, #57449, #83141, #14941, #6946, #19572, #8622, #14114, #27134, #46900, #39767, #7365, #14537, #65462, #59954, #40600, #38929, #8207, #71761, #72179, #52798, #32617, #51960, #71343, #40188, #58279, #59123, #65872, #78923, #33872, #644, #13690, #20831, #59536, #21245, #51539, #1893, #25877, #77666, #64609, #52376, #58703, #1069, #27553, #72594, #7795, #33461, #53212 ),
 ( #39344, #26722, #26301, #66282, #46484, #19997, #34293, #77242, #45648, #78084, #65030, #45231, #70932, #33035, #13277, #20416, #46068, #1480, #78508, #60373, #41019, #73849, #61195, #2721, #22072, #28382, #74678, #55286, #73006, #47732, #42663, #60783, #29626, #48979, #54042, #3551, #79755, #47316, #34712, #15358, #79336, #22491, #67943, #73430, #9038, #80589, #80996, #42248, #35533, #67526, #15780, #41432, #80176, #67115, #29217, #9863, #16189, #9446, #3135, #66705, #17024, #35117, #22896, #28799, #27970, #54884, #36355, #35951, #41836, #54462, #21656, #48154, #16604, #48564, #68361, #3963, #74262, #10700, #10285, #61621, #23309, #53628, #2309, #24132, #44298, #69989, #25366, #23723, #49801, #37181, #43066, #12344, #82632, #68763, #44708, #38000, #17435, #11524, #11107, #63676, #30035, #75088, #6017, #17842, #51029, #11934, #43477, #36763, #62439, #50212, #37589, #4776, #81822, #30452, #76728, #31688, #49394, #75503, #19060, #62860, #57347, #70404, #56116, #63262, #69173, #5196, #30861, #24946, #56526, #56936, #75910, #82228, #24548, #62031, #50619, #55698, #12760, #4367, #81406, #83043, #18249, #76324, #43891, #69588, #5603, #31270, #18654, #52286, #8116, #64513, #45131, #38418, #72503, #127, #71668, #59034, #14445, #19479, #32520, #45973, #70836, #77146, #39251, #53119, #40096, #13597, #58610, #32106, #21156, #26632, #39677, #59445, #77991, #19905, #27042, #20320, #64099, #78830, #51443, #20742, #978, #1389, #65369, #13184, #6850, #551, #52703, #38834, #14019, #78413, #33782, #46393, #58182, #26204, #33371, #72087, #1798, #6435, #65784, #57765, #51867, #77572, #64933, #71251, #7272, #27460, #46812, #7704, #25782, #45554, #32944, #15266, #15686, #67852, #28707, #67434, #35028, #55193, #14852, #61525, #3871, #80900, #28289, #2214, #22401, #79248, #80493, #29530, #10191, #48884, #8943, #54369, #80081, #23214, #40926, #22809, #35439, #34619, #27880, #21563, #40512, #47225, #48058, #53540, #21980, #16514, #72914, #9357, #66193, #60283, #60692, #53951, #73337, #16095, #3042, #73760, #41740, #8529, #9768, #54790, #35859, #79664, #34196, #59861, #66607, #42157, #61104, #3456, #2633, #47642, #41344, #67024, #29122, #48466, #74167, #25263, #24444, #43375, #55600, #69075, #5912, #62339, #43784, #36665, #82129, #37901, #63167, #61932, #57241, #50518, #44201, #49296, #49704, #63577, #81311, #68667, #5100, #56428, #82945, #74997, #82532, #11839, #11006, #4275, #23625, #74584, #17342, #30767, #29936, #81726, #76224, #42971, #11424, #31585, #4677, #37079, #30349, #75400, #75809, #62766, #50112, #18151, #68270, #69490, #31167, #12245, #56018, #69891, #16929, #42569, #18557, #37492, #5505, #24035, #36263, #17746, #56834, #24850, #10606, #14340, #1698, #871, #19801, #32004, #45450, #65688, #38733, #20218, #13080, #58508, #40000, #39572, #38315, #33679, #26939, #20639, #25679, #26100, #8015, #57664, #44606, #59341, #39145, #52183, #71987, #64829, #32417, #65262, #7168, #50929, #76627, #63990, #33272, #13489, #13915, #77887, #26, #77043, #64410, #7598, #51339, #26529, #58931, #46291, #1290, #19375, #6745, #45867, #52601, #18958, #70302, #78307, #12654, #45025, #6331, #77463, #445, #51761, #70726, #58079, #32839, #71565, #71148, #9259, #27776, #28190, #80394, #41239, #79980, #47540, #67751, #27356, #74063, #16409, #10085, #40819, #14754, #34931, #8425, #9670, #42055, #22706, #61416, #29017, #2532, #73230, #40408, #21053, #15581, #35340, #47123, #34093, #22293, #48364, #67337, #60593, #2943, #66503, #2111, #21874, #8838, #28607, #54264, #66927, #72812, #53848, #66090, #35749, #34514, #47954, #60179, #53015, #73657, #78729, #61003, #15999, #79561, #46713, #41646, #3351, #54682, #72405, #59756, #53440, #79148, #21465, #15162, #4172, #29430, #10505, #49193, #69391, #11744, #50422, #48780, #74894, #62241, #68161, #37400, #24346, #36158, #69799, #63072, #42462, #36564, #61832, #5409, #55088, #16826, #31070, #42870, #76122, #36981, #68564, #29836, #55499, #75300, #62662, #81208, #23523, #17242, #18463, #56739, #74479, #10906, #44107, #4579, #82436, #12146, #30250, #5002 ) ),
 .UNSPECIFIED., .F., .F., .F. ) 
 B_SPLINE_SURFACE_WITH_KNOTS ( ( 2, 2 ),
 ( 3, 2, 2, 2, 2, 2, 2, 2, 2, 2, 2, 2, 2, 2, 2, 2, 2, 2, 2, 2, 2, 2, 2, 2, 2, 2, 2, 2, 2, 2, 2, 2, 2, 2, 2, 2, 2, 2, 2, 2, 2, 2, 2, 2, 2, 2, 2, 2, 2, 2, 2, 2, 2, 2, 2, 2, 2, 2, 2, 2, 2, 2, 2, 2, 2, 2, 2, 2, 2, 2, 2, 2, 2, 2, 2, 2, 2, 2, 2, 2, 2, 2, 2, 2, 2, 2, 2, 2, 2, 2, 2, 2, 2, 2, 2, 2, 2, 2, 2, 2, 2, 2, 2, 2, 2, 2, 2, 2, 2, 2, 2, 2, 2, 2, 2, 2, 2, 2, 2, 2, 2, 2, 2, 2, 2, 2, 2, 2, 2, 2, 2, 2, 2, 2, 2, 2, 2, 2, 2, 2, 2, 2, 2, 2, 2, 2, 2, 2, 2, 2, 2, 2, 2, 2, 2, 2, 2, 2, 2, 2, 2, 2, 2, 2, 2, 2, 2, 2, 2, 2, 2, 2, 2, 2, 2, 2, 2, 2, 2, 2, 2, 2, 2, 2, 2, 2, 2, 2, 2, 2, 2, 2, 2, 2, 2, 2, 2, 2, 2, 2, 2, 2, 2, 2, 2, 2, 2, 2, 2, 2, 2, 2, 2, 2, 2, 2, 2, 2, 2, 2, 2, 2, 2, 2, 2, 2, 2, 2, 2, 2, 2, 2, 2, 2, 2, 2, 2, 2, 2, 2, 2, 2, 2, 2, 2, 2, 2, 2, 2, 2, 2, 2, 2, 2, 2, 3 ),
 ( 0.000000000000000000, 1.000000000000000000 ),
 ( 0.000000000000000000, 0.003787878787878787984, 0.007575757575757575968, 0.01136363636363636395, 0.01515151515151515194, 0.01893939393939393992, 0.02272727272727272790, 0.02651515151515151589, 0.03030303030303030387, 0.03409090909090908839, 0.03787878787878787984, 0.04166666666666666435, 0.04545454545454545581, 0.04924242424242424032, 0.05303030303030303177, 0.05681818181818181629, 0.06060606060606060774, 0.06439393939393939226, 0.06818181818181817677, 0.07196969696969697516, 0.07575757575757575968, 0.07954545454545454419, 0.08333333333333332871, 0.08712121212121212710, 0.09090909090909091161, 0.09469696969696969613, 0.09848484848484848064, 0.1022727272727272790, 0.1060606060606060635, 0.1098484848484848481, 0.1136363636363636326, 0.1174242424242424310, 0.1212121212121212155, 0.1250000000000000000, 0.1287878787878787845, 0.1325757575757575690, 0.1363636363636363535, 0.1401515151515151381, 0.1439393939393939503, 0.1477272727272727348, 0.1515151515151515194, 0.1553030303030303039, 0.1590909090909090884, 0.1628787878787878729, 0.1666666666666666574, 0.1704545454545454419, 0.1742424242424242542, 0.1780303030303030387, 0.1818181818181818232, 0.1856060606060606077, 0.1893939393939393923, 0.1931818181818181768, 0.1969696969696969613, 0.2007575757575757458, 0.2045454545454545581, 0.2083333333333333426, 0.2121212121212121271, 0.2159090909090909116, 0.2196969696969696961, 0.2234848484848484806, 0.2272727272727272652, 0.2310606060606060497, 0.2348484848484848619, 0.2386363636363636465, 0.2424242424242424310, 0.2462121212121212155, 0.2500000000000000000, 0.2537878787878787845, 0.2575757575757575690, 0.2613636363636363535, 0.2651515151515151381, 0.2689393939393939226, 0.2727272727272727071, 0.2765151515151514916, 0.2803030303030302761, 0.2840909090909091161, 0.2878787878787879007, 0.2916666666666666852, 0.2954545454545454697, 0.2992424242424242542, 0.3030303030303030387, 0.3068181818181818232, 0.3106060606060606077, 0.3143939393939393923, 0.3181818181818181768, 0.3219696969696969613, 0.3257575757575757458, 0.3295454545454545303, 0.3333333333333333148, 0.3371212121212120993, 0.3409090909090908839, 0.3446969696969697239, 0.3484848484848485084, 0.3522727272727272929, 0.3560606060606060774, 0.3598484848484848619, 0.3636363636363636465, 0.3674242424242424310, 0.3712121212121212155, 0.3750000000000000000, 0.3787878787878787845, 0.3825757575757575690, 0.3863636363636363535, 0.3901515151515151381, 0.3939393939393939226, 0.3977272727272727071, 0.4015151515151514916, 0.4053030303030302761, 0.4090909090909091161, 0.4128787878787879007, 0.4166666666666666852, 0.4204545454545454697, 0.4242424242424242542, 0.4280303030303030387, 0.4318181818181818232, 0.4356060606060606077, 0.4393939393939393923, 0.4431818181818181768, 0.4469696969696969613, 0.4507575757575757458, 0.4545454545454545303, 0.4583333333333333148, 0.4621212121212120993, 0.4659090909090908839, 0.4696969696969697239, 0.4734848484848485084, 0.4772727272727272929, 0.4810606060606060774, 0.4848484848484848619, 0.4886363636363636465, 0.4924242424242424310, 0.4962121212121212155, 0.5000000000000000000, 0.5037878787878787845, 0.5075757575757575690, 0.5113636363636363535, 0.5151515151515151381, 0.5189393939393939226, 0.5227272727272727071, 0.5265151515151514916, 0.5303030303030302761, 0.5340909090909090606, 0.5378787878787878451, 0.5416666666666666297, 0.5454545454545454142, 0.5492424242424241987, 0.5530303030303029832, 0.5568181818181817677, 0.5606060606060605522, 0.5643939393939394478, 0.5681818181818182323, 0.5719696969696970168, 0.5757575757575758013, 0.5795454545454545858, 0.5833333333333333703, 0.5871212121212121549, 0.5909090909090909394, 0.5946969696969697239, 0.5984848484848485084, 0.6022727272727272929, 0.6060606060606060774, 0.6098484848484848619, 0.6136363636363636465, 0.6174242424242424310, 0.6212121212121212155, 0.6250000000000000000, 0.6287878787878787845, 0.6325757575757575690, 0.6363636363636363535, 0.6401515151515151381, 0.6439393939393939226, 0.6477272727272727071, 0.6515151515151514916, 0.6553030303030302761, 0.6590909090909090606, 0.6628787878787878451, 0.6666666666666666297, 0.6704545454545454142, 0.6742424242424241987, 0.6780303030303029832, 0.6818181818181817677, 0.6856060606060605522, 0.6893939393939394478, 0.6931818181818182323, 0.6969696969696970168, 0.7007575757575758013, 0.7045454545454545858, 0.7083333333333333703, 0.7121212121212121549, 0.7159090909090909394, 0.7196969696969697239, 0.7234848484848485084, 0.7272727272727272929, 0.7310606060606060774, 0.7348484848484848619, 0.7386363636363636465, 0.7424242424242424310, 0.7462121212121212155, 0.7500000000000000000, 0.7537878787878787845, 0.7575757575757575690, 0.7613636363636363535, 0.7651515151515151381, 0.7689393939393939226, 0.7727272727272727071, 0.7765151515151514916, 0.7803030303030302761, 0.7840909090909090606, 0.7878787878787878451, 0.7916666666666666297, 0.7954545454545454142, 0.7992424242424241987, 0.8030303030303029832, 0.8068181818181817677, 0.8106060606060605522, 0.8143939393939394478, 0.8181818181818182323, 0.8219696969696970168, 0.8257575757575758013, 0.8295454545454545858, 0.8333333333333333703, 0.8371212121212121549, 0.8409090909090909394, 0.8446969696969697239, 0.8484848484848485084, 0.8522727272727272929, 0.8560606060606060774, 0.8598484848484848619, 0.8636363636363636465, 0.8674242424242424310, 0.8712121212121212155, 0.8750000000000000000, 0.8787878787878787845, 0.8825757575757575690, 0.8863636363636363535, 0.8901515151515151381, 0.8939393939393939226, 0.8977272727272727071, 0.9015151515151514916, 0.9053030303030302761, 0.9090909090909090606, 0.9128787878787878451, 0.9166666666666666297, 0.9204545454545454142, 0.9242424242424241987, 0.9280303030303029832, 0.9318181818181817677, 0.9356060606060605522, 0.9393939393939394478, 0.9431818181818182323, 0.9469696969696970168, 0.9507575757575758013, 0.9545454545454545858, 0.9583333333333333703, 0.9621212121212121549, 0.9659090909090909394 ),
 .UNSPECIFIED. ) 
 GEOMETRIC_REPRESENTATION_ITEM ( )  RATIONAL_B_SPLINE_SURFACE ( (
 ( 1.000000000000000000, 0.9659258262890683122, 1.000000000000000000, 0.9659258262890683122, 1.000000000000000000, 0.9659258262890683122, 1.000000000000000000, 0.9659258262890683122, 1.000000000000000000, 0.9659258262890683122, 1.000000000000000000, 0.9659258262890683122, 1.000000000000000000, 0.9659258262890683122, 1.000000000000000000, 0.9659258262890683122, 1.000000000000000000, 0.9659258262890683122, 1.000000000000000000, 0.9659258262890683122, 1.000000000000000000, 0.9659258262890683122, 1.000000000000000000, 0.9659258262890683122, 1.000000000000000000, 0.9659258262890683122, 1.000000000000000000, 0.9659258262890683122, 1.000000000000000000, 0.9659258262890683122, 1.000000000000000000, 0.9659258262890683122, 1.000000000000000000, 0.9659258262890683122, 1.000000000000000000, 0.9659258262890683122, 1.000000000000000000, 0.9659258262890683122, 1.000000000000000000, 0.9659258262890683122, 1.000000000000000000, 0.9659258262890683122, 1.000000000000000000, 0.9659258262890683122, 1.000000000000000000, 0.9659258262890683122, 1.000000000000000000, 0.9659258262890683122, 1.000000000000000000, 0.9659258262890683122, 1.000000000000000000, 0.9659258262890683122, 1.000000000000000000, 0.9659258262890683122, 1.000000000000000000, 0.9659258262890683122, 1.000000000000000000, 0.9659258262890683122, 1.000000000000000000, 0.9659258262890683122, 1.000000000000000000, 0.9659258262890683122, 1.000000000000000000, 0.9659258262890683122, 1.000000000000000000, 0.9659258262890683122, 1.000000000000000000, 0.9659258262890683122, 1.000000000000000000, 0.9659258262890683122, 1.000000000000000000, 0.9659258262890683122, 1.000000000000000000, 0.9659258262890683122, 1.000000000000000000, 0.9659258262890683122, 1.000000000000000000, 0.9659258262890683122, 1.000000000000000000, 0.9659258262890683122, 1.000000000000000000, 0.9659258262890683122, 1.000000000000000000, 0.9659258262890683122, 1.000000000000000000, 0.9659258262890683122, 1.000000000000000000, 0.9659258262890683122, 1.000000000000000000, 0.9659258262890683122, 1.000000000000000000, 0.9659258262890683122, 1.000000000000000000, 0.9659258262890683122, 1.000000000000000000, 0.9659258262890683122, 1.000000000000000000, 0.9659258262890683122, 1.000000000000000000, 0.9659258262890683122, 1.000000000000000000, 0.9659258262890683122, 1.000000000000000000, 0.9659258262890683122, 1.000000000000000000, 0.9659258262890683122, 1.000000000000000000, 0.9659258262890683122, 1.000000000000000000, 0.9659258262890683122, 1.000000000000000000, 0.9659258262890683122, 1.000000000000000000, 0.9659258262890683122, 1.000000000000000000, 0.9659258262890683122, 1.000000000000000000, 0.9659258262890683122, 1.000000000000000000, 0.9659258262890683122, 1.000000000000000000, 0.9659258262890683122, 1.000000000000000000, 0.9659258262890683122, 1.000000000000000000, 0.9659258262890683122, 1.000000000000000000, 0.9659258262890683122, 1.000000000000000000, 0.9659258262890683122, 1.000000000000000000, 0.9659258262890683122, 1.000000000000000000, 0.9659258262890683122, 1.000000000000000000, 0.9659258262890683122, 1.000000000000000000, 0.9659258262890683122, 1.000000000000000000, 0.9659258262890683122, 1.000000000000000000, 0.9659258262890683122, 1.000000000000000000, 0.9659258262890683122, 1.000000000000000000, 0.9659258262890683122, 1.000000000000000000, 0.9659258262890683122, 1.000000000000000000, 0.9659258262890683122, 1.000000000000000000, 0.9659258262890683122, 1.000000000000000000, 0.9659258262890683122, 1.000000000000000000, 0.9659258262890683122, 1.000000000000000000, 0.9659258262890683122, 1.000000000000000000, 0.9659258262890683122, 1.000000000000000000, 0.9659258262890683122, 1.000000000000000000, 0.9659258262890683122, 1.000000000000000000, 0.9659258262890683122, 1.000000000000000000, 0.9659258262890683122, 1.000000000000000000, 0.9659258262890683122, 1.000000000000000000, 0.9659258262890683122, 1.000000000000000000, 0.9659258262890683122, 1.000000000000000000, 0.9659258262890683122, 1.000000000000000000, 0.9659258262890683122, 1.000000000000000000, 0.9659258262890683122, 1.000000000000000000, 0.9659258262890683122, 1.000000000000000000, 0.9659258262890683122, 1.000000000000000000, 0.9659258262890683122, 1.000000000000000000, 0.9659258262890683122, 1.000000000000000000, 0.9659258262890683122, 1.000000000000000000, 0.9659258262890683122, 1.000000000000000000, 0.9659258262890683122, 1.000000000000000000, 0.9659258262890683122, 1.000000000000000000, 0.9659258262890683122, 1.000000000000000000, 0.9659258262890683122, 1.000000000000000000, 0.9659258262890683122, 1.000000000000000000, 0.9659258262890683122, 1.000000000000000000, 0.9659258262890683122, 1.000000000000000000, 0.9659258262890683122, 1.000000000000000000, 0.9659258262890683122, 1.000000000000000000, 0.9659258262890683122, 1.000000000000000000, 0.9659258262890683122, 1.000000000000000000, 0.9659258262890683122, 1.000000000000000000, 0.9659258262890683122, 1.000000000000000000, 0.9659258262890683122, 1.000000000000000000, 0.9659258262890683122, 1.000000000000000000, 0.9659258262890683122, 1.000000000000000000, 0.9659258262890683122, 1.000000000000000000, 0.9659258262890683122, 1.000000000000000000, 0.9659258262890683122, 1.000000000000000000, 0.9659258262890683122, 1.000000000000000000, 0.9659258262890683122, 1.000000000000000000, 0.9659258262890683122, 1.000000000000000000, 0.9659258262890683122, 1.000000000000000000, 0.9659258262890683122, 1.000000000000000000, 0.9659258262890683122, 1.000000000000000000, 0.9659258262890683122, 1.000000000000000000, 0.9659258262890683122, 1.000000000000000000, 0.9659258262890683122, 1.000000000000000000, 0.9659258262890683122, 1.000000000000000000, 0.9659258262890683122, 1.000000000000000000, 0.9659258262890683122, 1.000000000000000000, 0.9659258262890683122, 1.000000000000000000, 0.9659258262890683122, 1.000000000000000000, 0.9659258262890683122, 1.000000000000000000, 0.9659258262890683122, 1.000000000000000000, 0.9659258262890683122, 1.000000000000000000, 0.9659258262890683122, 1.000000000000000000, 0.9659258262890683122, 1.000000000000000000, 0.9659258262890683122, 1.000000000000000000, 0.9659258262890683122, 1.000000000000000000, 0.9659258262890683122, 1.000000000000000000, 0.9659258262890683122, 1.000000000000000000, 0.9659258262890683122, 1.000000000000000000, 0.9659258262890683122, 1.000000000000000000, 0.9659258262890683122, 1.000000000000000000, 0.9659258262890683122, 1.000000000000000000, 0.9659258262890683122, 1.000000000000000000, 0.9659258262890683122, 1.000000000000000000, 0.9659258262890683122, 1.000000000000000000, 0.9659258262890683122, 1.000000000000000000, 0.9659258262890683122, 1.000000000000000000, 0.9659258262890683122, 1.000000000000000000, 0.9659258262890683122, 1.000000000000000000, 0.9659258262890683122, 1.000000000000000000, 0.9659258262890683122, 1.000000000000000000, 0.9659258262890683122, 1.000000000000000000, 0.9659258262890683122, 1.000000000000000000, 0.9659258262890683122, 1.000000000000000000, 0.9659258262890683122, 1.000000000000000000, 0.9659258262890683122, 1.000000000000000000, 0.9659258262890683122, 1.000000000000000000, 0.9659258262890683122, 1.000000000000000000, 0.9659258262890683122, 1.000000000000000000, 0.9659258262890683122, 1.000000000000000000, 0.9659258262890683122, 1.000000000000000000, 0.9659258262890683122, 1.000000000000000000, 0.9659258262890683122, 1.000000000000000000, 0.9659258262890683122, 1.000000000000000000, 0.9659258262890683122, 1.000000000000000000, 0.9659258262890683122, 1.000000000000000000, 0.9659258262890683122, 1.000000000000000000, 0.9659258262890683122, 1.000000000000000000, 0.9659258262890683122, 1.000000000000000000, 0.9659258262890683122, 1.000000000000000000, 0.9659258262890683122, 1.000000000000000000, 0.9659258262890683122, 1.000000000000000000, 0.9659258262890683122, 1.000000000000000000, 0.9659258262890683122, 1.000000000000000000, 0.9659258262890683122, 1.000000000000000000, 0.9659258262890683122, 1.000000000000000000, 0.9659258262890683122, 1.000000000000000000, 0.9659258262890683122, 1.000000000000000000, 0.9659258262890683122, 1.000000000000000000, 0.9659258262890683122, 1.000000000000000000, 0.9659258262890683122, 1.000000000000000000, 0.9659258262890683122, 1.000000000000000000, 0.9659258262890683122, 1.000000000000000000, 0.9659258262890683122, 1.000000000000000000, 0.9659258262890683122, 1.000000000000000000, 0.9659258262890683122, 1.000000000000000000, 0.9659258262890683122, 1.000000000000000000, 0.9659258262890683122, 1.000000000000000000, 0.9659258262890683122, 1.000000000000000000, 0.9659258262890683122, 1.000000000000000000, 0.9659258262890683122, 1.000000000000000000, 0.9659258262890683122, 1.000000000000000000, 0.9659258262890683122, 1.000000000000000000, 0.9659258262890683122, 1.000000000000000000, 0.9659258262890683122, 1.000000000000000000, 0.9659258262890683122, 1.000000000000000000, 0.9659258262890683122, 1.000000000000000000, 0.9659258262890683122, 1.000000000000000000, 0.9659258262890683122, 1.000000000000000000, 0.9659258262890683122, 1.000000000000000000, 0.9659258262890683122, 1.000000000000000000, 0.9659258262890683122, 1.000000000000000000, 0.9659258262890683122, 1.000000000000000000, 0.9659258262890683122, 1.000000000000000000, 0.9659258262890683122, 1.000000000000000000, 0.9659258262890683122, 1.000000000000000000, 0.9659258262890683122, 1.000000000000000000, 0.9659258262890683122, 1.000000000000000000, 0.9659258262890683122, 1.000000000000000000, 0.9659258262890683122, 1.000000000000000000, 0.9659258262890683122, 1.000000000000000000, 0.9659258262890683122, 1.000000000000000000, 0.9659258262890683122, 1.000000000000000000, 0.9659258262890683122, 1.000000000000000000, 0.9659258262890683122, 1.000000000000000000, 0.9659258262890683122, 1.000000000000000000, 0.9659258262890683122, 1.000000000000000000, 0.9659258262890683122, 1.000000000000000000, 0.9659258262890683122, 1.000000000000000000, 0.9659258262890683122, 1.000000000000000000, 0.9659258262890683122, 1.000000000000000000, 0.9659258262890683122, 1.000000000000000000, 0.9659258262890683122, 1.000000000000000000, 0.9659258262890683122, 1.000000000000000000, 0.9659258262890683122, 1.000000000000000000, 0.9659258262890683122, 1.000000000000000000, 0.9659258262890683122, 1.000000000000000000, 0.9659258262890683122, 1.000000000000000000, 0.9659258262890683122, 1.000000000000000000, 0.9659258262890683122, 1.000000000000000000, 0.9659258262890683122, 1.000000000000000000, 0.9659258262890683122, 1.000000000000000000, 0.9659258262890683122, 1.000000000000000000, 0.9659258262890683122, 1.000000000000000000, 0.9659258262890683122, 1.000000000000000000, 0.9659258262890683122, 1.000000000000000000, 0.9659258262890683122, 1.000000000000000000, 0.9659258262890683122, 1.000000000000000000, 0.9659258262890683122, 1.000000000000000000, 0.9659258262890683122, 1.000000000000000000, 0.9659258262890683122, 1.000000000000000000, 0.9659258262890683122, 1.000000000000000000, 0.9659258262890683122, 1.000000000000000000, 0.9659258262890683122, 1.000000000000000000, 0.9659258262890683122, 1.000000000000000000, 0.9659258262890683122, 1.000000000000000000, 0.9659258262890683122, 1.000000000000000000, 0.9659258262890683122, 1.000000000000000000, 0.9659258262890683122, 1.000000000000000000, 0.9659258262890683122, 1.000000000000000000, 0.9659258262890683122, 1.000000000000000000, 0.9659258262890683122, 1.000000000000000000, 0.9659258262890683122, 1.000000000000000000, 0.9659258262890683122, 1.000000000000000000, 0.9659258262890683122, 1.000000000000000000),
 ( 1.000000000000000000, 0.9659258262890683122, 1.000000000000000000, 0.9659258262890683122, 1.000000000000000000, 0.9659258262890683122, 1.000000000000000000, 0.9659258262890683122, 1.000000000000000000, 0.9659258262890683122, 1.000000000000000000, 0.9659258262890683122, 1.000000000000000000, 0.9659258262890683122, 1.000000000000000000, 0.9659258262890683122, 1.000000000000000000, 0.9659258262890683122, 1.000000000000000000, 0.9659258262890683122, 1.000000000000000000, 0.9659258262890683122, 1.000000000000000000, 0.9659258262890683122, 1.000000000000000000, 0.9659258262890683122, 1.000000000000000000, 0.9659258262890683122, 1.000000000000000000, 0.9659258262890683122, 1.000000000000000000, 0.9659258262890683122, 1.000000000000000000, 0.9659258262890683122, 1.000000000000000000, 0.9659258262890683122, 1.000000000000000000, 0.9659258262890683122, 1.000000000000000000, 0.9659258262890683122, 1.000000000000000000, 0.9659258262890683122, 1.000000000000000000, 0.9659258262890683122, 1.000000000000000000, 0.9659258262890683122, 1.000000000000000000, 0.9659258262890683122, 1.000000000000000000, 0.9659258262890683122, 1.000000000000000000, 0.9659258262890683122, 1.000000000000000000, 0.9659258262890683122, 1.000000000000000000, 0.9659258262890683122, 1.000000000000000000, 0.9659258262890683122, 1.000000000000000000, 0.9659258262890683122, 1.000000000000000000, 0.9659258262890683122, 1.000000000000000000, 0.9659258262890683122, 1.000000000000000000, 0.9659258262890683122, 1.000000000000000000, 0.9659258262890683122, 1.000000000000000000, 0.9659258262890683122, 1.000000000000000000, 0.9659258262890683122, 1.000000000000000000, 0.9659258262890683122, 1.000000000000000000, 0.9659258262890683122, 1.000000000000000000, 0.9659258262890683122, 1.000000000000000000, 0.9659258262890683122, 1.000000000000000000, 0.9659258262890683122, 1.000000000000000000, 0.9659258262890683122, 1.000000000000000000, 0.9659258262890683122, 1.000000000000000000, 0.9659258262890683122, 1.000000000000000000, 0.9659258262890683122, 1.000000000000000000, 0.9659258262890683122, 1.000000000000000000, 0.9659258262890683122, 1.000000000000000000, 0.9659258262890683122, 1.000000000000000000, 0.9659258262890683122, 1.000000000000000000, 0.9659258262890683122, 1.000000000000000000, 0.9659258262890683122, 1.000000000000000000, 0.9659258262890683122, 1.000000000000000000, 0.9659258262890683122, 1.000000000000000000, 0.9659258262890683122, 1.000000000000000000, 0.9659258262890683122, 1.000000000000000000, 0.9659258262890683122, 1.000000000000000000, 0.9659258262890683122, 1.000000000000000000, 0.9659258262890683122, 1.000000000000000000, 0.9659258262890683122, 1.000000000000000000, 0.9659258262890683122, 1.000000000000000000, 0.9659258262890683122, 1.000000000000000000, 0.9659258262890683122, 1.000000000000000000, 0.9659258262890683122, 1.000000000000000000, 0.9659258262890683122, 1.000000000000000000, 0.9659258262890683122, 1.000000000000000000, 0.9659258262890683122, 1.000000000000000000, 0.9659258262890683122, 1.000000000000000000, 0.9659258262890683122, 1.000000000000000000, 0.9659258262890683122, 1.000000000000000000, 0.9659258262890683122, 1.000000000000000000, 0.9659258262890683122, 1.000000000000000000, 0.9659258262890683122, 1.000000000000000000, 0.9659258262890683122, 1.000000000000000000, 0.9659258262890683122, 1.000000000000000000, 0.9659258262890683122, 1.000000000000000000, 0.9659258262890683122, 1.000000000000000000, 0.9659258262890683122, 1.000000000000000000, 0.9659258262890683122, 1.000000000000000000, 0.9659258262890683122, 1.000000000000000000, 0.9659258262890683122, 1.000000000000000000, 0.9659258262890683122, 1.000000000000000000, 0.9659258262890683122, 1.000000000000000000, 0.9659258262890683122, 1.000000000000000000, 0.9659258262890683122, 1.000000000000000000, 0.9659258262890683122, 1.000000000000000000, 0.9659258262890683122, 1.000000000000000000, 0.9659258262890683122, 1.000000000000000000, 0.9659258262890683122, 1.000000000000000000, 0.9659258262890683122, 1.000000000000000000, 0.9659258262890683122, 1.000000000000000000, 0.9659258262890683122, 1.000000000000000000, 0.9659258262890683122, 1.000000000000000000, 0.9659258262890683122, 1.000000000000000000, 0.9659258262890683122, 1.000000000000000000, 0.9659258262890683122, 1.000000000000000000, 0.9659258262890683122, 1.000000000000000000, 0.9659258262890683122, 1.000000000000000000, 0.9659258262890683122, 1.000000000000000000, 0.9659258262890683122, 1.000000000000000000, 0.9659258262890683122, 1.000000000000000000, 0.9659258262890683122, 1.000000000000000000, 0.9659258262890683122, 1.000000000000000000, 0.9659258262890683122, 1.000000000000000000, 0.9659258262890683122, 1.000000000000000000, 0.9659258262890683122, 1.000000000000000000, 0.9659258262890683122, 1.000000000000000000, 0.9659258262890683122, 1.000000000000000000, 0.9659258262890683122, 1.000000000000000000, 0.9659258262890683122, 1.000000000000000000, 0.9659258262890683122, 1.000000000000000000, 0.9659258262890683122, 1.000000000000000000, 0.9659258262890683122, 1.000000000000000000, 0.9659258262890683122, 1.000000000000000000, 0.9659258262890683122, 1.000000000000000000, 0.9659258262890683122, 1.000000000000000000, 0.9659258262890683122, 1.000000000000000000, 0.9659258262890683122, 1.000000000000000000, 0.9659258262890683122, 1.000000000000000000, 0.9659258262890683122, 1.000000000000000000, 0.9659258262890683122, 1.000000000000000000, 0.9659258262890683122, 1.000000000000000000, 0.9659258262890683122, 1.000000000000000000, 0.9659258262890683122, 1.000000000000000000, 0.9659258262890683122, 1.000000000000000000, 0.9659258262890683122, 1.000000000000000000, 0.9659258262890683122, 1.000000000000000000, 0.9659258262890683122, 1.000000000000000000, 0.9659258262890683122, 1.000000000000000000, 0.9659258262890683122, 1.000000000000000000, 0.9659258262890683122, 1.000000000000000000, 0.9659258262890683122, 1.000000000000000000, 0.9659258262890683122, 1.000000000000000000, 0.9659258262890683122, 1.000000000000000000, 0.9659258262890683122, 1.000000000000000000, 0.9659258262890683122, 1.000000000000000000, 0.9659258262890683122, 1.000000000000000000, 0.9659258262890683122, 1.000000000000000000, 0.9659258262890683122, 1.000000000000000000, 0.9659258262890683122, 1.000000000000000000, 0.9659258262890683122, 1.000000000000000000, 0.9659258262890683122, 1.000000000000000000, 0.9659258262890683122, 1.000000000000000000, 0.9659258262890683122, 1.000000000000000000, 0.9659258262890683122, 1.000000000000000000, 0.9659258262890683122, 1.000000000000000000, 0.9659258262890683122, 1.000000000000000000, 0.9659258262890683122, 1.000000000000000000, 0.9659258262890683122, 1.000000000000000000, 0.9659258262890683122, 1.000000000000000000, 0.9659258262890683122, 1.000000000000000000, 0.9659258262890683122, 1.000000000000000000, 0.9659258262890683122, 1.000000000000000000, 0.9659258262890683122, 1.000000000000000000, 0.9659258262890683122, 1.000000000000000000, 0.9659258262890683122, 1.000000000000000000, 0.9659258262890683122, 1.000000000000000000, 0.9659258262890683122, 1.000000000000000000, 0.9659258262890683122, 1.000000000000000000, 0.9659258262890683122, 1.000000000000000000, 0.9659258262890683122, 1.000000000000000000, 0.9659258262890683122, 1.000000000000000000, 0.9659258262890683122, 1.000000000000000000, 0.9659258262890683122, 1.000000000000000000, 0.9659258262890683122, 1.000000000000000000, 0.9659258262890683122, 1.000000000000000000, 0.9659258262890683122, 1.000000000000000000, 0.9659258262890683122, 1.000000000000000000, 0.9659258262890683122, 1.000000000000000000, 0.9659258262890683122, 1.000000000000000000, 0.9659258262890683122, 1.000000000000000000, 0.9659258262890683122, 1.000000000000000000, 0.9659258262890683122, 1.000000000000000000, 0.9659258262890683122, 1.000000000000000000, 0.9659258262890683122, 1.000000000000000000, 0.9659258262890683122, 1.000000000000000000, 0.9659258262890683122, 1.000000000000000000, 0.9659258262890683122, 1.000000000000000000, 0.9659258262890683122, 1.000000000000000000, 0.9659258262890683122, 1.000000000000000000, 0.9659258262890683122, 1.000000000000000000, 0.9659258262890683122, 1.000000000000000000, 0.9659258262890683122, 1.000000000000000000, 0.9659258262890683122, 1.000000000000000000, 0.9659258262890683122, 1.000000000000000000, 0.9659258262890683122, 1.000000000000000000, 0.9659258262890683122, 1.000000000000000000, 0.9659258262890683122, 1.000000000000000000, 0.9659258262890683122, 1.000000000000000000, 0.9659258262890683122, 1.000000000000000000, 0.9659258262890683122, 1.000000000000000000, 0.9659258262890683122, 1.000000000000000000, 0.9659258262890683122, 1.000000000000000000, 0.9659258262890683122, 1.000000000000000000, 0.9659258262890683122, 1.000000000000000000, 0.9659258262890683122, 1.000000000000000000, 0.9659258262890683122, 1.000000000000000000, 0.9659258262890683122, 1.000000000000000000, 0.9659258262890683122, 1.000000000000000000, 0.9659258262890683122, 1.000000000000000000, 0.9659258262890683122, 1.000000000000000000, 0.9659258262890683122, 1.000000000000000000, 0.9659258262890683122, 1.000000000000000000, 0.9659258262890683122, 1.000000000000000000, 0.9659258262890683122, 1.000000000000000000, 0.9659258262890683122, 1.000000000000000000, 0.9659258262890683122, 1.000000000000000000, 0.9659258262890683122, 1.000000000000000000, 0.9659258262890683122, 1.000000000000000000, 0.9659258262890683122, 1.000000000000000000, 0.9659258262890683122, 1.000000000000000000, 0.9659258262890683122, 1.000000000000000000, 0.9659258262890683122, 1.000000000000000000, 0.9659258262890683122, 1.000000000000000000, 0.9659258262890683122, 1.000000000000000000, 0.9659258262890683122, 1.000000000000000000, 0.9659258262890683122, 1.000000000000000000, 0.9659258262890683122, 1.000000000000000000, 0.9659258262890683122, 1.000000000000000000, 0.9659258262890683122, 1.000000000000000000, 0.9659258262890683122, 1.000000000000000000, 0.9659258262890683122, 1.000000000000000000, 0.9659258262890683122, 1.000000000000000000, 0.9659258262890683122, 1.000000000000000000, 0.9659258262890683122, 1.000000000000000000, 0.9659258262890683122, 1.000000000000000000, 0.9659258262890683122, 1.000000000000000000, 0.9659258262890683122, 1.000000000000000000, 0.9659258262890683122, 1.000000000000000000, 0.9659258262890683122, 1.000000000000000000, 0.9659258262890683122, 1.000000000000000000, 0.9659258262890683122, 1.000000000000000000, 0.9659258262890683122, 1.000000000000000000, 0.9659258262890683122, 1.000000000000000000, 0.9659258262890683122, 1.000000000000000000, 0.9659258262890683122, 1.000000000000000000, 0.9659258262890683122, 1.000000000000000000, 0.9659258262890683122, 1.000000000000000000, 0.9659258262890683122, 1.000000000000000000, 0.9659258262890683122, 1.000000000000000000, 0.9659258262890683122, 1.000000000000000000, 0.9659258262890683122, 1.000000000000000000, 0.9659258262890683122, 1.000000000000000000, 0.9659258262890683122, 1.000000000000000000, 0.9659258262890683122, 1.000000000000000000, 0.9659258262890683122, 1.000000000000000000, 0.9659258262890683122, 1.000000000000000000, 0.9659258262890683122, 1.000000000000000000, 0.9659258262890683122, 1.000000000000000000, 0.9659258262890683122, 1.000000000000000000, 0.9659258262890683122, 1.000000000000000000, 0.9659258262890683122, 1.000000000000000000, 0.9659258262890683122, 1.000000000000000000, 0.9659258262890683122, 1.000000000000000000, 0.9659258262890683122, 1.000000000000000000, 0.9659258262890683122, 1.000000000000000000) ) ) 
 REPRESENTATION_ITEM ( '' )  SURFACE ( )  );
#49407 = CARTESIAN_POINT ( 'NONE',  ( 0.000000000000000000, 0.000000000000000000, 0.000000000000000000 ) ) ;
#49408 = CARTESIAN_POINT ( 'NONE',  ( 1.561679790026247350, -0.4281496062992124485, 0.4176697321401328655 ) ) ;
#49409 = AXIS2_PLACEMENT_3D ( 'NONE', #73975, #28925, #42374 ) ;
#49410 = CARTESIAN_POINT ( 'NONE',  ( 0.2362204724409451007, -0.4091458600556402980, -1.900918635170603554 ) ) ;
#49411 = CARTESIAN_POINT ( 'NONE',  ( -1.036745406824146176, 0.05413385826771626580, -0.4176697321401330321 ) ) ;
#49412 = CARTESIAN_POINT ( 'NONE',  ( -0.9842519685039360366, 0.1771653543307087630, 0.000000000000000000 ) ) ;
#49413 = CARTESIAN_POINT ( 'NONE',  ( -0.5643044619422565855, -0.004921259842519870586, -0.3153832671262229437 ) ) ;
#49414 = CARTESIAN_POINT ( 'NONE',  ( -1.220472440944881054, 0.000000000000000000, 0.5309055118110237448 ) ) ;
#49415 = CARTESIAN_POINT ( 'NONE',  ( 0.05905511811023709395, -0.5400638737290844871, 0.3530559997133364547 ) ) ;
#49416 = CARTESIAN_POINT ( 'NONE',  ( 0.05249343832021075018, -0.5023911411419708095, 0.1820866141732285504 ) ) ;
#49417 = CARTESIAN_POINT ( 'NONE',  ( -0.9973753280839886548, -0.5023911411419708095, -0.1820866141732282451 ) ) ;
#49418 = CARTESIAN_POINT ( 'NONE',  ( -1.496062992125983815, -0.1870078740157480879, -0.4822834645669291653 ) ) ;
#49419 = CARTESIAN_POINT ( 'NONE',  ( 1.154855643044620184, 0.1283753931104746893, -0.1820866141732285504 ) ) ;
#49420 = CARTESIAN_POINT ( 'NONE',  ( 0.8202099737532814183, -0.6692913385826773087, -0.1292274648535924053 ) ) ;
#49421 = CARTESIAN_POINT ( 'NONE',  ( 2.795275590551181910, 1.535433070866142335, 0.000000000000000000 ) ) ;
#49422 = CARTESIAN_POINT ( 'NONE',  ( 0.6561679790026253567, -0.5023911411419708095, -0.1820866141732282451 ) ) ;
#49423 = CARTESIAN_POINT ( 'NONE',  ( 0.7480314960629927956, 0.2952755905511811885, 0.000000000000000000 ) ) ;
#49424 = CARTESIAN_POINT ( 'NONE',  ( 1.030183727034121421, -0.2845877964562161244, -0.3641732283464567121 ) ) ;
#49425 = ORIENTED_EDGE ( 'NONE', *, *, #20715, .F. ) ;
#49426 = CARTESIAN_POINT ( 'NONE',  ( -1.227034120734907141, -0.6692913385826773087, -0.1292274648535924053 ) ) ;
#49427 = EDGE_CURVE ( 'NONE', #13254, #55363, #35455, .T. ) ;
#49428 = CARTESIAN_POINT ( 'NONE',  ( -0.8989501312335946848, -0.6692913385826771977, 0.1292274648535927661 ) ) ;
#49429 = CARTESIAN_POINT ( 'NONE',  ( 0.07874015748031558404, -0.1870078740157480879, -0.4822834645669291653 ) ) ;
#49430 = DIRECTION ( 'NONE',  ( 0.000000000000000000, 0.000000000000000000, 1.000000000000000000 ) ) ;
#49431 = CARTESIAN_POINT ( 'NONE',  ( 0.2925321140481932369, -0.2925321140481931814, -2.064960629921259727 ) ) ;
#49432 = CARTESIAN_POINT ( 'NONE',  ( 0.3280839895013130669, 0.05413385826771666132, 0.4176697321401328100 ) ) ;
#49433 = CARTESIAN_POINT ( 'NONE',  ( 1.594488188976378673, 0.07958543189024085140, 0.2665933059059887866 ) ) ;
#49434 = CARTESIAN_POINT ( 'NONE',  ( 0.006561679790026889343, -0.3162353388693409650, -0.4822834645669289433 ) ) ;
#49435 = CARTESIAN_POINT ( 'NONE',  ( 0.6299212598425204535, -0.1870078740157479769, 0.4822834645669291653 ) ) ;
#49436 = CARTESIAN_POINT ( 'NONE',  ( -0.3996062992125987146, 0.1070741851644051862, -1.765091863517059823 ) ) ;
#49437 = CARTESIAN_POINT ( 'NONE',  ( 0.3420746716998659953, 0.1974969037888705536, -1.706036745406824151 ) ) ;
#49438 = CARTESIAN_POINT ( 'NONE',  ( -0.3460692066303960868, 0.1998031496062990242, -2.860892388451443669 ) ) ;
#49439 = CARTESIAN_POINT ( 'NONE',  ( 3.912791665790199769, 1.724409448818897905, 0.4359958488159722534 ) ) ;
#49440 = CARTESIAN_POINT ( 'NONE',  ( 0.1958661417322834775, 0.3392501089628018884, -0.7664041994750655507 ) ) ;
#49441 = CARTESIAN_POINT ( 'NONE',  ( -0.4330708661417315697, 0.1771653543307087630, 0.000000000000000000 ) ) ;
#49442 = CARTESIAN_POINT ( 'NONE',  ( -0.8595800524934373854, -0.3162353388693409650, -0.4822834645669289433 ) ) ;
#49443 = CARTESIAN_POINT ( 'NONE',  ( 0.6167979002624678353, -0.4281496062992124485, 0.4176697321401328655 ) ) ;
#49444 = CARTESIAN_POINT ( 'NONE',  ( 0.1058382717557499880, 0.3949938075777409408, -2.117454068241470200 ) ) ;
#49445 = CARTESIAN_POINT ( 'NONE',  ( 1.049868766404200349, 0.2306618581243848609, 0.2411417322834645549 ) ) ;
#49446 = CARTESIAN_POINT ( 'NONE',  ( 1.541994750656168645, -0.6692913385826771977, 0.1292274648535927661 ) ) ;
#49447 = CARTESIAN_POINT ( 'NONE',  ( 1.338582677165355062, -0.1870078740157480879, -0.4822834645669291653 ) ) ;
#49448 = CARTESIAN_POINT ( 'NONE',  ( -1.157146581871515012E-16, 0.4724409448818898682, -2.519685039370078705 ) ) ;
#49449 = CARTESIAN_POINT ( 'NONE',  ( -0.3996062992125986035, -0.1070741851644056997, -1.620734908136482799 ) ) ;
#49450 = CARTESIAN_POINT ( 'NONE',  ( 1.128608923884514947, 0.2306618581243848609, 0.2411417322834645549 ) ) ;
#49451 = CARTESIAN_POINT ( 'NONE',  ( 0.8727034120734912248, -0.3162353388693409650, -0.4822834645669289433 ) ) ;
#49452 = CARTESIAN_POINT ( 'NONE',  ( 0.4396325459317590445, -0.6692913385826771977, 0.1292274648535927661 ) ) ;
#49453 = CARTESIAN_POINT ( 'NONE',  ( 1.056430446194226436, -0.5511811023622048555, -0.09757992244046775898 ) ) ;
#49455 = CARTESIAN_POINT ( 'NONE',  ( 1.587926509186352142, 0.05413385826771666132, 0.4176697321401328100 ) ) ;
#49454 = CARTESIAN_POINT ( 'NONE',  ( -1.594488188976377119, 0.07958543189024071263, -0.2665933059059888421 ) ) ;
#49456 = CARTESIAN_POINT ( 'NONE',  ( 4.797336870675655290E-17, -0.3917322834645669549, -2.678458374506874851 ) ) ;
#49457 = CARTESIAN_POINT ( 'NONE',  ( 0.7742782152230979209, 0.05413385826771626580, -0.4176697321401330321 ) ) ;
#49458 = CARTESIAN_POINT ( 'NONE',  ( 1.587926509186352586, -0.3690944881889765550, -0.3153832671262227771 ) ) ;
#49459 = CARTESIAN_POINT ( 'NONE',  ( -0.6824146981627291497, -0.6046776061558809534, -0.2411417322834644161 ) ) ;
#49460 = CARTESIAN_POINT ( 'NONE',  ( -0.3937007874015740483, -0.1870078740157480879, -0.4822834645669291653 ) ) ;
#49461 = EDGE_CURVE ( 'NONE', #50709, #40260, #42174, .T. ) ;
#49462 = CARTESIAN_POINT ( 'NONE',  ( -1.601049868766403650, 0.2306618581243847221, -0.2411417322834647770 ) ) ;
#49463 = CARTESIAN_POINT ( 'NONE',  ( 0.3917322834645670104, 2.398668435337828261E-17, -0.2027559055118111353 ) ) ;
#49464 = CARTESIAN_POINT ( 'NONE',  ( 0.1837270341207354329, 0.2306618581243848609, 0.2411417322834645549 ) ) ;
#49465 = CARTESIAN_POINT ( 'NONE',  ( -0.2867679344610364334, -0.2867679344610367109, -2.098425196850393526 ) ) ;
#49466 = CARTESIAN_POINT ( 'NONE',  ( -1.541994750656167090, -0.5511811023622048555, -0.09757992244046775898 ) ) ;
#49467 = ORIENTED_EDGE ( 'NONE', *, *, #52265, .F. ) ;
#49468 = CARTESIAN_POINT ( 'NONE',  ( 0.3420746716998659953, 0.1974969037888705536, -2.650918635170603554 ) ) ;
#49469 = VERTEX_POINT ( 'NONE', #24498 ) ;
#49470 = DIRECTION ( 'NONE',  ( 0.000000000000000000, -1.408710688920637755E-15, -1.000000000000000000 ) ) ;
#49471 = VECTOR ( 'NONE', #17759, 39.37007874015748143 ) ;
#49472 = CARTESIAN_POINT ( 'NONE',  ( 1.174540682414699111, -0.08942795157528024563, -0.3641732283464568787 ) ) ;
#49473 = CARTESIAN_POINT ( 'NONE',  ( 0.1998031496062994405, -0.3460692066303958092, -1.194225721784776928 ) ) ;
#49474 = CARTESIAN_POINT ( 'NONE',  ( 1.528871391076116026, 0.1771653543307087630, 0.09757992244046791164 ) ) ;
#49475 = CARTESIAN_POINT ( 'NONE',  ( -0.1115485564304456445, 0.2066929133858267098, -0.1054918080437494132 ) ) ;
#49476 = CARTESIAN_POINT ( 'NONE',  ( 0.4800390104732028540, 1.504150543744003032, 0.5309055118110234117 ) ) ;
#49477 = CARTESIAN_POINT ( 'NONE',  ( 0.5314960629921322566, 2.755905511811024056, -1.813482582612291782 ) ) ;
#49478 = CARTESIAN_POINT ( 'NONE',  ( -0.2867679344610364334, -0.2867679344610367109, -0.3011811023622048000 ) ) ;
#49479 = CARTESIAN_POINT ( 'NONE',  ( -0.7152230971128602510, -0.2845877964562159024, 0.3641732283464567677 ) ) ;
#49480 = CARTESIAN_POINT ( 'NONE',  ( -1.030183727034119867, -0.08942795157528024563, -0.3641732283464568787 ) ) ;
#49481 = CARTESIAN_POINT ( 'NONE',  ( -1.430446194225720724, 0.05413385826771626580, -0.4176697321401330321 ) ) ;
#49482 = CARTESIAN_POINT ( 'NONE',  ( 0.4855643044619428750, 0.05413385826771666132, 0.4176697321401328100 ) ) ;
#49483 = CARTESIAN_POINT ( 'NONE',  ( -1.128608923884513837, 0.2306618581243847221, -0.2411417322834647770 ) ) ;
#49484 = CARTESIAN_POINT ( 'NONE',  ( -0.2867679344610364334, -0.2867679344610367109, -0.2086614173228345248 ) ) ;
#49485 = VERTEX_POINT ( 'NONE', #6384 ) ;
#49486 = CARTESIAN_POINT ( 'NONE',  ( 1.404199475065617264, -0.4281496062992124485, 0.4176697321401328655 ) ) ;
#49487 = CARTESIAN_POINT ( 'NONE',  ( -0.7749820319012115100, 0.000000000000000000, 0.3464511005275205946 ) ) ;
#49488 = CARTESIAN_POINT ( 'NONE',  ( -0.4091458600556405756, 0.2362204724409446288, -1.601049868766404094 ) ) ;
#49489 = CARTESIAN_POINT ( 'NONE',  ( 0.4724409448818898682, 2.892866454678787531E-17, -2.242125984251968518 ) ) ;
#49490 = EDGE_CURVE ( 'NONE', #46160, #54098, #56067, .T. ) ;
#49491 = CARTESIAN_POINT ( 'NONE',  ( 0.4091458600556403535, 0.2362204724409449896, -0.9186351706036745002 ) ) ;
#49492 = CARTESIAN_POINT ( 'NONE',  ( -0.7611548556430438595, -0.6046776061558809534, -0.2411417322834644161 ) ) ;
#49493 = CARTESIAN_POINT ( 'NONE',  ( 0.8333333333333340365, -0.6692913385826771977, 0.1292274648535927661 ) ) ;
#49495 = CARTESIAN_POINT ( 'NONE',  ( 0.000000000000000000, 2.165354330708661568, 0.000000000000000000 ) ) ;
#49494 = PLANE ( 'NONE',  #36874 ) ;
#49496 = CARTESIAN_POINT ( 'NONE',  ( 1.482939632545932307, -0.4281496062992124485, 0.4176697321401328655 ) ) ;
#49497 = CARTESIAN_POINT ( 'NONE',  ( -1.292650918635170010, -0.6692913385826771977, 0.1292274648535927661 ) ) ;
#49498 = CARTESIAN_POINT ( 'NONE',  ( -0.3917322834645670659, 0.1049643490035301607, -0.4278022065278722641 ) ) ;
#49499 = CARTESIAN_POINT ( 'NONE',  ( 0.09186351706036799403, -0.3690944881889765550, -0.3153832671262227771 ) ) ;
#49500 = CARTESIAN_POINT ( 'NONE',  ( 0.3917322834645669549, 0.1049643490035304660, -0.3667979002624672802 ) ) ;
#49501 = CARTESIAN_POINT ( 'NONE',  ( -0.1837270341207340729, 0.1283753931104746893, -0.1820866141732285504 ) ) ;
#49502 = CARTESIAN_POINT ( 'NONE',  ( 0.4527559055118117182, -0.4536011799217367080, 0.2665933059059888421 ) ) ;
#49503 = CARTESIAN_POINT ( 'NONE',  ( 0.5577427821522314977, -0.3162353388693409650, -0.4822834645669289433 ) ) ;
#49504 = CARTESIAN_POINT ( 'NONE',  ( -0.7480314960629914633, -0.5511811023622047445, 6.969142054262312111E-17 ) ) ;
#49505 = CARTESIAN_POINT ( 'NONE',  ( -0.3917322834645671215, 0.1049643490035301469, -2.229658792650918819 ) ) ;
#49506 = CARTESIAN_POINT ( 'NONE',  ( -1.509186351706035767, -0.4281496062992124485, 0.4176697321401328655 ) ) ;
#49507 = CARTESIAN_POINT ( 'NONE',  ( -1.069553805774277722, -0.6692913385826773087, -0.1292274648535924053 ) ) ;
#49508 = CARTESIAN_POINT ( 'NONE',  ( 0.4091458600556404646, -0.2362204724409448231, -0.6541994750656167090 ) ) ;
#49509 = CARTESIAN_POINT ( 'NONE',  ( -0.04593175853018302557, -0.6692913385826773087, -0.1292274648535924053 ) ) ;
#49510 = CARTESIAN_POINT ( 'NONE',  ( -0.6036745406824141069, -0.6046776061558809534, -0.2411417322834644161 ) ) ;
#49511 = CARTESIAN_POINT ( 'NONE',  ( 1.338582677165355062, -0.1870078740157479769, 0.3641732283464567677 ) ) ;
#49512 = CARTESIAN_POINT ( 'NONE',  ( 0.3215223097112867578, -0.08942795157527998196, 0.3641732283464567121 ) ) ;
#49513 = CARTESIAN_POINT ( 'NONE',  ( -0.2690288713910754526, 0.2952755905511810774, -0.1292274648535930714 ) ) ;
#49514 = CARTESIAN_POINT ( 'NONE',  ( -1.272965879265091305, 0.05413385826771626580, -0.4176697321401330321 ) ) ;
#49515 = CARTESIAN_POINT ( 'NONE',  ( 0.7773926554473647998, 8.471767977567108961E-16, -0.4445507791589058955 ) ) ;
#49516 = CARTESIAN_POINT ( 'NONE',  ( -0.5611900217179893735, -2.567464376874931580E-15, -0.4445507791589072832 ) ) ;
#49517 = CARTESIAN_POINT ( 'NONE',  ( 0.08530183727034192087, -0.05778040916215522460, 0.4822834645669289988 ) ) ;
#49518 = ORIENTED_EDGE ( 'NONE', *, *, #54812, .F. ) ;
#49519 = CARTESIAN_POINT ( 'NONE',  ( 0.3996062992125986035, -0.1070741851644052972, -1.920603674540682038 ) ) ;
#49520 = CARTESIAN_POINT ( 'NONE',  ( 1.181102362204724976, -0.1870078740157480879, -0.4822834645669291653 ) ) ;
#49521 = CARTESIAN_POINT ( 'NONE',  ( -0.6758530183727028406, -0.5511811023622048555, -0.09757992244046775898 ) ) ;
#49522 = CARTESIAN_POINT ( 'NONE',  ( -0.5446194225721777693, -0.3162353388693409650, -0.4822834645669289433 ) ) ;
#49523 = CARTESIAN_POINT ( 'NONE',  ( 1.272965879265092637, -0.4281496062992127816, -0.4176697321401328100 ) ) ;
#49524 = CARTESIAN_POINT ( 'NONE',  ( 1.069553805774278832, 0.2952755905511810774, -0.1292274648535930714 ) ) ;
#49525 = CARTESIAN_POINT ( 'NONE',  ( -1.640419947506561060, 0.05413385826771666132, 0.4176697321401328100 ) ) ;
#49526 = CARTESIAN_POINT ( 'NONE',  ( -1.227034120734907585, 0.1771653543307087630, 0.09757992244046791164 ) ) ;
#49527 = CARTESIAN_POINT ( 'NONE',  ( -0.3996062992125985480, -7.340648628747423112E-17, -0.4311023622047244208 ) ) ;
#49528 = CARTESIAN_POINT ( 'NONE',  ( -0.3996062992125986035, -7.340648628747425578E-17, -0.6692913385826770867 ) ) ;
#49529 = CARTESIAN_POINT ( 'NONE',  ( 0.1058382717557499880, 0.3949938075777411073, 0.006561679790026190250 ) ) ;
#49530 = CARTESIAN_POINT ( 'NONE',  ( 1.397637795275591177, 0.07958543189024071263, -0.2665933059059888421 ) ) ;
#49531 = CARTESIAN_POINT ( 'NONE',  ( 0.5446194225721792126, -0.08942795157528024563, -0.3641732283464568787 ) ) ;
#49532 = CARTESIAN_POINT ( 'NONE',  ( 0.7020997375328090762, -0.05778040916215560624, -0.4822834645669293319 ) ) ;
#49533 = CARTESIAN_POINT ( 'NONE',  ( 0.5314960629921396951, 2.755905511811024056, -3.937007874015760578 ) ) ;
#49534 = CARTESIAN_POINT ( 'NONE',  ( -0.2891555358219911054, 0.2891555358219909388, -0.8838582677165351953 ) ) ;
#49535 = CARTESIAN_POINT ( 'NONE',  ( 0.9251968503937015864, 0.07958543189024071263, -0.2665933059059888421 ) ) ;
#49536 = CARTESIAN_POINT ( 'NONE',  ( -0.1771653543307080136, 0.1660481256975883668, -0.3530559997133364547 ) ) ;
#49537 = CARTESIAN_POINT ( 'NONE',  ( -0.7283464566929126471, -0.5400638737290844871, 0.3530559997133364547 ) ) ;
#49538 = CARTESIAN_POINT ( 'NONE',  ( 1.122047244094488860, -0.5400638737290845981, -0.3530559997133363437 ) ) ;
#49539 = CARTESIAN_POINT ( 'NONE',  ( -0.4724409448818898682, -8.678599364036362592E-17, -1.299212598425196985 ) ) ;
#49540 = CARTESIAN_POINT ( 'NONE',  ( 0.1998031496062992740, 0.3460692066303959757, -2.349081364829396446 ) ) ;
#49541 = CARTESIAN_POINT ( 'NONE',  ( -0.2230971128608915943, -0.3690944881889765550, -0.3153832671262227771 ) ) ;
#49542 = ORIENTED_EDGE ( 'NONE', *, *, #20457, .F. ) ;
#49543 = CARTESIAN_POINT ( 'NONE',  ( 0.3917322834645670659, -0.1049643490035303273, -0.5807279771991620265 ) ) ;
#49544 = EDGE_LOOP ( 'NONE', ( #25449, #44446, #73081, #37827 ) ) ;
#49545 = CARTESIAN_POINT ( 'NONE',  ( -0.9580052493438311334, -0.4281496062992124485, 0.4176697321401328655 ) ) ;
#49546 = CARTESIAN_POINT ( 'NONE',  ( -0.2624671916010490880, -0.6046776061558807314, 0.2411417322834647770 ) ) ;
#49547 = CARTESIAN_POINT ( 'NONE',  ( -0.2034120734908128059, 0.2952755905511811885, 0.1292274648535926551 ) ) ;
#49548 = CARTESIAN_POINT ( 'NONE',  ( 0.5118110236220480003, -0.6692913385826771977, 8.415575281601705876E-17 ) ) ;
#49549 = CARTESIAN_POINT ( 'NONE',  ( -0.6364829396325453192, -0.05778040916215560624, -0.4822834645669293319 ) ) ;
#49550 = CARTESIAN_POINT ( 'NONE',  ( -1.456692913385826182, 0.2952755905511811885, 0.000000000000000000 ) ) ;
#49551 = CARTESIAN_POINT ( 'NONE',  ( -0.6496062992125976043, -0.5400638737290844871, 0.3530559997133364547 ) ) ;
#49552 = CARTESIAN_POINT ( 'NONE',  ( 0.7480314960629927956, -0.6692913385826771977, 8.415575281601705876E-17 ) ) ;
#49553 = ADVANCED_FACE ( 'NONE', ( #19010 ), #53336, .F. ) ;
#49554 = CARTESIAN_POINT ( 'NONE',  ( 0.3477690288713918276, 0.2952755905511811885, 0.1292274648535926551 ) ) ;
#49555 = EDGE_CURVE ( 'NONE', #11621, #15186, #42928, .T. ) ;
#49556 = CARTESIAN_POINT ( 'NONE',  ( -9.594673741351313045E-17, 0.3917322834645670104, -0.9370078740157480324 ) ) ;
#49557 = CARTESIAN_POINT ( 'NONE',  ( -0.2755905511811015396, -0.5511811023622047445, 6.969142054262312111E-17 ) ) ;
#49558 = ORIENTED_EDGE ( 'NONE', *, *, #82624, .T. ) ;
#49559 = CARTESIAN_POINT ( 'NONE',  ( 0.1058382717557500713, -0.3949938075777409408, -1.345144356955380704 ) ) ;
#49560 = ORIENTED_EDGE ( 'NONE', *, *, #33065, .F. ) ;
#49561 = CARTESIAN_POINT ( 'NONE',  ( -1.102362204724408601, -0.1870078740157479769, 0.3641732283464567677 ) ) ;
#49562 = CARTESIAN_POINT ( 'NONE',  ( -1.286089238845143479, 0.2306618581243847221, -0.2411417322834647770 ) ) ;
#49563 = CARTESIAN_POINT ( 'NONE',  ( -0.3477690288713902178, 0.2952755905511810774, -0.1292274648535930714 ) ) ;
#49564 = CARTESIAN_POINT ( 'NONE',  ( 0.3836918680457899744, 8.471767977567108961E-16, -0.4445507791589058955 ) ) ;
#49565 = CARTESIAN_POINT ( 'NONE',  ( -0.7020997375328076329, -0.3162353388693409650, -0.4822834645669289433 ) ) ;
#49566 = CARTESIAN_POINT ( 'NONE',  ( -0.7283464566929126471, 0.1660481256975883668, -0.3530559997133364547 ) ) ;
#49567 = DIRECTION ( 'NONE',  ( 0.000000000000000000, 0.000000000000000000, -1.000000000000000000 ) ) ;
#49568 = CARTESIAN_POINT ( 'NONE',  ( 1.017060367454068803, -0.2845877964562159024, 0.3641732283464567677 ) ) ;
#49569 = LINE ( 'NONE', #37766, #59251 ) ;
#49570 = CARTESIAN_POINT ( 'NONE',  ( 0.3917322834645670104, -0.1049643490035303411, 0.1187664041994749703 ) ) ;
#49571 = CARTESIAN_POINT ( 'NONE',  ( -0.01312335958005186876, -0.3690944881889763329, 0.3153832671262228327 ) ) ;
#49572 = CARTESIAN_POINT ( 'NONE',  ( -0.5643044619422565855, -0.4281496062992124485, 0.4176697321401328655 ) ) ;
#49573 = CARTESIAN_POINT ( 'NONE',  ( -0.7080320533160963103, 1.900312960331933976, -0.5309055118110235227 ) ) ;
#49574 = CARTESIAN_POINT ( 'NONE',  ( 0.04593175853018440641, -0.6692913385826771977, 0.1292274648535927661 ) ) ;
#49575 = ORIENTED_EDGE ( 'NONE', *, *, #77389, .F. ) ;
#49576 = CARTESIAN_POINT ( 'NONE',  ( 0.3460692066303959202, 0.1998031496062993295, -2.020997375328084100 ) ) ;
#49577 = CARTESIAN_POINT ( 'NONE',  ( -0.8001742991414044770, 0.004960608223778509643, -0.3437734562760191848 ) ) ;
#49578 = VERTEX_POINT ( 'NONE', #30728 ) ;
#49579 = CARTESIAN_POINT ( 'NONE',  ( -0.1998031496062991630, -0.3460692066303959202, -1.717191601049868677 ) ) ;
#49580 = DIRECTION ( 'NONE',  ( -1.000000000000000000, 0.000000000000000000, 0.000000000000000000 ) ) ;
#49581 = CARTESIAN_POINT ( 'NONE',  ( -0.8792650918635160906, -0.004921259842519870586, -0.3153832671262229437 ) ) ;
#49582 = CARTESIAN_POINT ( 'NONE',  ( -0.7677165354330699465, 0.1660481256975885056, 0.3530559997133364547 ) ) ;
#49583 = CARTESIAN_POINT ( 'NONE',  ( 0.4724409448818896462, 0.1265901696524990294, -0.2821522309711286258 ) ) ;
#49584 = DIRECTION ( 'NONE',  ( 1.000000000000000000, 3.083952846180989294E-16, 0.000000000000000000 ) ) ;
#49585 = EDGE_CURVE ( 'NONE', #70572, #10673, #51096, .T. ) ;
#49586 = CARTESIAN_POINT ( 'NONE',  ( -0.1049643490035302024, -0.3917322834645671215, -2.833989501312335957 ) ) ;
#49587 = CARTESIAN_POINT ( 'NONE',  ( 1.161417322834646493, -0.5400638737290844871, 0.3530559997133364547 ) ) ;
#49588 = CARTESIAN_POINT ( 'NONE',  ( 0.2755905511811031494, -0.6692913385826771977, 8.415575281601705876E-17 ) ) ;
#49589 = CARTESIAN_POINT ( 'NONE',  ( 0.4199475065616805614, 0.2306618581243848609, 0.2411417322834645549 ) ) ;
#49590 = CARTESIAN_POINT ( 'NONE',  ( -0.6758530183727028406, 0.1771653543307087630, 0.09757992244046791164 ) ) ;
#49591 = CARTESIAN_POINT ( 'NONE',  ( -0.5249343832020990641, -0.6046776061558809534, -0.2411417322834644161 ) ) ;
#49592 = CARTESIAN_POINT ( 'NONE',  ( -0.2362204724409451284, 0.4091458600556402425, -2.137139107611548905 ) ) ;
#49593 = ADVANCED_FACE ( 'NONE', ( #18518 ), #13037, .F. ) ;
#49594 = CARTESIAN_POINT ( 'NONE',  ( -0.7742782152230965886, 0.05413385826771666132, 0.4176697321401328100 ) ) ;
#49595 = CARTESIAN_POINT ( 'NONE',  ( 0.3420746716998660508, -0.1974969037888704149, -2.386482939632546429 ) ) ;
#49596 = CARTESIAN_POINT ( 'NONE',  ( 1.469816272965879911, 0.1283753931104746893, -0.1820866141732285504 ) ) ;
#49597 = CARTESIAN_POINT ( 'NONE',  ( -0.3805774278215216522, -0.3690944881889765550, -0.3153832671262227771 ) ) ;
#49598 = CARTESIAN_POINT ( 'NONE',  ( 0.9908136482939640111, -0.5511811023622046335, 0.09757992244046803654 ) ) ;
#49599 = CARTESIAN_POINT ( 'NONE',  ( -1.581364829396324945, -0.3162353388693405765, 0.4822834645669290543 ) ) ;
#49600 = CARTESIAN_POINT ( 'NONE',  ( -1.194225721784776262, -0.3690944881889763329, 0.3153832671262228327 ) ) ;
#49601 = CARTESIAN_POINT ( 'NONE',  ( -0.4724409448818898682, -8.678599364036362592E-17, -2.163385826771653697 ) ) ;
#49602 = CARTESIAN_POINT ( 'NONE',  ( 0.6102362204724416372, 0.07958543189024071263, -0.2665933059059888421 ) ) ;
#49603 = CARTESIAN_POINT ( 'NONE',  ( -0.3215223097112853146, -0.05778040916215560624, -0.4822834645669293319 ) ) ;
#49604 = CARTESIAN_POINT ( 'NONE',  ( 0.3049517105654749871, 8.471767977567108961E-16, -0.4445507791589058955 ) ) ;
#49605 = CARTESIAN_POINT ( 'NONE',  ( -0.2755905511811015396, -0.5511811023622047445, 6.969142054262312111E-17 ) ) ;
#49606 = CARTESIAN_POINT ( 'NONE',  ( 0.8923884514435703741, 0.2306618581243848609, 0.2411417322834645549 ) ) ;
#49607 = CARTESIAN_POINT ( 'NONE',  ( 1.813482582612293559, 2.755905511811024056, 0.5314960629921260393 ) ) ;
#49608 = CARTESIAN_POINT ( 'NONE',  ( 1.174540682414699111, -0.08942795157528024563, -0.3641732283464568787 ) ) ;
#49609 = CARTESIAN_POINT ( 'NONE',  ( -0.8202099737532801971, -0.6692913385826771977, 0.1292274648535927661 ) ) ;
#49610 = CARTESIAN_POINT ( 'NONE',  ( -0.3412073490813641308, 0.1283753931104746893, -0.1820866141732285504 ) ) ;
#49611 = CARTESIAN_POINT ( 'NONE',  ( 1.035118193396260766, 4.339766966676338660E-16, 0.3791483426435169335 ) ) ;
#49612 = CARTESIAN_POINT ( 'NONE',  ( 0.2493438320209980519, -0.3690944881889765550, -0.3153832671262227771 ) ) ;
#49613 = ADVANCED_FACE ( 'NONE', ( #38690 ), #82494, .T. ) ;
#49614 = CARTESIAN_POINT ( 'NONE',  ( -0.6233595800524928121, -0.3162353388693409650, -0.4822834645669289433 ) ) ;
#49615 = CARTESIAN_POINT ( 'NONE',  ( -9.787531504996566615E-17, 0.3996062992125985480, -0.5492125984251968740 ) ) ;
#49616 = CARTESIAN_POINT ( 'NONE',  ( 0.1958661417322836440, -0.3392501089628017219, -2.223753280839895208 ) ) ;
#49617 = CARTESIAN_POINT ( 'NONE',  ( 0.5380577427821529035, -0.004921259842519870586, -0.3153832671262229437 ) ) ;
#49618 = CARTESIAN_POINT ( 'NONE',  ( -0.3674540682414689785, 0.2306618581243848609, 0.2411417322834645549 ) ) ;
#49619 = CARTESIAN_POINT ( 'NONE',  ( -0.8923884514435688198, -0.6046776061558807314, 0.2411417322834647770 ) ) ;
#49620 = CARTESIAN_POINT ( 'NONE',  ( -0.6167979002624665030, -0.3690944881889765550, -0.3153832671262227771 ) ) ;
#49621 = LINE ( 'NONE', #37820, #34707 ) ;
#49622 = CARTESIAN_POINT ( 'NONE',  ( -0.03937007874015669567, 0.2952755905511811885, 0.000000000000000000 ) ) ;
#49623 = AXIS2_PLACEMENT_3D ( 'NONE', #67000, #43243, #60668 ) ;
#49624 = CARTESIAN_POINT ( 'NONE',  ( -1.069553805774277722, 0.1771653543307087630, 0.09757992244046791164 ) ) ;
#49625 = CARTESIAN_POINT ( 'NONE',  ( -1.384514435695537005, -0.6692913385826773087, -0.1292274648535924053 ) ) ;
#49626 = CARTESIAN_POINT ( 'NONE',  ( -0.1265901696524993347, 0.4724409448818896462, -2.603018372703412187 ) ) ;
#49627 = VERTEX_POINT ( 'NONE', #64368 ) ;
#49628 = CARTESIAN_POINT ( 'NONE',  ( -1.620734908136482577, -0.5511811023622048555, -0.09757992244046775898 ) ) ;
#49629 = CARTESIAN_POINT ( 'NONE',  ( -1.384514435695537005, 0.2952755905511811885, 0.1292274648535926551 ) ) ;
#49630 = CARTESIAN_POINT ( 'NONE',  ( -1.056430446194224881, 0.2952755905511810774, -0.1292274648535930714 ) ) ;
#49631 = EDGE_CURVE ( 'NONE', #60937, #52641, #69853, .T. ) ;
#49632 = CARTESIAN_POINT ( 'NONE',  ( 1.587926509186352142, 0.05413385826771666132, 0.4176697321401328100 ) ) ;
#49633 = CARTESIAN_POINT ( 'NONE',  ( -0.3917322834645669549, -0.1049643490035306603, -1.547900262467191590 ) ) ;
#49634 = CARTESIAN_POINT ( 'NONE',  ( 0.1002886991238245706, 0.3788256970788722588, -1.220472440944881054 ) ) ;
#49635 = CARTESIAN_POINT ( 'NONE',  ( 1.082677165354331228, 0.1660481256975883668, -0.3530559997133364547 ) ) ;
#49636 = CARTESIAN_POINT ( 'NONE',  ( 0.2821522309711292364, 0.2952755905511810774, -0.1292274648535930714 ) ) ;
#49637 = CARTESIAN_POINT ( 'NONE',  ( 0.2362204724409449064, 0.4091458600556404646, -0.4593175853018372501 ) ) ;
#49638 = CARTESIAN_POINT ( 'NONE',  ( -0.3996062992125984925, -0.1070741851644056719, -2.327427821522309870 ) ) ;
#49639 = CARTESIAN_POINT ( 'NONE',  ( 1.174540682414699111, -0.08942795157528024563, -0.3641732283464568787 ) ) ;
#49640 = B_SPLINE_CURVE_WITH_KNOTS ( 'NONE', 3,
 ( #16142, #22854, #36714, #23673, #9402, #68715, #41789 ),
 .UNSPECIFIED., .F., .F.,
 ( 4, 3, 4 ),
 ( 1.232595164407830946E-32, 0.001246232571205264407, 0.002492492258783314020 ),
 .UNSPECIFIED. ) ;
#49641 = CARTESIAN_POINT ( 'NONE',  ( -0.1998031496062991907, -0.3460692066303959757, -1.010498687664042050 ) ) ;
#49642 = VERTEX_POINT ( 'NONE', #12204 ) ;
#49643 = CARTESIAN_POINT ( 'NONE',  ( -0.8530183727034112984, -0.004921259842519576551, 0.3153832671262227771 ) ) ;
#49644 = CARTESIAN_POINT ( 'NONE',  ( -0.1958661417322834220, -0.3392501089628018884, -2.734908136482939511 ) ) ;
#49645 = ORIENTED_EDGE ( 'NONE', *, *, #51403, .F. ) ;
#49646 = CARTESIAN_POINT ( 'NONE',  ( 0.4527559055118117182, -0.5400638737290844871, 0.3530559997133364547 ) ) ;
#49647 = CARTESIAN_POINT ( 'NONE',  ( -0.2230971128608915943, -0.4281496062992127816, -0.4176697321401328100 ) ) ;
#49648 = CARTESIAN_POINT ( 'NONE',  ( -1.286089238845143479, 0.2306618581243847221, -0.2411417322834647770 ) ) ;
#49649 = CARTESIAN_POINT ( 'NONE',  ( 1.108923884514436686, -0.3162353388693409650, -0.4822834645669289433 ) ) ;
#49650 = CARTESIAN_POINT ( 'NONE',  ( 1.692913385826772421, 0.2952755905511811885, 0.000000000000000000 ) ) ;
#49651 = CARTESIAN_POINT ( 'NONE',  ( 0.000000000000000000, 0.000000000000000000, -2.755905511811024056 ) ) ;
#49652 = CARTESIAN_POINT ( 'NONE',  ( -0.08530183727034056085, -0.3162353388693405765, 0.4822834645669290543 ) ) ;
#49653 = CARTESIAN_POINT ( 'NONE',  ( -1.266404199475064773, -0.05778040916215560624, -0.4822834645669293319 ) ) ;
#49654 = CARTESIAN_POINT ( 'NONE',  ( -0.3917322834645669549, -7.196005306013483243E-17, -2.009167035924197098 ) ) ;
#49655 = CARTESIAN_POINT ( 'NONE',  ( -1.016821367227983552, 1.537401574803149984, -0.4744094488188975722 ) ) ;
#49656 = CARTESIAN_POINT ( 'NONE',  ( 1.450131233595801428, -0.6692913385826773087, -0.1292274648535924053 ) ) ;
#49657 = ADVANCED_FACE ( 'NONE', ( #26059 ), #77845, .F. ) ;
#49658 = CARTESIAN_POINT ( 'NONE',  ( -0.3917322834645670104, -7.196005306013484475E-17, -2.801181102362204633 ) ) ;
#49659 = CARTESIAN_POINT ( 'NONE',  ( 0.7349081364829403995, 0.1283753931104748280, 0.1820866141732283561 ) ) ;
#49660 = ORIENTED_EDGE ( 'NONE', *, *, #45936, .F. ) ;
#49661 = CARTESIAN_POINT ( 'NONE',  ( -9.674558042662121740E-17, 0.3949938075777409963, -5.756223643949423463E-17 ) ) ;
#49662 = CARTESIAN_POINT ( 'NONE',  ( -0.6889763779527552368, 0.1660481256975885056, 0.3530559997133364547 ) ) ;
#49663 = EDGE_LOOP ( 'NONE', ( #47311, #56690, #54196, #11263, #81264 ) ) ;
#49664 = CARTESIAN_POINT ( 'NONE',  ( -0.1181102362204717315, 0.1771653543307087630, 0.000000000000000000 ) ) ;
#49665 = CARTESIAN_POINT ( 'NONE',  ( -1.555118110236219930, 0.1660481256975885056, 0.3530559997133364547 ) ) ;
#49666 = CARTESIAN_POINT ( 'NONE',  ( 0.3543307086614179147, 0.2952755905511811885, 0.000000000000000000 ) ) ;
#49667 = CARTESIAN_POINT ( 'NONE',  ( 0.3477690288713918276, 0.2952755905511811885, 0.1292274648535926551 ) ) ;
#49668 = CARTESIAN_POINT ( 'NONE',  ( -0.5183727034120726440, -0.6692913385826773087, -0.1292274648535924053 ) ) ;
#49669 = CARTESIAN_POINT ( 'NONE',  ( -0.1049643490035307158, 0.3917322834645670104, -1.105662360401261868 ) ) ;
#49670 = CARTESIAN_POINT ( 'NONE',  ( -0.9251968503937002541, -0.5400638737290845981, -0.3530559997133363437 ) ) ;
#49671 = CARTESIAN_POINT ( 'NONE',  ( -0.1958661417322834220, -0.3392501089628018884, -2.512467191601049699 ) ) ;
#49672 = CARTESIAN_POINT ( 'NONE',  ( 1.272965879265092637, -0.004921259842519576551, 0.3153832671262227771 ) ) ;
#49673 = CARTESIAN_POINT ( 'NONE',  ( -1.161417322834644716, 0.1660481256975885056, 0.3530559997133364547 ) ) ;
#49674 = CARTESIAN_POINT ( 'NONE',  ( 0.7414698162729663755, 0.2952755905511811885, 0.1292274648535926551 ) ) ;
#49675 = CARTESIAN_POINT ( 'NONE',  ( 1.371391076115485941, 0.2952755905511811885, 0.1292274648535926551 ) ) ;
#49676 = CARTESIAN_POINT ( 'NONE',  ( -0.3996062992125986035, -0.1070741851644056997, -0.6758530183727035068 ) ) ;
#49677 = CARTESIAN_POINT ( 'NONE',  ( -1.194225721784776262, 0.05413385826771626580, -0.4176697321401330321 ) ) ;
#49678 = CARTESIAN_POINT ( 'NONE',  ( 0.1070741851644054776, -0.3996062992125984925, -0.3195538057742782212 ) ) ;
#49679 = CARTESIAN_POINT ( 'NONE',  ( 0.4790026246719167324, -0.05778040916215522460, 0.4822834645669289988 ) ) ;
#49680 = CARTESIAN_POINT ( 'NONE',  ( -0.1998031496062991907, -0.3460692066303959757, -2.270341207349081181 ) ) ;
#49681 = CARTESIAN_POINT ( 'NONE',  ( -1.522309711286088607, -0.5023911411419708095, 0.1820866141732285504 ) ) ;
#49682 = CARTESIAN_POINT ( 'NONE',  ( 0.6692913385826778638, -0.5511811023622047445, 6.969142054262312111E-17 ) ) ;
#49683 = CARTESIAN_POINT ( 'NONE',  ( 1.102362204724410155, -0.1870078740157479769, 0.4822834645669291653 ) ) ;
#49684 = CARTESIAN_POINT ( 'NONE',  ( -0.4091458600556405756, 0.2362204724409446288, -0.8904199475065617264 ) ) ;
#49685 = CARTESIAN_POINT ( 'NONE',  ( 0.6430446194225729606, -0.3690944881889765550, -0.3153832671262227771 ) ) ;
#49686 = CARTESIAN_POINT ( 'NONE',  ( 0.4724409448818904789, -0.1870078740157479769, 0.4822834645669291653 ) ) ;
#49687 = CARTESIAN_POINT ( 'NONE',  ( 0.3949938075777408852, 0.1058382717557500435, -0.8313648293963256108 ) ) ;
#49688 = CARTESIAN_POINT ( 'NONE',  ( -0.9120734908136475250, 0.2952755905511811885, 0.1292274648535926551 ) ) ;
#49689 = CARTESIAN_POINT ( 'NONE',  ( -0.1674892343164145203, -2.567464376874931580E-15, -0.4445507791589072832 ) ) ;
#49690 = CARTESIAN_POINT ( 'NONE',  ( 0.9448818897637802916, -0.1870078740157479769, 0.3641732283464567677 ) ) ;
#49691 = CARTESIAN_POINT ( 'NONE',  ( 0.1771653543307093182, 0.1660481256975885056, 0.3530559997133364547 ) ) ;
#49692 = CARTESIAN_POINT ( 'NONE',  ( 0.4744094488189011805, 1.553651517367183210, -1.016821367227981776 ) ) ;
#49693 = CARTESIAN_POINT ( 'NONE',  ( -0.5118110236220466680, -0.6692913385826771977, 8.415575281601705876E-17 ) ) ;
#49694 = CARTESIAN_POINT ( 'NONE',  ( 0.3149606299212606708, -0.1870078740157480601, -0.3641732283464567677 ) ) ;
#49695 = CARTESIAN_POINT ( 'NONE',  ( -2.666390022512505453, 1.301092492065836659, -0.4123476441529835279 ) ) ;
#49696 = CARTESIAN_POINT ( 'NONE',  ( -0.04593175853018302557, 0.1771653543307087630, 0.09757992244046791164 ) ) ;
#49697 = CARTESIAN_POINT ( 'NONE',  ( 0.6364829396325465405, -0.08942795157527998196, 0.3641732283464567121 ) ) ;
#49698 = CYLINDRICAL_SURFACE ( 'NONE', #35786, 0.4744094488188972947 ) ;
#49699 = CARTESIAN_POINT ( 'NONE',  ( 0.1998031496062992463, 0.3460692066303959202, -1.795931758530183719 ) ) ;
#49700 = CARTESIAN_POINT ( 'NONE',  ( 0.1377952755905518800, 0.1660481256975883668, -0.3530559997133364547 ) ) ;
#49701 = CARTESIAN_POINT ( 'NONE',  ( 0.3917322834645670104, 2.398668435337828261E-17, -1.527559055118110409 ) ) ;
#49702 = CARTESIAN_POINT ( 'NONE',  ( 1.266404199475066328, -0.2845877964562161244, -0.3641732283464567121 ) ) ;
#49703 = CARTESIAN_POINT ( 'NONE',  ( 0.000000000000000000, 2.755905511811024056, 0.000000000000000000 ) ) ;
#49704 = CARTESIAN_POINT ( 'NONE',  ( -0.3018372703412066094, -0.004921259842519576551, 0.3153832671262227771 ) ) ;
#49705 = EDGE_CURVE ( 'NONE', #51988, #5969, #25223, .T. ) ;
#49706 = CARTESIAN_POINT ( 'NONE',  ( -0.2099737532808391705, -0.5023911411419708095, -0.1820866141732282451 ) ) ;
#49707 = CARTESIAN_POINT ( 'NONE',  ( -0.3740157480314953431, 0.1660481256975885056, 0.3530559997133364547 ) ) ;
#49708 = CARTESIAN_POINT ( 'NONE',  ( 0.7742782152230979209, -0.004921259842519870586, -0.3153832671262229437 ) ) ;
#49709 = CARTESIAN_POINT ( 'NONE',  ( -0.2945438235763074841, 0.02380624310431164042, 5.877921531841205471 ) ) ;
#49710 = CARTESIAN_POINT ( 'NONE',  ( 1.587926509186352142, -0.004921259842519576551, 0.3153832671262227771 ) ) ;
#49711 = EDGE_CURVE ( 'NONE', #78367, #5025, #26487, .T. ) ;
#49712 = CARTESIAN_POINT ( 'NONE',  ( 0.09842519685039434474, 0.1660481256975885056, 0.3530559997133364547 ) ) ;
#49713 = CARTESIAN_POINT ( 'NONE',  ( 1.174540682414699111, -0.3162353388693405765, 0.4822834645669290543 ) ) ;
#49714 = CARTESIAN_POINT ( 'NONE',  ( -1.595398199321655275, 1.839868176060737381, -0.1559797534342491077 ) ) ;
#49715 = CARTESIAN_POINT ( 'NONE',  ( 0.2427821522309716595, -0.3162353388693409650, -0.4822834645669289433 ) ) ;
#49716 = CARTESIAN_POINT ( 'NONE',  ( 0.2867679344610365999, -0.2867679344610365444, -1.127952755905512028 ) ) ;
#49717 = CARTESIAN_POINT ( 'NONE',  ( 0.7152230971128616943, -0.05778040916215522460, 0.4822834645669289988 ) ) ;
#49718 = CARTESIAN_POINT ( 'NONE',  ( 0.6233595800524942554, -0.05778040916215560624, -0.4822834645669293319 ) ) ;
#49719 = CARTESIAN_POINT ( 'NONE',  ( -0.5314960629921294810, 2.559055118110236560, 0.9881811337016624952 ) ) ;
#49720 = CARTESIAN_POINT ( 'NONE',  ( 0.6758530183727039509, -0.5511811023622046335, 0.09757992244046803654 ) ) ;
#49721 = CARTESIAN_POINT ( 'NONE',  ( 1.049868766404200349, 0.2306618581243848609, 0.2411417322834645549 ) ) ;
#49722 = CARTESIAN_POINT ( 'NONE',  ( 0.1509186351706042484, -0.2845877964562159024, 0.3641732283464567677 ) ) ;
#49723 = CARTESIAN_POINT ( 'NONE',  ( -0.4199475065616791736, -0.6046776061558807314, 0.2411417322834647770 ) ) ;
#49724 = CARTESIAN_POINT ( 'NONE',  ( 0.1443569553805781891, -0.4281496062992124485, 0.4176697321401328655 ) ) ;
#49725 = CARTESIAN_POINT ( 'NONE',  ( -0.7152230971128602510, -0.3162353388693405765, 0.4822834645669290543 ) ) ;
#49726 = CARTESIAN_POINT ( 'NONE',  ( -0.2952755905511804668, 0.07958543189024085140, 0.2665933059059887866 ) ) ;
#49727 = CARTESIAN_POINT ( 'NONE',  ( 0.8333333333333340365, 0.2952755905511810774, -0.1292274648535930714 ) ) ;
#49728 = CARTESIAN_POINT ( 'NONE',  ( 1.148293963254593875, -0.5511811023622046335, 0.09757992244046803654 ) ) ;
#49729 = CARTESIAN_POINT ( 'NONE',  ( -0.01968503937007793844, 0.1660481256975883668, -0.3530559997133364547 ) ) ;
#49730 = CARTESIAN_POINT ( 'NONE',  ( -0.4091458600556402980, -0.2362204724409451284, -0.5249343832020997302 ) ) ;
#49732 = CARTESIAN_POINT ( 'NONE',  ( 0.1070741851644054915, -0.3996062992125985480, -1.187664041994750619 ) ) ;
#49731 = CARTESIAN_POINT ( 'NONE',  ( -3.937007874015748143, 2.559055118110236560, -0.5314960629921260393 ) ) ;
#49733 = FACE_OUTER_BOUND ( 'NONE', #2996, .T. ) ;
#49734 = FACE_OUTER_BOUND ( 'NONE', #13852, .T. ) ;
#49735 = CARTESIAN_POINT ( 'NONE',  ( -1.049868766404198794, -0.6046776061558807314, 0.2411417322834647770 ) ) ;
#49736 = CARTESIAN_POINT ( 'NONE',  ( -1.056430446194224881, 0.2952755905511810774, -0.1292274648535930714 ) ) ;
#49737 = CARTESIAN_POINT ( 'NONE',  ( -0.4724409448818898682, -8.678599364036362592E-17, -0.1968503937007874127 ) ) ;
#49738 = CARTESIAN_POINT ( 'NONE',  ( 0.1974969037888706369, -0.3420746716998659953, -2.611548556430445700 ) ) ;
#49739 = ORIENTED_EDGE ( 'NONE', *, *, #70319, .F. ) ;
#49740 = CARTESIAN_POINT ( 'NONE',  ( 0.4724409448818904789, -0.1870078740157480601, -0.3641732283464567677 ) ) ;
#49741 = CARTESIAN_POINT ( 'NONE',  ( -9.594673741351313045E-17, 0.3917322834645670104, -1.409448818897637734 ) ) ;
#49742 = CARTESIAN_POINT ( 'NONE',  ( 0.5052493438320215802, 0.2952755905511811885, 0.1292274648535926551 ) ) ;
#49743 = CARTESIAN_POINT ( 'NONE',  ( -0.4724409448818899238, 0.1265901696524986686, -2.395013123359580387 ) ) ;
#49744 = CARTESIAN_POINT ( 'NONE',  ( -0.4724409448818899238, 0.1265901696524986964, -0.8969816272965878134 ) ) ;
#49745 = CARTESIAN_POINT ( 'NONE',  ( -0.3049517105654738214, -2.191421614605370878E-15, 0.4445507791589071167 ) ) ;
#49746 = CARTESIAN_POINT ( 'NONE',  ( 0.9973753280839902091, -0.6046776061558807314, 0.2411417322834647770 ) ) ;
#49747 = CARTESIAN_POINT ( 'NONE',  ( 1.351706036745407458, -0.3690944881889765550, -0.3153832671262227771 ) ) ;
#49748 = CARTESIAN_POINT ( 'NONE',  ( -0.03937007874015669567, 0.2952755905511811885, 0.000000000000000000 ) ) ;
#49749 = B_SPLINE_CURVE_WITH_KNOTS ( 'NONE', 3,
 ( #25504, #17571, #11252, #62586, #4928, #36910, #43204, #30596, #50764, #18394 ),
 .UNSPECIFIED., .F., .F.,
 ( 4, 2, 2, 2, 4 ),
 ( 0.000000000000000000, 0.0007778963758021317440, 0.001555792751604263488, 0.002333689127406395232, 0.003111585503208526976 ),
 .UNSPECIFIED. ) ;
#49750 = CARTESIAN_POINT ( 'NONE',  ( -0.3917322834645668994, -0.1049643490035306742, -0.5984058810685547458 ) ) ;
#49751 = CARTESIAN_POINT ( 'NONE',  ( -0.5380577427821514602, 0.05413385826771666132, 0.4176697321401328100 ) ) ;
#49752 = CARTESIAN_POINT ( 'NONE',  ( -0.7283464566929126471, 0.07958543189024071263, -0.2665933059059888421 ) ) ;
#49753 = CARTESIAN_POINT ( 'NONE',  ( 0.3346456692913390985, 0.1660481256975885056, 0.3530559997133364547 ) ) ;
#49754 = CARTESIAN_POINT ( 'NONE',  ( -0.4199475065616791736, 0.2306618581243847221, -0.2411417322834647770 ) ) ;
#49755 = CARTESIAN_POINT ( 'NONE',  ( 1.660104986876641320, -0.05778040916215522460, 0.4822834645669289988 ) ) ;
#49756 = CARTESIAN_POINT ( 'NONE',  ( 0.09115970038225353067, 3.421639014772782816E-16, 0.3464511005275203726 ) ) ;
#49757 = ORIENTED_EDGE ( 'NONE', *, *, #49168, .T. ) ;
#49758 = CARTESIAN_POINT ( 'NONE',  ( 0.3917322834645670104, 0.1049643490035304660, -2.011174171424884083 ) ) ;
#49759 = CARTESIAN_POINT ( 'NONE',  ( 0.2099737532808405305, -0.6046776061558807314, 0.2411417322834647770 ) ) ;
#49760 = CARTESIAN_POINT ( 'NONE',  ( -0.3805774278215216522, -0.4281496062992127816, -0.4176697321401328100 ) ) ;
#49761 = CARTESIAN_POINT ( 'NONE',  ( -1.601049868766403650, 0.2306618581243847221, -0.2411417322834647770 ) ) ;
#49762 = CARTESIAN_POINT ( 'NONE',  ( 0.8333333333333340365, 0.2952755905511810774, -0.1292274648535930714 ) ) ;
#49763 = CARTESIAN_POINT ( 'NONE',  ( 0.4855643044619430415, -0.4281496062992127816, -0.4176697321401328100 ) ) ;
#49764 = CARTESIAN_POINT ( 'NONE',  ( -0.1958661417322834220, -0.3392501089628018884, -1.567585301837270295 ) ) ;
#49765 = CARTESIAN_POINT ( 'NONE',  ( -0.6167979002624665030, 0.05413385826771666132, 0.4176697321401328100 ) ) ;
#49766 = CARTESIAN_POINT ( 'NONE',  ( 0.2099737532808405305, -0.6046776061558807314, 0.2411417322834647770 ) ) ;
#49767 = CARTESIAN_POINT ( 'NONE',  ( -0.2887139107611542133, -0.6046776061558809534, -0.2411417322834644161 ) ) ;
#49768 = CARTESIAN_POINT ( 'NONE',  ( 0.2099737532808405305, -0.5023911411419708095, 0.1820866141732285504 ) ) ;
#49769 = CARTESIAN_POINT ( 'NONE',  ( -1.561679790026246017, 0.05413385826771666132, 0.4176697321401328100 ) ) ;
#49770 = CARTESIAN_POINT ( 'NONE',  ( -0.2813683484248658551, -0.08970734455876072655, 5.854851642268653400 ) ) ;
#49771 = CARTESIAN_POINT ( 'NONE',  ( -0.2296587926509179312, -0.3162353388693409650, -0.4822834645669289433 ) ) ;
#49772 = CYLINDRICAL_SURFACE ( 'NONE', #76221, 1.181102362204724310 ) ;
#49773 = CARTESIAN_POINT ( 'NONE',  ( 1.614173228346457378, 0.2952755905511811885, 0.000000000000000000 ) ) ;
#49774 = CARTESIAN_POINT ( 'NONE',  ( 0.1958661417322836440, -0.3392501089628017219, -2.603674540682414218 ) ) ;
#49775 = ORIENTED_EDGE ( 'NONE', *, *, #78723, .T. ) ;
#49776 = VERTEX_POINT ( 'NONE', #44985 ) ;
#49777 = CARTESIAN_POINT ( 'NONE',  ( 0.7545931758530189937, 0.2952755905511810774, -0.1292274648535930714 ) ) ;
#49778 = CARTESIAN_POINT ( 'NONE',  ( 0.2034120734908142214, 0.1771653543307087075, -0.09757992244046823083 ) ) ;
#49780 = PLANE ( 'NONE',  #34427 ) ;
#49779 = CARTESIAN_POINT ( 'NONE',  ( 1.141392835773559211, 0.3937007874015748254, 1.141392835773562764 ) ) ;
#49781 = CARTESIAN_POINT ( 'NONE',  ( -0.3917322834645670104, -7.196005306013484475E-17, -0.9114173228346457156 ) ) ;
#49782 = CARTESIAN_POINT ( 'NONE',  ( -1.157146581871515012E-16, 0.4724409448818898682, 0.2381889763779527491 ) ) ;
#49783 = CARTESIAN_POINT ( 'NONE',  ( 0.3038629456265435902, -3.790565315793794774E-16, -0.3954974714151277548 ) ) ;
#49784 = CARTESIAN_POINT ( 'NONE',  ( -0.2891555358219909388, -0.2891555358219912164, 0.1791338582677165503 ) ) ;
#49785 = CARTESIAN_POINT ( 'NONE',  ( 0.3149606299212603933, -0.1870078740157479769, 0.4822834645669291653 ) ) ;
#49786 = CARTESIAN_POINT ( 'NONE',  ( -1.259842519685038686, -0.1870078740157480879, -0.4822834645669291653 ) ) ;
#49787 = CARTESIAN_POINT ( 'NONE',  ( -1.181102362204723644, -0.1870078740157480879, -0.4822834645669291653 ) ) ;
#49788 = CARTESIAN_POINT ( 'NONE',  ( 0.7152230971128614723, -0.3162353388693409650, -0.4822834645669289433 ) ) ;
#49789 = CARTESIAN_POINT ( 'NONE',  ( 0.7742782152230978099, -0.4281496062992124485, 0.4176697321401328655 ) ) ;
#49790 = CARTESIAN_POINT ( 'NONE',  ( 1.430446194225722500, -0.3690944881889765550, -0.3153832671262227771 ) ) ;
#49791 = CARTESIAN_POINT ( 'NONE',  ( 1.049868766404200349, 0.1283753931104748280, 0.1820866141732283561 ) ) ;
#49792 = CARTESIAN_POINT ( 'NONE',  ( -0.9711286089238838626, 0.2306618581243847221, -0.2411417322834647770 ) ) ;
#49793 = CARTESIAN_POINT ( 'NONE',  ( -0.1070741851644051862, -0.3996062992125986590, -0.6213910761154856077 ) ) ;
#49794 = CARTESIAN_POINT ( 'NONE',  ( 1.620734908136483465, -0.6692913385826771977, 0.1292274648535927661 ) ) ;
#49795 = CARTESIAN_POINT ( 'NONE',  ( -0.3917322834645671215, 0.1049643490035301469, -0.3398950131233596239 ) ) ;
#49796 = CARTESIAN_POINT ( 'NONE',  ( -0.3346456692913377662, 0.1660481256975883668, -0.3530559997133364547 ) ) ;
#49798 = CARTESIAN_POINT ( 'NONE',  ( -3.911375737184146661, 1.694783778358343707, -0.4487029277117119963 ) ) ;
#49797 = CARTESIAN_POINT ( 'NONE',  ( 1.154855643044620184, -0.6046776061558807314, 0.2411417322834647770 ) ) ;
#49799 = DIRECTION ( 'NONE',  ( -0.000000000000000000, -0.000000000000000000, -1.000000000000000000 ) ) ;
#49800 = CARTESIAN_POINT ( 'NONE',  ( 0.3018372703412079971, 0.05413385826771626580, -0.4176697321401330321 ) ) ;
#49801 = CARTESIAN_POINT ( 'NONE',  ( 1.036745406824147508, -0.3690944881889765550, -0.3153832671262227771 ) ) ;
#49802 = EDGE_CURVE ( 'NONE', #10785, #64866, #1818, .T. ) ;
#49803 = CARTESIAN_POINT ( 'NONE',  ( -0.2867679344610366554, 0.2867679344610365444, -1.832001681593488751 ) ) ;
#49804 = CARTESIAN_POINT ( 'NONE',  ( -1.207349081364828880, 0.1283753931104746893, -0.1820866141732285504 ) ) ;
#49805 = CARTESIAN_POINT ( 'NONE',  ( 1.017060367454068803, -0.3162353388693405765, 0.4822834645669290543 ) ) ;
#49806 = FACE_OUTER_BOUND ( 'NONE', #9096, .T. ) ;
#49807 = CARTESIAN_POINT ( 'NONE',  ( -0.4265091863517051496, 0.1771653543307087075, -0.09757992244046823083 ) ) ;
#49808 = CARTESIAN_POINT ( 'NONE',  ( -0.5380577427821514602, -0.4281496062992127816, -0.4176697321401328100 ) ) ;
#49809 = CARTESIAN_POINT ( 'NONE',  ( 1.502624671916010790, -0.05778040916215522460, 0.4822834645669289988 ) ) ;
#49810 = CARTESIAN_POINT ( 'NONE',  ( -0.7480314960629914633, 0.2952755905511811885, 0.000000000000000000 ) ) ;
#49811 = AXIS2_PLACEMENT_3D ( 'NONE', #20500, #13774, #71849 ) ;
#49812 = CARTESIAN_POINT ( 'NONE',  ( 1.469816272965879911, -0.6046776061558807314, 0.2411417322834647770 ) ) ;
#49813 = CARTESIAN_POINT ( 'NONE',  ( -0.3917322834645670659, -7.196005306013484475E-17, -0.8235101294301331309 ) ) ;
#49814 = CARTESIAN_POINT ( 'NONE',  ( -0.8202099737532799750, 0.1771653543307087075, -0.09757992244046823083 ) ) ;
#49815 = CARTESIAN_POINT ( 'NONE',  ( 2.575297182719591849, 1.629972608277045820, 0.4653577321740525186 ) ) ;
#49816 = CARTESIAN_POINT ( 'NONE',  ( 1.318897637795276356, 0.1660481256975883668, -0.3530559997133364547 ) ) ;
#49817 = CARTESIAN_POINT ( 'NONE',  ( -0.3458507752293909498, 0.3458507752293907833, -1.986220472440944906 ) ) ;
#49818 = CARTESIAN_POINT ( 'NONE',  ( -1.272965879265091305, -0.4281496062992124485, 0.4176697321401328655 ) ) ;
#49819 = CARTESIAN_POINT ( 'NONE',  ( -1.646981627296586703, -0.08942795157527998196, 0.3641732283464567121 ) ) ;
#49820 = CARTESIAN_POINT ( 'NONE',  ( -0.5118110236220466680, -0.5511811023622047445, 6.969142054262312111E-17 ) ) ;
#49821 = CARTESIAN_POINT ( 'NONE',  ( -1.620734908136482577, 0.2952755905511811885, 0.1292274648535926551 ) ) ;
#49822 = CARTESIAN_POINT ( 'NONE',  ( -0.2099737532808391705, 0.2306618581243848609, 0.2411417322834645549 ) ) ;
#49823 = CARTESIAN_POINT ( 'NONE',  ( 0.09842519685039434474, 0.07958543189024085140, 0.2665933059059887866 ) ) ;
#49824 = CARTESIAN_POINT ( 'NONE',  ( -1.036745406824146176, -0.004921259842519870586, -0.3153832671262229437 ) ) ;
#49825 = CARTESIAN_POINT ( 'NONE',  ( 1.233595800524935227, -0.5023911411419708095, 0.1820866141732285504 ) ) ;
#49826 = CARTESIAN_POINT ( 'NONE',  ( 0.9842519685039378130, -0.6692913385826771977, 8.415575281601705876E-17 ) ) ;
#49827 = DIRECTION ( 'NONE',  ( 0.000000000000000000, -0.000000000000000000, 1.000000000000000000 ) ) ;
#49828 = CARTESIAN_POINT ( 'NONE',  ( 0.4133858267716541968, 0.07958543189024085140, 0.2665933059059887866 ) ) ;
#49829 = CARTESIAN_POINT ( 'NONE',  ( 0.2887139107611556010, 0.2306618581243847221, -0.2411417322834647770 ) ) ;
#49830 = VECTOR ( 'NONE', #13517, 39.37007874015748143 ) ;
#49831 = CARTESIAN_POINT ( 'NONE',  ( 0.8858267716535438430, -0.4536011799217368745, -0.2665933059059886201 ) ) ;
#49832 = VERTEX_POINT ( 'NONE', #57202 ) ;
#49833 = CARTESIAN_POINT ( 'NONE',  ( -1.174540682414697335, -0.05778040916215522460, 0.4822834645669289988 ) ) ;
#49834 = CARTESIAN_POINT ( 'NONE',  ( -0.9711286089238838626, 0.2306618581243847221, -0.2411417322834647770 ) ) ;
#49835 = CARTESIAN_POINT ( 'NONE',  ( -0.06561679790026180015, -0.4281496062992127816, -0.4176697321401328100 ) ) ;
#49836 = CARTESIAN_POINT ( 'NONE',  ( -0.1070741851644051862, -0.3996062992125986590, -0.07217847769028871985 ) ) ;
#49837 = CARTESIAN_POINT ( 'NONE',  ( -0.1070741851644051862, -0.3996062992125986590, -2.511154855643044748 ) ) ;
#49838 = CARTESIAN_POINT ( 'NONE',  ( 0.6430446194225728496, 0.05413385826771666132, 0.4176697321401328100 ) ) ;
#49839 = CARTESIAN_POINT ( 'NONE',  ( -1.686351706036744558, 0.2952755905511810774, -0.1292274648535930714 ) ) ;
#49840 = CARTESIAN_POINT ( 'NONE',  ( 0.01312335958005323398, -0.4281496062992127816, -0.4176697321401328100 ) ) ;
#49841 = CARTESIAN_POINT ( 'NONE',  ( 0.8464566929133865436, 0.1660481256975883668, -0.3530559997133364547 ) ) ;
#49842 = CARTESIAN_POINT ( 'NONE',  ( -0.3996062992125986035, -0.1070741851644056997, -2.408136482939632561 ) ) ;
#49843 = CARTESIAN_POINT ( 'NONE',  ( 0.1974969037888706369, -0.3420746716998659953, -1.351706036745407014 ) ) ;
#49844 = CARTESIAN_POINT ( 'NONE',  ( 4.893765752498283924E-17, -0.3996062992125986035, -2.913385826771653697 ) ) ;
#49845 = DIRECTION ( 'NONE',  ( 1.776356839400250465E-15, 0.000000000000000000, -1.000000000000000000 ) ) ;
#49846 = CARTESIAN_POINT ( 'NONE',  ( 0.1049643490035303689, 0.3917322834645670104, -0.7729658792650917487 ) ) ;
#49847 = CARTESIAN_POINT ( 'NONE',  ( -0.6758530183727028406, -0.5511811023622048555, -0.09757992244046775898 ) ) ;
#49848 = CARTESIAN_POINT ( 'NONE',  ( -0.9448818897637790704, -0.1870078740157479769, 0.4822834645669291653 ) ) ;
#49849 = CARTESIAN_POINT ( 'NONE',  ( 0.5118110236220478892, 0.2952755905511811885, 0.000000000000000000 ) ) ;
#49850 = CARTESIAN_POINT ( 'NONE',  ( 0.3420746716998660508, 0.1974969037888705814, -2.727690288713910949 ) ) ;
#49851 = CARTESIAN_POINT ( 'NONE',  ( 0.9514435695538062676, -0.3162353388693409650, -0.4822834645669289433 ) ) ;
#49852 = CARTESIAN_POINT ( 'NONE',  ( -1.646981627296586703, -0.05778040916215522460, 0.4822834645669289988 ) ) ;
#49853 = CARTESIAN_POINT ( 'NONE',  ( 0.7217847769028878924, -0.4281496062992127816, -0.4176697321401328100 ) ) ;
#49854 = CARTESIAN_POINT ( 'NONE',  ( 0.3458507752293908943, -0.3458507752293908943, -2.303149606299212060 ) ) ;
#49855 = CARTESIAN_POINT ( 'NONE',  ( 0.1070741851644053527, 0.3996062992125986590, -2.198162729658792447 ) ) ;
#49856 = FACE_OUTER_BOUND ( 'NONE', #9298, .T. ) ;
#49857 = CARTESIAN_POINT ( 'NONE',  ( 0.9580052493438326877, 0.05413385826771666132, 0.4176697321401328100 ) ) ;
#49858 = CARTESIAN_POINT ( 'NONE',  ( 0.7874015748031503170, -0.1870078740157479769, 0.4822834645669291653 ) ) ;
#49859 = CARTESIAN_POINT ( 'NONE',  ( 1.049868766404200127, -0.5023911411419708095, -0.1820866141732282451 ) ) ;
#49861 = CARTESIAN_POINT ( 'NONE',  ( -1.574803149606298192, -0.1870078740157480879, -0.4822834645669291653 ) ) ;
#49860 = CARTESIAN_POINT ( 'NONE',  ( -1.568241469816272105, -0.2845877964562161244, -0.3641732283464567121 ) ) ;
#49862 = CARTESIAN_POINT ( 'NONE',  ( 4.797336870675656522E-17, -0.3917322834645670104, -0.005905511811023714773 ) ) ;
#49863 = CARTESIAN_POINT ( 'NONE',  ( 0.000000000000000000, 0.000000000000000000, -1.512162153811850596 ) ) ;
#49864 = CARTESIAN_POINT ( 'NONE',  ( 0.9120734908136490793, 0.2952755905511810774, -0.1292274648535930714 ) ) ;
#49865 = CARTESIAN_POINT ( 'NONE',  ( 1.541994750656168645, 0.1771653543307087075, -0.09757992244046823083 ) ) ;
#49866 = CARTESIAN_POINT ( 'NONE',  ( -0.5643044619422565855, 0.05413385826771626580, -0.4176697321401330321 ) ) ;
#49867 = CARTESIAN_POINT ( 'NONE',  ( -1.089238845144356427, 0.05413385826771666132, 0.4176697321401328100 ) ) ;
#49868 = AXIS2_PLACEMENT_3D ( 'NONE', #55871, #5370, #49567 ) ;
#49869 = CARTESIAN_POINT ( 'NONE',  ( -1.568241469816272105, -0.3162353388693409650, -0.4822834645669289433 ) ) ;
#49870 = CARTESIAN_POINT ( 'NONE',  ( -0.3392501089628019995, 0.1958661417322832277, -0.5833333333333334814 ) ) ;
#49871 = CARTESIAN_POINT ( 'NONE',  ( -0.1049643490035302024, -0.3917322834645671215, -1.481627296587926690 ) ) ;
#49872 = CARTESIAN_POINT ( 'NONE',  ( -0.3392501089628019995, 0.1958661417322832277, -2.380577427821522374 ) ) ;
#49873 = CARTESIAN_POINT ( 'NONE',  ( -1.528871391076114250, -0.5511811023622046335, 0.09757992244046803654 ) ) ;
#49874 = ORIENTED_EDGE ( 'NONE', *, *, #56663, .T. ) ;
#49875 = CARTESIAN_POINT ( 'NONE',  ( -9.674558042662121740E-17, 0.3949938075777409963, -2.677165354330708347 ) ) ;
#49876 = ORIENTED_EDGE ( 'NONE', *, *, #67320, .T. ) ;
#49877 = CARTESIAN_POINT ( 'NONE',  ( -0.04593175853018303251, 0.2066929133858267931, 0.1054918080437490802 ) ) ;
#49878 = CARTESIAN_POINT ( 'NONE',  ( 1.318897637795276356, 0.07958543189024071263, -0.2665933059059888421 ) ) ;
#49879 = CARTESIAN_POINT ( 'NONE',  ( -0.3996062992125986035, -7.340648628747425578E-17, -1.299212598425196985 ) ) ;
#49880 = LINE ( 'NONE', #22977, #4833 ) ;
#49881 = CARTESIAN_POINT ( 'NONE',  ( 0.4724409448818898127, -0.1265901696524988629, -0.8182414698162728817 ) ) ;
#49882 = CARTESIAN_POINT ( 'NONE',  ( 0.4935044252197980930, 1.488513638086841118, 0.5309055118110234117 ) ) ;
#49883 = CARTESIAN_POINT ( 'NONE',  ( -0.5314960629921148261, 2.742783305036532226, -3.197598447031737123 ) ) ;
#49884 = CARTESIAN_POINT ( 'NONE',  ( -0.1049643490035302024, -0.3917322834645671215, -0.4717847769028871152 ) ) ;
#49885 = CARTESIAN_POINT ( 'NONE',  ( -0.8858267716535425107, -0.4536011799217367080, 0.2665933059059888421 ) ) ;
#49886 = CARTESIAN_POINT ( 'NONE',  ( -1.115485564304461219, -0.3690944881889763329, 0.3153832671262228327 ) ) ;
#49887 = CARTESIAN_POINT ( 'NONE',  ( -1.128608923884513837, 0.2306618581243847221, -0.2411417322834647770 ) ) ;
#49888 = CARTESIAN_POINT ( 'NONE',  ( 0.2230971128608929543, 0.05413385826771626580, -0.4176697321401330321 ) ) ;
#49889 = CARTESIAN_POINT ( 'NONE',  ( -1.325459317585300889, 0.05413385826771666132, 0.4176697321401328100 ) ) ;
#49890 = AXIS2_PLACEMENT_3D ( 'NONE', #58817, #1174, #49278 ) ;
#49891 = ORIENTED_EDGE ( 'NONE', *, *, #48087, .T. ) ;
#49892 = CARTESIAN_POINT ( 'NONE',  ( 1.397637795275591177, -0.5400638737290844871, 0.3530559997133364547 ) ) ;
#49893 = CARTESIAN_POINT ( 'NONE',  ( -1.092353285368623750, -2.191421614605370878E-15, 0.4445507791589071167 ) ) ;
#49894 = DIRECTION ( 'NONE',  ( 0.000000000000000000, 0.000000000000000000, 1.000000000000000000 ) ) ;
#49895 = CARTESIAN_POINT ( 'NONE',  ( 0.1265901696524989462, 0.4724409448818897572, -1.568241469816272993 ) ) ;
#49896 = CARTESIAN_POINT ( 'NONE',  ( -1.646051170424378096, 0.8346805926620876059, 0.3149606299212598381 ) ) ;
#49897 = CARTESIAN_POINT ( 'NONE',  ( -0.3215223097112853146, -0.08942795157528024563, -0.3641732283464568787 ) ) ;
#49898 = EDGE_CURVE ( 'NONE', #72873, #23049, #48604, .T. ) ;
#49899 = CARTESIAN_POINT ( 'NONE',  ( -1.062992125984250968, -0.6692913385826771977, 8.415575281601705876E-17 ) ) ;
#49900 = CARTESIAN_POINT ( 'NONE',  ( 1.023622047244095334, -0.1870078740157479769, 0.4822834645669291653 ) ) ;
#49901 = ORIENTED_EDGE ( 'NONE', *, *, #41919, .T. ) ;
#49903 = CARTESIAN_POINT ( 'NONE',  ( -0.4562955581495677371, 1.668131542012051494, 2.594245572444889625 ) ) ;
#49902 = CARTESIAN_POINT ( 'NONE',  ( 0.1265901696524990572, -0.4724409448818897017, -2.290026246719159886 ) ) ;
#49904 = CARTESIAN_POINT ( 'NONE',  ( 1.581364829396326277, -0.3162353388693409650, -0.4822834645669289433 ) ) ;
#49905 = CARTESIAN_POINT ( 'NONE',  ( -1.377952755905511140, 0.2952755905511811885, 0.000000000000000000 ) ) ;
#49906 = CARTESIAN_POINT ( 'NONE',  ( -0.1049643490035306742, 0.3917322834645668994, -0.5590358023283972244 ) ) ;
#49907 = EDGE_CURVE ( 'NONE', #62516, #47058, #53398, .T. ) ;
#49908 = CARTESIAN_POINT ( 'NONE',  ( -0.1443569553805768291, -0.004921259842519576551, 0.3153832671262227771 ) ) ;
#49909 = CARTESIAN_POINT ( 'NONE',  ( -0.3917322834645671215, 0.1049643490035301469, -0.7473753280839894320 ) ) ;
#49910 = CARTESIAN_POINT ( 'NONE',  ( -0.1771653543307080136, 0.07958543189024071263, -0.2665933059059888421 ) ) ;
#49911 = CARTESIAN_POINT ( 'NONE',  ( 0.3805774278215230400, -0.004921259842519870586, -0.3153832671262229437 ) ) ;
#49912 = CARTESIAN_POINT ( 'NONE',  ( 0.5118110236220478892, 0.2952755905511811885, 0.000000000000000000 ) ) ;
#49913 = CARTESIAN_POINT ( 'NONE',  ( -0.7217847769028863381, -0.3690944881889763329, 0.3153832671262228327 ) ) ;
#49914 = CARTESIAN_POINT ( 'NONE',  ( -0.3392501089628017219, -0.1958661417322836718, -2.721784776902886893 ) ) ;
#49915 = CARTESIAN_POINT ( 'NONE',  ( 1.141732283464567566, 0.2952755905511811885, 0.000000000000000000 ) ) ;
#49916 = CARTESIAN_POINT ( 'NONE',  ( -0.9514435695538050464, -0.05778040916215560624, -0.4822834645669293319 ) ) ;
#49917 = CARTESIAN_POINT ( 'NONE',  ( -0.4724409448818898682, -8.678599364036362592E-17, -0.9035433070866141225 ) ) ;
#49918 = CARTESIAN_POINT ( 'NONE',  ( 0.006561679790026889343, -0.05778040916215522460, 0.4822834645669289988 ) ) ;
#49919 = CARTESIAN_POINT ( 'NONE',  ( -0.3346456692913377662, 0.1660481256975883668, -0.3530559997133364547 ) ) ;
#49920 = CARTESIAN_POINT ( 'NONE',  ( 1.410761154855643795, -0.08942795157528024563, -0.3641732283464568787 ) ) ;
#49921 = CARTESIAN_POINT ( 'NONE',  ( 0.2559055118110243332, -0.4536011799217368745, -0.2665933059059886201 ) ) ;
#49922 = CARTESIAN_POINT ( 'NONE',  ( -0.2821522309711278487, 0.2952755905511811885, 0.1292274648535926551 ) ) ;
#49923 = CARTESIAN_POINT ( 'NONE',  ( -1.082677165354329896, -0.5400638737290845981, -0.3530559997133363437 ) ) ;
#49924 = CARTESIAN_POINT ( 'NONE',  ( -3.900447471620230200, 2.687524476698323284, 0.5314960629921260393 ) ) ;
#49925 = CARTESIAN_POINT ( 'NONE',  ( 0.3937007874015751585, 1.771653543307086354, 0.000000000000000000 ) ) ;
#49926 = CARTESIAN_POINT ( 'NONE',  ( -0.1968503937007867743, 0.2952755905511811885, 0.000000000000000000 ) ) ;
#49927 = AXIS2_PLACEMENT_3D ( 'NONE', #59103, #65009, #32597 ) ;
#49928 = ORIENTED_EDGE ( 'NONE', *, *, #38011, .F. ) ;
#49929 = CARTESIAN_POINT ( 'NONE',  ( -0.1998031496062991630, -0.3460692066303959202, -1.874671916010498762 ) ) ;
#49930 = CARTESIAN_POINT ( 'NONE',  ( 1.003937007874016185, 0.1660481256975883668, -0.3530559997133364547 ) ) ;
#49931 = CARTESIAN_POINT ( 'NONE',  ( -0.5446194225721777693, -0.2845877964562161244, -0.3641732283464567121 ) ) ;
#49932 = CARTESIAN_POINT ( 'NONE',  ( -0.4527559055118102749, 0.1660481256975885056, 0.3530559997133364547 ) ) ;
#49933 = CARTESIAN_POINT ( 'NONE',  ( 1.410761154855643795, -0.05778040916215560624, -0.4822834645669293319 ) ) ;
#49934 = CARTESIAN_POINT ( 'NONE',  ( 0.9055118110236227702, 0.2952755905511811885, 0.000000000000000000 ) ) ;
#49935 = FACE_OUTER_BOUND ( 'NONE', #23693, .T. ) ;
#49936 = CARTESIAN_POINT ( 'NONE',  ( -1.069553805774277722, 0.1771653543307087630, 0.09757992244046791164 ) ) ;
#49937 = CARTESIAN_POINT ( 'NONE',  ( 4.893765752498283308E-17, -0.3996062992125985480, -0.6279527559055118058 ) ) ;
#49938 = CARTESIAN_POINT ( 'NONE',  ( 0.1070741851644054915, -0.3996062992125986035, -1.030183727034120533 ) ) ;
#49939 = CARTESIAN_POINT ( 'NONE',  ( -0.2891555358219908833, -0.2891555358219912164, -0.05905511811023628904 ) ) ;
#49940 = CARTESIAN_POINT ( 'NONE',  ( 0.3334193678581618414, 1.199601195606732063, 2.750748997350709324 ) ) ;
#49941 = CARTESIAN_POINT ( 'NONE',  ( 1.036745406824147731, -0.004921259842519576551, 0.3153832671262227771 ) ) ;
#49942 = CARTESIAN_POINT ( 'NONE',  ( 0.5249343832021003964, 0.1283753931104746893, -0.1820866141732285504 ) ) ;
#49943 = CARTESIAN_POINT ( 'NONE',  ( 0.3083989501312343062, -0.3162353388693405765, 0.4822834645669290543 ) ) ;
#49944 = DIRECTION ( 'NONE',  ( 0.000000000000000000, 0.000000000000000000, -1.000000000000000000 ) ) ;
#49945 = CARTESIAN_POINT ( 'NONE',  ( 0.1058382717557499880, 0.3949938075777409408, -1.330052493438319994 ) ) ;
#49946 = CARTESIAN_POINT ( 'NONE',  ( 0.8202099737532814183, -0.5511811023622048555, -0.09757992244046775898 ) ) ;
#49947 = CARTESIAN_POINT ( 'NONE',  ( -0.3346456692913377662, 0.1660481256975883668, -0.3530559997133364547 ) ) ;
#49948 = CARTESIAN_POINT ( 'NONE',  ( -0.6955380577427815458, 0.05413385826771666132, 0.4176697321401328100 ) ) ;
#49949 = CARTESIAN_POINT ( 'NONE',  ( 1.371391076115485941, 0.2952755905511811885, 0.1292274648535926551 ) ) ;
#49950 = CARTESIAN_POINT ( 'NONE',  ( 0.2362204724409451007, -0.4091458600556402980, -1.036745406824147064 ) ) ;
#49951 = CARTESIAN_POINT ( 'NONE',  ( -9.787531504996567848E-17, 0.3996062992125986035, -2.519685039370078705 ) ) ;
#49952 = CARTESIAN_POINT ( 'NONE',  ( -0.1312335958005241554, 0.1283753931104748280, 0.1820866141732283561 ) ) ;
#49953 = ORIENTED_EDGE ( 'NONE', *, *, #24452, .T. ) ;
#49954 = CARTESIAN_POINT ( 'NONE',  ( 0.3917322834645670104, 0.1049643490035304660, -0.9088119667004745938 ) ) ;
#49955 = ORIENTED_EDGE ( 'NONE', *, *, #59980, .T. ) ;
#49956 = CARTESIAN_POINT ( 'NONE',  ( -0.8136482939632537770, -0.6046776061558807314, 0.2411417322834647770 ) ) ;
#49957 = ADVANCED_FACE ( 'NONE', ( #1656 ), #20678, .T. ) ;
#49958 = CARTESIAN_POINT ( 'NONE',  ( -0.3083989501312330295, -0.3162353388693409650, -0.4822834645669289433 ) ) ;
#49959 = CARTESIAN_POINT ( 'NONE',  ( -0.3543307086614165824, 0.2952755905511811885, 0.000000000000000000 ) ) ;
#49960 = CARTESIAN_POINT ( 'NONE',  ( 0.3280839895013130669, -0.4281496062992127816, -0.4176697321401328100 ) ) ;
#49961 = CARTESIAN_POINT ( 'NONE',  ( -0.5380577427821514602, 0.05413385826771666132, 0.4176697321401328100 ) ) ;
#49962 = CARTESIAN_POINT ( 'NONE',  ( -1.417322834645668772, -0.1870078740157480879, -0.4822834645669291653 ) ) ;
#49963 = CARTESIAN_POINT ( 'NONE',  ( -0.6824146981627291497, -0.6046776061558809534, -0.2411417322834644161 ) ) ;
#49964 = CARTESIAN_POINT ( 'NONE',  ( 0.6627296587926515548, 0.2952755905511811885, 0.1292274648535926551 ) ) ;
#49965 = CARTESIAN_POINT ( 'NONE',  ( -0.1958661417322834220, -0.3392501089628018884, -1.002624671916010568 ) ) ;
#49966 = CARTESIAN_POINT ( 'NONE',  ( -0.2887139107611542133, -0.5023911411419708095, -0.1820866141732282451 ) ) ;
#49967 = ORIENTED_EDGE ( 'NONE', *, *, #53789, .T. ) ;
#49968 = CARTESIAN_POINT ( 'NONE',  ( 0.3420746716998659953, 0.1974969037888705536, -1.548556430446194065 ) ) ;
#49969 = VERTEX_POINT ( 'NONE', #22250 ) ;
#49970 = CARTESIAN_POINT ( 'NONE',  ( -1.108923884514435132, -0.2845877964562159024, 0.3641732283464567677 ) ) ;
#49971 = CARTESIAN_POINT ( 'NONE',  ( -0.9908136482939626788, 0.2952755905511811885, 0.1292274648535926551 ) ) ;
#49972 = CARTESIAN_POINT ( 'NONE',  ( -0.7939632545931750718, -0.05778040916215560624, -0.4822834645669293319 ) ) ;
#49973 = CARTESIAN_POINT ( 'NONE',  ( 0.4624320255261049062, 8.471767977567108961E-16, -0.4445507791589058955 ) ) ;
#49974 = CARTESIAN_POINT ( 'NONE',  ( -0.5839895013123351797, 0.2952755905511810774, -0.1292274648535930714 ) ) ;
#49975 = CARTESIAN_POINT ( 'NONE',  ( -0.6824146981627291497, -0.6046776061558809534, -0.2411417322834644161 ) ) ;
#49976 = DIRECTION ( 'NONE',  ( 0.000000000000000000, -1.000000000000000000, 0.000000000000000000 ) ) ;
#49977 = CARTESIAN_POINT ( 'NONE',  ( -0.4744094488188833059, 1.537401574803149984, -3.908320185825793658 ) ) ;
#49978 = CARTESIAN_POINT ( 'NONE',  ( 0.4593175853018380828, -0.004921259842519870586, -0.3153832671262229437 ) ) ;
#49979 = LINE ( 'NONE', #76499, #32326 ) ;
#49980 = CARTESIAN_POINT ( 'NONE',  ( -0.2867679344610365999, 0.2867679344610364889, -0.1043307086614174151 ) ) ;
#49981 = CARTESIAN_POINT ( 'NONE',  ( -0.08530183727034056085, -0.08942795157528024563, -0.3641732283464568787 ) ) ;
#49982 = CARTESIAN_POINT ( 'NONE',  ( -0.1902887139107604098, 0.2952755905511810774, -0.1292274648535930714 ) ) ;
#49983 = CARTESIAN_POINT ( 'NONE',  ( 3.910245801258434462, 1.413806224366693121, 0.4582898429536017004 ) ) ;
#49984 = CARTESIAN_POINT ( 'NONE',  ( 8.195543980992789655E-16, -0.1870078740157480879, -0.4822834645669291653 ) ) ;
#49985 = ORIENTED_EDGE ( 'NONE', *, *, #61823, .T. ) ;
#49986 = CARTESIAN_POINT ( 'NONE',  ( 0.3996062992125986590, -0.1070741851644053111, -2.001312335958005395 ) ) ;
#49987 = CARTESIAN_POINT ( 'NONE',  ( -0.5314960629921170465, 2.742779987576671186, -2.570293860457457225 ) ) ;
#49988 = VERTEX_POINT ( 'NONE', #47908 ) ;
#49989 = CARTESIAN_POINT ( 'NONE',  ( -0.3460692066303960313, 0.1998031496062989965, -1.677821522309711266 ) ) ;
#49990 = CIRCLE ( 'NONE', #16435, 0.1190944881889763746 ) ;
#49991 = CARTESIAN_POINT ( 'NONE',  ( -1.033875059083676939, 1.724409448818897905, 0.4359958488159718093 ) ) ;
#49992 = CARTESIAN_POINT ( 'NONE',  ( -1.213910761154854745, 0.1771653543307087075, -0.09757992244046823083 ) ) ;
#49993 = CARTESIAN_POINT ( 'NONE',  ( -1.338582677165353729, -0.1870078740157480879, -0.4822834645669291653 ) ) ;
#49994 = CARTESIAN_POINT ( 'NONE',  ( -0.4724409448818899238, 0.1265901696524986686, -0.5052493438320209140 ) ) ;
#49995 = CARTESIAN_POINT ( 'NONE',  ( 0.4037097067573611753, 1.223219560026271499E-15, 0.4445507791589056734 ) ) ;
#49996 = CARTESIAN_POINT ( 'NONE',  ( -0.2867679344610365999, 0.2867679344610364889, -2.781496062992125040 ) ) ;
#49997 = CARTESIAN_POINT ( 'NONE',  ( 1.325459317585302665, -0.4281496062992124485, 0.4176697321401328655 ) ) ;
#49998 = CARTESIAN_POINT ( 'NONE',  ( 0.6299212598425204535, -0.1870078740157479769, 0.4822834645669291653 ) ) ;
#49999 = CARTESIAN_POINT ( 'NONE',  ( -0.09842519685039295696, -0.5400638737290844871, 0.3530559997133364547 ) ) ;
#50000 = CARTESIAN_POINT ( 'NONE',  ( -0.9317585301837263412, -0.3690944881889765550, -0.3153832671262227771 ) ) ;
#50001 = CARTESIAN_POINT ( 'NONE',  ( -0.3412073490813641308, -0.6046776061558807314, 0.2411417322834647770 ) ) ;
#50002 = CARTESIAN_POINT ( 'NONE',  ( -0.4091458600556402980, -0.2362204724409451284, -2.491469816272966042 ) ) ;
#50003 = CARTESIAN_POINT ( 'NONE',  ( -0.8792650918635160906, 0.05413385826771626580, -0.4176697321401330321 ) ) ;
#50004 = CARTESIAN_POINT ( 'NONE',  ( -0.1974969037888704149, -0.3420746716998661063, -2.189632545931758489 ) ) ;
#50005 = CARTESIAN_POINT ( 'NONE',  ( 1.305774278215223960, 0.1771653543307087075, -0.09757992244046823083 ) ) ;
#50006 = CARTESIAN_POINT ( 'NONE',  ( -0.5249343832020990641, -0.5023911411419708095, -0.1820866141732282451 ) ) ;
#50007 = CARTESIAN_POINT ( 'NONE',  ( 1.299212598425197429, -0.5511811023622047445, 6.969142054262312111E-17 ) ) ;
#50008 = CARTESIAN_POINT ( 'NONE',  ( -1.482939632545930975, -0.4281496062992127816, -0.4176697321401328100 ) ) ;
#50009 = CARTESIAN_POINT ( 'NONE',  ( -1.207349081364828436, -0.5023911411419708095, 0.1820866141732285504 ) ) ;
#50010 = CARTESIAN_POINT ( 'NONE',  ( 0.1459841489473573395, 2.110655687203366066E-15, -0.3791475997938226761 ) ) ;
#50011 = CARTESIAN_POINT ( 'NONE',  ( 0.3871391076115493490, -0.2845877964562159024, 0.3641732283464567677 ) ) ;
#50012 = CARTESIAN_POINT ( 'NONE',  ( -0.4133858267716528645, -0.5400638737290844871, 0.3530559997133364547 ) ) ;
#50013 = CARTESIAN_POINT ( 'NONE',  ( -2.159244633716660644, 1.469861850861823083, 0.4698711669589715201 ) ) ;
#50014 = CARTESIAN_POINT ( 'NONE',  ( -0.006561679790025524116, -0.08942795157528024563, -0.3641732283464568787 ) ) ;
#50015 = DIRECTION ( 'NONE',  ( 0.000000000000000000, 0.000000000000000000, 1.000000000000000000 ) ) ;
#50016 = CARTESIAN_POINT ( 'NONE',  ( 0.8070866141732289112, -0.5400638737290845981, -0.3530559997133363437 ) ) ;
#50017 = DIRECTION ( 'NONE',  ( 0.000000000000000000, 0.000000000000000000, 1.000000000000000000 ) ) ;
#50018 = CARTESIAN_POINT ( 'NONE',  ( 1.240157480314961314, -0.4536011799217367080, 0.2665933059059888421 ) ) ;
#50019 = CARTESIAN_POINT ( 'NONE',  ( -0.8595800524934373854, -0.3162353388693409650, -0.4822834645669289433 ) ) ;
#50020 = CARTESIAN_POINT ( 'NONE',  ( -0.3083989501312330295, -0.2845877964562161244, -0.3641732283464567121 ) ) ;
#50021 = CARTESIAN_POINT ( 'NONE',  ( 1.033630966599880630, -4.927456884911482678E-16, 0.4445507791589062840 ) ) ;
#50022 = CARTESIAN_POINT ( 'NONE',  ( 0.3018372703412079971, -0.3690944881889763329, 0.3153832671262228327 ) ) ;
#50023 = CARTESIAN_POINT ( 'NONE',  ( -1.135170603674539924, -0.6692913385826771977, 0.1292274648535927661 ) ) ;
#50024 = EDGE_CURVE ( 'NONE', #22657, #65086, #50517, .T. ) ;
#50025 = CARTESIAN_POINT ( 'NONE',  ( -0.5380577427821514602, 0.05413385826771666132, 0.4176697321401328100 ) ) ;
#50026 = CARTESIAN_POINT ( 'NONE',  ( 0.3996062992125986035, -0.1070741851644052972, -0.8182414698162727706 ) ) ;
#50027 = EDGE_CURVE ( 'NONE', #8695, #72978, #483, .T. ) ;
#50028 = CARTESIAN_POINT ( 'NONE',  ( -0.2867679344610365999, 0.2867679344610364889, -2.151574803149605586 ) ) ;
#50029 = CARTESIAN_POINT ( 'NONE',  ( 0.4068241469816279987, -0.3690944881889765550, -0.3153832671262227771 ) ) ;
#50030 = CARTESIAN_POINT ( 'NONE',  ( -0.2034120734908128059, 0.2952755905511811885, 0.1292274648535926551 ) ) ;
#50031 = CARTESIAN_POINT ( 'NONE',  ( -0.5249343832020990641, 0.2306618581243848609, 0.2411417322834645549 ) ) ;
#50032 = CARTESIAN_POINT ( 'NONE',  ( -0.7152230971128602510, -0.2845877964562159024, 0.3641732283464567677 ) ) ;
#50033 = CARTESIAN_POINT ( 'NONE',  ( -3.926414575749307634, 1.160756069412853808, -0.2888700564287320360 ) ) ;
#50034 = CARTESIAN_POINT ( 'NONE',  ( 0.02624671916010564918, -0.6046776061558809534, -0.2411417322834644161 ) ) ;
#50035 = CARTESIAN_POINT ( 'NONE',  ( -1.154855643044618851, -0.5023911411419708095, -0.1820866141732282451 ) ) ;
#50036 = CARTESIAN_POINT ( 'NONE',  ( -1.607611548556429737, 0.2952755905511810774, -0.1292274648535930714 ) ) ;
#50037 = CARTESIAN_POINT ( 'NONE',  ( 0.1265901696524989184, 0.4724409448818898127, -2.198162729658792447 ) ) ;
#50038 = B_SPLINE_CURVE_WITH_KNOTS ( 'NONE', 3,
 ( #18732, #62524, #49883, #83122 ),
 .UNSPECIFIED., .F., .F.,
 ( 4, 4 ),
 ( 9.960895303349699888E-07, 0.001424104692945738371 ),
 .UNSPECIFIED. ) ;
#50039 = ORIENTED_EDGE ( 'NONE', *, *, #83256, .T. ) ;
#50040 = CARTESIAN_POINT ( 'NONE',  ( -1.699475065616797398, 0.1771653543307087630, 0.09757992244046791164 ) ) ;
#50041 = CARTESIAN_POINT ( 'NONE',  ( -1.391076115485563758, 0.2306618581243848609, 0.2411417322834645549 ) ) ;
#50042 = CIRCLE ( 'NONE', #79654, 1.968503937007874072 ) ;
#50043 = CARTESIAN_POINT ( 'NONE',  ( -0.7217847769028863381, 0.05413385826771626580, -0.4176697321401330321 ) ) ;
#50044 = CARTESIAN_POINT ( 'NONE',  ( -1.489501312335957062, -0.05778040916215522460, 0.4822834645669289988 ) ) ;
#50045 = CARTESIAN_POINT ( 'NONE',  ( 0.3917322834645670104, -0.1049643490035303411, -1.613517060367454237 ) ) ;
#50046 = CARTESIAN_POINT ( 'NONE',  ( -0.3808816823641234528, 0.09156050430092053938, -1.220472440944881942 ) ) ;
#50047 = EDGE_CURVE ( 'NONE', #69251, #78176, #41604, .T. ) ;
#50048 = CARTESIAN_POINT ( 'NONE',  ( 1.154855643044620184, -0.6046776061558807314, 0.2411417322834647770 ) ) ;
#50049 = CARTESIAN_POINT ( 'NONE',  ( 0.5643044619422579178, 0.05413385826771666132, 0.4176697321401328100 ) ) ;
#50050 = CARTESIAN_POINT ( 'NONE',  ( 1.141392835773559211, 0.3937007874015748254, 0.8264322058523028147 ) ) ;
#50051 = CARTESIAN_POINT ( 'NONE',  ( 0.3460692066303959202, -0.1998031496062991630, -2.543963254593176071 ) ) ;
#50052 = CARTESIAN_POINT ( 'NONE',  ( 1.279527559055118724, 0.07958543189024085140, 0.2665933059059887866 ) ) ;
#50053 = CARTESIAN_POINT ( 'NONE',  ( -0.3460692066303960868, 0.1998031496062990242, -0.9711286089238845287 ) ) ;
#50054 = EDGE_LOOP ( 'NONE', ( #79086, #59280, #10474, #56220, #75764, #50575, #52551 ) ) ;
#50055 = CARTESIAN_POINT ( 'NONE',  ( -0.2867679344610364334, -0.2867679344610367109, -2.570866141732283339 ) ) ;
#50056 = ORIENTED_EDGE ( 'NONE', *, *, #22073, .T. ) ;
#50057 = CARTESIAN_POINT ( 'NONE',  ( 0.4396325459317590445, -0.6692913385826771977, 0.1292274648535927661 ) ) ;
#50058 = CARTESIAN_POINT ( 'NONE',  ( -0.7611548556430438595, 0.2306618581243848609, 0.2411417322834645549 ) ) ;
#50059 = CARTESIAN_POINT ( 'NONE',  ( 1.581364829396326277, -0.05778040916215522460, 0.4822834645669289988 ) ) ;
#50060 = CARTESIAN_POINT ( 'NONE',  ( 1.266404199475066328, -0.3162353388693409650, -0.4822834645669289433 ) ) ;
#50061 = CARTESIAN_POINT ( 'NONE',  ( 1.587926509186352586, -0.4281496062992127816, -0.4176697321401328100 ) ) ;
#50062 = CARTESIAN_POINT ( 'NONE',  ( 0.3492006680983059663, -0.3045572308828553565, -0.01849200668098333403 ) ) ;
#50063 = CARTESIAN_POINT ( 'NONE',  ( -0.1115485564304453947, -0.6692913385826771977, 0.1292274648535927661 ) ) ;
#50064 = CARTESIAN_POINT ( 'NONE',  ( -1.410761154855641575, -0.3162353388693409650, -0.4822834645669289433 ) ) ;
#50065 = CARTESIAN_POINT ( 'NONE',  ( -1.496062992125983815, -0.1870078740157479769, 0.4822834645669291653 ) ) ;
#50066 = CARTESIAN_POINT ( 'NONE',  ( 1.423884514435696413, -0.3162353388693409650, -0.4822834645669289433 ) ) ;
#50067 = CARTESIAN_POINT ( 'NONE',  ( -0.3392501089628019995, 0.1958661417322832277, -2.630577427821522374 ) ) ;
#50068 = CARTESIAN_POINT ( 'NONE',  ( 0.7020997375328090762, -0.2845877964562159024, 0.3641732283464567677 ) ) ;
#50069 = ORIENTED_EDGE ( 'NONE', *, *, #4912, .T. ) ;
#50070 = CARTESIAN_POINT ( 'NONE',  ( 0.3949938075777411073, -0.1058382717557499464, -0.2690288713910761742 ) ) ;
#50071 = VERTEX_POINT ( 'NONE', #4959 ) ;
#50072 = CARTESIAN_POINT ( 'NONE',  ( -0.05249343832020938322, -0.5023911411419708095, -0.1820866141732282451 ) ) ;
#50073 = CARTESIAN_POINT ( 'NONE',  ( 0.2362204724409449064, 0.4091458600556404646, -0.1443569553805774397 ) ) ;
#50074 = CARTESIAN_POINT ( 'NONE',  ( 0.7480314960629927956, -0.6692913385826771977, 8.415575281601705876E-17 ) ) ;
#50075 = CARTESIAN_POINT ( 'NONE',  ( 0.2821522309711292364, -0.6692913385826771977, 0.1292274648535927661 ) ) ;
#50076 = CARTESIAN_POINT ( 'NONE',  ( -0.6758530183727028406, -0.6692913385826773087, -0.1292274648535924053 ) ) ;
#50077 = CARTESIAN_POINT ( 'NONE',  ( -0.1958661417322836995, 0.3392501089628017219, -1.584664985073177546 ) ) ;
#50078 = CARTESIAN_POINT ( 'NONE',  ( -1.279527559055116948, 0.1660481256975883668, -0.3530559997133364547 ) ) ;
#50079 = CARTESIAN_POINT ( 'NONE',  ( 0.3917322834645670104, -0.1049643490035303411, -2.558398950131233196 ) ) ;
#50080 = CARTESIAN_POINT ( 'NONE',  ( 1.450131233595801428, 0.1771653543307087630, 0.09757992244046791164 ) ) ;
#50081 = CARTESIAN_POINT ( 'NONE',  ( -1.108923884514435132, -0.05778040916215560624, -0.4822834645669293319 ) ) ;
#50082 = CARTESIAN_POINT ( 'NONE',  ( 0.8267716535433078384, -0.6692913385826771977, 8.415575281601705876E-17 ) ) ;
#50083 = CARTESIAN_POINT ( 'NONE',  ( 1.187664041994751285, -0.05778040916215522460, 0.4822834645669289988 ) ) ;
#50084 = CARTESIAN_POINT ( 'NONE',  ( -0.1998031496062991907, -0.3460692066303959757, -1.010498687664042050 ) ) ;
#50085 = CARTESIAN_POINT ( 'NONE',  ( -1.292650918635170010, -0.6692913385826771977, 0.1292274648535927661 ) ) ;
#50086 = CARTESIAN_POINT ( 'NONE',  ( 4.893765752498283308E-17, -0.3996062992125985480, -0.4704724409448819422 ) ) ;
#50087 = CARTESIAN_POINT ( 'NONE',  ( 0.2427821522309716595, -0.3162353388693409650, -0.4822834645669289433 ) ) ;
#50088 = CARTESIAN_POINT ( 'NONE',  ( -0.1998031496062991907, -0.3460692066303959757, -2.427821522309711266 ) ) ;
#50089 = CARTESIAN_POINT ( 'NONE',  ( 0.3917322834645670104, 2.398668435337828261E-17, -1.620078740157480324 ) ) ;
#50090 = CARTESIAN_POINT ( 'NONE',  ( 1.646981627296588035, -0.3162353388693405765, 0.4822834645669290543 ) ) ;
#50091 = CARTESIAN_POINT ( 'NONE',  ( 0.1509186351706045259, -0.08942795157528024563, -0.3641732283464568787 ) ) ;
#50092 = CARTESIAN_POINT ( 'NONE',  ( 0.8989501312335963501, -0.6692913385826773087, -0.1292274648535924053 ) ) ;
#50093 = CARTESIAN_POINT ( 'NONE',  ( 5.785732909357575061E-17, -0.4724409448818898682, -0.9429133858267716439 ) ) ;
#50094 = CARTESIAN_POINT ( 'NONE',  ( 0.8136482939632553313, -0.5023911411419708095, -0.1820866141732282451 ) ) ;
#50095 = CARTESIAN_POINT ( 'NONE',  ( 0.3477690288713918276, 0.2952755905511811885, 0.1292274648535926551 ) ) ;
#50096 = CARTESIAN_POINT ( 'NONE',  ( 0.1058382717557500852, -0.3949938075777408852, -1.106955380577427706 ) ) ;
#50097 = CARTESIAN_POINT ( 'NONE',  ( -0.9580052493438311334, -0.4281496062992124485, 0.4176697321401328655 ) ) ;
#50098 = CARTESIAN_POINT ( 'NONE',  ( -1.646051170424378096, 0.000000000000000000, 0.3464511005275205946 ) ) ;
#50099 = CARTESIAN_POINT ( 'NONE',  ( 0.8005249343832027131, -0.004921259842519576551, 0.3153832671262227771 ) ) ;
#50100 = CARTESIAN_POINT ( 'NONE',  ( -3.937007874015748143, 1.537401574803149984, 0.4744094488188970171 ) ) ;
#50101 = CARTESIAN_POINT ( 'NONE',  ( -0.2887139107611542133, 0.2306618581243848609, 0.2411417322834645549 ) ) ;
#50102 = CARTESIAN_POINT ( 'NONE',  ( 0.2296587926509192634, -0.2845877964562159024, 0.3641732283464567677 ) ) ;
#50103 = CARTESIAN_POINT ( 'NONE',  ( -2.554854094587807101, 1.520093187801264900, 0.4741711390158121486 ) ) ;
#50104 = CARTESIAN_POINT ( 'NONE',  ( -0.4658792650918627265, -0.05778040916215522460, 0.4822834645669289988 ) ) ;
#50105 = CARTESIAN_POINT ( 'NONE',  ( 0.7611548556430451917, -0.5023911411419708095, 0.1820866141732285504 ) ) ;
#50106 = CARTESIAN_POINT ( 'NONE',  ( -1.114781747626346187, -2.609869883881465018E-15, -0.3464511005275220379 ) ) ;
#50107 = EDGE_CURVE ( 'NONE', #42092, #56464, #25662, .T. ) ;
#50108 = CARTESIAN_POINT ( 'NONE',  ( -9.787531504996566615E-17, 0.3996062992125985480, -1.809055118110236560 ) ) ;
#50109 = CARTESIAN_POINT ( 'NONE',  ( 0.1771653543307093182, -0.5400638737290845981, -0.3530559997133363437 ) ) ;
#50110 = CARTESIAN_POINT ( 'NONE',  ( 1.292650918635171564, -0.5511811023622048555, -0.09757992244046775898 ) ) ;
#50111 = LINE ( 'NONE', #25, #68810 ) ;
#50112 = CARTESIAN_POINT ( 'NONE',  ( -0.4855643044619415427, -0.3690944881889763329, 0.3153832671262228327 ) ) ;
#50113 = CARTESIAN_POINT ( 'NONE',  ( -0.6430446194225716283, -0.3690944881889763329, 0.3153832671262228327 ) ) ;
#50114 = CARTESIAN_POINT ( 'NONE',  ( -0.5052493438320203589, 0.2952755905511810774, -0.1292274648535930714 ) ) ;
#50115 = CARTESIAN_POINT ( 'NONE',  ( 0.1640419947506569498, -0.05778040916215522460, 0.4822834645669289988 ) ) ;
#50116 = CARTESIAN_POINT ( 'NONE',  ( 1.043307086614173818, 0.07958543189024085140, 0.2665933059059887866 ) ) ;
#50117 = CARTESIAN_POINT ( 'NONE',  ( -1.686351706036744558, 0.1771653543307087075, -0.09757992244046823083 ) ) ;
#50118 = CARTESIAN_POINT ( 'NONE',  ( -1.699475065616797398, 0.2952755905511811885, 0.1292274648535926551 ) ) ;
#50119 = CARTESIAN_POINT ( 'NONE',  ( 0.9383202099737538715, -0.05778040916215560624, -0.4822834645669293319 ) ) ;
#50120 = DIRECTION ( 'NONE',  ( 0.000000000000000000, -1.000000000000000000, 0.000000000000000000 ) ) ;
#50121 = CARTESIAN_POINT ( 'NONE',  ( -0.3674540682414692561, -0.6046776061558809534, -0.2411417322834644161 ) ) ;
#50122 = CARTESIAN_POINT ( 'NONE',  ( -0.3392501089628019995, 0.1958661417322832277, -0.8982939632545933195 ) ) ;
#50123 = CARTESIAN_POINT ( 'NONE',  ( 0.9711286089238851948, -0.6046776061558809534, -0.2411417322834644161 ) ) ;
#50124 = CARTESIAN_POINT ( 'NONE',  ( 0.5446194225721792126, -0.3162353388693405765, 0.4822834645669290543 ) ) ;
#50125 = CARTESIAN_POINT ( 'NONE',  ( 0.000000000000000000, 2.755905511811024056, 0.000000000000000000 ) ) ;
#50126 = CARTESIAN_POINT ( 'NONE',  ( 0.4396325459317593221, 0.1771653543307087075, -0.09757992244046823083 ) ) ;
#50127 = CARTESIAN_POINT ( 'NONE',  ( 1.246719160104987623, 0.05413385826771626580, -0.4176697321401330321 ) ) ;
#50128 = CARTESIAN_POINT ( 'NONE',  ( 0.1902887139107617975, 0.1771653543307087630, 0.09757992244046791164 ) ) ;
#50129 = CARTESIAN_POINT ( 'NONE',  ( -0.3740157480314953431, 0.1660481256975885056, 0.3530559997133364547 ) ) ;
#50130 = CARTESIAN_POINT ( 'NONE',  ( -0.7137454485294948414, 2.793565526369265584, 0.4917280318828576857 ) ) ;
#50131 = CARTESIAN_POINT ( 'NONE',  ( 0.2427821522309716595, -0.3162353388693409650, -0.4822834645669289433 ) ) ;
#50132 = CARTESIAN_POINT ( 'NONE',  ( -0.7480314960629914633, -0.6692913385826771977, 8.415575281601705876E-17 ) ) ;
#50133 = AXIS2_PLACEMENT_3D ( 'NONE', #51983, #83161, #44412 ) ;
#50134 = CARTESIAN_POINT ( 'NONE',  ( -0.2821522309711278487, 0.1771653543307087630, 0.09757992244046791164 ) ) ;
#50135 = B_SPLINE_CURVE_WITH_KNOTS ( 'NONE', 3,
 ( #7561, #33233, #1255, #59719 ),
 .UNSPECIFIED., .F., .F.,
 ( 4, 4 ),
 ( 3.210432057730625665E-07, 0.001287787053612126763 ),
 .UNSPECIFIED. ) ;
#50136 = CARTESIAN_POINT ( 'NONE',  ( 0.4002624671916016896, -0.3162353388693409650, -0.4822834645669289433 ) ) ;
#50137 = CARTESIAN_POINT ( 'NONE',  ( 0.8202099737532814183, -0.5511811023622048555, -0.09757992244046775898 ) ) ;
#50138 = CARTESIAN_POINT ( 'NONE',  ( -0.3018372703412066094, -0.4281496062992127816, -0.4176697321401328100 ) ) ;
#50139 = CARTESIAN_POINT ( 'NONE',  ( 0.1265901696524990572, -0.4724409448818897017, -0.5577427821522309426 ) ) ;
#50141 = CARTESIAN_POINT ( 'NONE',  ( 1.482939632545932307, 0.05413385826771626580, -0.4176697321401330321 ) ) ;
#50140 = CARTESIAN_POINT ( 'NONE',  ( 0.6986524979670498681, 8.471767977567108961E-16, -0.4445507791589058955 ) ) ;
#50142 = CARTESIAN_POINT ( 'NONE',  ( 1.660104986876641320, -0.05778040916215522460, 0.4822834645669289988 ) ) ;
#50143 = CARTESIAN_POINT ( 'NONE',  ( 0.3917322834645669549, 0.1049643490035304660, -2.006561679790026531 ) ) ;
#50144 = CARTESIAN_POINT ( 'NONE',  ( -1.076115485564303809, -0.6046776061558809534, -0.2411417322834644161 ) ) ;
#50145 = CARTESIAN_POINT ( 'NONE',  ( -0.9317585301837263412, 0.05413385826771666132, 0.4176697321401328100 ) ) ;
#50146 = CARTESIAN_POINT ( 'NONE',  ( 0.3458507752293908943, 0.3458507752293908943, -0.2952755905511811330 ) ) ;
#50147 = CARTESIAN_POINT ( 'NONE',  ( -0.2891555358219908833, -0.2891555358219912164, -2.893700787401575436 ) ) ;
#50148 = ORIENTED_EDGE ( 'NONE', *, *, #41951, .T. ) ;
#50149 = CARTESIAN_POINT ( 'NONE',  ( 0.3805774278215230400, -0.3690944881889763329, 0.3153832671262228327 ) ) ;
#50151 = CARTESIAN_POINT ( 'NONE',  ( 0.3917322834645669549, 0.1049643490035304660, -1.534120734908136052 ) ) ;
#50150 = VECTOR ( 'NONE', #12263, 39.37007874015748143 ) ;
#50152 = CARTESIAN_POINT ( 'NONE',  ( 0.8792650918635177559, -0.4281496062992127816, -0.4176697321401328100 ) ) ;
#50153 = CARTESIAN_POINT ( 'NONE',  ( 0.4724409448818896462, 0.1265901696524990294, -2.486876640419947382 ) ) ;
#50154 = CARTESIAN_POINT ( 'NONE',  ( -0.3458507752293909498, 0.3458507752293908388, -0.8838582677165351953 ) ) ;
#50155 = CARTESIAN_POINT ( 'NONE',  ( -0.3083989501312330295, -0.2845877964562161244, -0.3641732283464567121 ) ) ;
#50156 = CARTESIAN_POINT ( 'NONE',  ( -0.2690288713910753970, 0.2952755905511810219, -0.1292274648535930437 ) ) ;
#50157 = CARTESIAN_POINT ( 'NONE',  ( 1.194225721784777594, 0.05413385826771666132, 0.4176697321401328100 ) ) ;
#50158 = CARTESIAN_POINT ( 'NONE',  ( 1.489501312335958172, -0.08942795157528024563, -0.3641732283464568787 ) ) ;
#50159 = CARTESIAN_POINT ( 'NONE',  ( -0.1049868766404193215, -0.6046776061558807314, 0.2411417322834647770 ) ) ;
#50160 = CARTESIAN_POINT ( 'NONE',  ( -9.594673741351310580E-17, 0.3917322834645669549, -0.5524741225383709153 ) ) ;
#50161 = CARTESIAN_POINT ( 'NONE',  ( -0.4133858267716528645, -0.5400638737290844871, 0.3530559997133364547 ) ) ;
#50162 = CARTESIAN_POINT ( 'NONE',  ( -1.154855643044618851, -0.5023911411419708095, -0.1820866141732282451 ) ) ;
#50163 = CARTESIAN_POINT ( 'NONE',  ( -0.6364829396325453192, -0.3162353388693405765, 0.4822834645669290543 ) ) ;
#50164 = CARTESIAN_POINT ( 'NONE',  ( -1.646051170424378096, 0.000000000000000000, 0.3464511005275205946 ) ) ;
#50165 = CARTESIAN_POINT ( 'NONE',  ( -0.3005662378122840872, 1.170051713876987920, -1.947704203106506604 ) ) ;
#50166 = ORIENTED_EDGE ( 'NONE', *, *, #39397, .F. ) ;
#50167 = CARTESIAN_POINT ( 'NONE',  ( 0.3917322834645670659, -0.1049643490035303273, -2.155531126805461550 ) ) ;
#50168 = CARTESIAN_POINT ( 'NONE',  ( 0.6036745406824154392, 0.2306618581243847221, -0.2411417322834647770 ) ) ;
#50169 = VERTEX_POINT ( 'NONE', #74433 ) ;
#50170 = CARTESIAN_POINT ( 'NONE',  ( -0.3674540682414692561, -0.6046776061558809534, -0.2411417322834644161 ) ) ;
#50171 = CARTESIAN_POINT ( 'NONE',  ( -1.351706036745406347, -0.4281496062992124485, 0.4176697321401328655 ) ) ;
#50172 = EDGE_CURVE ( 'NONE', #51375, #2979, #52917, .T. ) ;
#50173 = CARTESIAN_POINT ( 'NONE',  ( 0.8792650918635177559, -0.4281496062992127816, -0.4176697321401328100 ) ) ;
#50174 = CARTESIAN_POINT ( 'NONE',  ( -0.03937007874015669567, 0.2952755905511811885, 0.000000000000000000 ) ) ;
#50175 = CARTESIAN_POINT ( 'NONE',  ( -0.1958661417322834220, -0.3392501089628018884, -1.410104986876640654 ) ) ;
#50176 = CARTESIAN_POINT ( 'NONE',  ( -0.8202099737532801971, -0.6692913385826771977, 0.1292274648535927661 ) ) ;
#50177 = CARTESIAN_POINT ( 'NONE',  ( 0.3083989501312343062, -0.05778040916215560624, -0.4822834645669293319 ) ) ;
#50178 = CARTESIAN_POINT ( 'NONE',  ( -0.5577427821522301654, -0.3162353388693405765, 0.4822834645669290543 ) ) ;
#50179 = EDGE_CURVE ( 'NONE', #45807, #60543, #80349, .T. ) ;
#50180 = CARTESIAN_POINT ( 'NONE',  ( 0.2034120734908144990, -0.5511811023622046335, 0.09757992244046803654 ) ) ;
#50181 = CARTESIAN_POINT ( 'NONE',  ( -0.2431881074996896375, -0.1674863405202415556, 5.643916622257989957 ) ) ;
#50182 = CARTESIAN_POINT ( 'NONE',  ( -0.09842519685039295696, 0.1660481256975883668, -0.3530559997133364547 ) ) ;
#50183 = CARTESIAN_POINT ( 'NONE',  ( 1.522309711286089939, -0.6046776061558809534, -0.2411417322834644161 ) ) ;
#50184 = CARTESIAN_POINT ( 'NONE',  ( 0.1958661417322836440, -0.3392501089628017219, -2.761154855643044304 ) ) ;
#50185 = ORIENTED_EDGE ( 'NONE', *, *, #42797, .T. ) ;
#50186 = ORIENTED_EDGE ( 'NONE', *, *, #81979, .T. ) ;
#50187 = CARTESIAN_POINT ( 'NONE',  ( 0.7414698162729663755, 0.2952755905511811885, 0.1292274648535926551 ) ) ;
#50188 = CARTESIAN_POINT ( 'NONE',  ( 0.3215223097112867578, -0.08942795157527998196, 0.3641732283464567121 ) ) ;
#50190 = DIRECTION ( 'NONE',  ( 0.000000000000000000, -1.000000000000000000, 0.000000000000000000 ) ) ;
#50189 = CARTESIAN_POINT ( 'NONE',  ( 0.9568149321855670131, 1.522401787774001735E-16, 0.3627985898453514046 ) ) ;
#50191 = CARTESIAN_POINT ( 'NONE',  ( 0.1049643490035303689, 0.3917322834645670104, -1.022965879265091749 ) ) ;
#50192 = CARTESIAN_POINT ( 'NONE',  ( 0.3458507752293908943, -0.3458507752293908943, 0.1397637795275590289 ) ) ;
#50193 = FACE_OUTER_BOUND ( 'NONE', #78578, .T. ) ;
#50194 = CARTESIAN_POINT ( 'NONE',  ( 0.3949938075777409963, 2.418639510665530743E-17, 0.1200787401574803376 ) ) ;
#50195 = CARTESIAN_POINT ( 'NONE',  ( 0.3215223097112867578, -0.05778040916215522460, 0.4822834645669289988 ) ) ;
#50196 = CARTESIAN_POINT ( 'NONE',  ( -1.023622047244093558, -0.1870078740157479769, 0.4822834645669291653 ) ) ;
#50197 = VECTOR ( 'NONE', #2019, 39.37007874015748143 ) ;
#50198 = CARTESIAN_POINT ( 'NONE',  ( -0.9711286089238838626, -0.6046776061558807314, 0.2411417322834647770 ) ) ;
#50199 = CARTESIAN_POINT ( 'NONE',  ( 0.1968503937007881344, 0.2952755905511811885, 0.000000000000000000 ) ) ;
#50200 = CARTESIAN_POINT ( 'NONE',  ( 1.023622047244095112, -0.1870078740157480879, -0.4822834645669291653 ) ) ;
#50201 = CARTESIAN_POINT ( 'NONE',  ( 1.358267716535433323, 0.07958543189024085140, 0.2665933059059887866 ) ) ;
#50202 = CARTESIAN_POINT ( 'NONE',  ( 1.187664041994751285, -0.08942795157527998196, 0.3641732283464567121 ) ) ;
#50203 = CARTESIAN_POINT ( 'NONE',  ( -0.8070866141732276899, 0.1660481256975883668, -0.3530559997133364547 ) ) ;
#50204 = CARTESIAN_POINT ( 'NONE',  ( -0.3996062992125984925, -0.1070741851644056858, -0.4376640419947506744 ) ) ;
#50205 = CARTESIAN_POINT ( 'NONE',  ( -1.594488188976377119, 0.07958543189024071263, -0.2665933059059888421 ) ) ;
#50206 = CARTESIAN_POINT ( 'NONE',  ( 4.797336870675656522E-17, -0.3917322834645670104, -0.3858267716535432879 ) ) ;
#50207 = CARTESIAN_POINT ( 'NONE',  ( -0.2296587926509179312, -0.05778040916215522460, 0.4822834645669289988 ) ) ;
#50209 = CARTESIAN_POINT ( 'NONE',  ( -1.220472440944881054, 2.362204724409448620, 0.5309055118110237448 ) ) ;
#50208 = CARTESIAN_POINT ( 'NONE',  ( 1.332020997375329197, -0.3162353388693405765, 0.4822834645669290543 ) ) ;
#50210 = CARTESIAN_POINT ( 'NONE',  ( -1.450131233595799651, -0.5511811023622046335, 0.09757992244046803654 ) ) ;
#50211 = CARTESIAN_POINT ( 'NONE',  ( 0.05249343832021075018, -0.6046776061558807314, 0.2411417322834647770 ) ) ;
#50212 = CARTESIAN_POINT ( 'NONE',  ( 0.8989501312335963501, -0.5511811023622048555, -0.09757992244046775898 ) ) ;
#50213 = EDGE_CURVE ( 'NONE', #895, #74332, #17602, .T. ) ;
#50214 = AXIS2_PLACEMENT_3D ( 'NONE', #80948, #55241, #80542 ) ;
#50215 = CARTESIAN_POINT ( 'NONE',  ( -1.482939632545930975, -0.3690944881889765550, -0.3153832671262227771 ) ) ;
#50216 = CARTESIAN_POINT ( 'NONE',  ( 0.9580052493438327987, -0.4281496062992127816, -0.4176697321401328100 ) ) ;
#50217 = CARTESIAN_POINT ( 'NONE',  ( 0.6299212598425341092, 2.165354330708662012, -3.937007874015759690 ) ) ;
#50218 = CARTESIAN_POINT ( 'NONE',  ( -0.3083989501312330295, -0.08942795157527998196, 0.3641732283464567121 ) ) ;
#50219 = CARTESIAN_POINT ( 'NONE',  ( -0.6824146981627291497, -0.6046776061558809534, -0.2411417322834644161 ) ) ;
#50220 = CARTESIAN_POINT ( 'NONE',  ( 1.614173228346457378, -0.6692913385826771977, 8.415575281601705876E-17 ) ) ;
#50221 = CARTESIAN_POINT ( 'NONE',  ( -1.318897637795274802, -0.5400638737290845981, -0.3530559997133363437 ) ) ;
#50222 = CARTESIAN_POINT ( 'NONE',  ( 1.482939632545932307, -0.4281496062992124485, 0.4176697321401328655 ) ) ;
#50223 = CARTESIAN_POINT ( 'NONE',  ( -0.1958661417322833942, -0.3392501089628018884, -1.007237163550868120 ) ) ;
#50224 = CARTESIAN_POINT ( 'NONE',  ( -1.515748031496062076, -0.4536011799217367080, 0.2665933059059888421 ) ) ;
#50225 = CARTESIAN_POINT ( 'NONE',  ( 2.594245572444920267, 1.668131542012050827, 0.4562955581495592994 ) ) ;
#50226 = CARTESIAN_POINT ( 'NONE',  ( 1.371391076115485719, -0.6692913385826773087, -0.1292274648535924053 ) ) ;
#50227 = CARTESIAN_POINT ( 'NONE',  ( 0.1265901696524990294, -0.4724409448818896462, -2.524278215223096478 ) ) ;
#50228 = CARTESIAN_POINT ( 'NONE',  ( -1.469816272965878357, -0.6046776061558809534, -0.2411417322834644161 ) ) ;
#50229 = CARTESIAN_POINT ( 'NONE',  ( 1.627296587926509996, -0.6046776061558807314, 0.2411417322834647770 ) ) ;
#50230 = CARTESIAN_POINT ( 'NONE',  ( -1.043307086614172707, 0.07958543189024071263, -0.2665933059059888421 ) ) ;
#50231 = CARTESIAN_POINT ( 'NONE',  ( 1.548556430446194954, 0.1283753931104746893, -0.1820866141732285504 ) ) ;
#50232 = CARTESIAN_POINT ( 'NONE',  ( -0.2821522309711278487, -0.6692913385826773087, -0.1292274648535924053 ) ) ;
#50233 = CARTESIAN_POINT ( 'NONE',  ( -0.08530183727034056085, -0.2845877964562159024, 0.3641732283464567677 ) ) ;
#50234 = CARTESIAN_POINT ( 'NONE',  ( -0.9711286089238838626, -0.5023911411419708095, 0.1820866141732285504 ) ) ;
#50235 = CARTESIAN_POINT ( 'NONE',  ( 1.384514435695538337, -0.5511811023622046335, 0.09757992244046803654 ) ) ;
#50236 = CARTESIAN_POINT ( 'NONE',  ( 0.8595800524934390507, -0.3162353388693405765, 0.4822834645669290543 ) ) ;
#50237 = CARTESIAN_POINT ( 'NONE',  ( 1.463254593175853824, 0.2952755905511810774, -0.1292274648535930714 ) ) ;
#50238 = CARTESIAN_POINT ( 'NONE',  ( 0.6167979002624679463, -0.004921259842519870586, -0.3153832671262229437 ) ) ;
#50239 = DIMENSIONAL_EXPONENTS ( 1.000000000000000000, 0.000000000000000000, 0.000000000000000000, 0.000000000000000000, 0.000000000000000000, 0.000000000000000000, 0.000000000000000000 ) ;
#50240 = CARTESIAN_POINT ( 'NONE',  ( 0.4133858267716541968, 0.1660481256975885056, 0.3530559997133364547 ) ) ;
#50241 = CARTESIAN_POINT ( 'NONE',  ( 0.9120734908136489683, -0.5511811023622046335, 0.09757992244046803654 ) ) ;
#50242 = ORIENTED_EDGE ( 'NONE', *, *, #61206, .F. ) ;
#50243 = CARTESIAN_POINT ( 'NONE',  ( -1.463254593175852492, 0.2952755905511811885, 0.1292274648535926551 ) ) ;
#50244 = CARTESIAN_POINT ( 'NONE',  ( -1.417322834645668772, -0.1870078740157480879, -0.4822834645669291653 ) ) ;
#50245 = CARTESIAN_POINT ( 'NONE',  ( -0.01312335958005186876, -0.4281496062992124485, 0.4176697321401328655 ) ) ;
#50246 = CARTESIAN_POINT ( 'NONE',  ( -2.158884350236584204, 1.606100245667701598, -0.4697171261335985060 ) ) ;
#50247 = CARTESIAN_POINT ( 'NONE',  ( -0.3460692066303957537, -0.1998031496062994405, -2.648950131233595684 ) ) ;
#50248 = CARTESIAN_POINT ( 'NONE',  ( 0.3412073490813655186, 0.2306618581243848609, 0.2411417322834645549 ) ) ;
#50249 = CARTESIAN_POINT ( 'NONE',  ( 1.233595800524935227, -0.5023911411419708095, 0.1820866141732285504 ) ) ;
#50250 = CARTESIAN_POINT ( 'NONE',  ( -0.1706036745406816491, 0.05413385826771626580, -0.4176697321401330321 ) ) ;
#50251 = CARTESIAN_POINT ( 'NONE',  ( 0.2362204724409456558, -0.1870078740157480879, -0.4822834645669291653 ) ) ;
#50252 = CARTESIAN_POINT ( 'NONE',  ( 0.3996062992125986590, -0.1070741851644053111, -2.316272965879265122 ) ) ;
#50253 = CARTESIAN_POINT ( 'NONE',  ( -0.1058382717557503211, 0.3949938075777409408, -1.423884514435695969 ) ) ;
#50254 = CARTESIAN_POINT ( 'NONE',  ( -0.3460692066303958092, -0.1998031496062994683, -2.887139107611548461 ) ) ;
#50255 = DIRECTION ( 'NONE',  ( 0.000000000000000000, 1.000000000000000000, 0.000000000000000000 ) ) ;
#50256 = CIRCLE ( 'NONE', #44886, 0.1771653543307085410 ) ;
#50257 = CARTESIAN_POINT ( 'NONE',  ( -0.3392501089628017219, -0.1958661417322836718, -0.6745406824146981117 ) ) ;
#50258 = CARTESIAN_POINT ( 'NONE',  ( -0.4461942257217840213, 0.1283753931104748280, 0.1820866141732283561 ) ) ;
#50259 = CARTESIAN_POINT ( 'NONE',  ( -0.6692913385826764205, -0.6692913385826771977, 8.415575281601705876E-17 ) ) ;
#50260 = CARTESIAN_POINT ( 'NONE',  ( 0.6299212598425204535, -0.1870078740157479769, 0.4822834645669291653 ) ) ;
#50261 = CARTESIAN_POINT ( 'NONE',  ( 0.3420746716998660508, 0.1974969037888705814, -2.412729658792650778 ) ) ;
#50262 = CARTESIAN_POINT ( 'NONE',  ( 0.7480314960629927956, 0.2952755905511811885, 0.000000000000000000 ) ) ;
#50263 = CARTESIAN_POINT ( 'NONE',  ( 1.561679790026247350, -0.4281496062992124485, 0.4176697321401328655 ) ) ;
#50264 = CARTESIAN_POINT ( 'NONE',  ( 0.9776902887139113929, 0.2952755905511811885, 0.1292274648535926551 ) ) ;
#50265 = CARTESIAN_POINT ( 'NONE',  ( 0.1265901696524990294, -0.4724409448818896462, -2.919947506561679784 ) ) ;
#50266 = CARTESIAN_POINT ( 'NONE',  ( -0.1998031496062991907, -0.3460692066303959757, -2.112860892388451539 ) ) ;
#50267 = CARTESIAN_POINT ( 'NONE',  ( 1.633858267716535639, -0.5400638737290844871, 0.3530559997133364547 ) ) ;
#50268 = CARTESIAN_POINT ( 'NONE',  ( 0.7611548556430451917, -0.6046776061558807314, 0.2411417322834647770 ) ) ;
#50269 = EDGE_CURVE ( 'NONE', #32791, #11499, #73676, .T. ) ;
#50270 = CARTESIAN_POINT ( 'NONE',  ( 0.3937007874015754361, -0.1870078740157480879, -0.4822834645669291653 ) ) ;
#50271 = CARTESIAN_POINT ( 'NONE',  ( 1.443569553805774897, 0.1283753931104748280, 0.1820866141732283561 ) ) ;
#50272 = CARTESIAN_POINT ( 'NONE',  ( -1.489501312335957062, -0.08942795157527998196, 0.3641732283464567121 ) ) ;
#50273 = CARTESIAN_POINT ( 'NONE',  ( -0.3917322834645671215, 0.1049643490035301469, 0.04002624671916000382 ) ) ;
#50274 = CARTESIAN_POINT ( 'NONE',  ( 0.6102362204724416372, 0.1660481256975883668, -0.3530559997133364547 ) ) ;
#50275 = DIRECTION ( 'NONE',  ( -1.000000000000000000, -3.412570772413389987E-16, 0.000000000000000000 ) ) ;
#50276 = CARTESIAN_POINT ( 'NONE',  ( -0.3543307086614165824, -0.6692913385826771977, 8.415575281601705876E-17 ) ) ;
#50277 = CARTESIAN_POINT ( 'NONE',  ( -1.082677165354329896, 0.1660481256975885056, 0.3530559997133364547 ) ) ;
#50278 = CARTESIAN_POINT ( 'NONE',  ( 1.030183727034121421, -0.3162353388693409650, -0.4822834645669289433 ) ) ;
#50279 = CARTESIAN_POINT ( 'NONE',  ( -0.3917322834645671215, 0.1049643490035301469, -0.5898950131233595684 ) ) ;
#50280 = CARTESIAN_POINT ( 'NONE',  ( -0.3917322834645670104, -7.196005306013484475E-17, -1.606299212598425452 ) ) ;
#50281 = CARTESIAN_POINT ( 'NONE',  ( -0.2867679344610364334, -0.2867679344610367109, -2.570866141732283339 ) ) ;
#50282 = CARTESIAN_POINT ( 'NONE',  ( 1.528871391076116026, 0.2952755905511811885, 0.1292274648535926551 ) ) ;
#50283 = ORIENTED_EDGE ( 'NONE', *, *, #64378, .F. ) ;
#50284 = CARTESIAN_POINT ( 'NONE',  ( -0.3949938075777411628, 0.1058382717557497937, -2.552493438320210473 ) ) ;
#50285 = ORIENTED_EDGE ( 'NONE', *, *, #19337, .T. ) ;
#50286 = CARTESIAN_POINT ( 'NONE',  ( 0.5027385518326215053, 1.496062992125283708, 0.5309055118110234117 ) ) ;
#50287 = CARTESIAN_POINT ( 'NONE',  ( 1.482939632545932307, -0.004921259842519870586, -0.3153832671262229437 ) ) ;
#50288 = CARTESIAN_POINT ( 'NONE',  ( -0.3460692066303958092, -0.1998031496062994683, -1.469816272965879245 ) ) ;
#50289 = CARTESIAN_POINT ( 'NONE',  ( 1.456692913385827515, -0.5511811023622047445, 6.969142054262312111E-17 ) ) ;
#50290 = CARTESIAN_POINT ( 'NONE',  ( -0.1265901696524986964, -0.4724409448818899238, -0.7788713910761155823 ) ) ;
#50291 = DIRECTION ( 'NONE',  ( -1.000000000000000000, -0.000000000000000000, -0.000000000000000000 ) ) ;
#50292 = CARTESIAN_POINT ( 'NONE',  ( -0.4724409448818898682, -8.678599364036362592E-17, -1.929133858267716439 ) ) ;
#50293 = CARTESIAN_POINT ( 'NONE',  ( -0.3917322834645670104, -7.196005306013484475E-17, -0.5964566929133858775 ) ) ;
#50294 = CARTESIAN_POINT ( 'NONE',  ( -0.8005249343832011588, -0.004921259842519870586, -0.3153832671262229437 ) ) ;
#50295 = CARTESIAN_POINT ( 'NONE',  ( -1.384514435695537005, 0.1771653543307087630, 0.09757992244046791164 ) ) ;
#50296 = CARTESIAN_POINT ( 'NONE',  ( -1.417322834645668772, -0.1870078740157480879, -0.4822834645669291653 ) ) ;
#50297 = CARTESIAN_POINT ( 'NONE',  ( 0.1771653543307093182, 0.1660481256975885056, 0.3530559997133364547 ) ) ;
#50298 = CARTESIAN_POINT ( 'NONE',  ( -1.627296587926508442, 0.2306618581243848609, 0.2411417322834645549 ) ) ;
#50299 = VERTEX_POINT ( 'NONE', #74854 ) ;
#50300 = CARTESIAN_POINT ( 'NONE',  ( 1.509186351706037543, -0.4281496062992127816, -0.4176697321401328100 ) ) ;
#50301 = DIRECTION ( 'NONE',  ( 0.000000000000000000, 0.000000000000000000, -1.000000000000000000 ) ) ;
#50302 = DIRECTION ( 'NONE',  ( 1.000000000000000000, 0.000000000000000000, 0.000000000000000000 ) ) ;
#50303 = CARTESIAN_POINT ( 'NONE',  ( 0.4724409448818898682, 2.892866454678787531E-17, -2.165354330708661568 ) ) ;
#50304 = CARTESIAN_POINT ( 'NONE',  ( 2.158884350236621064, 1.606100245667702708, 0.4697171261335982284 ) ) ;
#50305 = CARTESIAN_POINT ( 'NONE',  ( -0.3871391076115476282, -0.08942795157527998196, 0.3641732283464567121 ) ) ;
#50306 = CARTESIAN_POINT ( 'NONE',  ( -1.345144356955379816, -0.3162353388693405765, 0.4822834645669290543 ) ) ;
#50307 = CARTESIAN_POINT ( 'NONE',  ( 1.181102362204725198, -0.1870078740157479769, 0.4822834645669291653 ) ) ;
#50308 = VERTEX_POINT ( 'NONE', #48321 ) ;
#50310 = LINE ( 'NONE', #76418, #47902 ) ;
#50309 = CARTESIAN_POINT ( 'NONE',  ( 0.7611548556430454138, 0.2306618581243847221, -0.2411417322834647770 ) ) ;
#50311 = CARTESIAN_POINT ( 'NONE',  ( -1.692913385826770645, 0.2952755905511811885, 0.000000000000000000 ) ) ;
#50312 = CARTESIAN_POINT ( 'NONE',  ( -1.259842519685038686, -0.1870078740157479769, 0.4822834645669291653 ) ) ;
#50313 = CARTESIAN_POINT ( 'NONE',  ( -0.1958661417322834497, -0.3392501089628018884, -0.3031302905173735573 ) ) ;
#50314 = CARTESIAN_POINT ( 'NONE',  ( -0.5249343832020990641, -0.5023911411419708095, -0.1820866141732282451 ) ) ;
#50315 = CARTESIAN_POINT ( 'NONE',  ( 0.3392501089628018884, -0.1958661417322834220, -0.6620734908136483021 ) ) ;
#50316 = AXIS2_PLACEMENT_3D ( 'NONE', #19151, #41428, #48560 ) ;
#50317 = CARTESIAN_POINT ( 'NONE',  ( -0.6167979002624665030, -0.3690944881889765550, -0.3153832671262227771 ) ) ;
#50318 = CARTESIAN_POINT ( 'NONE',  ( 0.3477690288713918276, 0.1771653543307087630, 0.09757992244046791164 ) ) ;
#50319 = CARTESIAN_POINT ( 'NONE',  ( 0.6364829396325465405, -0.05778040916215522460, 0.4822834645669289988 ) ) ;
#50320 = CARTESIAN_POINT ( 'NONE',  ( -0.7742782152230962556, -0.3690944881889765550, -0.3153832671262227771 ) ) ;
#50321 = CARTESIAN_POINT ( 'NONE',  ( 0.3917322834645669549, 0.1049643490035304660, -2.793963254593175183 ) ) ;
#50322 = CARTESIAN_POINT ( 'NONE',  ( 1.253280839895013710, -0.3162353388693405765, 0.4822834645669290543 ) ) ;
#50323 = CARTESIAN_POINT ( 'NONE',  ( -1.023622047244093558, -0.1870078740157479769, 0.4822834645669291653 ) ) ;
#50324 = CARTESIAN_POINT ( 'NONE',  ( -0.1265901696524986964, -0.4724409448818899238, -0.6213910761154856077 ) ) ;
#50325 = CARTESIAN_POINT ( 'NONE',  ( -0.5183727034120726440, -0.6692913385826773087, -0.1292274648535924053 ) ) ;
#50326 = CARTESIAN_POINT ( 'NONE',  ( -0.3280839895013117347, 0.05413385826771626580, -0.4176697321401330321 ) ) ;
#50327 = CARTESIAN_POINT ( 'NONE',  ( 1.397637795275591177, 0.07958543189024071263, -0.2665933059059888421 ) ) ;
#50328 = VECTOR ( 'NONE', #59274, 39.37007874015748143 ) ;
#50329 = CARTESIAN_POINT ( 'NONE',  ( 0.1902887139107617975, 0.1771653543307087630, 0.09757992244046791164 ) ) ;
#50330 = CARTESIAN_POINT ( 'NONE',  ( -0.07217847769028813698, -0.3162353388693409650, -0.4822834645669289433 ) ) ;
#50331 = CARTESIAN_POINT ( 'NONE',  ( -1.010498687664041384, 0.05413385826771666132, 0.4176697321401328100 ) ) ;
#50332 = DIRECTION ( 'NONE',  ( -0.000000000000000000, -0.000000000000000000, -1.000000000000000000 ) ) ;
#50333 = CARTESIAN_POINT ( 'NONE',  ( 1.666666666666667185, -0.004921259842519576551, 0.3153832671262227771 ) ) ;
#50334 = CARTESIAN_POINT ( 'NONE',  ( -0.3215223097112853146, -0.05778040916215560624, -0.4822834645669293319 ) ) ;
#50335 = CARTESIAN_POINT ( 'NONE',  ( -0.9645669291338575535, -0.5400638737290844871, 0.3530559997133364547 ) ) ;
#50336 = ORIENTED_EDGE ( 'NONE', *, *, #40513, .F. ) ;
#50337 = CARTESIAN_POINT ( 'NONE',  ( -0.1070741851644051862, -0.3996062992125986590, -1.881233595800524849 ) ) ;
#50338 = CARTESIAN_POINT ( 'NONE',  ( 1.358267716535433323, -0.5400638737290845981, -0.3530559997133363437 ) ) ;
#50339 = CARTESIAN_POINT ( 'NONE',  ( -0.5577427821522301654, -0.08942795157528024563, -0.3641732283464568787 ) ) ;
#50340 = CARTESIAN_POINT ( 'NONE',  ( -0.4593175853018366950, 0.05413385826771666132, 0.4176697321401328100 ) ) ;
#50341 = CARTESIAN_POINT ( 'NONE',  ( 1.200787401574803681, 0.1660481256975885056, 0.3530559997133364547 ) ) ;
#50342 = CARTESIAN_POINT ( 'NONE',  ( 0.7611548556430454138, 0.2306618581243847221, -0.2411417322834647770 ) ) ;
#50343 = CARTESIAN_POINT ( 'NONE',  ( 0.2362204724409451007, -0.4091458600556402980, -0.09186351706036745279 ) ) ;
#50344 = CARTESIAN_POINT ( 'NONE',  ( -1.122047244094487306, -0.4536011799217367080, 0.2665933059059888421 ) ) ;
#50345 = CARTESIAN_POINT ( 'NONE',  ( 0.1070741851644054637, -0.3996062992125984925, -0.7919947506561678674 ) ) ;
#50346 = CARTESIAN_POINT ( 'NONE',  ( 0.1070741851644053527, 0.3996062992125986590, -0.9383202099737533164 ) ) ;
#50347 = CARTESIAN_POINT ( 'NONE',  ( -0.2891555358219908833, -0.2891555358219912164, -0.2165354330708662567 ) ) ;
#50348 = CARTESIAN_POINT ( 'NONE',  ( 0.2406358745268415145, 1.128551111081926850, -1.544744577296102150 ) ) ;
#50349 = CARTESIAN_POINT ( 'NONE',  ( 1.246719160104987623, -0.004921259842519870586, -0.3153832671262229437 ) ) ;
#50350 = CARTESIAN_POINT ( 'NONE',  ( 0.8923884514435701520, -0.5023911411419708095, -0.1820866141732282451 ) ) ;
#50351 = CARTESIAN_POINT ( 'NONE',  ( 0.5905511811023629321, -0.6692913385826771977, 8.415575281601705876E-17 ) ) ;
#50352 = CARTESIAN_POINT ( 'NONE',  ( 1.522309711286089939, -0.6046776061558809534, -0.2411417322834644161 ) ) ;
#50353 = CARTESIAN_POINT ( 'NONE',  ( -0.3949938075777411073, 0.1058382717557497660, -1.211942257217847763 ) ) ;
#50354 = CARTESIAN_POINT ( 'NONE',  ( 0.9383202099737538715, -0.08942795157528024563, -0.3641732283464568787 ) ) ;
#50355 = EDGE_CURVE ( 'NONE', #54650, #60631, #22662, .T. ) ;
#50356 = CARTESIAN_POINT ( 'NONE',  ( -0.2755905511811015396, -0.6692913385826771977, 8.415575281601705876E-17 ) ) ;
#50357 = CARTESIAN_POINT ( 'NONE',  ( -1.161417322834644716, 0.1660481256975885056, 0.3530559997133364547 ) ) ;
#50358 = CARTESIAN_POINT ( 'NONE',  ( 1.318897637795276356, -0.5400638737290844871, 0.3530559997133364547 ) ) ;
#50359 = CARTESIAN_POINT ( 'NONE',  ( -0.1265901696524986964, -0.4724409448818899238, -1.804461942257217677 ) ) ;
#50360 = CARTESIAN_POINT ( 'NONE',  ( -0.3996062992125985480, -0.1070741851644057135, -2.565616797900262647 ) ) ;
#50361 = CARTESIAN_POINT ( 'NONE',  ( -0.08530183727034056085, -0.08942795157528024563, -0.3641732283464568787 ) ) ;
#50362 = ORIENTED_EDGE ( 'NONE', *, *, #53188, .T. ) ;
#50363 = EDGE_LOOP ( 'NONE', ( #6284, #3791, #59709, #25484, #17211, #60204, #70375, #48302, #38236, #52029 ) ) ;
#50364 = EDGE_CURVE ( 'NONE', #78262, #50071, #15285, .T. ) ;
#50365 = CARTESIAN_POINT ( 'NONE',  ( -0.8858267716535425107, 0.1660481256975883668, -0.3530559997133364547 ) ) ;
#50366 = CARTESIAN_POINT ( 'NONE',  ( -0.4265091863517051496, -0.6692913385826771977, 0.1292274648535927661 ) ) ;
#50367 = CARTESIAN_POINT ( 'NONE',  ( -0.1968503937007867743, 0.2952755905511811885, 0.000000000000000000 ) ) ;
#50368 = CARTESIAN_POINT ( 'NONE',  ( 0.4461942257217856311, 0.2306618581243847221, -0.2411417322834647770 ) ) ;
#50369 = CARTESIAN_POINT ( 'NONE',  ( -0.4461942257217840213, -0.6046776061558809534, -0.2411417322834644161 ) ) ;
#50370 = CARTESIAN_POINT ( 'NONE',  ( -1.515748031496062076, -0.5400638737290844871, 0.3530559997133364547 ) ) ;
#50371 = CARTESIAN_POINT ( 'NONE',  ( -0.8595800524934373854, -0.3162353388693409650, -0.4822834645669289433 ) ) ;
#50372 = CARTESIAN_POINT ( 'NONE',  ( 0.6889763779527563470, 0.1660481256975883668, -0.3530559997133364547 ) ) ;
#50373 = CARTESIAN_POINT ( 'NONE',  ( -0.1958661417322834220, -0.3392501089628018884, -1.475065616797900381 ) ) ;
#50374 = CARTESIAN_POINT ( 'NONE',  ( -0.4855643044619415427, -0.004921259842519870586, -0.3153832671262229437 ) ) ;
#50375 = ORIENTED_EDGE ( 'NONE', *, *, #39222, .F. ) ;
#50376 = CARTESIAN_POINT ( 'NONE',  ( 4.837279021331060870E-17, -0.3949938075777409963, -1.496062992125984037 ) ) ;
#50377 = ORIENTED_EDGE ( 'NONE', *, *, #8937, .F. ) ;
#50378 = CARTESIAN_POINT ( 'NONE',  ( -1.345144356955379816, -0.08942795157528024563, -0.3641732283464568787 ) ) ;
#50379 = CARTESIAN_POINT ( 'NONE',  ( -1.043307086614172041, -0.5400638737290844871, 0.3530559997133364547 ) ) ;
#50380 = CARTESIAN_POINT ( 'NONE',  ( -0.7349081364829387342, -0.6046776061558807314, 0.2411417322834647770 ) ) ;
#50381 = CARTESIAN_POINT ( 'NONE',  ( 0.3996062992125986035, 2.446882876249141962E-17, -0.1181102362204724671 ) ) ;
#50382 = CARTESIAN_POINT ( 'NONE',  ( -1.128608923884513837, -0.6046776061558807314, 0.2411417322834647770 ) ) ;
#50383 = CARTESIAN_POINT ( 'NONE',  ( -0.6889763779527552368, -0.5400638737290845981, -0.3530559997133363437 ) ) ;
#50384 = CARTESIAN_POINT ( 'NONE',  ( -1.515748031496062076, -0.5400638737290844871, 0.3530559997133364547 ) ) ;
#50385 = LINE ( 'NONE', #18825, #3923 ) ;
#50386 = CIRCLE ( 'NONE', #49021, 0.2952755905511810774 ) ;
#50387 = CARTESIAN_POINT ( 'NONE',  ( 0.4002624671916016896, -0.08942795157527998196, 0.3641732283464567121 ) ) ;
#50388 = CARTESIAN_POINT ( 'NONE',  ( -0.4835386291766053946, -3.153061149046662969E-15, -0.3954974714151482384 ) ) ;
#50389 = FACE_OUTER_BOUND ( 'NONE', #47576, .T. ) ;
#50390 = CARTESIAN_POINT ( 'NONE',  ( 0.04593175853018440641, 0.1771653543307087075, -0.09757992244046823083 ) ) ;
#50391 = CARTESIAN_POINT ( 'NONE',  ( -0.4068241469816264999, -0.4281496062992124485, 0.4176697321401328655 ) ) ;
#50392 = CARTESIAN_POINT ( 'NONE',  ( 1.528871391076116026, -0.6692913385826773087, -0.1292274648535924053 ) ) ;
#50393 = CARTESIAN_POINT ( 'NONE',  ( -0.1443569553805765515, -0.4281496062992127816, -0.4176697321401328100 ) ) ;
#50394 = VERTEX_POINT ( 'NONE', #49147 ) ;
#50395 = CARTESIAN_POINT ( 'NONE',  ( -0.3996062992125987146, 0.1070741851644051862, -2.080052493438320216 ) ) ;
#50396 = DIRECTION ( 'NONE',  ( -0.000000000000000000, 1.000000000000000000, -0.000000000000000000 ) ) ;
#50397 = ORIENTED_EDGE ( 'NONE', *, *, #29128, .T. ) ;
#50398 = CARTESIAN_POINT ( 'NONE',  ( 0.1998031496062994128, -0.3460692066303957537, -1.743438320209973469 ) ) ;
#50399 = CARTESIAN_POINT ( 'NONE',  ( 1.161417322834646271, 0.1660481256975883668, -0.3530559997133364547 ) ) ;
#50400 = CARTESIAN_POINT ( 'NONE',  ( -1.115485564304461219, -0.3690944881889763329, 0.3153832671262228327 ) ) ;
#50401 = CARTESIAN_POINT ( 'NONE',  ( -1.358267716535432434, 0.1660481256975883668, -0.3530559997133364547 ) ) ;
#50402 = CARTESIAN_POINT ( 'NONE',  ( 0.4724409448818898682, 2.892866454678787531E-17, -0.9055118110236221041 ) ) ;
#50403 = CARTESIAN_POINT ( 'NONE',  ( 2.795275590551181466, 2.244094488188977277, 0.000000000000000000 ) ) ;
#50404 = CARTESIAN_POINT ( 'NONE',  ( -0.1049643490035307020, 0.3917322834645669549, -2.768372703412072866 ) ) ;
#50405 = CARTESIAN_POINT ( 'NONE',  ( 1.351706036745407680, 0.05413385826771666132, 0.4176697321401328100 ) ) ;
#50406 = CARTESIAN_POINT ( 'NONE',  ( -0.1049643490035307020, 0.3917322834645669549, -1.980971128608923992 ) ) ;
#50407 = CARTESIAN_POINT ( 'NONE',  ( 0.1574803149606306130, -0.1870078740157480879, -0.4822834645669291653 ) ) ;
#50408 = CARTESIAN_POINT ( 'NONE',  ( -1.010498687664041384, -0.004921259842519576551, 0.3153832671262227771 ) ) ;
#50409 = CARTESIAN_POINT ( 'NONE',  ( -0.5314960629921254842, -0.5400638737290845981, -0.3530559997133363437 ) ) ;
#50410 = CARTESIAN_POINT ( 'NONE',  ( 0.1070741851644054776, -0.3996062992125984925, 0.1528871391076114805 ) ) ;
#50411 = CARTESIAN_POINT ( 'NONE',  ( -1.076115485564303809, 0.2306618581243848609, 0.2411417322834645549 ) ) ;
#50412 = CARTESIAN_POINT ( 'NONE',  ( -0.3420746716998660508, -0.1974969037888706924, -2.333989501312335957 ) ) ;
#50413 = CARTESIAN_POINT ( 'NONE',  ( 1.108923884514436242, -0.08942795157527998196, 0.3641732283464567121 ) ) ;
#50414 = CARTESIAN_POINT ( 'NONE',  ( -0.1246719160104980823, 0.1771653543307087630, 0.09757992244046791164 ) ) ;
#50415 = CARTESIAN_POINT ( 'NONE',  ( 0.7086614173228353852, -0.1870078740157479769, 0.3641732283464567677 ) ) ;
#50416 = CARTESIAN_POINT ( 'NONE',  ( -1.673228346456691717, 0.1660481256975883668, -0.3530559997133364547 ) ) ;
#50417 = CARTESIAN_POINT ( 'NONE',  ( 0.8561328129276796206, 8.471767977567108961E-16, -0.4445507791589058955 ) ) ;
#50418 = CARTESIAN_POINT ( 'NONE',  ( 0.5643044619422579178, -0.004921259842519576551, 0.3153832671262227771 ) ) ;
#50419 = CARTESIAN_POINT ( 'NONE',  ( -0.7545931758530176614, -0.6692913385826773087, -0.1292274648535924053 ) ) ;
#50420 = CARTESIAN_POINT ( 'NONE',  ( 0.2462293917967310342, -2.191421614605370878E-15, 0.4445507791589071167 ) ) ;
#50421 = CARTESIAN_POINT ( 'NONE',  ( 0.09842519685039434474, 0.07958543189024085140, 0.2665933059059887866 ) ) ;
#50422 = CARTESIAN_POINT ( 'NONE',  ( -1.489501312335957062, -0.2845877964562161244, -0.3641732283464567121 ) ) ;
#50423 = CARTESIAN_POINT ( 'NONE',  ( 0.5839895013123367340, 0.2952755905511811885, 0.1292274648535926551 ) ) ;
#50424 = CARTESIAN_POINT ( 'NONE',  ( -0.3149606299212629468, -5.463695987328517809E-17, 1.076935383196056639 ) ) ;
#50425 = CARTESIAN_POINT ( 'NONE',  ( 1.430446194225722500, -0.004921259842519576551, 0.3153832671262227771 ) ) ;
#50426 = CARTESIAN_POINT ( 'NONE',  ( -1.305774278215222184, -0.6692913385826773087, -0.1292274648535924053 ) ) ;
#50427 = CARTESIAN_POINT ( 'NONE',  ( -0.4199475065616791736, -0.5023911411419708095, 0.1820866141732285504 ) ) ;
#50428 = CARTESIAN_POINT ( 'NONE',  ( -0.3149606299212459048, 2.559055118110236560, -3.937007874015763242 ) ) ;
#50429 = CARTESIAN_POINT ( 'NONE',  ( 0.05905511811023681640, 0.07958543189024071263, -0.2665933059059888421 ) ) ;
#50430 = CARTESIAN_POINT ( 'NONE',  ( -1.351706036745406347, 0.05413385826771626580, -0.4176697321401330321 ) ) ;
#50431 = CARTESIAN_POINT ( 'NONE',  ( -0.6627296587926501115, 0.2952755905511810774, -0.1292274648535930714 ) ) ;
#50432 = CARTESIAN_POINT ( 'NONE',  ( -0.1998031496062991630, -0.3460692066303959202, -0.9297900262467192478 ) ) ;
#50433 = CARTESIAN_POINT ( 'NONE',  ( -0.3917322834645670104, -7.196005306013484475E-17, -2.328740157480315265 ) ) ;
#50434 = CARTESIAN_POINT ( 'NONE',  ( 0.7217847769028878924, -0.3690944881889765550, -0.3153832671262227771 ) ) ;
#50435 = CARTESIAN_POINT ( 'NONE',  ( -0.3740157480314953431, 0.1660481256975885056, 0.3530559997133364547 ) ) ;
#50436 = AXIS2_PLACEMENT_3D ( 'NONE', #8126, #70845, #27469 ) ;
#50437 = CARTESIAN_POINT ( 'NONE',  ( -0.8858267716535425107, -0.5400638737290844871, 0.3530559997133364547 ) ) ;
#50438 = CARTESIAN_POINT ( 'NONE',  ( -0.8989501312335946848, -0.5511811023622046335, 0.09757992244046803654 ) ) ;
#50439 = CARTESIAN_POINT ( 'NONE',  ( -3.937008591613926800, 1.062986170812217024, -0.01541001446542844891 ) ) ;
#50440 = CARTESIAN_POINT ( 'NONE',  ( -0.2493438320209966919, -0.4281496062992124485, 0.4176697321401328655 ) ) ;
#50441 = FACE_OUTER_BOUND ( 'NONE', #45718, .T. ) ;
#50442 = CARTESIAN_POINT ( 'NONE',  ( 1.561679790026247350, -0.4281496062992124485, 0.4176697321401328655 ) ) ;
#50443 = LINE ( 'NONE', #19294, #21944 ) ;
#50444 = ORIENTED_EDGE ( 'NONE', *, *, #7531, .F. ) ;
#50445 = LINE ( 'NONE', #43712, #20326 ) ;
#50446 = CARTESIAN_POINT ( 'NONE',  ( -1.522309711286088607, 0.2306618581243847221, -0.2411417322834647770 ) ) ;
#50447 = CARTESIAN_POINT ( 'NONE',  ( -0.8858267716535425107, 0.1660481256975883668, -0.3530559997133364547 ) ) ;
#50448 = CARTESIAN_POINT ( 'NONE',  ( -1.502624671916009680, -0.3162353388693405765, 0.4822834645669290543 ) ) ;
#50449 = CARTESIAN_POINT ( 'NONE',  ( 0.3917322834645670104, -0.1049643490035303411, -1.928477690288713742 ) ) ;
#50450 = CARTESIAN_POINT ( 'NONE',  ( 0.1308238996069422677, 0.3698506310978945111, -1.220472440944881942 ) ) ;
#50451 = EDGE_CURVE ( 'NONE', #57855, #62837, #21999, .T. ) ;
#50452 = CARTESIAN_POINT ( 'NONE',  ( 0.7611548556430454138, 0.2306618581243847221, -0.2411417322834647770 ) ) ;
#50453 = CARTESIAN_POINT ( 'NONE',  ( 0.1902887139107617975, -0.6692913385826773087, -0.1292274648535924053 ) ) ;
#50454 = DIRECTION ( 'NONE',  ( 8.673617379884035472E-16, 0.000000000000000000, -1.000000000000000000 ) ) ;
#50455 = CARTESIAN_POINT ( 'NONE',  ( -0.6955380577427815458, 0.05413385826771666132, 0.4176697321401328100 ) ) ;
#50456 = CARTESIAN_POINT ( 'NONE',  ( 1.240157480314961314, -0.4536011799217367080, 0.2665933059059888421 ) ) ;
#50457 = CARTESIAN_POINT ( 'NONE',  ( -0.1998031496062994683, 0.3460692066303958092, -0.9580052493438320216 ) ) ;
#50458 = ORIENTED_EDGE ( 'NONE', *, *, #62746, .T. ) ;
#50459 = CARTESIAN_POINT ( 'NONE',  ( 0.3392501089628018329, 0.1958661417322835607, -2.800524934383201714 ) ) ;
#50460 = ORIENTED_EDGE ( 'NONE', *, *, #72282, .T. ) ;
#50461 = CARTESIAN_POINT ( 'NONE',  ( 0.6036745406824153282, -0.6046776061558807314, 0.2411417322834647770 ) ) ;
#50462 = CARTESIAN_POINT ( 'NONE',  ( -0.8530183727034112984, -0.4281496062992127816, -0.4176697321401328100 ) ) ;
#50463 = CARTESIAN_POINT ( 'NONE',  ( -1.646981627296586703, -0.05778040916215522460, 0.4822834645669289988 ) ) ;
#50464 = CARTESIAN_POINT ( 'NONE',  ( 0.6233595800524942554, -0.05778040916215560624, -0.4822834645669293319 ) ) ;
#50465 = CARTESIAN_POINT ( 'NONE',  ( 1.482939632545932307, -0.4281496062992124485, 0.4176697321401328655 ) ) ;
#50466 = CARTESIAN_POINT ( 'NONE',  ( 1.345144356955381593, -0.3162353388693409650, -0.4822834645669289433 ) ) ;
#50467 = CARTESIAN_POINT ( 'NONE',  ( 0.1246719160104994284, 0.2952755905511810774, -0.1292274648535930714 ) ) ;
#50468 = CARTESIAN_POINT ( 'NONE',  ( -1.069553805774277722, -0.6692913385826773087, -0.1292274648535924053 ) ) ;
#50469 = CARTESIAN_POINT ( 'NONE',  ( -1.220472440944881054, 0.4405861044731111953, 0.5309055118110237448 ) ) ;
#50470 = CARTESIAN_POINT ( 'NONE',  ( 0.4607143505782487214, 1.423150415408461544, -2.585258496787425919 ) ) ;
#50471 = CARTESIAN_POINT ( 'NONE',  ( -0.3917322834645669549, -0.1049643490035306603, -0.1955380577427821009 ) ) ;
#50472 = CARTESIAN_POINT ( 'NONE',  ( 0.7480314960629927956, 0.1771653543307087630, 0.000000000000000000 ) ) ;
#50473 = ORIENTED_EDGE ( 'NONE', *, *, #25974, .T. ) ;
#50474 = CARTESIAN_POINT ( 'NONE',  ( -0.2891555358219911054, 0.2891555358219909388, -0.01968503937007880233 ) ) ;
#50475 = VERTEX_POINT ( 'NONE', #30206 ) ;
#50476 = CARTESIAN_POINT ( 'NONE',  ( -0.04593175853018302557, -0.5511811023622048555, -0.09757992244046775898 ) ) ;
#50477 = DIRECTION ( 'NONE',  ( 0.000000000000000000, 0.000000000000000000, -1.000000000000000000 ) ) ;
#50478 = CARTESIAN_POINT ( 'NONE',  ( 0.6496062992125991586, 0.1660481256975885056, 0.3530559997133364547 ) ) ;
#50479 = CARTESIAN_POINT ( 'NONE',  ( 0.2362204724409456558, -0.1870078740157480879, -0.4822834645669291653 ) ) ;
#50480 = CARTESIAN_POINT ( 'NONE',  ( -0.5314960629921254842, -0.5400638737290845981, -0.3530559997133363437 ) ) ;
#50481 = CARTESIAN_POINT ( 'NONE',  ( -0.3392501089628019995, 0.1958661417322831999, -1.755268659613860249 ) ) ;
#50482 = CARTESIAN_POINT ( 'NONE',  ( -1.069553805774277722, -0.6692913385826773087, -0.1292274648535924053 ) ) ;
#50483 = CARTESIAN_POINT ( 'NONE',  ( 0.1049643490035304938, -0.3917322834645669549, -2.532152230971127960 ) ) ;
#50484 = CARTESIAN_POINT ( 'NONE',  ( 1.181102362204724976, -0.1870078740157480601, -0.3641732283464567677 ) ) ;
#50485 = CARTESIAN_POINT ( 'NONE',  ( -1.417322834645668772, -0.1870078740157480879, -0.4822834645669291653 ) ) ;
#50486 = CARTESIAN_POINT ( 'NONE',  ( 0.7874015748031503170, -0.1870078740157480879, -0.4822834645669291653 ) ) ;
#50487 = CARTESIAN_POINT ( 'NONE',  ( 1.128608923884515169, -0.6046776061558809534, -0.2411417322834644161 ) ) ;
#50488 = EDGE_CURVE ( 'NONE', #34044, #49485, #39474, .T. ) ;
#50489 = CARTESIAN_POINT ( 'NONE',  ( -0.1070741851644051862, -0.3996062992125987146, -0.8595800524934383846 ) ) ;
#50490 = CARTESIAN_POINT ( 'NONE',  ( -1.358267716535432434, 0.1660481256975883668, -0.3530559997133364547 ) ) ;
#50491 = CARTESIAN_POINT ( 'NONE',  ( 0.1998031496062994128, -0.3460692066303957537, -0.1686351706036745557 ) ) ;
#50492 = CARTESIAN_POINT ( 'NONE',  ( -0.1246719160104980823, 0.2952755905511811885, 0.1292274648535926551 ) ) ;
#50493 = CARTESIAN_POINT ( 'NONE',  ( 0.3996062992125986035, 2.446882876249141962E-17, -2.480314960629921295 ) ) ;
#50494 = CARTESIAN_POINT ( 'NONE',  ( -0.3917322834645670104, -7.196005306013484475E-17, -1.856299212598425230 ) ) ;
#50495 = CIRCLE ( 'NONE', #19624, 3.543307086614173596 ) ;
#50496 = CARTESIAN_POINT ( 'NONE',  ( 1.515748031496063408, 0.1660481256975885056, 0.3530559997133364547 ) ) ;
#50497 = CARTESIAN_POINT ( 'NONE',  ( 0.1640419947506569498, -0.2845877964562161244, -0.3641732283464567121 ) ) ;
#50498 = CARTESIAN_POINT ( 'NONE',  ( 0.7480314960629927956, -0.6692913385826771977, 8.415575281601705876E-17 ) ) ;
#50499 = CARTESIAN_POINT ( 'NONE',  ( 0.4091458600556403535, 0.2362204724409449896, -1.467847769028871596 ) ) ;
#50500 = CARTESIAN_POINT ( 'NONE',  ( 0.1771653543307093182, -0.4536011799217368745, -0.2665933059059886201 ) ) ;
#50501 = CARTESIAN_POINT ( 'NONE',  ( 0.4265091863517067039, -0.6692913385826773087, -0.1292274648535924053 ) ) ;
#50502 = CARTESIAN_POINT ( 'NONE',  ( 0.3949938075777409963, 2.418639510665530743E-17, -1.139763779527559251 ) ) ;
#50503 = CARTESIAN_POINT ( 'NONE',  ( -0.7152230971128602510, -0.05778040916215560624, -0.4822834645669293319 ) ) ;
#50504 = DIRECTION ( 'NONE',  ( -3.491481338843132961E-15, -0.000000000000000000, 1.000000000000000000 ) ) ;
#50505 = CARTESIAN_POINT ( 'NONE',  ( 0.7545931758530188826, -0.5511811023622046335, 0.09757992244046803654 ) ) ;
#50506 = DIRECTION ( 'NONE',  ( 0.000000000000000000, 0.000000000000000000, 1.000000000000000000 ) ) ;
#50507 = CARTESIAN_POINT ( 'NONE',  ( -0.2362204724409442680, -0.1870078740157480879, -0.4822834645669291653 ) ) ;
#50508 = CARTESIAN_POINT ( 'NONE',  ( 0.1706036745406830368, -0.3690944881889765550, -0.3153832671262227771 ) ) ;
#50509 = CARTESIAN_POINT ( 'NONE',  ( -2.808613111760737802, 1.134406187872312843, -0.2508088161067581479 ) ) ;
#50510 = CARTESIAN_POINT ( 'NONE',  ( -0.2099737532808391705, -0.6046776061558809534, -0.2411417322834644161 ) ) ;
#50511 = CARTESIAN_POINT ( 'NONE',  ( 0.3871391076115492380, -0.08942795157528024563, -0.3641732283464568787 ) ) ;
#50512 = CARTESIAN_POINT ( 'NONE',  ( -0.3996062992125985480, -7.340648628747423112E-17, -1.848425196850393748 ) ) ;
#50513 = CARTESIAN_POINT ( 'NONE',  ( 0.4002624671916016896, -0.05778040916215522460, 0.4822834645669289988 ) ) ;
#50514 = ADVANCED_FACE ( 'NONE', ( #23068 ), #51459, .T. ) ;
#50515 = CARTESIAN_POINT ( 'NONE',  ( 1.017060367454068803, -0.2845877964562159024, 0.3641732283464567677 ) ) ;
#50516 = CARTESIAN_POINT ( 'NONE',  ( 0.2165354330708668951, 0.1660481256975883391, -0.3530559997133364547 ) ) ;
#50517 = B_SPLINE_CURVE_WITH_KNOTS ( 'NONE', 3,
 ( #58889, #27733, #46248, #15120 ),
 .UNSPECIFIED., .F., .F.,
 ( 4, 4 ),
 ( 3.210432057746194131E-07, 0.001287787053612155170 ),
 .UNSPECIFIED. ) ;
#50518 = CARTESIAN_POINT ( 'NONE',  ( -0.2821522309711278487, 0.1771653543307087630, 0.09757992244046791164 ) ) ;
#50519 = CARTESIAN_POINT ( 'NONE',  ( -0.7414698162729651543, 0.1771653543307087075, -0.09757992244046823083 ) ) ;
#50520 = CARTESIAN_POINT ( 'NONE',  ( -0.4396325459317577122, -0.6692913385826773087, -0.1292274648535924053 ) ) ;
#50521 = CARTESIAN_POINT ( 'NONE',  ( 0.4068241469816279987, -0.4281496062992127816, -0.4176697321401328100 ) ) ;
#50522 = CARTESIAN_POINT ( 'NONE',  ( 0.7874015748031503170, -0.1870078740157480601, -0.3641732283464567677 ) ) ;
#50523 = CARTESIAN_POINT ( 'NONE',  ( -1.594488188976377563, -0.4536011799217367080, 0.2665933059059888421 ) ) ;
#50524 = CARTESIAN_POINT ( 'NONE',  ( 1.430446194225722500, -0.004921259842519576551, 0.3153832671262227771 ) ) ;
#50525 = CARTESIAN_POINT ( 'NONE',  ( 0.6692913385826778638, -0.6692913385826771977, 8.415575281601705876E-17 ) ) ;
#50526 = CARTESIAN_POINT ( 'NONE',  ( 0.4725434569952585706, 1.494547573005087671, -2.165586928937583977 ) ) ;
#50527 = CARTESIAN_POINT ( 'NONE',  ( -0.4133858267716528645, 0.1660481256975883668, -0.3530559997133364547 ) ) ;
#50528 = CARTESIAN_POINT ( 'NONE',  ( 0.3917322834645669549, 0.1049643490035304660, -0.8392388451443569819 ) ) ;
#50530 = CARTESIAN_POINT ( 'NONE',  ( 0.7414698162729663755, 0.2952755905511811885, 0.1292274648535926551 ) ) ;
#50529 = AXIS2_PLACEMENT_3D ( 'NONE', #7213, #45911, #52648 ) ;
#50531 = AXIS2_PLACEMENT_3D ( 'NONE', #75913, #38420, #55702 ) ;
#50532 = CARTESIAN_POINT ( 'NONE',  ( 0.7152230971128616943, -0.05778040916215522460, 0.4822834645669289988 ) ) ;
#50533 = FACE_BOUND ( 'NONE', #21002, .T. ) ;
#50534 = CARTESIAN_POINT ( 'NONE',  ( 0.3937007874015754361, -0.1870078740157479769, 0.3641732283464567677 ) ) ;
#50535 = CARTESIAN_POINT ( 'NONE',  ( 1.358267716535433323, 0.1660481256975885056, 0.3530559997133364547 ) ) ;
#50536 = CARTESIAN_POINT ( 'NONE',  ( -0.3608923884514428360, -0.5511811023622048555, -0.09757992244046775898 ) ) ;
#50537 = CARTESIAN_POINT ( 'NONE',  ( -0.3608923884514428360, 0.2952755905511811885, 0.1292274648535926551 ) ) ;
#50538 = CARTESIAN_POINT ( 'NONE',  ( 0.2362204724409451007, -0.4091458600556402980, -2.611548556430446144 ) ) ;
#50539 = CARTESIAN_POINT ( 'NONE',  ( 0.2362204724409456558, -0.1870078740157480879, -0.4822834645669291653 ) ) ;
#50540 = CARTESIAN_POINT ( 'NONE',  ( -0.7217847769028863381, -0.4281496062992124485, 0.4176697321401328655 ) ) ;
#50541 = CARTESIAN_POINT ( 'NONE',  ( -0.6692913385826764205, -0.5511811023622047445, 6.969142054262312111E-17 ) ) ;
#50542 = CARTESIAN_POINT ( 'NONE',  ( 0.2690288713910767848, -0.6692913385826773087, -0.1292274648535924053 ) ) ;
#50543 = CARTESIAN_POINT ( 'NONE',  ( -1.253280839895012377, -0.05778040916215522460, 0.4822834645669289988 ) ) ;
#50544 = CARTESIAN_POINT ( 'NONE',  ( -0.4330708661417315697, -0.6692913385826771977, 8.415575281601705876E-17 ) ) ;
#50545 = CARTESIAN_POINT ( 'NONE',  ( -0.4724409448818895907, -0.01881781417526964470, -1.219479340321617311 ) ) ;
#50547 = CARTESIAN_POINT ( 'NONE',  ( 1.450131233595801428, 0.2952755905511811885, 0.1292274648535926551 ) ) ;
#50546 = CARTESIAN_POINT ( 'NONE',  ( -0.9345427628023836863, -4.378520898609941727E-15, 0.4281989832122466977 ) ) ;
#50548 = CARTESIAN_POINT ( 'NONE',  ( 1.581364829396326277, -0.3162353388693409650, -0.4822834645669289433 ) ) ;
#50549 = CARTESIAN_POINT ( 'NONE',  ( 0.2867679344610366554, -0.2867679344610365444, -1.980314960629921073 ) ) ;
#50551 = VECTOR ( 'NONE', #20298, 39.37007874015748143 ) ;
#50550 = CARTESIAN_POINT ( 'NONE',  ( -1.633858267716534529, 0.1660481256975885056, 0.3530559997133364547 ) ) ;
#50552 = CARTESIAN_POINT ( 'NONE',  ( -1.095800524934382292, -0.05778040916215522460, 0.4822834645669289988 ) ) ;
#50553 = CARTESIAN_POINT ( 'NONE',  ( -0.3458507752293909498, 0.3458507752293907833, -0.1771653543307086520 ) ) ;
#50554 = CARTESIAN_POINT ( 'NONE',  ( 0.3949938075777409408, 0.1058382717557500574, -2.644356955380577912 ) ) ;
#50555 = ORIENTED_EDGE ( 'NONE', *, *, #19718, .T. ) ;
#50556 = CARTESIAN_POINT ( 'NONE',  ( 0.1771653543307093182, -0.4536011799217368745, -0.2665933059059886201 ) ) ;
#50557 = CARTESIAN_POINT ( 'NONE',  ( 0.3917322834645670104, -0.1049643490035303411, -1.206036745406823707 ) ) ;
#50558 = CARTESIAN_POINT ( 'NONE',  ( 0.8398950131233602345, 0.2306618581243847221, -0.2411417322834647770 ) ) ;
#50559 = CARTESIAN_POINT ( 'NONE',  ( 0.01966910102760669257, 0.3928700489057007639, -2.755905511811024944 ) ) ;
#50560 = CARTESIAN_POINT ( 'NONE',  ( -0.1265901696524993347, 0.4724409448818896462, -0.8707349081364829102 ) ) ;
#50561 = CARTESIAN_POINT ( 'NONE',  ( -0.6233595800524928121, -0.2845877964562161244, -0.3641732283464567121 ) ) ;
#50562 = CARTESIAN_POINT ( 'NONE',  ( 0.000000000000000000, 0.000000000000000000, 0.1574803149606299191 ) ) ;
#50563 = CARTESIAN_POINT ( 'NONE',  ( 1.069553805774278832, 0.2952755905511810774, -0.1292274648535930714 ) ) ;
#50564 = CARTESIAN_POINT ( 'NONE',  ( 0.8005249343832027131, -0.004921259842519576551, 0.3153832671262227771 ) ) ;
#50565 = CARTESIAN_POINT ( 'NONE',  ( -0.01968503937007793844, 0.1660481256975883668, -0.3530559997133364547 ) ) ;
#50566 = CARTESIAN_POINT ( 'NONE',  ( -0.3917322834645670659, 0.1049643490035301607, -0.9002431514097621879 ) ) ;
#50567 = CARTESIAN_POINT ( 'NONE',  ( -0.5511811023622038563, -0.1870078740157479769, 0.4822834645669291653 ) ) ;
#50568 = CARTESIAN_POINT ( 'NONE',  ( -1.325459317585300889, -0.3690944881889765550, -0.3153832671262227771 ) ) ;
#50569 = CARTESIAN_POINT ( 'NONE',  ( -0.3543307086614165824, -0.6692913385826771977, 8.415575281601705876E-17 ) ) ;
#50570 = CARTESIAN_POINT ( 'NONE',  ( 0.000000000000000000, 2.165354330708661568, 0.000000000000000000 ) ) ;
#50571 = CARTESIAN_POINT ( 'NONE',  ( 0.000000000000000000, 2.755905511811024056, 0.000000000000000000 ) ) ;
#50572 = ORIENTED_EDGE ( 'NONE', *, *, #38397, .T. ) ;
#50573 = CARTESIAN_POINT ( 'NONE',  ( -0.1049643490035307158, 0.3917322834645670104, -2.208024565125671135 ) ) ;
#50574 = CARTESIAN_POINT ( 'NONE',  ( 0.5380577427821529035, -0.4281496062992124485, 0.4176697321401328655 ) ) ;
#50575 = ORIENTED_EDGE ( 'NONE', *, *, #13421, .T. ) ;
#50576 = CARTESIAN_POINT ( 'NONE',  ( -0.8989501312335946848, 0.2952755905511810774, -0.1292274648535930714 ) ) ;
#50577 = CARTESIAN_POINT ( 'NONE',  ( -1.299212598425196097, 0.2952755905511811885, 0.000000000000000000 ) ) ;
#50578 = CARTESIAN_POINT ( 'NONE',  ( 0.5446194225721792126, -0.05778040916215560624, -0.4822834645669293319 ) ) ;
#50579 = CARTESIAN_POINT ( 'NONE',  ( 0.1377952755905518800, 0.1660481256975883668, -0.3530559997133364547 ) ) ;
#50580 = CARTESIAN_POINT ( 'NONE',  ( 0.2867679344610365999, -0.2867679344610365444, -1.600393700787401619 ) ) ;
#50581 = CARTESIAN_POINT ( 'NONE',  ( -0.7217847769028863381, 0.05413385826771626580, -0.4176697321401330321 ) ) ;
#50582 = CARTESIAN_POINT ( 'NONE',  ( -0.2427821522309703550, -0.3162353388693405765, 0.4822834645669290543 ) ) ;
#50583 = CARTESIAN_POINT ( 'NONE',  ( -0.9973753280839886548, 0.2306618581243848609, 0.2411417322834645549 ) ) ;
#50584 = CARTESIAN_POINT ( 'NONE',  ( 0.4396325459317593221, 0.1771653543307087075, -0.09757992244046823083 ) ) ;
#50585 = DIRECTION ( 'NONE',  ( 0.000000000000000000, 1.601283208593975810E-15, -1.000000000000000000 ) ) ;
#50586 = CARTESIAN_POINT ( 'NONE',  ( -0.03937007874015669567, -0.6692913385826771977, 8.415575281601705876E-17 ) ) ;
#50587 = CARTESIAN_POINT ( 'NONE',  ( 0.4724409448818898682, 2.892866454678787531E-17, -0.9822834645669291653 ) ) ;
#50588 = CARTESIAN_POINT ( 'NONE',  ( 0.9645669291338588858, 0.1660481256975885056, 0.3530559997133364547 ) ) ;
#50589 = CARTESIAN_POINT ( 'NONE',  ( -9.594673741351313045E-17, 0.3917322834645670104, -2.669291338582676865 ) ) ;
#50590 = ORIENTED_EDGE ( 'NONE', *, *, #76918, .F. ) ;
#50591 = ORIENTED_EDGE ( 'NONE', *, *, #26304, .T. ) ;
#50592 = CARTESIAN_POINT ( 'NONE',  ( 0.4265091863517067594, 0.2952755905511811885, 0.1292274648535926551 ) ) ;
#50593 = CARTESIAN_POINT ( 'NONE',  ( -0.07217847769028813698, -0.2845877964562161244, -0.3641732283464567121 ) ) ;
#50594 = CIRCLE ( 'NONE', #37156, 0.2165354330708660069 ) ;
#50596 = CARTESIAN_POINT ( 'NONE',  ( 0.4091458600556404646, -0.2362204724409448231, -0.4199475065616797842 ) ) ;
#50595 = CARTESIAN_POINT ( 'NONE',  ( 1.627296587926509996, -0.5023911411419708095, 0.1820866141732285504 ) ) ;
#50597 = CARTESIAN_POINT ( 'NONE',  ( 0.3392501089628018329, 0.1958661417322835607, -1.160761154855643129 ) ) ;
#50598 = CARTESIAN_POINT ( 'NONE',  ( -0.4091458600556405756, 0.2362204724409446288, 0.2119422572178477626 ) ) ;
#50599 = LINE ( 'NONE', #10681, #25702 ) ;
#50600 = CARTESIAN_POINT ( 'NONE',  ( -0.3460692066303960313, 0.1998031496062989965, -2.780183727034120977 ) ) ;
#50601 = CARTESIAN_POINT ( 'NONE',  ( 0.6167979002624678353, -0.4281496062992124485, 0.4176697321401328655 ) ) ;
#50602 = CARTESIAN_POINT ( 'NONE',  ( -1.220472440944881054, -0.6692913385826771977, 8.415575281601705876E-17 ) ) ;
#50603 = CARTESIAN_POINT ( 'NONE',  ( -1.167979002624671470, -0.4281496062992127816, -0.4176697321401328100 ) ) ;
#50604 = CARTESIAN_POINT ( 'NONE',  ( 0.2690288713910767848, -0.6692913385826773087, -0.1292274648535924053 ) ) ;
#50605 = CARTESIAN_POINT ( 'NONE',  ( 1.115485564304462551, 0.05413385826771666132, 0.4176697321401328100 ) ) ;
#50606 = CARTESIAN_POINT ( 'NONE',  ( 1.522309711286089939, 0.1283753931104748280, 0.1820866141732283561 ) ) ;
#50607 = CONTEXT_DEPENDENT_SHAPE_REPRESENTATION ( #28291, #64079 ) ;
#50608 = CARTESIAN_POINT ( 'NONE',  ( 0.7152230971128616943, -0.08942795157527998196, 0.3641732283464567121 ) ) ;
#50609 = CARTESIAN_POINT ( 'NONE',  ( -0.6758530183727028406, 0.2952755905511811885, 0.1292274648535926551 ) ) ;
#50610 = CARTESIAN_POINT ( 'NONE',  ( 0.3460692066303959202, -0.1998031496062991630, -0.6541994750656167090 ) ) ;
#50611 = CARTESIAN_POINT ( 'NONE',  ( -1.633858267716534529, 0.07958543189024085140, 0.2665933059059887866 ) ) ;
#50612 =( BOUNDED_CURVE ( )  B_SPLINE_CURVE ( 2, ( #58099, #32023, #64011, #51782, #57264, #58527, #37921, #44626, #64849, #18977, #50949, #77486, #77907 ),
 .UNSPECIFIED., .F., .F. ) 
 B_SPLINE_CURVE_WITH_KNOTS ( ( 3, 2, 2, 2, 2, 2, 3 ),
 ( 0.2187856400893463393, 0.2196969696969696961, 0.2234848484848484806, 0.2272727272727272652, 0.2310606060606060497, 0.2348484848484848619, 0.2357598144561083298 ),
 .UNSPECIFIED. ) 
 CURVE ( )  GEOMETRIC_REPRESENTATION_ITEM ( )  RATIONAL_B_SPLINE_CURVE ( ( 0.9875488213027530104, 0.9918020599134685922, 1.000000000000000000, 0.9659258262890683122, 1.000000000000000000, 0.9659258262890683122, 1.000000000000000000, 0.9659258262890683122, 1.000000000000000000, 0.9659258262890683122, 1.000000000000000000, 0.9918020599134675930, 0.9875488213027519002 ) ) 
 REPRESENTATION_ITEM ( '' )  );
#50613 = CARTESIAN_POINT ( 'NONE',  ( 0.3917322834645670104, -0.1049643490035303411, -0.4186351706036745557 ) ) ;
#50614 = ADVANCED_FACE ( 'NONE', ( #6372 ), #82571, .F. ) ;
#50616 = DIRECTION ( 'NONE',  ( 1.000000000000000000, 0.000000000000000000, 0.000000000000000000 ) ) ;
#50615 = CARTESIAN_POINT ( 'NONE',  ( 1.246719160104987623, 0.05413385826771626580, -0.4176697321401330321 ) ) ;
#50617 = CARTESIAN_POINT ( 'NONE',  ( -1.410761154855642463, -0.08942795157527998196, 0.3641732283464567121 ) ) ;
#50618 = CARTESIAN_POINT ( 'NONE',  ( 0.01312335958005323398, -0.4281496062992127816, -0.4176697321401328100 ) ) ;
#50619 = CARTESIAN_POINT ( 'NONE',  ( 0.7349081364829402885, -0.5023911411419708095, -0.1820866141732282451 ) ) ;
#50620 = CARTESIAN_POINT ( 'NONE',  ( -1.706036745406823485, 0.1283753931104748280, 0.1820866141732283561 ) ) ;
#50621 = CARTESIAN_POINT ( 'NONE',  ( 0.8727034120734913358, -0.05778040916215522460, 0.4822834645669289988 ) ) ;
#50622 = CARTESIAN_POINT ( 'NONE',  ( 0.2017716535433070613, -0.2017716535433070890, -0.3937007874015748254 ) ) ;
#50623 = CARTESIAN_POINT ( 'NONE',  ( -0.3740157480314953431, -0.4536011799217368745, -0.2665933059059886201 ) ) ;
#50624 = CARTESIAN_POINT ( 'NONE',  ( -0.7742782152230965886, 0.05413385826771666132, 0.4176697321401328100 ) ) ;
#50625 = CARTESIAN_POINT ( 'NONE',  ( 1.397637795275591177, 0.1660481256975883668, -0.3530559997133364547 ) ) ;
#50626 = CARTESIAN_POINT ( 'NONE',  ( -1.187664041994750175, -0.05778040916215560624, -0.4822834645669293319 ) ) ;
#50627 = CARTESIAN_POINT ( 'NONE',  ( 1.181102362204725198, -0.1870078740157479769, 0.4822834645669291653 ) ) ;
#50628 = CARTESIAN_POINT ( 'NONE',  ( 0.2867679344610366554, -0.2867679344610365999, -1.040045562500999443 ) ) ;
#50629 = CARTESIAN_POINT ( 'NONE',  ( -1.286089238845143479, 0.1283753931104746893, -0.1820866141732285504 ) ) ;
#50630 = CARTESIAN_POINT ( 'NONE',  ( 1.028288428836420909, 1.383544431970676447, 0.4490413120122265789 ) ) ;
#50631 = CARTESIAN_POINT ( 'NONE',  ( 0.8464566929133865436, 0.1660481256975883668, -0.3530559997133364547 ) ) ;
#50632 = CARTESIAN_POINT ( 'NONE',  ( -1.157146581871515012E-16, 0.4724409448818898682, -2.438976377952756014 ) ) ;
#50633 = CARTESIAN_POINT ( 'NONE',  ( -1.627296587926508442, -0.6046776061558809534, -0.2411417322834644161 ) ) ;
#50634 = CARTESIAN_POINT ( 'NONE',  ( -1.384514435695537005, -0.5511811023622048555, -0.09757992244046775898 ) ) ;
#50635 = CARTESIAN_POINT ( 'NONE',  ( -0.8202099737532801971, -0.5511811023622046335, 0.09757992244046803654 ) ) ;
#50636 = EDGE_CURVE ( 'NONE', #43843, #17617, #25166, .T. ) ;
#50637 = CARTESIAN_POINT ( 'NONE',  ( 1.443569553805774897, -0.5023911411419708095, -0.1820866141732282451 ) ) ;
#50638 = CARTESIAN_POINT ( 'NONE',  ( -0.3543307086614165824, 0.2952755905511811885, 0.000000000000000000 ) ) ;
#50639 = CARTESIAN_POINT ( 'NONE',  ( 0.04593175853018440641, -0.5511811023622046335, 0.09757992244046803654 ) ) ;
#50640 = CARTESIAN_POINT ( 'NONE',  ( -1.502624671916009680, -0.08942795157528024563, -0.3641732283464568787 ) ) ;
#50641 = CARTESIAN_POINT ( 'NONE',  ( 1.253280839895013710, -0.2845877964562159024, 0.3641732283464567677 ) ) ;
#50642 = CARTESIAN_POINT ( 'NONE',  ( 1.128608923884515169, -0.6046776061558809534, -0.2411417322834644161 ) ) ;
#50643 = CARTESIAN_POINT ( 'NONE',  ( 1.391076115485564868, -0.6046776061558807314, 0.2411417322834647770 ) ) ;
#50644 = CARTESIAN_POINT ( 'NONE',  ( -0.04593175853018302557, 0.1771653543307087630, 0.09757992244046791164 ) ) ;
#50645 = CARTESIAN_POINT ( 'NONE',  ( 0.5839895013123367340, 0.2952755905511811885, 0.1292274648535926551 ) ) ;
#50646 = EDGE_CURVE ( 'NONE', #57846, #57445, #7478, .T. ) ;
#50647 = CARTESIAN_POINT ( 'NONE',  ( 1.174540682414699111, -0.08942795157528024563, -0.3641732283464568787 ) ) ;
#50648 = ORIENTED_EDGE ( 'NONE', *, *, #32070, .T. ) ;
#50650 = AXIS2_PLACEMENT_3D ( 'NONE', #72514, #45568, #27056 ) ;
#50649 = CARTESIAN_POINT ( 'NONE',  ( -1.509186351706035767, -0.4281496062992124485, 0.4176697321401328655 ) ) ;
#50651 = CARTESIAN_POINT ( 'NONE',  ( -1.345144356955379816, -0.3162353388693405765, 0.4822834645669290543 ) ) ;
#50652 = CARTESIAN_POINT ( 'NONE',  ( -0.1049868766404193215, 0.2306618581243847221, -0.2411417322834647770 ) ) ;
#50653 = VECTOR ( 'NONE', #27347, 39.37007874015748143 ) ;
#50654 = CARTESIAN_POINT ( 'NONE',  ( 0.1070741851644053666, 0.3996062992125986035, -0.3083989501312335846 ) ) ;
#50655 = CARTESIAN_POINT ( 'NONE',  ( 0.2925321140481932369, -0.2925321140481931814, -2.537401574803149984 ) ) ;
#50656 = CARTESIAN_POINT ( 'NONE',  ( 0.4461942257217855201, -0.6046776061558807314, 0.2411417322834647770 ) ) ;
#50657 = CARTESIAN_POINT ( 'NONE',  ( 1.246719160104987623, -0.3690944881889763329, 0.3153832671262228327 ) ) ;
#50658 = AXIS2_PLACEMENT_3D ( 'NONE', #43037, #54016, #79727 ) ;
#50659 = AXIS2_PLACEMENT_3D ( 'NONE', #28576, #9639, #67304 ) ;
#50660 = CARTESIAN_POINT ( 'NONE',  ( -0.3280839895013117347, 0.05413385826771626580, -0.4176697321401330321 ) ) ;
#50661 = CARTESIAN_POINT ( 'NONE',  ( 0.3018372703412079971, -0.4281496062992124485, 0.4176697321401328655 ) ) ;
#50662 = CARTESIAN_POINT ( 'NONE',  ( 0.1070741851644053527, 0.3996062992125986590, -2.198162729658792447 ) ) ;
#50663 = CARTESIAN_POINT ( 'NONE',  ( -0.2891555358219911054, 0.2891555358219909388, -1.594488188976378007 ) ) ;
#50664 = CARTESIAN_POINT ( 'NONE',  ( -0.2114499243052200550, 1.112441217203876676, 1.102030475220129535 ) ) ;
#50665 = CARTESIAN_POINT ( 'NONE',  ( 3.264097702071373064, 2.755905511811024056, 0.5314960629921260393 ) ) ;
#50666 = CARTESIAN_POINT ( 'NONE',  ( -0.3917322834645670104, -7.196005306013484475E-17, -0.6614173228346454936 ) ) ;
#50667 = CARTESIAN_POINT ( 'NONE',  ( -0.6955380577427815458, -0.3690944881889765550, -0.3153832671262227771 ) ) ;
#50668 = CARTESIAN_POINT ( 'NONE',  ( -0.9645669291338575535, -0.5400638737290844871, 0.3530559997133364547 ) ) ;
#50669 = CARTESIAN_POINT ( 'NONE',  ( -0.1058382717557497660, -0.3949938075777411073, -2.511154855643044748 ) ) ;
#50670 = EDGE_CURVE ( 'NONE', #49068, #22657, #22529, .T. ) ;
#50671 = CARTESIAN_POINT ( 'NONE',  ( 0.6824146981627303710, -0.6046776061558807314, 0.2411417322834647770 ) ) ;
#50672 = CARTESIAN_POINT ( 'NONE',  ( -1.450131233595799651, 0.2952755905511810774, -0.1292274648535930714 ) ) ;
#50673 = CARTESIAN_POINT ( 'NONE',  ( 0.5971128608923890191, -0.6692913385826771977, 0.1292274648535927661 ) ) ;
#50674 = CYLINDRICAL_SURFACE ( 'NONE', #69035, 1.181102362204724310 ) ;
#50675 = CARTESIAN_POINT ( 'NONE',  ( -0.1070741851644056997, 0.3996062992125986035, -2.053805774278214979 ) ) ;
#50676 = CARTESIAN_POINT ( 'NONE',  ( 1.141392835773559211, 0.3937007874015747699, 1.141392835773562764 ) ) ;
#50677 = CARTESIAN_POINT ( 'NONE',  ( 1.108923884514436242, -0.05778040916215522460, 0.4822834645669289988 ) ) ;
#50678 = CARTESIAN_POINT ( 'NONE',  ( 0.5643044619422579178, -0.4281496062992127816, -0.4176697321401328100 ) ) ;
#50679 = ADVANCED_FACE ( 'NONE', ( #37375 ), #43663, .F. ) ;
#50680 = CARTESIAN_POINT ( 'NONE',  ( 0.8005249343832027131, -0.004921259842519576551, 0.3153832671262227771 ) ) ;
#50681 = CARTESIAN_POINT ( 'NONE',  ( 1.227034120734908917, 0.2952755905511810774, -0.1292274648535930714 ) ) ;
#50682 = CARTESIAN_POINT ( 'NONE',  ( -0.3917322834645670104, -7.196005306013484475E-17, 0.03346456692913377107 ) ) ;
#50683 = CARTESIAN_POINT ( 'NONE',  ( -0.5314960629921348101, 2.742784456114268909, 2.516666439024516144 ) ) ;
#50684 = CARTESIAN_POINT ( 'NONE',  ( 0.7349081364829403995, 0.2306618581243848609, 0.2411417322834645549 ) ) ;
#50685 = CARTESIAN_POINT ( 'NONE',  ( 1.456692913385827515, -0.5511811023622047445, 6.969142054262312111E-17 ) ) ;
#50686 = CARTESIAN_POINT ( 'NONE',  ( -1.122047244094487306, -0.5400638737290844871, 0.3530559997133364547 ) ) ;
#50687 = CARTESIAN_POINT ( 'NONE',  ( -0.9973753280839886548, -0.6046776061558809534, -0.2411417322834644161 ) ) ;
#50688 = CARTESIAN_POINT ( 'NONE',  ( 0.9645669291338588858, 0.1660481256975885056, 0.3530559997133364547 ) ) ;
#50689 = CARTESIAN_POINT ( 'NONE',  ( -0.1958661417322836718, 0.3392501089628017219, -0.7276902887139108378 ) ) ;
#50690 = CARTESIAN_POINT ( 'NONE',  ( 0.1958661417322834775, 0.3392501089628018884, -1.396325459317585338 ) ) ;
#50691 = CARTESIAN_POINT ( 'NONE',  ( -0.3392501089628017219, -0.1958661417322836718, -2.564304461942256808 ) ) ;
#50692 = EDGE_CURVE ( 'NONE', #55882, #55851, #63678, .T. ) ;
#50693 = ORIENTED_EDGE ( 'NONE', *, *, #81557, .F. ) ;
#50694 = CARTESIAN_POINT ( 'NONE',  ( -0.3996062992125986035, -0.1070741851644056997, 0.1115485564304461580 ) ) ;
#50695 = ORIENTED_EDGE ( 'NONE', *, *, #60327, .T. ) ;
#50696 = CARTESIAN_POINT ( 'NONE',  ( 1.640419947506562393, -0.4281496062992124485, 0.4176697321401328655 ) ) ;
#50697 = CARTESIAN_POINT ( 'NONE',  ( 1.227034120734908917, -0.5511811023622046335, 0.09757992244046803654 ) ) ;
#50698 = CARTESIAN_POINT ( 'NONE',  ( 0.2925321140481932369, 0.2925321140481932369, -1.240157480314960647 ) ) ;
#50699 = CARTESIAN_POINT ( 'NONE',  ( 1.417322834645670104, -0.1870078740157480601, -0.3641732283464567677 ) ) ;
#50700 = CARTESIAN_POINT ( 'NONE',  ( -0.3149606299212458493, 2.165354330708661568, -3.937007874015763242 ) ) ;
#50701 = DIRECTION ( 'NONE',  ( 0.000000000000000000, -1.000000000000000000, -0.000000000000000000 ) ) ;
#50702 = CARTESIAN_POINT ( 'NONE',  ( 0.4330708661417329575, 1.568468489416427580, 0.000000000000000000 ) ) ;
#50703 = CARTESIAN_POINT ( 'NONE',  ( 0.1958661417322834775, 0.3392501089628018884, -0.3864829396325459854 ) ) ;
#50704 = CARTESIAN_POINT ( 'NONE',  ( -0.8595800524934373854, -0.08942795157527998196, 0.3641732283464567121 ) ) ;
#50705 = CARTESIAN_POINT ( 'NONE',  ( -1.528871391076114250, 0.1771653543307087075, -0.09757992244046823083 ) ) ;
#50706 = CARTESIAN_POINT ( 'NONE',  ( -1.456692913385826182, 0.2952755905511811885, 0.000000000000000000 ) ) ;
#50707 = CARTESIAN_POINT ( 'NONE',  ( -0.07217847769028813698, -0.3162353388693409650, -0.4822834645669289433 ) ) ;
#50708 = CARTESIAN_POINT ( 'NONE',  ( 1.384514435695538337, -0.6692913385826771977, 0.1292274648535927661 ) ) ;
#50709 = VERTEX_POINT ( 'NONE', #81598 ) ;
#50710 = FACE_OUTER_BOUND ( 'NONE', #40056, .T. ) ;
#50711 = CARTESIAN_POINT ( 'NONE',  ( 5.885823870150372450, 3.916330350904249524, 5.973313079581529017 ) ) ;
#50712 = CARTESIAN_POINT ( 'NONE',  ( -0.4724409448818895907, -0.1265901696524993070, -2.250656167979002920 ) ) ;
#50713 = CARTESIAN_POINT ( 'NONE',  ( 0.000000000000000000, 2.755905511811024056, 0.000000000000000000 ) ) ;
#50714 = CARTESIAN_POINT ( 'NONE',  ( -0.5118110236220466680, 0.1771653543307087630, 0.000000000000000000 ) ) ;
#50715 = TOROIDAL_SURFACE ( 'NONE', #33266, 3.858267716535433323, 0.07874015748031495954 ) ;
#50716 = CARTESIAN_POINT ( 'NONE',  ( -1.220472440944881054, -0.6692913385826771977, 8.415575281601705876E-17 ) ) ;
#50717 = CARTESIAN_POINT ( 'NONE',  ( 0.9645669291338591078, -0.5400638737290845981, -0.3530559997133363437 ) ) ;
#50718 = AXIS2_PLACEMENT_3D ( 'NONE', #49651, #5454, #82483 ) ;
#50719 = EDGE_LOOP ( 'NONE', ( #58118, #20506, #8178, #81664 ) ) ;
#50721 = CARTESIAN_POINT ( 'NONE',  ( -2.787279214012418738, 0.000000000000000000, 0.000000000000000000 ) ) ;
#50720 = CARTESIAN_POINT ( 'NONE',  ( 0.7773926554473647998, 8.471767977567108961E-16, -0.4445507791589058955 ) ) ;
#50722 = CARTESIAN_POINT ( 'NONE',  ( 1.325459317585302665, -0.4281496062992124485, 0.4176697321401328655 ) ) ;
#50723 = CARTESIAN_POINT ( 'NONE',  ( -1.095800524934382292, -0.05778040916215522460, 0.4822834645669289988 ) ) ;
#50724 = CARTESIAN_POINT ( 'NONE',  ( -0.2867679344610364334, -0.2867679344610368219, -0.2965686107273473038 ) ) ;
#50725 = CARTESIAN_POINT ( 'NONE',  ( -0.3215223097112853146, -0.2845877964562159024, 0.3641732283464567677 ) ) ;
#50726 = CARTESIAN_POINT ( 'NONE',  ( -0.2867679344610364334, -0.2867679344610367109, -0.9311023622047244208 ) ) ;
#50727 = CARTESIAN_POINT ( 'NONE',  ( -0.5052493438320203589, 0.1771653543307087075, -0.09757992244046823083 ) ) ;
#50728 = CARTESIAN_POINT ( 'NONE',  ( 0.6824146981627303710, 0.1283753931104746893, -0.1820866141732285504 ) ) ;
#50729 = CARTESIAN_POINT ( 'NONE',  ( 0.06561679790026316017, 0.05413385826771626580, -0.4176697321401330321 ) ) ;
#50730 = CARTESIAN_POINT ( 'NONE',  ( -0.6102362204724400829, -0.4536011799217368745, -0.2665933059059886201 ) ) ;
#50731 = CARTESIAN_POINT ( 'NONE',  ( 0.1049643490035304938, -0.3917322834645669549, -2.912073490813647858 ) ) ;
#50732 = CARTESIAN_POINT ( 'NONE',  ( 1.305774278215223960, 0.2952755905511810774, -0.1292274648535930714 ) ) ;
#50733 = CARTESIAN_POINT ( 'NONE',  ( -1.450131233595799651, 0.2952755905511810774, -0.1292274648535930714 ) ) ;
#50734 = CARTESIAN_POINT ( 'NONE',  ( -0.1265901696524986964, -0.4724409448818899238, -1.408792650918635259 ) ) ;
#50735 = CARTESIAN_POINT ( 'NONE',  ( -0.4986876640419942164, -0.6046776061558807314, 0.2411417322834647770 ) ) ;
#50736 = EDGE_CURVE ( 'NONE', #7519, #1243, #35515, .T. ) ;
#50737 = CARTESIAN_POINT ( 'NONE',  ( -0.9908136482939626788, 0.2952755905511811885, 0.1292274648535926551 ) ) ;
#50738 = CARTESIAN_POINT ( 'NONE',  ( 1.450131233595801428, -0.5511811023622048555, -0.09757992244046775898 ) ) ;
#50739 = CARTESIAN_POINT ( 'NONE',  ( -0.4593175853018366950, -0.004921259842519576551, 0.3153832671262227771 ) ) ;
#50740 = CARTESIAN_POINT ( 'NONE',  ( -0.4593175853018366950, 0.05413385826771666132, 0.4176697321401328100 ) ) ;
#50741 = CARTESIAN_POINT ( 'NONE',  ( -1.240157480314959759, -0.5400638737290845981, -0.3530559997133363437 ) ) ;
#50742 = FACE_OUTER_BOUND ( 'NONE', #42784, .T. ) ;
#50743 = CARTESIAN_POINT ( 'NONE',  ( 1.148293963254593875, -0.5511811023622046335, 0.09757992244046803654 ) ) ;
#50744 = CARTESIAN_POINT ( 'NONE',  ( -0.3412073490813641308, 0.2306618581243847221, -0.2411417322834647770 ) ) ;
#50745 = CARTESIAN_POINT ( 'NONE',  ( -1.128608923884513837, -0.6046776061558807314, 0.2411417322834647770 ) ) ;
#50746 = EDGE_LOOP ( 'NONE', ( #73198, #37434, #26879, #45624 ) ) ;
#50747 = CARTESIAN_POINT ( 'NONE',  ( 0.3996062992125984925, 0.1070741851644054637, -2.248687664041994605 ) ) ;
#50748 = CARTESIAN_POINT ( 'NONE',  ( -0.7677165354330699465, -0.4536011799217368745, -0.2665933059059886201 ) ) ;
#50749 = CARTESIAN_POINT ( 'NONE',  ( 1.246719160104987623, -0.4281496062992124485, 0.4176697321401328655 ) ) ;
#50750 = CARTESIAN_POINT ( 'NONE',  ( -0.8661417322834640276, -0.1870078740157480601, -0.3641732283464567677 ) ) ;
#50751 = CARTESIAN_POINT ( 'NONE',  ( -0.3460692066303960313, 0.1998031496062989965, -1.205380577427821454 ) ) ;
#50752 = CARTESIAN_POINT ( 'NONE',  ( -1.076115485564303809, 0.2306618581243848609, 0.2411417322834645549 ) ) ;
#50753 = CARTESIAN_POINT ( 'NONE',  ( 1.377952755905512472, 0.2952755905511811885, 0.000000000000000000 ) ) ;
#50754 = CARTESIAN_POINT ( 'NONE',  ( 0.7808398950131241190, -0.05778040916215560624, -0.4822834645669293319 ) ) ;
#50755 = CARTESIAN_POINT ( 'NONE',  ( 0.4091458600556404646, -0.2362204724409448231, -0.1049868766404199460 ) ) ;
#50756 = CARTESIAN_POINT ( 'NONE',  ( -1.292650918635170010, -0.5511811023622046335, 0.09757992244046803654 ) ) ;
#50757 = CARTESIAN_POINT ( 'NONE',  ( -0.3460692066303957537, -0.1998031496062994405, -0.6017060367454067915 ) ) ;
#50758 = CARTESIAN_POINT ( 'NONE',  ( -0.3460692066303960868, 0.1998031496062990242, -1.128608923884514503 ) ) ;
#50759 = CARTESIAN_POINT ( 'NONE',  ( 0.3420746716998659953, 0.1974969037888705536, -0.4461942257217848540 ) ) ;
#50760 = CARTESIAN_POINT ( 'NONE',  ( 0.06791843738633827898, 1.067571514150120526, 2.869773448292317397 ) ) ;
#50761 = CARTESIAN_POINT ( 'NONE',  ( 1.364829396325460076, 0.1283753931104748280, 0.1820866141732283561 ) ) ;
#50762 = CARTESIAN_POINT ( 'NONE',  ( 0.8202099737532813073, 0.1771653543307087630, 0.09757992244046791164 ) ) ;
#50763 = CARTESIAN_POINT ( 'NONE',  ( 0.4593175853018379162, -0.4281496062992124485, 0.4176697321401328655 ) ) ;
#50764 = CARTESIAN_POINT ( 'NONE',  ( 0.2686849592492765448, -0.1228903193441468061, 0.1574803149606299191 ) ) ;
#50765 = CARTESIAN_POINT ( 'NONE',  ( 0.3420746716998660508, -0.1974969037888704149, -1.441601049868766804 ) ) ;
#50766 = CARTESIAN_POINT ( 'NONE',  ( 0.8267716535433078384, -0.5511811023622047445, 6.969142054262312111E-17 ) ) ;
#50767 = CARTESIAN_POINT ( 'NONE',  ( -0.2821522309711278487, -0.6692913385826773087, -0.1292274648535924053 ) ) ;
#50768 = CARTESIAN_POINT ( 'NONE',  ( -1.102362204724408601, -0.1870078740157480879, -0.4822834645669291653 ) ) ;
#50769 = CARTESIAN_POINT ( 'NONE',  ( 0.8595800524934390507, -0.3162353388693405765, 0.4822834645669290543 ) ) ;
#50770 = CARTESIAN_POINT ( 'NONE',  ( 0.1265901696524990294, -0.4724409448818896462, -1.660104986876640210 ) ) ;
#50771 = AXIS2_PLACEMENT_3D ( 'NONE', #22722, #3369, #41661 ) ;
#50772 = CARTESIAN_POINT ( 'NONE',  ( 0.2925321140481932369, -0.2925321140481931814, -2.618110236220472675 ) ) ;
#50773 = VERTEX_POINT ( 'NONE', #69365 ) ;
#50774 = VERTEX_POINT ( 'NONE', #42846 ) ;
#50775 = CARTESIAN_POINT ( 'NONE',  ( -1.089238845144356427, 0.05413385826771666132, 0.4176697321401328100 ) ) ;
#50776 = CARTESIAN_POINT ( 'NONE',  ( -0.7677165354330699465, -0.5400638737290845981, -0.3530559997133363437 ) ) ;
#50778 = CARTESIAN_POINT ( 'NONE',  ( -0.7414698162729651543, -0.6692913385826771977, 0.1292274648535927661 ) ) ;
#50777 = CARTESIAN_POINT ( 'NONE',  ( -0.5971128608923877978, -0.5511811023622048555, -0.09757992244046775898 ) ) ;
#50779 = CARTESIAN_POINT ( 'NONE',  ( 0.3018372703412079971, 0.05413385826771626580, -0.4176697321401330321 ) ) ;
#50780 = CARTESIAN_POINT ( 'NONE',  ( -0.6036745406824141069, -0.6046776061558809534, -0.2411417322834644161 ) ) ;
#50781 = CARTESIAN_POINT ( 'NONE',  ( -1.194225721784776262, -0.4281496062992124485, 0.4176697321401328655 ) ) ;
#50782 = CARTESIAN_POINT ( 'NONE',  ( -0.8923884514435688198, 0.2306618581243847221, -0.2411417322834647770 ) ) ;
#50783 = CARTESIAN_POINT ( 'NONE',  ( 0.7677165354330716118, -0.5400638737290844871, 0.3530559997133364547 ) ) ;
#50784 = CARTESIAN_POINT ( 'NONE',  ( -0.3917322834645670104, -7.196005306013484475E-17, -1.291338582677165503 ) ) ;
#50785 = CARTESIAN_POINT ( 'NONE',  ( -0.6233595800524928121, -0.2845877964562161244, -0.3641732283464567121 ) ) ;
#50786 = VERTEX_POINT ( 'NONE', #49991 ) ;
#50787 = CARTESIAN_POINT ( 'NONE',  ( 0.3420746716998660508, -0.1974969037888703871, -1.837270341207348556 ) ) ;
#50788 = ORIENTED_EDGE ( 'NONE', *, *, #30484, .T. ) ;
#50789 = CARTESIAN_POINT ( 'NONE',  ( -1.410761154855642463, -0.08942795157527998196, 0.3641732283464567121 ) ) ;
#50790 = CARTESIAN_POINT ( 'NONE',  ( -0.9186351706036736120, -0.6046776061558809534, -0.2411417322834644161 ) ) ;
#50791 = CARTESIAN_POINT ( 'NONE',  ( -0.9908136482939626788, 0.2952755905511811885, 0.1292274648535926551 ) ) ;
#50792 = CARTESIAN_POINT ( 'NONE',  ( -0.1070741851644056997, 0.3996062992125986035, -0.006561679790026256169 ) ) ;
#50793 = CARTESIAN_POINT ( 'NONE',  ( -0.9842519685039365918, -0.6692913385826771977, 8.415575281601705876E-17 ) ) ;
#50794 = CARTESIAN_POINT ( 'NONE',  ( -1.056430446194224881, 0.2952755905511810774, -0.1292274648535930714 ) ) ;
#50795 = FACE_OUTER_BOUND ( 'NONE', #24282, .T. ) ;
#50796 = DIRECTION ( 'NONE',  ( 1.000000000000000000, -0.000000000000000000, -0.000000000000000000 ) ) ;
#50797 = CARTESIAN_POINT ( 'NONE',  ( 0.3937007874015754361, -0.1870078740157479769, 0.3641732283464567677 ) ) ;
#50798 = FACE_OUTER_BOUND ( 'NONE', #1345, .T. ) ;
#50799 = CARTESIAN_POINT ( 'NONE',  ( -0.3392501089628017219, -0.1958661417322836718, 0.1778215223097112108 ) ) ;
#50800 = CARTESIAN_POINT ( 'NONE',  ( -0.5380577427821514602, -0.3690944881889765550, -0.3153832671262227771 ) ) ;
#50801 = CARTESIAN_POINT ( 'NONE',  ( -0.3608923884514428360, 0.2952755905511811885, 0.1292274648535926551 ) ) ;
#50802 = CARTESIAN_POINT ( 'NONE',  ( 1.318897637795276356, 0.1660481256975883668, -0.3530559997133364547 ) ) ;
#50803 = CARTESIAN_POINT ( 'NONE',  ( -0.3805774278215216522, 0.05413385826771666132, 0.4176697321401328100 ) ) ;
#50804 = ORIENTED_EDGE ( 'NONE', *, *, #62891, .F. ) ;
#50805 = ORIENTED_EDGE ( 'NONE', *, *, #2022, .T. ) ;
#50806 = CARTESIAN_POINT ( 'NONE',  ( -0.1998031496062991630, -0.3460692066303959202, -1.559711286089238591 ) ) ;
#50807 = CARTESIAN_POINT ( 'NONE',  ( -0.4396325459317577122, -0.6692913385826773087, -0.1292274648535924053 ) ) ;
#50808 = CARTESIAN_POINT ( 'NONE',  ( 1.345144356955381593, -0.3162353388693409650, -0.4822834645669289433 ) ) ;
#50809 = CARTESIAN_POINT ( 'NONE',  ( -1.128608923884513837, -0.5023911411419708095, 0.1820866141732285504 ) ) ;
#50810 = CARTESIAN_POINT ( 'NONE',  ( -1.482939632545930975, -0.4281496062992127816, -0.4176697321401328100 ) ) ;
#50811 = CARTESIAN_POINT ( 'NONE',  ( -0.1265901696524993347, 0.4724409448818895907, -0.9514435695538056015 ) ) ;
#50812 = CARTESIAN_POINT ( 'NONE',  ( 1.813482582612293559, 2.755905511811024056, -0.5314960629921260393 ) ) ;
#50813 = CARTESIAN_POINT ( 'NONE',  ( 0.2867679344610365999, 0.2867679344610365999, -2.742125984251967630 ) ) ;
#50814 = CARTESIAN_POINT ( 'NONE',  ( 1.213910761154856299, 0.2952755905511811885, 0.1292274648535926551 ) ) ;
#50815 = CARTESIAN_POINT ( 'NONE',  ( 0.3392501089628018329, 0.1958661417322835607, -2.105643044619422533 ) ) ;
#50816 = CARTESIAN_POINT ( 'NONE',  ( 0.006561679790026889343, -0.3162353388693409650, -0.4822834645669289433 ) ) ;
#50817 = CARTESIAN_POINT ( 'NONE',  ( -1.062992125984250968, -0.5511811023622047445, 6.969142054262312111E-17 ) ) ;
#50818 = CARTESIAN_POINT ( 'NONE',  ( -0.3608923884514428360, -0.6692913385826773087, -0.1292274648535924053 ) ) ;
#50819 = CARTESIAN_POINT ( 'NONE',  ( 0.4091458600556404646, -0.2362204724409448231, -2.701443569553806157 ) ) ;
#50820 = CARTESIAN_POINT ( 'NONE',  ( -0.8661417322834640276, -0.1870078740157480879, -0.4822834645669291653 ) ) ;
#50821 = CARTESIAN_POINT ( 'NONE',  ( -0.8398950131233589023, -0.6046776061558809534, -0.2411417322834644161 ) ) ;
#50822 = CARTESIAN_POINT ( 'NONE',  ( 4.837279021331061486E-17, -0.3949938075777409963, -2.045275590551181022 ) ) ;
#50823 = CARTESIAN_POINT ( 'NONE',  ( 0.8464566929133865436, 0.07958543189024071263, -0.2665933059059888421 ) ) ;
#50824 = CARTESIAN_POINT ( 'NONE',  ( -0.4068241469816267775, -0.004921259842519870586, -0.3153832671262229437 ) ) ;
#50825 = CARTESIAN_POINT ( 'NONE',  ( 0.6758530183727039509, -0.5511811023622046335, 0.09757992244046803654 ) ) ;
#50826 = CARTESIAN_POINT ( 'NONE',  ( -1.456692913385826182, -0.6692913385826771977, 8.415575281601705876E-17 ) ) ;
#50827 = CARTESIAN_POINT ( 'NONE',  ( 1.482939632545932307, 0.05413385826771626580, -0.4176697321401330321 ) ) ;
#50828 = CARTESIAN_POINT ( 'NONE',  ( 0.4461942257217856311, 0.1283753931104746893, -0.1820866141732285504 ) ) ;
#50829 = CARTESIAN_POINT ( 'NONE',  ( -0.8464566929133852113, 0.1660481256975885056, 0.3530559997133364547 ) ) ;
#50830 = CARTESIAN_POINT ( 'NONE',  ( 1.312335958005249825, 0.2306618581243847221, -0.2411417322834647770 ) ) ;
#50831 = CONICAL_SURFACE ( 'NONE', #14415, 1.181102362204724310, 0.7853981633974621568 ) ;
#50832 = CARTESIAN_POINT ( 'NONE',  ( 0.4724409448818896462, 0.1265901696524990294, 0.1135170603674540563 ) ) ;
#50833 = CARTESIAN_POINT ( 'NONE',  ( 0.01312335958005323398, -0.3690944881889765550, -0.3153832671262227771 ) ) ;
#50834 = DIRECTION ( 'NONE',  ( 9.929802617766423249E-17, -0.7071067811865507924, -0.7071067811865442421 ) ) ;
#50835 = EDGE_CURVE ( 'NONE', #28101, #7205, #18042, .T. ) ;
#50836 = CARTESIAN_POINT ( 'NONE',  ( 0.1509186351706045259, -0.05778040916215560624, -0.4822834645669293319 ) ) ;
#50837 = CARTESIAN_POINT ( 'NONE',  ( -1.948818897637795367, 0.000000000000000000, 5.544487991299990703 ) ) ;
#50838 = CARTESIAN_POINT ( 'NONE',  ( 1.502624671916010790, -0.2845877964562161244, -0.3641732283464567121 ) ) ;
#50839 = CARTESIAN_POINT ( 'NONE',  ( 0.06561679790026316017, -0.004921259842519870586, -0.3153832671262229437 ) ) ;
#50840 = CARTESIAN_POINT ( 'NONE',  ( -1.233595800524933894, 0.2306618581243848609, 0.2411417322834645549 ) ) ;
#50841 = CARTESIAN_POINT ( 'NONE',  ( -0.4921259842519677963, 0.07958543189024071263, -0.2665933059059888421 ) ) ;
#50842 = DIRECTION ( 'NONE',  ( 0.000000000000000000, 0.000000000000000000, -1.000000000000000000 ) ) ;
#50843 = CARTESIAN_POINT ( 'NONE',  ( -1.259842519685038686, -0.1870078740157479769, 0.4822834645669291653 ) ) ;
#50844 = CARTESIAN_POINT ( 'NONE',  ( -0.3149606299212590610, -0.1870078740157480879, -0.4822834645669291653 ) ) ;
#50845 = CARTESIAN_POINT ( 'NONE',  ( -0.3996062992125986590, 0.1070741851644051723, -0.7395013123359580609 ) ) ;
#50846 = CARTESIAN_POINT ( 'NONE',  ( 0.2867679344610365999, -0.2867679344610365444, -2.230314960629921295 ) ) ;
#50847 = CARTESIAN_POINT ( 'NONE',  ( 0.7283464566929140904, -0.4536011799217368745, -0.2665933059059886201 ) ) ;
#50848 = CARTESIAN_POINT ( 'NONE',  ( -0.5708661417322825615, -0.5400638737290844871, 0.3530559997133364547 ) ) ;
#50849 = CARTESIAN_POINT ( 'NONE',  ( -0.6889763779527552368, 0.1660481256975885056, 0.3530559997133364547 ) ) ;
#50850 = CARTESIAN_POINT ( 'NONE',  ( -0.6036745406824141069, -0.5023911411419708095, -0.1820866141732282451 ) ) ;
#50851 = DIRECTION ( 'NONE',  ( 0.000000000000000000, 1.000000000000000000, -1.734723475976805862E-16 ) ) ;
#50852 = CARTESIAN_POINT ( 'NONE',  ( 0.05249343832021075018, -0.6046776061558807314, 0.2411417322834647770 ) ) ;
#50853 = CARTESIAN_POINT ( 'NONE',  ( -1.482939632545930975, -0.3690944881889765550, -0.3153832671262227771 ) ) ;
#50854 = CARTESIAN_POINT ( 'NONE',  ( 1.423884514435696191, -0.05778040916215522460, 0.4822834645669289988 ) ) ;
#50855 = CARTESIAN_POINT ( 'NONE',  ( 0.4091458600556404646, -0.2362204724409448231, -0.7349081364829396223 ) ) ;
#50856 = CARTESIAN_POINT ( 'NONE',  ( 0.3917322834645670104, 0.1049643490035304660, -2.168654486385513724 ) ) ;
#50857 = ORIENTED_EDGE ( 'NONE', *, *, #46912, .F. ) ;
#50858 = CARTESIAN_POINT ( 'NONE',  ( -0.7461015444985823475, 1.969952063678500842, 0.5309055118110236338 ) ) ;
#50859 = CARTESIAN_POINT ( 'NONE',  ( -1.220472440944881054, 0.2952755905511811885, 0.000000000000000000 ) ) ;
#50860 = CARTESIAN_POINT ( 'NONE',  ( -0.8923884514435688198, 0.2306618581243847221, -0.2411417322834647770 ) ) ;
#50861 = CARTESIAN_POINT ( 'NONE',  ( -1.437007874015747477, 0.1660481256975883668, -0.3530559997133364547 ) ) ;
#50862 = CARTESIAN_POINT ( 'NONE',  ( -0.2867679344610364334, -0.2867679344610367109, -2.033464566929133355 ) ) ;
#50863 = CARTESIAN_POINT ( 'NONE',  ( -0.3078094465263064294, 0.2432155562301229479, -1.220472440944882164 ) ) ;
#50864 = CARTESIAN_POINT ( 'NONE',  ( 1.062992125984252745, 0.2952755905511811885, 0.000000000000000000 ) ) ;
#50865 = CARTESIAN_POINT ( 'NONE',  ( -0.08530183727034056085, -0.3162353388693405765, 0.4822834645669290543 ) ) ;
#50866 = CARTESIAN_POINT ( 'NONE',  ( -1.313877454013331780, 0.2929341459200028863, 0.8967544760595741460 ) ) ;
#50867 = CARTESIAN_POINT ( 'NONE',  ( 4.893765752498283308E-17, -0.3996062992125985480, -2.675196850393700920 ) ) ;
#50868 = CARTESIAN_POINT ( 'NONE',  ( 1.017060367454068581, -0.08942795157528024563, -0.3641732283464568787 ) ) ;
#50869 = CARTESIAN_POINT ( 'NONE',  ( 0.3460692066303959757, -0.1998031496062991907, -1.522309711286089273 ) ) ;
#50870 = EDGE_LOOP ( 'NONE', ( #40753, #22466, #18801, #19430 ) ) ;
#50871 = CARTESIAN_POINT ( 'NONE',  ( -0.2867679344610365444, -0.2867679344610367664, 0.1016867209635676783 ) ) ;
#50872 = ORIENTED_EDGE ( 'NONE', *, *, #51075, .F. ) ;
#50873 = CARTESIAN_POINT ( 'NONE',  ( 0.3871391076115492380, -0.05778040916215560624, -0.4822834645669293319 ) ) ;
#50874 = CARTESIAN_POINT ( 'NONE',  ( -0.6824146981627291497, -0.6046776061558809534, -0.2411417322834644161 ) ) ;
#50875 = CARTESIAN_POINT ( 'NONE',  ( 1.574803149606299746, -0.1870078740157479769, 0.4822834645669291653 ) ) ;
#50876 = CARTESIAN_POINT ( 'NONE',  ( 0.4724409448818904789, -0.1870078740157480879, -0.4822834645669291653 ) ) ;
#50877 = CARTESIAN_POINT ( 'NONE',  ( 1.502624671916010790, -0.05778040916215522460, 0.4822834645669289988 ) ) ;
#50878 = CARTESIAN_POINT ( 'NONE',  ( 1.410761154855643795, -0.3162353388693405765, 0.4822834645669290543 ) ) ;
#50879 = CARTESIAN_POINT ( 'NONE',  ( -0.03280839895013062252, 0.2952755905511810774, -0.1292274648535930714 ) ) ;
#50880 = CARTESIAN_POINT ( 'NONE',  ( -1.351706036745406347, -0.4281496062992124485, 0.4176697321401328655 ) ) ;
#50881 = CARTESIAN_POINT ( 'NONE',  ( 1.463254593175853824, 0.2952755905511810774, -0.1292274648535930714 ) ) ;
#50882 = CARTESIAN_POINT ( 'NONE',  ( 1.482939632545932307, -0.4281496062992124485, 0.4176697321401328655 ) ) ;
#50883 = CARTESIAN_POINT ( 'NONE',  ( -0.2867679344610364334, -0.2867679344610367109, -0.05118110236220468900 ) ) ;
#50884 = CARTESIAN_POINT ( 'NONE',  ( 0.9514435695538062676, -0.2845877964562161244, -0.3641732283464567121 ) ) ;
#50885 = ORIENTED_EDGE ( 'NONE', *, *, #70415, .T. ) ;
#50886 = CARTESIAN_POINT ( 'NONE',  ( -0.3420746716998659953, -0.1974969037888706647, -0.05249343832021002854 ) ) ;
#50887 = VERTEX_POINT ( 'NONE', #49164 ) ;
#50888 = CARTESIAN_POINT ( 'NONE',  ( 0.1706036745406830368, -0.004921259842519576551, 0.3153832671262227771 ) ) ;
#50889 = CARTESIAN_POINT ( 'NONE',  ( 0.4724409448818898682, 0.000000000000000000, -2.755905511811024056 ) ) ;
#50890 = CARTESIAN_POINT ( 'NONE',  ( 0.09842519685039434474, -0.5400638737290845981, -0.3530559997133363437 ) ) ;
#50891 = CARTESIAN_POINT ( 'NONE',  ( 0.5183727034120741983, 0.2952755905511810774, -0.1292274648535930714 ) ) ;
#50892 = CARTESIAN_POINT ( 'NONE',  ( -0.3871391076115479057, -0.3162353388693409650, -0.4822834645669289433 ) ) ;
#50893 = CARTESIAN_POINT ( 'NONE',  ( 0.3917322834645670659, -0.1049643490035303273, -1.683090181923571294 ) ) ;
#50894 = CARTESIAN_POINT ( 'NONE',  ( -1.023622047244093558, -0.1870078740157479769, 0.4822834645669291653 ) ) ;
#50895 = CARTESIAN_POINT ( 'NONE',  ( 0.3392501089628018329, 0.1958661417322835607, -2.735564304461941987 ) ) ;
#50896 = CARTESIAN_POINT ( 'NONE',  ( 1.187664041994751285, -0.2845877964562161244, -0.3641732283464567121 ) ) ;
#50897 = CARTESIAN_POINT ( 'NONE',  ( 0.8333333333333340365, -0.6692913385826771977, 0.1292274648535927661 ) ) ;
#50898 = CARTESIAN_POINT ( 'NONE',  ( 0.6561679790026253567, -0.6046776061558809534, -0.2411417322834644161 ) ) ;
#50899 = CARTESIAN_POINT ( 'NONE',  ( -0.3996062992125986035, -7.340648628747425578E-17, -0.8267716535433070613 ) ) ;
#50900 = CARTESIAN_POINT ( 'NONE',  ( -1.318897637795274802, -0.5400638737290845981, -0.3530559997133363437 ) ) ;
#50901 = CARTESIAN_POINT ( 'NONE',  ( -0.1998031496062991630, -0.3460692066303959202, -0.2998687664041995160 ) ) ;
#50902 = CARTESIAN_POINT ( 'NONE',  ( -9.787531504996566615E-17, 0.3996062992125985480, -0.07677165354330711677 ) ) ;
#50903 = CARTESIAN_POINT ( 'NONE',  ( -0.05905511811023545637, -0.5400638737290845981, -0.3530559997133363437 ) ) ;
#50904 = CARTESIAN_POINT ( 'NONE',  ( 0.1998031496062994405, -0.3460692066303958092, -2.611548556430446144 ) ) ;
#50905 = CARTESIAN_POINT ( 'NONE',  ( 0.3917322834645669549, 0.1049643490035304660, -1.784120734908136274 ) ) ;
#50906 = CARTESIAN_POINT ( 'NONE',  ( 1.397637795275591177, -0.5400638737290844871, 0.3530559997133364547 ) ) ;
#50907 = CARTESIAN_POINT ( 'NONE',  ( 1.469816272965879911, -0.6046776061558807314, 0.2411417322834647770 ) ) ;
#50908 = CARTESIAN_POINT ( 'NONE',  ( 0.05249343832021075018, -0.5023911411419708095, 0.1820866141732285504 ) ) ;
#50909 = CARTESIAN_POINT ( 'NONE',  ( 0.9383202099737536495, -0.3162353388693405765, 0.4822834645669290543 ) ) ;
#50910 = CARTESIAN_POINT ( 'NONE',  ( -0.4091458600556405756, 0.2362204724409446288, -1.520341207349081181 ) ) ;
#50911 = CARTESIAN_POINT ( 'NONE',  ( 0.2624671916010504757, 0.1283753931104748280, 0.1820866141732283561 ) ) ;
#50912 = CARTESIAN_POINT ( 'NONE',  ( 0.2296587926509192634, -0.05778040916215560624, -0.4822834645669293319 ) ) ;
#50913 = B_SPLINE_CURVE_WITH_KNOTS ( 'NONE', 3,
 ( #25988, #70610, #62759, #11418, #64300, #32306, #51647, #81720, #57967, #38622, #29930, #12965, #30343, #42560, #45341, #42966, #334, #77351, #56424, #36256, #64717, #62333, #19683, #71037 ),
 .UNSPECIFIED., .F., .F.,
 ( 4, 2, 2, 2, 2, 2, 2, 2, 2, 2, 2, 4 ),
 ( 0.008892801244818756071, 0.009319797321957692601, 0.009746793399096627397, 0.01017378947623556393, 0.01060078555337450046, 0.01145477770765237005, 0.01230876986193024138, 0.01316276201620811097, 0.01401675417048598056, 0.01487074632476385189, 0.01529774240190278148, 0.01572473847904171107 ),
 .UNSPECIFIED. ) ;
#50914 = CARTESIAN_POINT ( 'NONE',  ( -0.3420746716998660508, -0.1974969037888706924, -1.074146981627296826 ) ) ;
#50915 = CARTESIAN_POINT ( 'NONE',  ( -1.364829396325458521, 0.2306618581243847221, -0.2411417322834647770 ) ) ;
#50916 = CARTESIAN_POINT ( 'NONE',  ( 1.122047244094488860, 0.07958543189024085140, 0.2665933059059887866 ) ) ;
#50917 = CARTESIAN_POINT ( 'NONE',  ( -2.563288228875834296, 1.597527518877481123, -0.4706608522957235197 ) ) ;
#50918 = CARTESIAN_POINT ( 'NONE',  ( -0.3674540682414692561, -0.6046776061558809534, -0.2411417322834644161 ) ) ;
#50919 = CARTESIAN_POINT ( 'NONE',  ( 0.1115485564304470323, 0.1771653543307087630, 0.09757992244046791164 ) ) ;
#50920 = CARTESIAN_POINT ( 'NONE',  ( 0.4531182788721078158, 1.771653543307086354, 0.5309055118110234117 ) ) ;
#50921 = CARTESIAN_POINT ( 'NONE',  ( -0.3608923884514428360, -0.6692913385826773087, -0.1292274648535924053 ) ) ;
#50922 = CARTESIAN_POINT ( 'NONE',  ( 0.1706036745406830368, -0.004921259842519576551, 0.3153832671262227771 ) ) ;
#50923 = CARTESIAN_POINT ( 'NONE',  ( -0.3996062992125986590, 0.1070741851644051723, -1.999343832020997525 ) ) ;
#50924 = CARTESIAN_POINT ( 'NONE',  ( -0.2165354330708654795, 0.1660481256975885056, 0.3530559997133364547 ) ) ;
#50925 = EDGE_CURVE ( 'NONE', #66357, #43843, #3455, .T. ) ;
#50926 = CARTESIAN_POINT ( 'NONE',  ( 1.062992125984252745, 0.1771653543307087630, 0.000000000000000000 ) ) ;
#50927 = CARTESIAN_POINT ( 'NONE',  ( 1.614173228346457378, 0.2952755905511811885, 0.000000000000000000 ) ) ;
#50928 = AXIS2_PLACEMENT_3D ( 'NONE', #65952, #57937, #77321 ) ;
#50929 = CARTESIAN_POINT ( 'NONE',  ( -0.8070866141732276899, -0.4536011799217367080, 0.2665933059059888421 ) ) ;
#50930 = CARTESIAN_POINT ( 'NONE',  ( -0.6036745406824141069, 0.1283753931104748280, 0.1820866141732283561 ) ) ;
#50931 = CARTESIAN_POINT ( 'NONE',  ( -0.4199475065616791736, -0.6046776061558807314, 0.2411417322834647770 ) ) ;
#50932 = CARTESIAN_POINT ( 'NONE',  ( -0.1771653543307080136, -0.5400638737290844871, 0.3530559997133364547 ) ) ;
#50933 = CARTESIAN_POINT ( 'NONE',  ( 1.082677165354331228, 0.07958543189024071263, -0.2665933059059888421 ) ) ;
#50934 = CARTESIAN_POINT ( 'NONE',  ( 0.1685177960138025954, 1.093661989145994884, -1.109414537943555601 ) ) ;
#50935 = CARTESIAN_POINT ( 'NONE',  ( 1.437007874015748810, 0.07958543189024085140, 0.2665933059059887866 ) ) ;
#50936 = B_SPLINE_CURVE_WITH_KNOTS ( 'NONE', 3,
 ( #48438, #3013, #16482, #60255 ),
 .UNSPECIFIED., .F., .F.,
 ( 4, 4 ),
 ( 0.2143416721067105124, 0.2157535705625736044 ),
 .UNSPECIFIED. ) ;
#50937 = CARTESIAN_POINT ( 'NONE',  ( 0.5446194225721792126, -0.3162353388693405765, 0.4822834645669290543 ) ) ;
#50938 = CARTESIAN_POINT ( 'NONE',  ( -1.603475055217291612, 1.819038169495759361, -0.04573490813648263542 ) ) ;
#50939 = CARTESIAN_POINT ( 'NONE',  ( -0.4527559055118102749, 0.1660481256975885056, 0.3530559997133364547 ) ) ;
#50940 = CARTESIAN_POINT ( 'NONE',  ( 0.1958661417322836440, -0.3392501089628017219, -0.8064304461942258806 ) ) ;
#50941 = CARTESIAN_POINT ( 'NONE',  ( -1.423884514435694859, -0.3162353388693405765, 0.4822834645669290543 ) ) ;
#50942 = CARTESIAN_POINT ( 'NONE',  ( 0.8267716535433078384, -0.6692913385826771977, 8.415575281601705876E-17 ) ) ;
#50943 = CARTESIAN_POINT ( 'NONE',  ( 0.5249343832021005074, -0.6046776061558807314, 0.2411417322834647770 ) ) ;
#50944 = CARTESIAN_POINT ( 'NONE',  ( -0.07763836211493191364, 1.069131175596405026, -3.936271682215574330 ) ) ;
#50945 = CARTESIAN_POINT ( 'NONE',  ( 0.2296587926509192634, -0.2845877964562159024, 0.3641732283464567677 ) ) ;
#50946 = CARTESIAN_POINT ( 'NONE',  ( 1.391076115485564868, 0.2306618581243847221, -0.2411417322834647770 ) ) ;
#50947 = CARTESIAN_POINT ( 'NONE',  ( -0.4593175853018366950, -0.004921259842519576551, 0.3153832671262227771 ) ) ;
#50948 = CARTESIAN_POINT ( 'NONE',  ( -0.7349081364829387342, -0.6046776061558807314, 0.2411417322834647770 ) ) ;
#50949 = CARTESIAN_POINT ( 'NONE',  ( 0.8005249343832027131, 0.05413385826771666132, 0.4176697321401328100 ) ) ;
#50950 = CARTESIAN_POINT ( 'NONE',  ( 0.1509186351706042484, -0.3162353388693405765, 0.4822834645669290543 ) ) ;
#50951 = CARTESIAN_POINT ( 'NONE',  ( -0.9251968503937002541, -0.5400638737290845981, -0.3530559997133363437 ) ) ;
#50952 = CARTESIAN_POINT ( 'NONE',  ( -0.7217847769028863381, -0.004921259842519870586, -0.3153832671262229437 ) ) ;
#50953 = CARTESIAN_POINT ( 'NONE',  ( 0.3740157480314966754, 0.1660481256975883668, -0.3530559997133364547 ) ) ;
#50954 = CARTESIAN_POINT ( 'NONE',  ( -1.443569553805773564, -0.6046776061558807314, 0.2411417322834647770 ) ) ;
#50955 = CARTESIAN_POINT ( 'NONE',  ( -0.1837270341207340729, 0.2306618581243847221, -0.2411417322834647770 ) ) ;
#50957 = CARTESIAN_POINT ( 'NONE',  ( 1.253280839895013710, -0.3162353388693405765, 0.4822834645669290543 ) ) ;
#50956 = DIRECTION ( 'NONE',  ( 1.000000000000000000, -0.000000000000000000, -0.000000000000000000 ) ) ;
#50958 = CARTESIAN_POINT ( 'NONE',  ( 1.174540682414699111, -0.3162353388693405765, 0.4822834645669290543 ) ) ;
#50959 = CARTESIAN_POINT ( 'NONE',  ( 0.1958661417322834775, 0.3392501089628018884, -2.026246719160105236 ) ) ;
#50960 = DIRECTION ( 'NONE',  ( 0.000000000000000000, 0.000000000000000000, 1.000000000000000000 ) ) ;
#50961 = CARTESIAN_POINT ( 'NONE',  ( -0.7020997375328076329, -0.3162353388693409650, -0.4822834645669289433 ) ) ;
#50962 = CARTESIAN_POINT ( 'NONE',  ( -0.1265901696524993347, 0.4724409448818895907, -0.3215223097112860362 ) ) ;
#50963 = CARTESIAN_POINT ( 'NONE',  ( 0.3949938075777409963, 2.418639510665530435E-17, -2.795275590551181022 ) ) ;
#50964 = VERTEX_POINT ( 'NONE', #61390 ) ;
#50965 = CARTESIAN_POINT ( 'NONE',  ( -0.04593175853018302557, 0.1771653543307087630, 0.09757992244046791164 ) ) ;
#50966 = CARTESIAN_POINT ( 'NONE',  ( 0.2867679344610365999, -0.2867679344610365444, -1.350393700787401619 ) ) ;
#50967 = CARTESIAN_POINT ( 'NONE',  ( 0.8530183727034126306, 0.05413385826771626580, -0.4176697321401330321 ) ) ;
#50968 = CARTESIAN_POINT ( 'NONE',  ( -0.02707642104390568794, 0.3965571307776177834, -2.755905511811025388 ) ) ;
#50969 = DIRECTION ( 'NONE',  ( 0.000000000000000000, 0.000000000000000000, -1.000000000000000000 ) ) ;
#50970 = CARTESIAN_POINT ( 'NONE',  ( -0.4461942257217840213, -0.5023911411419708095, -0.1820866141732282451 ) ) ;
#50971 = FACE_OUTER_BOUND ( 'NONE', #29805, .T. ) ;
#50972 = CARTESIAN_POINT ( 'NONE',  ( 1.286089238845145033, -0.6046776061558809534, -0.2411417322834644161 ) ) ;
#50973 = CARTESIAN_POINT ( 'NONE',  ( 0.9776902887139113929, 0.1771653543307087630, 0.09757992244046791164 ) ) ;
#50974 = CARTESIAN_POINT ( 'NONE',  ( -0.1574803149606292529, -0.1870078740157480879, -0.4822834645669291653 ) ) ;
#50975 = CARTESIAN_POINT ( 'NONE',  ( -0.1049643490035306742, 0.3917322834645668994, -0.7165161172890270880 ) ) ;
#50976 = CARTESIAN_POINT ( 'NONE',  ( -0.2362204724409440182, -0.1870078740157479769, 0.4822834645669291653 ) ) ;
#50977 = CARTESIAN_POINT ( 'NONE',  ( -1.397637795275589623, 0.07958543189024085140, 0.2665933059059887866 ) ) ;
#50978 = CARTESIAN_POINT ( 'NONE',  ( -0.5708661417322828946, 0.1660481256975883668, -0.3530559997133364547 ) ) ;
#50979 = CARTESIAN_POINT ( 'NONE',  ( 0.4849061582275022153, 1.967896864084103914, -0.4921425059946357705 ) ) ;
#50980 = CARTESIAN_POINT ( 'NONE',  ( 0.6423408027444581503, 0.000000000000000000, 0.3464511005275205946 ) ) ;
#50981 = VERTEX_POINT ( 'NONE', #22678 ) ;
#50982 = CARTESIAN_POINT ( 'NONE',  ( 0.3392501089628018329, 0.1958661417322835607, -2.175216166175539811 ) ) ;
#50983 = CARTESIAN_POINT ( 'NONE',  ( 0.4790026246719168435, -0.3162353388693409650, -0.4822834645669289433 ) ) ;
#50984 = ORIENTED_EDGE ( 'NONE', *, *, #65884, .F. ) ;
#50985 = CARTESIAN_POINT ( 'NONE',  ( -0.6364829396325453192, -0.3162353388693405765, 0.4822834645669290543 ) ) ;
#50986 = CARTESIAN_POINT ( 'NONE',  ( 1.555118110236221041, -0.5400638737290844871, 0.3530559997133364547 ) ) ;
#50987 = CARTESIAN_POINT ( 'NONE',  ( 0.5380577427821529035, 0.05413385826771626580, -0.4176697321401330321 ) ) ;
#50988 = CARTESIAN_POINT ( 'NONE',  ( 0.1706036745406830368, -0.4281496062992127816, -0.4176697321401328100 ) ) ;
#50989 = CARTESIAN_POINT ( 'NONE',  ( -0.2867679344610365999, 0.2867679344610364889, -1.364173228346456268 ) ) ;
#50990 = CARTESIAN_POINT ( 'NONE',  ( -0.8464566929133852113, -0.5400638737290845981, -0.3530559997133363437 ) ) ;
#50991 = CARTESIAN_POINT ( 'NONE',  ( -0.2362204724409440182, -0.1870078740157479769, 0.4822834645669291653 ) ) ;
#50992 = CARTESIAN_POINT ( 'NONE',  ( -1.062992125984250968, -0.6692913385826771977, 8.415575281601705876E-17 ) ) ;
#50993 = CARTESIAN_POINT ( 'NONE',  ( -0.1509186351706028884, -0.2845877964562161244, -0.3641732283464567121 ) ) ;
#50994 = CARTESIAN_POINT ( 'NONE',  ( -0.2710308418177483358, -0.1175056764482960703, 5.568898341878665725 ) ) ;
#50995 = CARTESIAN_POINT ( 'NONE',  ( -0.09186351706036689768, 0.05413385826771626580, -0.4176697321401330321 ) ) ;
#50996 = CARTESIAN_POINT ( 'NONE',  ( 3.908320185825791881, 1.537401574803149984, -0.4744094488188970171 ) ) ;
#50997 = CARTESIAN_POINT ( 'NONE',  ( 1.095800524934383846, -0.3162353388693405765, 0.4822834645669290543 ) ) ;
#50998 = CARTESIAN_POINT ( 'NONE',  ( 4.797336870675656522E-17, -0.3917322834645670104, -2.905511811023621771 ) ) ;
#50999 = VERTEX_POINT ( 'NONE', #36540 ) ;
#51000 = ORIENTED_EDGE ( 'NONE', *, *, #24627, .F. ) ;
#51001 = CARTESIAN_POINT ( 'NONE',  ( 0.2493438320209980519, 0.05413385826771666132, 0.4176697321401328100 ) ) ;
#51002 = CARTESIAN_POINT ( 'NONE',  ( -0.1181102362204717315, 0.1771653543307087630, 0.000000000000000000 ) ) ;
#51004 = DIRECTION ( 'NONE',  ( -0.000000000000000000, -0.000000000000000000, 1.000000000000000000 ) ) ;
#51003 = CARTESIAN_POINT ( 'NONE',  ( 1.541994750656168645, 0.1771653543307087075, -0.09757992244046823083 ) ) ;
#51005 = CARTESIAN_POINT ( 'NONE',  ( 0.3917322834645670104, 2.398668435337828261E-17, -1.305118110236220375 ) ) ;
#51006 = CARTESIAN_POINT ( 'NONE',  ( -0.4091458600556402980, -0.2362204724409451284, -0.2867454068241469534 ) ) ;
#51007 = CARTESIAN_POINT ( 'NONE',  ( 1.469816272965879911, -0.5023911411419708095, 0.1820866141732285504 ) ) ;
#51008 = CARTESIAN_POINT ( 'NONE',  ( 1.496062992125984703, -0.1870078740157480879, -0.4822834645669291653 ) ) ;
#51009 = CARTESIAN_POINT ( 'NONE',  ( -0.3420746716998660508, -0.1974969037888706924, 0.1856955380577428039 ) ) ;
#51010 = CARTESIAN_POINT ( 'NONE',  ( 0.6627296587926515548, 0.2952755905511811885, 0.1292274648535926551 ) ) ;
#51011 = CARTESIAN_POINT ( 'NONE',  ( -1.286089238845143479, 0.2306618581243847221, -0.2411417322834647770 ) ) ;
#51012 = CARTESIAN_POINT ( 'NONE',  ( -1.266404199475064773, -0.3162353388693405765, 0.4822834645669290543 ) ) ;
#51013 = CARTESIAN_POINT ( 'NONE',  ( 0.1049868766404206816, -0.6046776061558809534, -0.2411417322834644161 ) ) ;
#51014 = CARTESIAN_POINT ( 'NONE',  ( -0.3949938075777411073, 0.1058382717557497660, -0.1095800524934383707 ) ) ;
#51015 = CARTESIAN_POINT ( 'NONE',  ( 1.541994750656168645, 0.2952755905511810774, -0.1292274648535930714 ) ) ;
#51016 = CARTESIAN_POINT ( 'NONE',  ( 0.9251968503937015864, -0.5400638737290844871, 0.3530559997133364547 ) ) ;
#51017 = CARTESIAN_POINT ( 'NONE',  ( 1.496062992125985147, -0.1870078740157479769, 0.3641732283464567677 ) ) ;
#51018 = LINE ( 'NONE', #80682, #58658 ) ;
#51019 = CONTEXT_DEPENDENT_SHAPE_REPRESENTATION ( #19681, #33209 ) ;
#51020 = CARTESIAN_POINT ( 'NONE',  ( 0.7611548556430454138, 0.1283753931104746893, -0.1820866141732285504 ) ) ;
#51021 = CARTESIAN_POINT ( 'NONE',  ( -0.9776902887139098386, 0.2952755905511810774, -0.1292274648535930714 ) ) ;
#51022 = CARTESIAN_POINT ( 'NONE',  ( -9.787531504996566615E-17, 0.3996062992125985480, -0.3917322834645669549 ) ) ;
#51023 = CARTESIAN_POINT ( 'NONE',  ( -1.640419947506561060, -0.004921259842519576551, 0.3153832671262227771 ) ) ;
#51024 = CARTESIAN_POINT ( 'NONE',  ( 0.2867679344610365999, 0.2867679344610365999, -0.2874015748031494843 ) ) ;
#51026 = CARTESIAN_POINT ( 'NONE',  ( -0.2639696576368211201, 1.142922413699642092, 1.923474121562456451 ) ) ;
#51025 = CARTESIAN_POINT ( 'NONE',  ( 0.6364829396325465405, -0.3162353388693409650, -0.4822834645669289433 ) ) ;
#51027 = CARTESIAN_POINT ( 'NONE',  ( -1.548556430446193399, 0.1283753931104748280, 0.1820866141732283561 ) ) ;
#51028 = CARTESIAN_POINT ( 'NONE',  ( -0.09842519685039295696, -0.5400638737290844871, 0.3530559997133364547 ) ) ;
#51029 = CARTESIAN_POINT ( 'NONE',  ( 0.9317585301837276734, -0.3690944881889763329, 0.3153832671262228327 ) ) ;
#51030 = CARTESIAN_POINT ( 'NONE',  ( 0.9645669291338591078, -0.5400638737290845981, -0.3530559997133363437 ) ) ;
#51031 = DIRECTION ( 'NONE',  ( 0.000000000000000000, -1.000000000000000000, 0.000000000000000000 ) ) ;
#51032 = CARTESIAN_POINT ( 'NONE',  ( -0.6692913385826764205, -0.5511811023622047445, 6.969142054262312111E-17 ) ) ;
#51033 = CARTESIAN_POINT ( 'NONE',  ( -0.6233595800524928121, -0.05778040916215522460, 0.4822834645669289988 ) ) ;
#51034 = CARTESIAN_POINT ( 'NONE',  ( 1.601049868766404982, -0.6046776061558809534, -0.2411417322834644161 ) ) ;
#51035 = CARTESIAN_POINT ( 'NONE',  ( -1.154855643044618851, -0.6046776061558809534, -0.2411417322834644161 ) ) ;
#51036 = CARTESIAN_POINT ( 'NONE',  ( 1.010498687664042716, -0.4281496062992124485, 0.4176697321401328655 ) ) ;
#51037 = CARTESIAN_POINT ( 'NONE',  ( -0.1049643490035302301, -0.3917322834645671770, -0.6988382134196345907 ) ) ;
#51038 = CARTESIAN_POINT ( 'NONE',  ( -1.266404199475064773, -0.08942795157528024563, -0.3641732283464568787 ) ) ;
#51039 = DIRECTION ( 'NONE',  ( 1.000000000000000000, -0.000000000000000000, -0.000000000000000000 ) ) ;
#51040 = CARTESIAN_POINT ( 'NONE',  ( 1.095800524934383846, -0.3162353388693405765, 0.4822834645669290543 ) ) ;
#51041 = CARTESIAN_POINT ( 'NONE',  ( 5.785732909357575061E-17, -0.4724409448818898682, -2.360236220472441193 ) ) ;
#51042 = CARTESIAN_POINT ( 'NONE',  ( -1.732283464566928277, -0.1870078740157479769, 0.4822834645669291653 ) ) ;
#51043 = CARTESIAN_POINT ( 'NONE',  ( 1.607611548556431069, -0.6692913385826773087, -0.1292274648535924053 ) ) ;
#51044 = CARTESIAN_POINT ( 'NONE',  ( -1.174540682414697335, -0.2845877964562161244, -0.3641732283464567121 ) ) ;
#51045 = LINE ( 'NONE', #43908, #78309 ) ;
#51046 = CARTESIAN_POINT ( 'NONE',  ( -0.4593175853018364174, -0.4281496062992127816, -0.4176697321401328100 ) ) ;
#51047 = CARTESIAN_POINT ( 'NONE',  ( -0.2296587926509179312, -0.08942795157527998196, 0.3641732283464567121 ) ) ;
#51048 = CARTESIAN_POINT ( 'NONE',  ( -1.706036745406823485, 0.1283753931104748280, 0.1820866141732283561 ) ) ;
#51049 = CARTESIAN_POINT ( 'NONE',  ( 1.076115485564305141, -0.5023911411419708095, 0.1820866141732285504 ) ) ;
#51050 = CARTESIAN_POINT ( 'NONE',  ( 1.115485564304462551, -0.4281496062992127816, -0.4176697321401328100 ) ) ;
#51051 = CARTESIAN_POINT ( 'NONE',  ( 1.548556430446194954, -0.6046776061558807314, 0.2411417322834647770 ) ) ;
#51052 = CARTESIAN_POINT ( 'NONE',  ( -0.1049868766404193215, -0.5023911411419708095, 0.1820866141732285504 ) ) ;
#51053 = CARTESIAN_POINT ( 'NONE',  ( 0.5183727034120741983, -0.6692913385826771977, 0.1292274648535927661 ) ) ;
#51054 = EDGE_CURVE ( 'NONE', #14996, #25851, #11719, .T. ) ;
#51055 = CARTESIAN_POINT ( 'NONE',  ( 0.4461942257217855201, -0.5023911411419708095, 0.1820866141732285504 ) ) ;
#51056 = CARTESIAN_POINT ( 'NONE',  ( 1.456692913385827515, 0.2952755905511811885, 0.000000000000000000 ) ) ;
#51057 = ADVANCED_FACE ( 'NONE', ( #75276 ), #45571, .F. ) ;
#51058 = CARTESIAN_POINT ( 'NONE',  ( -1.292650918635170010, 0.2952755905511810774, -0.1292274648535930714 ) ) ;
#51059 = CARTESIAN_POINT ( 'NONE',  ( -0.3740157480314953431, -0.5400638737290845981, -0.3530559997133363437 ) ) ;
#51060 = CARTESIAN_POINT ( 'NONE',  ( -0.1998031496062994683, 0.3460692066303958092, -0.3280839895013123453 ) ) ;
#51061 = CARTESIAN_POINT ( 'NONE',  ( 0.3996062992125984925, 0.1070741851644054637, -2.563648293963254776 ) ) ;
#51062 = CARTESIAN_POINT ( 'NONE',  ( 0.6364829396325465405, -0.05778040916215522460, 0.4822834645669289988 ) ) ;
#51063 = CARTESIAN_POINT ( 'NONE',  ( 1.181102362204724976, -0.1870078740157480601, -0.3641732283464567677 ) ) ;
#51064 = CARTESIAN_POINT ( 'NONE',  ( -0.4593175853018364174, -0.4281496062992127816, -0.4176697321401328100 ) ) ;
#51065 = CARTESIAN_POINT ( 'NONE',  ( 0.5249343832021003964, 0.2306618581243847221, -0.2411417322834647770 ) ) ;
#51066 = CARTESIAN_POINT ( 'NONE',  ( -0.2925321140481932924, 0.2925321140481931814, -2.066929133858267154 ) ) ;
#51067 = CARTESIAN_POINT ( 'NONE',  ( 0.1974969037888704704, 0.3420746716998660508, -1.561679790026246684 ) ) ;
#51068 = CARTESIAN_POINT ( 'NONE',  ( 0.1998031496062994405, -0.3460692066303958092, -2.769028871391076230 ) ) ;
#51069 = CARTESIAN_POINT ( 'NONE',  ( 0.3458507752293908943, 0.3458507752293908943, -2.500000000000000000 ) ) ;
#51070 = CARTESIAN_POINT ( 'NONE',  ( -0.1049643490035301885, -0.3917322834645671215, -0.8517060367454067915 ) ) ;
#51071 = CARTESIAN_POINT ( 'NONE',  ( -0.8136482939632537770, -0.5023911411419708095, 0.1820866141732285504 ) ) ;
#51072 = CARTESIAN_POINT ( 'NONE',  ( -0.9842519685039365918, -0.6692913385826771977, 8.415575281601705876E-17 ) ) ;
#51073 = CARTESIAN_POINT ( 'NONE',  ( 0.1974969037888706092, -0.3420746716998660508, -2.373359580052493811 ) ) ;
#51074 = CARTESIAN_POINT ( 'NONE',  ( 0.9842519685039378130, -0.6692913385826771977, 8.415575281601705876E-17 ) ) ;
#51075 = EDGE_CURVE ( 'NONE', #66439, #53376, #63679, .T. ) ;
#51076 = CARTESIAN_POINT ( 'NONE',  ( 1.312335958005249825, 0.2306618581243847221, -0.2411417322834647770 ) ) ;
#51077 = CARTESIAN_POINT ( 'NONE',  ( 0.7414698162729663755, -0.6692913385826773087, -0.1292274648535924053 ) ) ;
#51078 = CARTESIAN_POINT ( 'NONE',  ( -0.2362204724409447953, -0.4091458600556404646, -2.900262467191600635 ) ) ;
#51079 = CARTESIAN_POINT ( 'NONE',  ( 0.3460692066303959202, 0.1998031496062993295, -2.020997375328084100 ) ) ;
#51080 = DIRECTION ( 'NONE',  ( -0.000000000000000000, -1.000000000000000000, -0.000000000000000000 ) ) ;
#51081 = EDGE_CURVE ( 'NONE', #4880, #81379, #32836, .T. ) ;
#51082 = CARTESIAN_POINT ( 'NONE',  ( 0.4199475065616803948, -0.6046776061558809534, -0.2411417322834644161 ) ) ;
#51083 = CARTESIAN_POINT ( 'NONE',  ( 0.7283464566929140904, -0.5400638737290845981, -0.3530559997133363437 ) ) ;
#51084 = CARTESIAN_POINT ( 'NONE',  ( 0.6430446194225728496, -0.004921259842519576551, 0.3153832671262227771 ) ) ;
#51085 = CARTESIAN_POINT ( 'NONE',  ( 1.502624671916010790, -0.05778040916215522460, 0.4822834645669289988 ) ) ;
#51086 = CARTESIAN_POINT ( 'NONE',  ( -0.1958661417322836718, 0.3392501089628017219, -0.09776902887139117537 ) ) ;
#51087 = CARTESIAN_POINT ( 'NONE',  ( 0.5708661417322841158, -0.5400638737290845981, -0.3530559997133363437 ) ) ;
#51088 = CARTESIAN_POINT ( 'NONE',  ( 1.056430446194226658, 0.2952755905511811885, 0.1292274648535926551 ) ) ;
#51089 = CARTESIAN_POINT ( 'NONE',  ( 0.4790026246719168435, -0.3162353388693409650, -0.4822834645669289433 ) ) ;
#51090 = CARTESIAN_POINT ( 'NONE',  ( 1.325459317585302665, -0.3690944881889763329, 0.3153832671262228327 ) ) ;
#51091 = CARTESIAN_POINT ( 'NONE',  ( -0.9645669291338575535, -0.5400638737290844871, 0.3530559997133364547 ) ) ;
#51092 = CARTESIAN_POINT ( 'NONE',  ( -0.7874015748031489847, -0.1870078740157479769, 0.4822834645669291653 ) ) ;
#51093 = CARTESIAN_POINT ( 'NONE',  ( 1.181102362204724976, -0.1870078740157480879, -0.4822834645669291653 ) ) ;
#51094 = CARTESIAN_POINT ( 'NONE',  ( 0.3392501089628018884, -0.1958661417322834220, -0.5045931758530184386 ) ) ;
#51095 = CARTESIAN_POINT ( 'NONE',  ( -0.2867679344610364334, -0.2867679344610367109, -1.625984251968503491 ) ) ;
#51096 =( BOUNDED_CURVE ( )  B_SPLINE_CURVE ( 2, ( #23997, #69031, #11382, #37039, #50073, #37453, #29078, #22763, #38272, #18918, #19333, #52138, #13448 ),
 .UNSPECIFIED., .F., .F. ) 
 B_SPLINE_CURVE_WITH_KNOTS ( ( 3, 2, 2, 2, 2, 2, 3 ),
 ( 0.08750000000000000833, 0.09166666666666667407, 0.09583333333333335369, 0.1000000000000000056, 0.1041666666666666713, 0.1083333333333333370, 0.1125000000000000028 ),
 .UNSPECIFIED. ) 
 CURVE ( )  GEOMETRIC_REPRESENTATION_ITEM ( )  RATIONAL_B_SPLINE_CURVE ( ( 0.9999999999999998890, 0.9659258262890684232, 1.000000000000000000, 0.9659258262890683122, 1.000000000000000000, 0.9659258262890683122, 1.000000000000000000, 0.9659258262890683122, 1.000000000000000000, 0.9659258262890683122, 1.000000000000000000, 0.9659258262890683122, 1.000000000000000000 ) ) 
 REPRESENTATION_ITEM ( '' )  );
#51097 = CARTESIAN_POINT ( 'NONE',  ( 0.3917322834645670104, 2.398668435337828261E-17, -2.629921259842519898 ) ) ;
#51098 = ORIENTED_EDGE ( 'NONE', *, *, #27052, .F. ) ;
#51099 = CARTESIAN_POINT ( 'NONE',  ( 0.3996062992125986035, 0.1070741851644054776, -0.1246719160104987068 ) ) ;
#51100 = ORIENTED_EDGE ( 'NONE', *, *, #53209, .F. ) ;
#51101 = CARTESIAN_POINT ( 'NONE',  ( 1.660104986876641320, -0.05778040916215522460, 0.4822834645669289988 ) ) ;
#51102 = CARTESIAN_POINT ( 'NONE',  ( 1.240157480314961314, -0.4536011799217367080, 0.2665933059059888421 ) ) ;
#51103 = CARTESIAN_POINT ( 'NONE',  ( -0.1998031496062991907, -0.3460692066303959757, -1.325459317585301777 ) ) ;
#51104 = CARTESIAN_POINT ( 'NONE',  ( 1.410761154855643795, -0.08942795157528024563, -0.3641732283464568787 ) ) ;
#51105 = CARTESIAN_POINT ( 'NONE',  ( -0.4724409448818898682, -8.678599364036362592E-17, -2.478346456692913868 ) ) ;
#51106 = CARTESIAN_POINT ( 'NONE',  ( -0.09842519685039295696, 0.1660481256975883391, -0.3530559997133364547 ) ) ;
#51107 = CARTESIAN_POINT ( 'NONE',  ( 0.3857547143408419088, -0.07128922432405931930, -1.929133858267716661 ) ) ;
#51108 = CARTESIAN_POINT ( 'NONE',  ( 0.2867679344610365999, 0.2867679344610365999, -0.6948818897637795144 ) ) ;
#51109 = CARTESIAN_POINT ( 'NONE',  ( -0.6758530183727028406, 0.1771653543307087630, 0.09757992244046791164 ) ) ;
#51110 = CARTESIAN_POINT ( 'NONE',  ( -1.706036745406823485, 0.1283753931104748280, 0.1820866141732283561 ) ) ;
#51111 = CARTESIAN_POINT ( 'NONE',  ( -1.463254593175852492, 0.2952755905511811885, 0.1292274648535926551 ) ) ;
#51112 = CARTESIAN_POINT ( 'NONE',  ( 0.2624671916010504757, -0.6046776061558809534, -0.2411417322834644161 ) ) ;
#51113 = CARTESIAN_POINT ( 'NONE',  ( 1.489501312335958172, -0.05778040916215560624, -0.4822834645669293319 ) ) ;
#51114 = ORIENTED_EDGE ( 'NONE', *, *, #48765, .F. ) ;
#51115 = VECTOR ( 'NONE', #41849, 39.37007874015748143 ) ;
#51116 = CARTESIAN_POINT ( 'NONE',  ( 0.3495983942378627085, -0.3045330818767438275, -0.01888973282054022887 ) ) ;
#51117 = DIRECTION ( 'NONE',  ( 0.2986341967253129948, 0.000000000000000000, -0.9543676527136840670 ) ) ;
#51118 = CARTESIAN_POINT ( 'NONE',  ( -0.2362204724409451284, 0.4091458600556402425, -2.060367454068241511 ) ) ;
#51119 = CARTESIAN_POINT ( 'NONE',  ( 0.4091458600556403535, 0.2362204724409449896, -2.650918635170603554 ) ) ;
#51120 = CARTESIAN_POINT ( 'NONE',  ( -0.6889763779527552368, 0.07958543189024085140, 0.2665933059059887866 ) ) ;
#51121 = CARTESIAN_POINT ( 'NONE',  ( -1.141732283464566011, 0.2952755905511811885, 0.000000000000000000 ) ) ;
#51122 = CARTESIAN_POINT ( 'NONE',  ( 0.9186351706036752773, 0.2306618581243847221, -0.2411417322834647770 ) ) ;
#51123 = ORIENTED_EDGE ( 'NONE', *, *, #55596, .F. ) ;
#51124 = ADVANCED_FACE ( 'NONE', ( #39997 ), #65259, .F. ) ;
#51126 = CARTESIAN_POINT ( 'NONE',  ( 0.3458507752293908943, -0.3458507752293908943, -2.694881889763779625 ) ) ;
#51125 = CARTESIAN_POINT ( 'NONE',  ( 0.4091458600556404646, -0.2362204724409448231, -2.543963254593176071 ) ) ;
#51127 = CARTESIAN_POINT ( 'NONE',  ( 1.056430446194226658, 0.2952755905511811885, 0.1292274648535926551 ) ) ;
#51128 = CARTESIAN_POINT ( 'NONE',  ( -1.043307086614172707, 0.1660481256975883668, -0.3530559997133364547 ) ) ;
#51129 = CARTESIAN_POINT ( 'NONE',  ( 0.1049643490035303689, 0.3917322834645668994, -1.018353387630234419 ) ) ;
#51130 = CARTESIAN_POINT ( 'NONE',  ( -0.5511811023622041894, -0.1870078740157480601, -0.3641732283464567677 ) ) ;
#51131 = CARTESIAN_POINT ( 'NONE',  ( 0.3917322834645670104, -0.1049643490035303273, -0.6686351706036747222 ) ) ;
#51132 = CARTESIAN_POINT ( 'NONE',  ( -0.3346456692913377662, 0.07958543189024071263, -0.2665933059059888421 ) ) ;
#51133 = CARTESIAN_POINT ( 'NONE',  ( -0.04593175853018302557, -0.5511811023622048555, -0.09757992244046775898 ) ) ;
#51134 = CARTESIAN_POINT ( 'NONE',  ( 0.1377952755905518800, -0.5400638737290844871, 0.3530559997133364547 ) ) ;
#51135 = CARTESIAN_POINT ( 'NONE',  ( -0.8333333333333323711, 0.1771653543307087630, 0.09757992244046791164 ) ) ;
#51136 = CARTESIAN_POINT ( 'NONE',  ( -0.3392501089628017219, -0.1958661417322836718, -2.564304461942256808 ) ) ;
#51137 = CARTESIAN_POINT ( 'NONE',  ( 1.128608923884514947, 0.2306618581243848609, 0.2411417322834645549 ) ) ;
#51138 = EDGE_CURVE ( 'NONE', #16450, #35701, #80687, .T. ) ;
#51139 = CARTESIAN_POINT ( 'NONE',  ( -1.305774278215222184, 0.2952755905511811885, 0.1292274648535926551 ) ) ;
#51140 = CARTESIAN_POINT ( 'NONE',  ( 0.4724409448818898682, 2.892866454678787531E-17, -1.139763779527559029 ) ) ;
#51141 = CARTESIAN_POINT ( 'NONE',  ( -0.1771653543307080136, -0.5400638737290844871, 0.3530559997133364547 ) ) ;
#51142 = CARTESIAN_POINT ( 'NONE',  ( -0.7874015748031489847, -0.1870078740157480879, -0.4822834645669291653 ) ) ;
#51143 = CARTESIAN_POINT ( 'NONE',  ( 1.456692913385827515, -0.5511811023622047445, 6.969142054262312111E-17 ) ) ;
#51144 = CARTESIAN_POINT ( 'NONE',  ( -0.4658792650918627265, -0.08942795157527998196, 0.3641732283464567121 ) ) ;
#51145 = CARTESIAN_POINT ( 'NONE',  ( -0.6102362204724400829, 0.1660481256975885056, 0.3530559997133364547 ) ) ;
#51146 = CARTESIAN_POINT ( 'NONE',  ( -1.167979002624671470, 0.05413385826771666132, 0.4176697321401328100 ) ) ;
#51147 = FACE_OUTER_BOUND ( 'NONE', #56894, .T. ) ;
#51148 = CARTESIAN_POINT ( 'NONE',  ( 1.404199475065617708, -0.004921259842519870586, -0.3153832671262229437 ) ) ;
#51149 = CARTESIAN_POINT ( 'NONE',  ( -0.05905511811023545637, 0.1660481256975885056, 0.3530559997133364547 ) ) ;
#51150 = CARTESIAN_POINT ( 'NONE',  ( -1.496062992125983815, -0.1870078740157480879, -0.4822834645669291653 ) ) ;
#51151 = ORIENTED_EDGE ( 'NONE', *, *, #35152, .F. ) ;
#51152 = CARTESIAN_POINT ( 'NONE',  ( -0.3996062992125986590, 0.1070741851644051723, -2.314304461942256808 ) ) ;
#51153 = CARTESIAN_POINT ( 'NONE',  ( -0.8136482939632537770, 0.1283753931104746893, -0.1820866141732285504 ) ) ;
#51154 = CARTESIAN_POINT ( 'NONE',  ( 0.6561679790026253567, 0.2306618581243848609, 0.2411417322834645549 ) ) ;
#51155 = CARTESIAN_POINT ( 'NONE',  ( -0.9383202099737524282, -0.08942795157527998196, 0.3641732283464567121 ) ) ;
#51156 = CARTESIAN_POINT ( 'NONE',  ( -0.3996062992125986590, 0.1070741851644051723, -1.526902887139107490 ) ) ;
#51157 = CARTESIAN_POINT ( 'NONE',  ( -1.141732283464566011, -0.6692913385826771977, 8.415575281601705876E-17 ) ) ;
#51158 = CARTESIAN_POINT ( 'NONE',  ( 0.9580052493438327987, -0.4281496062992127816, -0.4176697321401328100 ) ) ;
#51159 = CARTESIAN_POINT ( 'NONE',  ( 0.5971128608923891301, 0.2952755905511810774, -0.1292274648535930714 ) ) ;
#51160 = CARTESIAN_POINT ( 'NONE',  ( -0.4091458600556402980, -0.2362204724409451284, -0.05249343832020997302 ) ) ;
#51161 = CARTESIAN_POINT ( 'NONE',  ( -1.581364829396324945, -0.2845877964562159024, 0.3641732283464567677 ) ) ;
#51162 = CARTESIAN_POINT ( 'NONE',  ( 0.3996062992125985480, 2.446882876249141654E-17, -0.5098425196850393526 ) ) ;
#51163 = CARTESIAN_POINT ( 'NONE',  ( 0.3996062992125986035, 2.446882876249141962E-17, -0.9055118110236221041 ) ) ;
#51164 = CARTESIAN_POINT ( 'NONE',  ( 0.1058382717557500713, -0.3949938075777409408, -0.2427821522309712154 ) ) ;
#51165 = CARTESIAN_POINT ( 'NONE',  ( 0.3636368138136163997, 1.231320578257675713, 2.723393322692795770 ) ) ;
#51166 = CARTESIAN_POINT ( 'NONE',  ( 1.122047244094488860, -0.4536011799217368745, -0.2665933059059886201 ) ) ;
#51167 = CARTESIAN_POINT ( 'NONE',  ( 0.8005249343832027131, -0.004921259842519576551, 0.3153832671262227771 ) ) ;
#51168 = CIRCLE ( 'NONE', #61955, 0.09842519685039351207 ) ;
#51169 = CARTESIAN_POINT ( 'NONE',  ( 0.1049868766404206816, -0.6046776061558809534, -0.2411417322834644161 ) ) ;
#51170 = DIRECTION ( 'NONE',  ( -0.000000000000000000, -1.000000000000000000, -0.000000000000000000 ) ) ;
#51171 = CARTESIAN_POINT ( 'NONE',  ( 0.3420746716998660508, 0.1974969037888705814, -1.310367454068241511 ) ) ;
#51172 = CARTESIAN_POINT ( 'NONE',  ( 0.2624671916010504757, 0.1283753931104748280, 0.1820866141732283561 ) ) ;
#51173 = CARTESIAN_POINT ( 'NONE',  ( -0.6430446194225712953, 0.05413385826771626580, -0.4176697321401330321 ) ) ;
#51174 = CARTESIAN_POINT ( 'NONE',  ( -1.318897637795274802, 0.1660481256975885056, 0.3530559997133364547 ) ) ;
#51175 = CARTESIAN_POINT ( 'NONE',  ( 0.7152230971128616943, -0.05778040916215522460, 0.4822834645669289988 ) ) ;
#51176 = CARTESIAN_POINT ( 'NONE',  ( 0.4724409448818897572, -0.1265901696524988906, -1.528871391076114916 ) ) ;
#51177 = DIRECTION ( 'NONE',  ( 0.000000000000000000, 0.000000000000000000, -1.000000000000000000 ) ) ;
#51178 = ORIENTED_EDGE ( 'NONE', *, *, #13421, .F. ) ;
#51179 = VERTEX_POINT ( 'NONE', #53845 ) ;
#51180 = CARTESIAN_POINT ( 'NONE',  ( -1.148293963254592542, -0.6692913385826773087, -0.1292274648535924053 ) ) ;
#51181 = CARTESIAN_POINT ( 'NONE',  ( -0.7480314960629914633, -0.6692913385826771977, 8.415575281601705876E-17 ) ) ;
#51183 = CARTESIAN_POINT ( 'NONE',  ( -0.6692913385826764205, 0.2952755905511811885, 0.000000000000000000 ) ) ;
#51182 = CARTESIAN_POINT ( 'NONE',  ( -0.7874015748031489847, -0.1870078740157480601, -0.3641732283464567677 ) ) ;
#51184 = CARTESIAN_POINT ( 'NONE',  ( -0.3917322834645669549, -7.196005306013483243E-17, -1.851686720963567456 ) ) ;
#51185 = CARTESIAN_POINT ( 'NONE',  ( -0.3460692066303960313, 0.1998031496062989965, -2.780183727034120977 ) ) ;
#51186 = CARTESIAN_POINT ( 'NONE',  ( 1.496062992125985147, -0.1870078740157479769, 0.4822834645669291653 ) ) ;
#51187 = AXIS2_PLACEMENT_3D ( 'NONE', #19829, #45478, #80424 ) ;
#51188 = CARTESIAN_POINT ( 'NONE',  ( -0.6561679790026240244, -0.6046776061558807314, 0.2411417322834647770 ) ) ;
#51189 = CARTESIAN_POINT ( 'NONE',  ( 0.3805774278215230400, 0.05413385826771626580, -0.4176697321401330321 ) ) ;
#51190 = CARTESIAN_POINT ( 'NONE',  ( -0.9120734908136475250, -0.6692913385826773087, -0.1292274648535924053 ) ) ;
#51191 = CARTESIAN_POINT ( 'NONE',  ( 0.3917322834645669549, 0.1049643490035304660, -1.376640419947506189 ) ) ;
#51192 = CARTESIAN_POINT ( 'NONE',  ( -0.9908136482939626788, 0.1771653543307087630, 0.09757992244046791164 ) ) ;
#51193 = ORIENTED_EDGE ( 'NONE', *, *, #61945, .T. ) ;
#51194 = CARTESIAN_POINT ( 'NONE',  ( -9.674558042662121740E-17, 0.3949938075777409963, -1.732283464566929165 ) ) ;
#51195 = VERTEX_POINT ( 'NONE', #66924 ) ;
#51196 = CARTESIAN_POINT ( 'NONE',  ( -1.502624671916009680, -0.08942795157528024563, -0.3641732283464568787 ) ) ;
#51197 = CARTESIAN_POINT ( 'NONE',  ( -1.272965879265091305, 0.05413385826771626580, -0.4176697321401330321 ) ) ;
#51198 = CARTESIAN_POINT ( 'NONE',  ( -1.082677165354329896, -0.5400638737290845981, -0.3530559997133363437 ) ) ;
#51199 = CARTESIAN_POINT ( 'NONE',  ( 4.893765752498283924E-17, -0.3996062992125986035, -0.2362204724409449064 ) ) ;
#51200 = CARTESIAN_POINT ( 'NONE',  ( -1.220472440944881054, 0.2952755905511811885, 0.000000000000000000 ) ) ;
#51201 = CARTESIAN_POINT ( 'NONE',  ( -1.122047244094487306, -0.5400638737290844871, 0.3530559997133364547 ) ) ;
#51202 = CARTESIAN_POINT ( 'NONE',  ( 0.4606732211678788991, 2.793565526369266028, 0.5309055118110233007 ) ) ;
#51203 = EDGE_CURVE ( 'NONE', #73164, #12831, #72809, .T. ) ;
#51204 = DIRECTION ( 'NONE',  ( 1.000000000000000000, -0.000000000000000000, -0.000000000000000000 ) ) ;
#51205 = CARTESIAN_POINT ( 'NONE',  ( 0.3215223097112867578, -0.2845877964562161244, -0.3641732283464567121 ) ) ;
#51206 = CARTESIAN_POINT ( 'NONE',  ( 2.795275590551181910, 1.488513638086842006, 0.000000000000000000 ) ) ;
#51207 = CARTESIAN_POINT ( 'NONE',  ( 0.3917322834645669549, 0.1049643490035304660, -0.2093175853018373611 ) ) ;
#51208 = CARTESIAN_POINT ( 'NONE',  ( -0.1968503937007867743, -0.5511811023622047445, 6.969142054262312111E-17 ) ) ;
#51209 = CARTESIAN_POINT ( 'NONE',  ( -0.8727034120734901146, -0.3162353388693405765, 0.4822834645669290543 ) ) ;
#51210 = EDGE_CURVE ( 'NONE', #44792, #22351, #36826, .T. ) ;
#51211 = CARTESIAN_POINT ( 'NONE',  ( 1.535433070866142335, -0.6692913385826771977, 8.415575281601705876E-17 ) ) ;
#51212 = CARTESIAN_POINT ( 'NONE',  ( -0.4068241469816264999, -0.4281496062992124485, 0.4176697321401328655 ) ) ;
#51213 = ORIENTED_EDGE ( 'NONE', *, *, #78524, .F. ) ;
#51214 = ORIENTED_EDGE ( 'NONE', *, *, #48987, .F. ) ;
#51215 = CARTESIAN_POINT ( 'NONE',  ( -0.3996062992125985480, -7.340648628747423112E-17, -2.005905511811023612 ) ) ;
#51216 = CARTESIAN_POINT ( 'NONE',  ( -0.4133858267716528645, -0.5400638737290844871, 0.3530559997133364547 ) ) ;
#51217 = CARTESIAN_POINT ( 'NONE',  ( 1.207349081364829990, -0.6046776061558809534, -0.2411417322834644161 ) ) ;
#51218 = CARTESIAN_POINT ( 'NONE',  ( -1.318897637795274802, -0.4536011799217368745, -0.2665933059059886201 ) ) ;
#51219 = CARTESIAN_POINT ( 'NONE',  ( -1.207349081364828880, 0.2306618581243847221, -0.2411417322834647770 ) ) ;
#51220 = CARTESIAN_POINT ( 'NONE',  ( -0.4091458600556405756, 0.2362204724409446288, -0.9711286089238845287 ) ) ;
#51221 = CARTESIAN_POINT ( 'NONE',  ( 2.077216372526538013, 1.325969025732677053, 0.4256800600601886586 ) ) ;
#51222 = CARTESIAN_POINT ( 'NONE',  ( 0.3917322834645670104, -0.1049643490035303411, 0.05380577427821527092 ) ) ;
#51223 = CARTESIAN_POINT ( 'NONE',  ( -0.3917322834645670104, -7.196005306013484475E-17, -2.013779527559055094 ) ) ;
#51224 = CARTESIAN_POINT ( 'NONE',  ( 0.2624671916010504757, 0.2306618581243848609, 0.2411417322834645549 ) ) ;
#51225 = CARTESIAN_POINT ( 'NONE',  ( -1.017060367454067249, -0.08942795157527998196, 0.3641732283464567121 ) ) ;
#51226 = CARTESIAN_POINT ( 'NONE',  ( -0.6233595800524928121, -0.05778040916215522460, 0.4822834645669289988 ) ) ;
#51227 = CARTESIAN_POINT ( 'NONE',  ( 0.1265901696524989462, 0.4724409448818897572, -2.589895013123359568 ) ) ;
#51228 = CARTESIAN_POINT ( 'NONE',  ( -0.6824146981627291497, -0.6046776061558809534, -0.2411417322834644161 ) ) ;
#51229 = CARTESIAN_POINT ( 'NONE',  ( -1.148293963254592542, -0.6692913385826773087, -0.1292274648535924053 ) ) ;
#51230 = CARTESIAN_POINT ( 'NONE',  ( 0.01312335958005323398, 0.05413385826771666132, 0.4176697321401328100 ) ) ;
#51231 = CARTESIAN_POINT ( 'NONE',  ( -0.1974969037888704149, -0.3420746716998661063, -2.504593175853018661 ) ) ;
#51232 = CARTESIAN_POINT ( 'NONE',  ( 1.003937007874016185, 0.07958543189024071263, -0.2665933059059888421 ) ) ;
#51233 = CARTESIAN_POINT ( 'NONE',  ( -0.9055118110236215490, 0.1771653543307087630, 0.000000000000000000 ) ) ;
#51234 = CARTESIAN_POINT ( 'NONE',  ( 0.7283464566929143125, 0.07958543189024085140, 0.2665933059059887866 ) ) ;
#51235 = CARTESIAN_POINT ( 'NONE',  ( 1.227034120734908917, -0.5511811023622046335, 0.09757992244046803654 ) ) ;
#51236 = CARTESIAN_POINT ( 'NONE',  ( 1.272965879265092637, 0.05413385826771666132, 0.4176697321401328100 ) ) ;
#51237 = CARTESIAN_POINT ( 'NONE',  ( 0.5249343832021005074, -0.5023911411419708095, 0.1820866141732285504 ) ) ;
#51238 = CARTESIAN_POINT ( 'NONE',  ( -0.3392501089628017219, -0.1958661417322836718, -1.619422572178477848 ) ) ;
#51239 = CARTESIAN_POINT ( 'NONE',  ( -0.6889763779527552368, 0.1660481256975885056, 0.3530559997133364547 ) ) ;
#51240 = CARTESIAN_POINT ( 'NONE',  ( 1.062992125984252745, -0.6692913385826771977, 8.415575281601705876E-17 ) ) ;
#51241 = CARTESIAN_POINT ( 'NONE',  ( 0.01968503937007957949, -0.4536011799217368745, -0.2665933059059886201 ) ) ;
#51242 = CYLINDRICAL_SURFACE ( 'NONE', #52031, 0.1968503937007874405 ) ;
#51243 = CARTESIAN_POINT ( 'NONE',  ( 0.3477690288713918276, -0.6692913385826773087, -0.1292274648535924053 ) ) ;
#51244 = CARTESIAN_POINT ( 'NONE',  ( 0.4724409448818898682, 2.892866454678787531E-17, -0.1181102362204724532 ) ) ;
#51245 = CARTESIAN_POINT ( 'NONE',  ( 0.8595800524934390507, -0.08942795157528024563, -0.3641732283464568787 ) ) ;
#51246 = CARTESIAN_POINT ( 'NONE',  ( 0.2034120734908142214, 0.1771653543307087075, -0.09757992244046823083 ) ) ;
#51247 = CARTESIAN_POINT ( 'NONE',  ( 0.05905511811023709395, -0.5400638737290844871, 0.3530559997133364547 ) ) ;
#51248 = CARTESIAN_POINT ( 'NONE',  ( -1.253280839895012377, -0.05778040916215522460, 0.4822834645669289988 ) ) ;
#51249 = CARTESIAN_POINT ( 'NONE',  ( -0.8727034120734901146, -0.2845877964562159024, 0.3641732283464567677 ) ) ;
#51250 = DIRECTION ( 'NONE',  ( -3.096699300667737957E-16, 1.000000000000000000, -0.000000000000000000 ) ) ;
#51251 = CARTESIAN_POINT ( 'NONE',  ( -0.5511811023622038563, -0.1870078740157479769, 0.4822834645669291653 ) ) ;
#51252 = CARTESIAN_POINT ( 'NONE',  ( -0.1070741851644051862, -0.3996062992125986590, -1.251312335958005173 ) ) ;
#51253 = CARTESIAN_POINT ( 'NONE',  ( 0.1049643490035303689, 0.3917322834645670104, -2.125328083989501682 ) ) ;
#51254 = CARTESIAN_POINT ( 'NONE',  ( 0.01312335958005323398, -0.004921259842519576551, 0.3153832671262227771 ) ) ;
#51255 = CARTESIAN_POINT ( 'NONE',  ( -0.4921259842519677963, 0.1660481256975883668, -0.3530559997133364547 ) ) ;
#51256 = CARTESIAN_POINT ( 'NONE',  ( -1.128608923884513837, 0.2306618581243847221, -0.2411417322834647770 ) ) ;
#51257 = CARTESIAN_POINT ( 'NONE',  ( -1.095800524934382292, -0.2845877964562161244, -0.3641732283464567121 ) ) ;
#51258 = CARTESIAN_POINT ( 'NONE',  ( -3.921749386317083363, 1.212948189903745311, 0.3464575048171062432 ) ) ;
#51259 = CARTESIAN_POINT ( 'NONE',  ( -0.3937007874015740483, -0.1870078740157479769, 0.4822834645669291653 ) ) ;
#51260 = CARTESIAN_POINT ( 'NONE',  ( -0.7020997375328074108, -0.08942795157527998196, 0.3641732283464567121 ) ) ;
#51261 = CARTESIAN_POINT ( 'NONE',  ( -1.496062992125983815, -0.1870078740157480601, -0.3641732283464567677 ) ) ;
#51262 = CARTESIAN_POINT ( 'NONE',  ( 1.148293963254593653, 0.2952755905511810774, -0.1292274648535930714 ) ) ;
#51263 = DIRECTION ( 'NONE',  ( -1.000000000000000000, -3.050063254464715781E-16, 0.000000000000000000 ) ) ;
#51264 = CARTESIAN_POINT ( 'NONE',  ( 0.3917322834645670659, 2.398668435337828261E-17, -2.004612491634857552 ) ) ;
#51265 = ORIENTED_EDGE ( 'NONE', *, *, #58971, .T. ) ;
#51266 = CARTESIAN_POINT ( 'NONE',  ( 1.603475055217291612, 1.054977578535739591, 0.04573490813648269093 ) ) ;
#51267 = CARTESIAN_POINT ( 'NONE',  ( -1.351706036745406347, 0.05413385826771626580, -0.4176697321401330321 ) ) ;
#51268 = CARTESIAN_POINT ( 'NONE',  ( -1.069553805774277722, 0.2952755905511811885, 0.1292274648535926551 ) ) ;
#51269 = CARTESIAN_POINT ( 'NONE',  ( -1.443569553805773564, 0.2306618581243847221, -0.2411417322834647770 ) ) ;
#51270 = CARTESIAN_POINT ( 'NONE',  ( -0.3917322834645671215, 0.1049643490035301469, -1.849737532808399143 ) ) ;
#51271 = CARTESIAN_POINT ( 'NONE',  ( -0.3428707098288043542, 0.1906283239483336500, -1.220472440944882386 ) ) ;
#51272 = CARTESIAN_POINT ( 'NONE',  ( 0.9842519685039378130, -0.6692913385826771977, 8.415575281601705876E-17 ) ) ;
#51273 = CARTESIAN_POINT ( 'NONE',  ( -0.1246719160104980823, -0.6692913385826773087, -0.1292274648535924053 ) ) ;
#51274 = CARTESIAN_POINT ( 'NONE',  ( -0.3260583142159755865, -3.773335473449285555E-15, -0.3954974714151476278 ) ) ;
#51275 = CARTESIAN_POINT ( 'NONE',  ( 0.3460692066303959202, -0.1998031496062991630, -2.701443569553806157 ) ) ;
#51276 = CARTESIAN_POINT ( 'NONE',  ( 1.010498687664042716, -0.004921259842519870586, -0.3153832671262229437 ) ) ;
#51277 = CARTESIAN_POINT ( 'NONE',  ( -0.1070741851644056997, 0.3996062992125986035, -1.266404199475065440 ) ) ;
#51278 = ORIENTED_EDGE ( 'NONE', *, *, #61945, .F. ) ;
#51279 = CARTESIAN_POINT ( 'NONE',  ( 0.1049643490035304938, -0.3917322834645669549, -2.912073490813647858 ) ) ;
#51280 = ORIENTED_EDGE ( 'NONE', *, *, #81557, .T. ) ;
#51281 = CARTESIAN_POINT ( 'NONE',  ( -0.1902887139107604098, -0.6692913385826771977, 0.1292274648535927661 ) ) ;
#51282 = CARTESIAN_POINT ( 'NONE',  ( -0.9317585301837263412, 0.05413385826771666132, 0.4176697321401328100 ) ) ;
#51283 = CARTESIAN_POINT ( 'NONE',  ( -1.391076115485563314, -0.6046776061558809534, -0.2411417322834644161 ) ) ;
#51284 = CARTESIAN_POINT ( 'NONE',  ( 0.5446194225721792126, -0.3162353388693405765, 0.4822834645669290543 ) ) ;
#51285 = CARTESIAN_POINT ( 'NONE',  ( -1.541994750656167090, -0.5511811023622048555, -0.09757992244046775898 ) ) ;
#51286 = CARTESIAN_POINT ( 'NONE',  ( 1.299212598425197429, 0.2952755905511811885, 0.000000000000000000 ) ) ;
#51287 = CARTESIAN_POINT ( 'NONE',  ( -0.6167979002624665030, -0.4281496062992127816, -0.4176697321401328100 ) ) ;
#51288 = CARTESIAN_POINT ( 'NONE',  ( 0.5249343832021003964, 0.2306618581243847221, -0.2411417322834647770 ) ) ;
#51289 = CARTESIAN_POINT ( 'NONE',  ( 1.469816272965879911, 0.2306618581243847221, -0.2411417322834647770 ) ) ;
#51290 = CARTESIAN_POINT ( 'NONE',  ( 1.318897637795276356, 0.1660481256975883668, -0.3530559997133364547 ) ) ;
#51291 = CARTESIAN_POINT ( 'NONE',  ( 1.404199475065617708, 0.05413385826771626580, -0.4176697321401330321 ) ) ;
#51292 = CARTESIAN_POINT ( 'NONE',  ( -0.1640419947506555343, -0.3162353388693405765, 0.4822834645669290543 ) ) ;
#51293 = CARTESIAN_POINT ( 'NONE',  ( -0.3917322834645670104, -7.196005306013484475E-17, -0.1889763779527558474 ) ) ;
#51294 = CARTESIAN_POINT ( 'NONE',  ( 0.4396325459317593221, 0.1771653543307087075, -0.09757992244046823083 ) ) ;
#51295 = EDGE_LOOP ( 'NONE', ( #60954, #82186, #39919, #69363 ) ) ;
#51296 = CARTESIAN_POINT ( 'NONE',  ( 0.2891555358219910499, -0.2891555358219909944, -0.4133858267716535861 ) ) ;
#51297 = ORIENTED_EDGE ( 'NONE', *, *, #61511, .T. ) ;
#51298 = CARTESIAN_POINT ( 'NONE',  ( -0.3280839895013117347, -0.3690944881889763329, 0.3153832671262228327 ) ) ;
#51299 = CARTESIAN_POINT ( 'NONE',  ( 0.000000000000000000, 0.000000000000000000, -2.755905511811024056 ) ) ;
#51300 = CARTESIAN_POINT ( 'NONE',  ( 0.1181102362204730916, -0.6692913385826771977, 8.415575281601705876E-17 ) ) ;
#51301 = CARTESIAN_POINT ( 'NONE',  ( 0.08530183727034192087, -0.3162353388693409650, -0.4822834645669289433 ) ) ;
#51302 = EDGE_CURVE ( 'NONE', #11783, #74653, #70657, .T. ) ;
#51303 = CARTESIAN_POINT ( 'NONE',  ( -0.7152230971128602510, -0.05778040916215560624, -0.4822834645669293319 ) ) ;
#51304 = CARTESIAN_POINT ( 'NONE',  ( 4.797336870675656522E-17, -0.3917322834645670659, -1.650281782973440192 ) ) ;
#51305 = CARTESIAN_POINT ( 'NONE',  ( -1.181102362204723644, -0.1870078740157479769, 0.4822834645669291653 ) ) ;
#51306 = CARTESIAN_POINT ( 'NONE',  ( 1.436417322834644184, 2.401574803149606474, 0.3149606299212598381 ) ) ;
#51307 = CARTESIAN_POINT ( 'NONE',  ( 0.9317585301837276734, -0.3690944881889763329, 0.3153832671262228327 ) ) ;
#51308 = CARTESIAN_POINT ( 'NONE',  ( 0.5446194225721792126, -0.3162353388693405765, 0.4822834645669290543 ) ) ;
#51309 = CARTESIAN_POINT ( 'NONE',  ( 0.8530183727034128527, -0.4281496062992124485, 0.4176697321401328655 ) ) ;
#51310 = CARTESIAN_POINT ( 'NONE',  ( -0.1070741851644056997, 0.3996062992125986035, -1.423884514435695525 ) ) ;
#51311 = CARTESIAN_POINT ( 'NONE',  ( -1.266404199475064773, -0.3162353388693405765, 0.4822834645669290543 ) ) ;
#51312 = CARTESIAN_POINT ( 'NONE',  ( -0.1998031496062994405, 0.3460692066303957537, -0.8772965879265091083 ) ) ;
#51313 = CARTESIAN_POINT ( 'NONE',  ( -0.3996062992125985480, -7.340648628747423112E-17, 0.04133858267716532947 ) ) ;
#51314 = CARTESIAN_POINT ( 'NONE',  ( -0.07217847769028813698, -0.3162353388693409650, -0.4822834645669289433 ) ) ;
#51315 = CARTESIAN_POINT ( 'NONE',  ( -0.1998031496062991907, -0.3460692066303959757, -2.585301837270341352 ) ) ;
#51316 = CARTESIAN_POINT ( 'NONE',  ( 4.797336870675656522E-17, -0.3917322834645670104, -1.895669291338582640 ) ) ;
#51317 = CARTESIAN_POINT ( 'NONE',  ( -1.108923884514435132, -0.08942795157528024563, -0.3641732283464568787 ) ) ;
#51318 = CARTESIAN_POINT ( 'NONE',  ( 1.345144356955381593, -0.3162353388693409650, -0.4822834645669289433 ) ) ;
#51319 = CARTESIAN_POINT ( 'NONE',  ( 1.266404199475066328, -0.3162353388693409650, -0.4822834645669289433 ) ) ;
#51320 = CARTESIAN_POINT ( 'NONE',  ( 0.2624671916010504757, 0.1283753931104748280, 0.1820866141732283561 ) ) ;
#51321 = CARTESIAN_POINT ( 'NONE',  ( 0.9645669291338588858, 0.1660481256975885056, 0.3530559997133364547 ) ) ;
#51322 = CARTESIAN_POINT ( 'NONE',  ( -0.3458507752293906723, -0.3458507752293910609, -1.395669291338582196 ) ) ;
#51323 = CARTESIAN_POINT ( 'NONE',  ( 0.4593175853018380828, -0.004921259842519870586, -0.3153832671262229437 ) ) ;
#51324 = CARTESIAN_POINT ( 'NONE',  ( 0.3805774278215230400, 0.05413385826771626580, -0.4176697321401330321 ) ) ;
#51325 = CARTESIAN_POINT ( 'NONE',  ( 0.2891555358219910499, -0.2891555358219909944, -0.8051181102362204856 ) ) ;
#51326 = CARTESIAN_POINT ( 'NONE',  ( -1.345144356955379816, -0.05778040916215560624, -0.4822834645669293319 ) ) ;
#51327 = CARTESIAN_POINT ( 'NONE',  ( 0.4921259842519691285, 0.07958543189024085140, 0.2665933059059887866 ) ) ;
#51328 = CARTESIAN_POINT ( 'NONE',  ( 2.362204724409448620, 1.724409448818897461, 8.247593713802677664E-15 ) ) ;
#51329 = CARTESIAN_POINT ( 'NONE',  ( -0.3149606299212590610, -0.1870078740157479769, 0.4822834645669291653 ) ) ;
#51330 = CARTESIAN_POINT ( 'NONE',  ( -0.4133858267716528645, -0.4536011799217367080, 0.2665933059059888421 ) ) ;
#51331 = DIRECTION ( 'NONE',  ( -0.000000000000000000, 1.000000000000000000, -0.000000000000000000 ) ) ;
#51332 = CARTESIAN_POINT ( 'NONE',  ( -0.4002624671916004129, -0.05778040916215560624, -0.4822834645669293319 ) ) ;
#51333 = CARTESIAN_POINT ( 'NONE',  ( 0.4461942257217855201, -0.5023911411419708095, 0.1820866141732285504 ) ) ;
#51334 = CARTESIAN_POINT ( 'NONE',  ( -0.1998031496062991630, -0.3460692066303959202, -2.189632545931758489 ) ) ;
#51335 = CARTESIAN_POINT ( 'NONE',  ( -0.05905511811023545637, 0.1660481256975885056, 0.3530559997133364547 ) ) ;
#51336 = CARTESIAN_POINT ( 'NONE',  ( -0.3392501089628018329, -0.1958661417322836440, -1.707329765582990211 ) ) ;
#51337 = CARTESIAN_POINT ( 'NONE',  ( 1.272965879265092637, -0.3690944881889765550, -0.3153832671262227771 ) ) ;
#51338 = CARTESIAN_POINT ( 'NONE',  ( 0.1968503937007881344, 0.2952755905511811885, 0.000000000000000000 ) ) ;
#51339 = CARTESIAN_POINT ( 'NONE',  ( -0.8792650918635160906, -0.004921259842519870586, -0.3153832671262229437 ) ) ;
#51340 = CARTESIAN_POINT ( 'NONE',  ( -0.8923884514435688198, 0.1283753931104746893, -0.1820866141732285504 ) ) ;
#51341 = CARTESIAN_POINT ( 'NONE',  ( -0.6233595800524928121, -0.3162353388693409650, -0.4822834645669289433 ) ) ;
#51342 = CARTESIAN_POINT ( 'NONE',  ( -0.05249343832020938322, -0.6046776061558809534, -0.2411417322834644161 ) ) ;
#51343 = CARTESIAN_POINT ( 'NONE',  ( 0.7283464566929143125, 0.07958543189024085140, 0.2665933059059887866 ) ) ;
#51344 = CARTESIAN_POINT ( 'NONE',  ( 0.3149606299212184268, 2.559055118110236560, 3.937007874015792552 ) ) ;
#51345 = CARTESIAN_POINT ( 'NONE',  ( 1.338582677165355062, -0.1870078740157480601, -0.3641732283464567677 ) ) ;
#51346 = AXIS2_PLACEMENT_3D ( 'NONE', #54814, #48490, #12271 ) ;
#51347 = CARTESIAN_POINT ( 'NONE',  ( 0.8989501312335964611, 0.2952755905511811885, 0.1292274648535926551 ) ) ;
#51348 = CARTESIAN_POINT ( 'NONE',  ( 0.2925321140481932369, 0.2925321140481932369, -0.05708661417322836301 ) ) ;
#51349 = CARTESIAN_POINT ( 'NONE',  ( -0.4658792650918627265, -0.05778040916215522460, 0.4822834645669289988 ) ) ;
#51350 = CARTESIAN_POINT ( 'NONE',  ( 0.3917322834645670104, 2.398668435337828261E-17, -0.9901574803149607584 ) ) ;
#51351 = CARTESIAN_POINT ( 'NONE',  ( 1.614173228346457378, 0.1771653543307087630, 0.000000000000000000 ) ) ;
#51352 = CARTESIAN_POINT ( 'NONE',  ( 0.7939632545931766261, -0.3162353388693409650, -0.4822834645669289433 ) ) ;
#51353 = CARTESIAN_POINT ( 'NONE',  ( -0.03937007874015669567, 0.2952755905511811885, 0.000000000000000000 ) ) ;
#51354 = CARTESIAN_POINT ( 'NONE',  ( -0.2101277439827862470, 1.111780837440068392, -3.931420396975905174 ) ) ;
#51355 = CARTESIAN_POINT ( 'NONE',  ( 0.4330708661417329575, 0.1771653543307087630, 0.000000000000000000 ) ) ;
#51356 = CARTESIAN_POINT ( 'NONE',  ( 0.5774278215223104249, 0.2306618581243848609, 0.2411417322834645549 ) ) ;
#51357 = CARTESIAN_POINT ( 'NONE',  ( -0.4068241469816267775, -0.004921259842519870586, -0.3153832671262229437 ) ) ;
#51358 = CARTESIAN_POINT ( 'NONE',  ( -0.9186351706036736120, -0.6046776061558809534, -0.2411417322834644161 ) ) ;
#51359 = CARTESIAN_POINT ( 'NONE',  ( -0.5120078740157480990, 0.000000000000000000, -0.3051181102362204856 ) ) ;
#51360 = CARTESIAN_POINT ( 'NONE',  ( 0.1049868766404206816, -0.6046776061558809534, -0.2411417322834644161 ) ) ;
#51361 = CARTESIAN_POINT ( 'NONE',  ( -0.7939632545931750718, -0.05778040916215560624, -0.4822834645669293319 ) ) ;
#51362 = CARTESIAN_POINT ( 'NONE',  ( -0.7545931758530177724, 0.1771653543307087630, 0.09757992244046791164 ) ) ;
#51363 = CARTESIAN_POINT ( 'NONE',  ( 0.4593175853018379162, -0.4281496062992124485, 0.4176697321401328655 ) ) ;
#51364 = CARTESIAN_POINT ( 'NONE',  ( -1.233595800524933894, 0.2306618581243848609, 0.2411417322834645549 ) ) ;
#51365 = CARTESIAN_POINT ( 'NONE',  ( -0.4593175853018364174, -0.4281496062992127816, -0.4176697321401328100 ) ) ;
#51366 = CARTESIAN_POINT ( 'NONE',  ( 1.154855643044620184, 0.1539470093639521697, -0.1968503937007875793 ) ) ;
#51368 = CARTESIAN_POINT ( 'NONE',  ( 1.384514435695538337, -0.6692913385826771977, 0.1292274648535927661 ) ) ;
#51367 = DIRECTION ( 'NONE',  ( 0.000000000000000000, 0.000000000000000000, -1.000000000000000000 ) ) ;
#51369 = CARTESIAN_POINT ( 'NONE',  ( 1.482939632545932307, -0.4281496062992124485, 0.4176697321401328655 ) ) ;
#51370 = CARTESIAN_POINT ( 'NONE',  ( 0.3917322834645670104, -0.1049643490035303273, -2.623359580052492923 ) ) ;
#51371 = CARTESIAN_POINT ( 'NONE',  ( -1.515748031496062076, -0.5400638737290844871, 0.3530559997133364547 ) ) ;
#51372 = CARTESIAN_POINT ( 'NONE',  ( -0.8923884514435688198, 0.2306618581243847221, -0.2411417322834647770 ) ) ;
#51373 = CARTESIAN_POINT ( 'NONE',  ( 0.2362204724409449064, 0.4091458600556404646, -0.9317585301837270073 ) ) ;
#51374 = CARTESIAN_POINT ( 'NONE',  ( -0.1070741851644056997, 0.3996062992125986035, -0.006561679790026264843 ) ) ;
#51375 = VERTEX_POINT ( 'NONE', #61413 ) ;
#51376 = CARTESIAN_POINT ( 'NONE',  ( 0.03937007874015833325, -0.5511811023622047445, 6.969142054262312111E-17 ) ) ;
#51377 = CARTESIAN_POINT ( 'NONE',  ( -0.2867679344610365999, 0.2867679344610364889, -1.901574803149606252 ) ) ;
#51378 = VERTEX_POINT ( 'NONE', #16406 ) ;
#51379 = CARTESIAN_POINT ( 'NONE',  ( 0.2624671916010504757, -0.6046776061558809534, -0.2411417322834644161 ) ) ;
#51380 = CARTESIAN_POINT ( 'NONE',  ( 0.1265901696524990294, -0.4724409448818896462, -2.762467191601049255 ) ) ;
#51381 = CARTESIAN_POINT ( 'NONE',  ( -0.03443470937339728616, 0.2755905511811023723, -1.537015892239756099 ) ) ;
#51382 = CARTESIAN_POINT ( 'NONE',  ( -0.3149606299212590610, -0.1870078740157480601, -0.3641732283464567677 ) ) ;
#51383 = CARTESIAN_POINT ( 'NONE',  ( 0.3265464962716623232, 0.02791078216816386681, 0.4328096321851896966 ) ) ;
#51384 = CARTESIAN_POINT ( 'NONE',  ( 0.5708661417322842269, 0.1660481256975885056, 0.3530559997133364547 ) ) ;
#51385 = CARTESIAN_POINT ( 'NONE',  ( 0.7217847769028878924, -0.3690944881889765550, -0.3153832671262227771 ) ) ;
#51386 = CARTESIAN_POINT ( 'NONE',  ( 0.1115485564304470323, 0.2952755905511811885, 0.1292274648535926551 ) ) ;
#51387 = CARTESIAN_POINT ( 'NONE',  ( 0.1958661417322836162, -0.3392501089628018329, -0.9592982695199985255 ) ) ;
#51388 = CARTESIAN_POINT ( 'NONE',  ( -0.6167979002624665030, -0.4281496062992127816, -0.4176697321401328100 ) ) ;
#51389 = CARTESIAN_POINT ( 'NONE',  ( -1.200787401574802349, 0.07958543189024071263, -0.2665933059059888421 ) ) ;
#51390 = EDGE_CURVE ( 'NONE', #66675, #42693, #36526, .T. ) ;
#51391 = CARTESIAN_POINT ( 'NONE',  ( -0.5577427821522301654, -0.05778040916215560624, -0.4822834645669293319 ) ) ;
#51392 = DIRECTION ( 'NONE',  ( 0.000000000000000000, -1.000000000000000000, 0.000000000000000000 ) ) ;
#51393 = CARTESIAN_POINT ( 'NONE',  ( -0.4607143505782321236, 1.423150415408463987, -2.139150952031436237 ) ) ;
#51394 = ORIENTED_EDGE ( 'NONE', *, *, #2818, .F. ) ;
#51395 = CARTESIAN_POINT ( 'NONE',  ( -0.3392501089628017219, -0.1958661417322836995, -2.411436638616484718 ) ) ;
#51396 = CARTESIAN_POINT ( 'NONE',  ( 0.4199475065616805614, 0.2306618581243848609, 0.2411417322834645549 ) ) ;
#51397 = VERTEX_POINT ( 'NONE', #12144 ) ;
#51398 = CARTESIAN_POINT ( 'NONE',  ( -0.5905511811023615998, 0.2952755905511811885, 0.000000000000000000 ) ) ;
#51399 = CARTESIAN_POINT ( 'NONE',  ( 1.443569553805774897, 0.2306618581243848609, 0.2411417322834645549 ) ) ;
#51400 = CARTESIAN_POINT ( 'NONE',  ( 1.095800524934383846, -0.3162353388693405765, 0.4822834645669290543 ) ) ;
#51401 = CARTESIAN_POINT ( 'NONE',  ( 0.7677165354330716118, -0.5400638737290844871, 0.3530559997133364547 ) ) ;
#51402 = AXIS2_PLACEMENT_3D ( 'NONE', #60876, #3228, #49070 ) ;
#51403 = EDGE_CURVE ( 'NONE', #19450, #9917, #28380, .T. ) ;
#51404 = CARTESIAN_POINT ( 'NONE',  ( 0.1640419947506569498, -0.3162353388693409650, -0.4822834645669289433 ) ) ;
#51405 = CARTESIAN_POINT ( 'NONE',  ( -0.2867679344610365999, 0.2867679344610364889, -1.206692913385826627 ) ) ;
#51406 = CARTESIAN_POINT ( 'NONE',  ( -1.167979002624671470, -0.4281496062992127816, -0.4176697321401328100 ) ) ;
#51407 = CARTESIAN_POINT ( 'NONE',  ( -0.3543307086614165824, 0.2952755905511811885, 0.000000000000000000 ) ) ;
#51408 = CARTESIAN_POINT ( 'NONE',  ( -0.1771653543307080136, 0.07958543189024071263, -0.2665933059059888421 ) ) ;
#51409 = CARTESIAN_POINT ( 'NONE',  ( -0.2635274766024540694, -0.1334916279589803412, 5.819004606509202482 ) ) ;
#51410 = CARTESIAN_POINT ( 'NONE',  ( -0.1246719160104980823, 0.2952755905511811885, 0.1292274648535926551 ) ) ;
#51411 = DIRECTION ( 'NONE',  ( 0.000000000000000000, -1.601283208593975810E-15, -1.000000000000000000 ) ) ;
#51412 = CARTESIAN_POINT ( 'NONE',  ( 0.9383202099737536495, -0.3162353388693405765, 0.4822834645669290543 ) ) ;
#51413 = CARTESIAN_POINT ( 'NONE',  ( 3.909774025758389726, 1.429695482061029477, -0.4622850232133952075 ) ) ;
#51414 = VERTEX_POINT ( 'NONE', #24752 ) ;
#51415 = VERTEX_POINT ( 'NONE', #63479 ) ;
#51416 = CARTESIAN_POINT ( 'NONE',  ( 0.1640419947506569498, -0.3162353388693409650, -0.4822834645669289433 ) ) ;
#51417 = CARTESIAN_POINT ( 'NONE',  ( -0.1902887139107604098, -0.5511811023622046335, 0.09757992244046803654 ) ) ;
#51419 = CARTESIAN_POINT ( 'NONE',  ( 0.5314960629921325896, 2.729653106663536555, -1.868118594278512345 ) ) ;
#51418 = CARTESIAN_POINT ( 'NONE',  ( 1.614173228346457378, -0.5511811023622047445, 6.969142054262312111E-17 ) ) ;
#51420 = CARTESIAN_POINT ( 'NONE',  ( 0.1049643490035304938, -0.3917322834645669549, -1.114829396325459410 ) ) ;
#51421 = CARTESIAN_POINT ( 'NONE',  ( -0.1265901696524986964, -0.4724409448818899238, -0.3064304461942257141 ) ) ;
#51422 = CARTESIAN_POINT ( 'NONE',  ( 1.476377952755906442, -0.4536011799217367080, 0.2665933059059888421 ) ) ;
#51423 = CARTESIAN_POINT ( 'NONE',  ( -1.627296587926508442, 0.2306618581243848609, 0.2411417322834645549 ) ) ;
#51424 = CARTESIAN_POINT ( 'NONE',  ( -0.1974969037888706924, 0.3420746716998658843, 0.06758530183727033680 ) ) ;
#51425 = CARTESIAN_POINT ( 'NONE',  ( 0.2427821522309716595, -0.3162353388693409650, -0.4822834645669289433 ) ) ;
#51426 = CARTESIAN_POINT ( 'NONE',  ( -1.089238845144356427, -0.4281496062992127816, -0.4176697321401328100 ) ) ;
#51427 = CARTESIAN_POINT ( 'NONE',  ( -1.056430446194224881, 0.2952755905511810774, -0.1292274648535930714 ) ) ;
#51428 = CARTESIAN_POINT ( 'NONE',  ( 0.1312335958005255154, -0.6046776061558807314, 0.2411417322834647770 ) ) ;
#51429 = CARTESIAN_POINT ( 'NONE',  ( -0.2891555358219911054, 0.2891555358219909388, -0.2539370078740157410 ) ) ;
#51430 = CARTESIAN_POINT ( 'NONE',  ( -1.509186351706035767, -0.3690944881889763329, 0.3153832671262228327 ) ) ;
#51431 = CARTESIAN_POINT ( 'NONE',  ( 1.017060367454068581, -0.05778040916215560624, -0.4822834645669293319 ) ) ;
#51432 = CARTESIAN_POINT ( 'NONE',  ( 0.7939632545931766261, -0.2845877964562161244, -0.3641732283464567121 ) ) ;
#51433 = CARTESIAN_POINT ( 'NONE',  ( 0.8202099737532814183, 0.2066929133858267931, 0.1054918080437490802 ) ) ;
#51434 = CARTESIAN_POINT ( 'NONE',  ( 0.9842519685039378130, -0.5511811023622047445, 6.969142054262312111E-17 ) ) ;
#51435 = CARTESIAN_POINT ( 'NONE',  ( -1.266404199475064773, -0.05778040916215560624, -0.4822834645669293319 ) ) ;
#51436 = CARTESIAN_POINT ( 'NONE',  ( -0.3460692066303960313, 0.1998031496062989965, -0.8904199475065617264 ) ) ;
#51437 = CARTESIAN_POINT ( 'NONE',  ( 1.030183727034121421, -0.05778040916215522460, 0.4822834645669289988 ) ) ;
#51438 = CARTESIAN_POINT ( 'NONE',  ( 0.2867679344610365999, -0.2867679344610365444, -0.7204724409448818312 ) ) ;
#51440 = LINE ( 'NONE', #17839, #81575 ) ;
#51439 = CARTESIAN_POINT ( 'NONE',  ( 0.8267716535433078384, -0.6692913385826771977, 8.415575281601705876E-17 ) ) ;
#51441 = CARTESIAN_POINT ( 'NONE',  ( -1.603475055217291612, 1.054977578535736926, 0.04573490813648253134 ) ) ;
#51442 = CARTESIAN_POINT ( 'NONE',  ( -0.03937007874015669567, 0.2952755905511811885, 0.000000000000000000 ) ) ;
#51443 = CARTESIAN_POINT ( 'NONE',  ( 0.4461942257217855201, -0.5023911411419708095, 0.1820866141732285504 ) ) ;
#51444 = CARTESIAN_POINT ( 'NONE',  ( 0.8136482939632553313, -0.6046776061558809534, -0.2411417322834644161 ) ) ;
#51445 = CARTESIAN_POINT ( 'NONE',  ( 1.633858267716535639, -0.4536011799217367080, 0.2665933059059888421 ) ) ;
#51446 = CARTESIAN_POINT ( 'NONE',  ( -0.7611548556430438595, 0.1283753931104748280, 0.1820866141732283561 ) ) ;
#51447 = CARTESIAN_POINT ( 'NONE',  ( -0.8005249343832013809, -0.4281496062992124485, 0.4176697321401328655 ) ) ;
#51448 = CIRCLE ( 'NONE', #15207, 0.1574803149606300579 ) ;
#51449 = CARTESIAN_POINT ( 'NONE',  ( 1.541994750656168645, 0.2952755905511810774, -0.1292274648535930714 ) ) ;
#51450 = CARTESIAN_POINT ( 'NONE',  ( -1.161417322834644716, -0.5400638737290845981, -0.3530559997133363437 ) ) ;
#51451 = CARTESIAN_POINT ( 'NONE',  ( 1.128608923884515169, -0.6046776061558809534, -0.2411417322834644161 ) ) ;
#51452 = CARTESIAN_POINT ( 'NONE',  ( -1.154855643044618851, 0.1283753931104748280, 0.1820866141732283561 ) ) ;
#51453 = CARTESIAN_POINT ( 'NONE',  ( 1.087350715983457228, 1.152082538880340179, 0.2771893343846333901 ) ) ;
#51454 = CARTESIAN_POINT ( 'NONE',  ( 1.043307086614173818, -0.5400638737290845981, -0.3530559997133363437 ) ) ;
#51455 = CARTESIAN_POINT ( 'NONE',  ( -0.1265901696524993347, 0.4724409448818895907, -2.603018372703412631 ) ) ;
#51456 = CARTESIAN_POINT ( 'NONE',  ( -1.719160104986876103, 0.05413385826771666132, 0.4176697321401328100 ) ) ;
#51457 = CARTESIAN_POINT ( 'NONE',  ( -1.423884514435694859, -0.08942795157528024563, -0.3641732283464568787 ) ) ;
#51458 = CARTESIAN_POINT ( 'NONE',  ( -1.233595800524933894, 0.1283753931104748280, 0.1820866141732283561 ) ) ;
#51460 = CARTESIAN_POINT ( 'NONE',  ( 1.476377952755906442, -0.4536011799217367080, 0.2665933059059888421 ) ) ;
#51459 =( BOUNDED_SURFACE ( )  B_SPLINE_SURFACE ( 1, 2, ( 
 ( #48736, #17196, #16780, #42418, #11280, #9624, #81581, #68118, #3307, #10463, #75258, #29794, #81164, #23480, #43234, #68931, #36939, #56292, #15955, #60957, #28972, #63029, #64683, #6602, #38590, #50792, #31028, #45308, #75671, #69348, #38172, #5367, #70576, #56696, #57521, #44064, #7022, #64268, #51612, #32274, #83212, #13346, #50381, #76493, #32690, #82395, #76079, #18423, #69756, #24713, #63846, #12102, #18011, #58357, #82798, #25534, #12930, #77317, #37760, #25122, #51199, #12511, #43645, #76897, #18820, #57103, #19227, #63435, #19647, #5771, #31440, #57934, #44467, #70158, #298, #71003, #25954, #44877, #39000, #719, #26377, #6184, #11702, #37356, #31862, #52452, #34370, #27631, #8283, #33949, #26795, #9121, #20910, #71421, #46563, #2802, #2391, #65947, #59198, #71842, #47396, #53293, #1557, #78584, #79005, #27211, #34791, #13768, #15437, #60450, #73087, #58787, #14192, #60035, #28047, #20493, #39425, #52037, #20072, #41098, #1145, #45724, #39849, #65109, #66786, #66361, #72262, #53705, #21733, #7447, #40264, #33117, #59613, #46147, #79414, #77741, #78162, #52874, #65540, #7871, #33535, #14610, #1968, #21324, #46977, #72671, #15020, #40676, #8699, #17102, #81484, #35611, #62106, #68023, #29295, #36026, #54539, #79836, #47812, #42323, #15863, #61274, #28461, #54957, #80664, #3627, #68433, #16684, #11186, #22153, #73514, #62519, #22976, #41511, #10366, #80254, #23800, #9527, #61698, #49055, #10773, #4038, #35199, #67196, #4449, #22571, #81071, #55366, #48643, #67608, #29703, #17511, #30114, #54122, #60860, #3214, #23387, #41914, #74754, #36847, #28876, #73927, #48231, #42737, #74337, #36433, #49473, #16269, #55776, #9939, #75166, #43143, #68840, #50698, #63340, #43555, #6509, #62938, #24621, #30935, #70062, #82302, #49879, #75579, #77218, #19131, #51103, #5675, #69256, #57834, #4858, #81897, #76396, #17919, #83119, #11603, #12416, #56602, #19547, #76800, #64175, #44780, #38074, #25854, #5271, #31343, #45206, #37262, #50288, #75986, #18328, #43968, #18728, #69665, #30532, #70906, #6089, #70477, #12008, #37662, #12834, #44370, #38492, #31764, #57009, #82705, #25025, #32179, #63750, #57425, #25437, #202, #51514, #13257, #38906, #56196, #24208, #60667, #21127, #8504, #35001, #66164, #73733, #9331, #15238, #40898, #67408, #3429, #14826, #34170, #16070, #66579, #21955, #41716, #48440, #8914, #46786, #3015, #61079, #54343, #29092, #54762, #22779, #79222, #9743, #72889, #35414, #41316, #15657, #48031, #80468, #34590, #74140, #66999, #28682, #16484, #72477, #53090, #64586, #59833, #80053, #22372, #60257, #21538, #47613, #6923, #32594, #59415, #27429, #1772, #53925, #47198, #78802, #40486, #2186, #27854, #53514, #2605, #28263, #79637, #73309, #10164, #69048, #61905, #29504, #4247, #75372, #4651, #17316, #80874, #43758, #16902, #29909, #68243, #24012, #36235, #3844, #55164, #31143, #56406, #5074, #42944, #23186, #11814, #42131, #35830, #30322, #48856, #37054, #74557, #49680, #10578, #56810, #30743, #18126, #82105, #17718, #63142, #42541, #68639, #82509, #55573, #81281, #23597, #49268, #74970, #55990, #10978, #67826, #24825, #43346, #24418, #36638, #62314, #50088, #81701, #75784, #11397, #62737, #69464, #37469, #5483, #50493, #76196, #61496, #77860, #83309, #70699, #19350, #45424, #25653, #13463, #57217, #44583, #71120, #18935, #26502, #39120, #51315, #77018, #20189, #39545, #50904, #70276, #52155, #45000, #58053, #45840, #1265, #13052, #82919, #64801, #13886, #7140, #65234, #7571, #58905, #31978, #32813, #71538, #25239, #38705, #77436, #64384, #18534, #19771, #6720, #32390, #58480, #76604, #33243, #31560, #63965, #844, #38289, #12630, #26913, #52573, #44177, #51734, #419, #69870, #12222, #26075, #37879, #63553, #5887, #6302, #57638, #53821, #34488, #60154, #52989, #35314, #47096 ),
 ( #21440, #59316, #73205, #73632, #66902, #41621, #67310, #60976, #8400, #2919, #2085, #47927, #79535, #28165, #60568, #1672, #65660, #28582, #21026, #47513, #21849, #53414, #34067, #2506, #9645, #54239, #28991, #39973, #14313, #66477, #59730, #15555, #3327, #78702, #40381, #14728, #41214, #27750, #79123, #15974, #46265, #9232, #66064, #7989, #72786, #34905, #40792, #15136, #33653, #79956, #46686, #8812, #72379, #22269, #78282, #27329, #20613, #71960, #68951, #17622, #29813, #10060, #24324, #54657, #48340, #17216, #42030, #49583, #35723, #36543, #23088, #69368, #43254, #30647, #11301, #62219, #75691, #29406, #36960, #56312, #62637, #4557, #18032, #55065, #55474, #43666, #61393, #80773, #48755, #74454, #3742, #42849, #16800, #80368, #37378, #55890, #4981, #42437, #68137, #82009, #68542, #49994, #81601, #10482, #36135, #61808, #11722, #10883, #30227, #4148, #63048, #81184, #23501, #49167, #23918, #74873, #75279, #5387, #22681, #74037, #16384, #67724, #57952, #63866, #6203, #32712, #52055, #63457, #31462, #39019, #31881, #70596, #64703, #13787, #57541, #12123, #25973, #26397, #19665, #77761, #20093, #71439, #44486, #7043, #38191, #740, #6621, #64286, #13366, #37781, #18443, #58378, #57124, #320, #51632, #83232, #70178, #12950, #45744, #39444, #65132, #76099, #50402, #19246, #12530, #77336, #31048, #5792, #76512, #50811, #32292, #25553, #51220, #56718, #82415, #45327, #18841, #44085, #76917, #71022, #44897, #38608, #69779, #24734, #82818, #25142, #33553, #72689, #1577, #52474, #78182, #79852, #21749, #53722, #65965, #46165, #60467, #7467, #1165, #53311, #20513, #2407, #71861, #15037, #59215, #22169, #60051, #15878, #65558, #52891, #27232, #40692, #40283, #8301, #2817, #58807, #34386, #78604, #14211, #20927, #66378, #79024, #33969, #39868, #9137, #7891, #46583, #72281, #8715, #14628, #59630, #1986, #47828, #47413, #79430, #27649, #21342, #28478, #33136, #26816, #46996, #28065, #73103, #15455, #41113, #66802, #73531, #34808, #54138, #41526, #74770, #4874, #41931, #42340, #56211, #48246, #67625, #9957, #35628, #16287, #29719, #61290, #9545, #49895, #68448, #55793, #73942, #3644, #49488, #55381, #30129, #10788, #29311, #54972, #80679, #81499, #23404, #81087, #22993, #43158, #48658, #36041, #68038, #36448, #74356, #62121, #22585, #16699, #4464, #10384, #75181, #23818, #61713, #4052, #68854, #30547, #49071, #17118, #17526, #42754, #11203, #36862, #75594, #62536, #81912, #24224, #17933, #67212, #35214, #60878, #3229, #28894, #54555, #80270, #32192, #31777, #6104, #70491, #56617, #5289, #38507, #76001, #25451, #57439, #82719, #5689, #12430, #51529, #64188, #70921, #62953, #37277, #70077, #63355, #12023, #12848, #69680, #82316, #51118, #57849, #6523, #83132, #38089, #25867, #19145, #44383, #216, #77232, #19561, #18343, #45220, #76813, #63763, #44795, #50303, #43569, #76411, #30950, #18741, #69270, #11616, #24636, #43983, #37679, #31359, #57025, #25039, #50712, #11044, #10642, #18191, #54826, #82170, #75849, #30803, #42193, #80935, #17782, #43416, #3906, #22842, #43824, #3491, #56469, #67888, #29157, #55228, #80530, #24486, #49743, #55638, #11462, #5138, #48501, #23662, #74202, #49333, #29566, #69114, #69528, #10226, #42604, #35475, #50153, #16549, #61139, #61563, #81348, #35893, #37120, #23251, #56055, #48921, #24074, #74621, #68306, #62804, #75034, #36297, #43009, #16965, #61971, #4310, #17379, #29974, #68703, #36703, #62377, #4715, #30389, #75443, #81764, #77930, #63206, #5545, #45910, #44647, #31210, #66, #37941, #7212, #76262, #25720, #32459, #77509, #51380, #18998, #45069, #58121, #71190, #18597, #70344, #70772, #32044, #11878, #13123, #12698, #76665, #38774, #44240, #13532, #24890, #63618, #57703, #69929, #19844, #917, #488, #37530, #26143, #64872, #38357, #45493, #77085, #64033 ) ),
 .UNSPECIFIED., .F., .F., .F. ) 
 B_SPLINE_SURFACE_WITH_KNOTS ( ( 2, 2 ),
 ( 3, 2, 2, 2, 2, 2, 2, 2, 2, 2, 2, 2, 2, 2, 2, 2, 2, 2, 2, 2, 2, 2, 2, 2, 2, 2, 2, 2, 2, 2, 2, 2, 2, 2, 2, 2, 2, 2, 2, 2, 2, 2, 2, 2, 2, 2, 2, 2, 2, 2, 2, 2, 2, 2, 2, 2, 2, 2, 2, 2, 2, 2, 2, 2, 2, 2, 2, 2, 2, 2, 2, 2, 2, 2, 2, 2, 2, 2, 2, 2, 2, 2, 2, 2, 2, 2, 2, 2, 2, 2, 2, 2, 2, 2, 2, 2, 2, 2, 2, 2, 2, 2, 2, 2, 2, 2, 2, 2, 2, 2, 2, 2, 2, 2, 2, 2, 2, 2, 2, 2, 2, 2, 2, 2, 2, 2, 2, 2, 2, 2, 2, 2, 2, 2, 2, 2, 2, 2, 2, 2, 2, 2, 2, 2, 2, 2, 2, 2, 2, 2, 2, 2, 2, 2, 2, 2, 2, 2, 2, 2, 2, 2, 2, 2, 2, 2, 2, 2, 2, 2, 2, 2, 2, 2, 2, 2, 2, 2, 2, 2, 2, 2, 2, 2, 2, 2, 2, 2, 2, 2, 2, 2, 2, 2, 2, 2, 2, 2, 2, 2, 2, 2, 2, 2, 2, 2, 2, 2, 2, 2, 2, 2, 2, 2, 2, 2, 2, 2, 2, 2, 2, 2, 2, 2, 2, 2, 2, 2, 2, 2, 2, 2, 2, 2, 2, 2, 2, 3 ),
 ( 0.000000000000000000, 1.000000000000000000 ),
 ( 0.000000000000000000, 0.004166666666666666609, 0.008333333333333333218, 0.01250000000000000069, 0.01666666666666666644, 0.02083333333333333218, 0.02500000000000000139, 0.02916666666666666713, 0.03333333333333333287, 0.03749999999999999861, 0.04166666666666666435, 0.04583333333333333010, 0.05000000000000000278, 0.05416666666666666852, 0.05833333333333333426, 0.06250000000000000000, 0.06666666666666666574, 0.07083333333333333148, 0.07499999999999999722, 0.07916666666666666297, 0.08333333333333332871, 0.08749999999999999445, 0.09166666666666666019, 0.09583333333333333981, 0.1000000000000000056, 0.1041666666666666713, 0.1083333333333333370, 0.1125000000000000028, 0.1166666666666666685, 0.1208333333333333343, 0.1250000000000000000, 0.1291666666666666796, 0.1333333333333333315, 0.1375000000000000111, 0.1416666666666666630, 0.1458333333333333426, 0.1499999999999999944, 0.1541666666666666741, 0.1583333333333333259, 0.1625000000000000056, 0.1666666666666666574, 0.1708333333333333370, 0.1749999999999999889, 0.1791666666666666685, 0.1833333333333333204, 0.1875000000000000000, 0.1916666666666666796, 0.1958333333333333315, 0.2000000000000000111, 0.2041666666666666630, 0.2083333333333333426, 0.2124999999999999944, 0.2166666666666666741, 0.2208333333333333259, 0.2250000000000000056, 0.2291666666666666574, 0.2333333333333333370, 0.2374999999999999889, 0.2416666666666666685, 0.2458333333333333204, 0.2500000000000000000, 0.2541666666666666519, 0.2583333333333333592, 0.2625000000000000111, 0.2666666666666666630, 0.2708333333333333148, 0.2750000000000000222, 0.2791666666666666741, 0.2833333333333333259, 0.2874999999999999778, 0.2916666666666666852, 0.2958333333333333370, 0.2999999999999999889, 0.3041666666666666408, 0.3083333333333333481, 0.3125000000000000000, 0.3166666666666666519, 0.3208333333333333592, 0.3250000000000000111, 0.3291666666666666630, 0.3333333333333333148, 0.3375000000000000222, 0.3416666666666666741, 0.3458333333333333259, 0.3499999999999999778, 0.3541666666666666852, 0.3583333333333333370, 0.3624999999999999889, 0.3666666666666666408, 0.3708333333333333481, 0.3750000000000000000, 0.3791666666666666519, 0.3833333333333333592, 0.3875000000000000111, 0.3916666666666666630, 0.3958333333333333148, 0.4000000000000000222, 0.4041666666666666741, 0.4083333333333333259, 0.4124999999999999778, 0.4166666666666666852, 0.4208333333333333370, 0.4249999999999999889, 0.4291666666666666408, 0.4333333333333333481, 0.4375000000000000000, 0.4416666666666666519, 0.4458333333333333592, 0.4500000000000000111, 0.4541666666666666630, 0.4583333333333333148, 0.4625000000000000222, 0.4666666666666666741, 0.4708333333333333259, 0.4749999999999999778, 0.4791666666666666852, 0.4833333333333333370, 0.4874999999999999889, 0.4916666666666666408, 0.4958333333333333481, 0.5000000000000000000, 0.5041666666666666519, 0.5083333333333333037, 0.5124999999999999556, 0.5166666666666667185, 0.5208333333333333703, 0.5250000000000000222, 0.5291666666666666741, 0.5333333333333333259, 0.5374999999999999778, 0.5416666666666666297, 0.5458333333333332815, 0.5500000000000000444, 0.5541666666666666963, 0.5583333333333333481, 0.5625000000000000000, 0.5666666666666666519, 0.5708333333333333037, 0.5749999999999999556, 0.5791666666666667185, 0.5833333333333333703, 0.5875000000000000222, 0.5916666666666666741, 0.5958333333333333259, 0.5999999999999999778, 0.6041666666666666297, 0.6083333333333332815, 0.6125000000000000444, 0.6166666666666666963, 0.6208333333333333481, 0.6250000000000000000, 0.6291666666666666519, 0.6333333333333333037, 0.6374999999999999556, 0.6416666666666667185, 0.6458333333333333703, 0.6500000000000000222, 0.6541666666666666741, 0.6583333333333333259, 0.6624999999999999778, 0.6666666666666666297, 0.6708333333333332815, 0.6750000000000000444, 0.6791666666666666963, 0.6833333333333333481, 0.6875000000000000000, 0.6916666666666666519, 0.6958333333333333037, 0.6999999999999999556, 0.7041666666666667185, 0.7083333333333333703, 0.7125000000000000222, 0.7166666666666666741, 0.7208333333333333259, 0.7249999999999999778, 0.7291666666666666297, 0.7333333333333332815, 0.7375000000000000444, 0.7416666666666666963, 0.7458333333333333481, 0.7500000000000000000, 0.7541666666666666519, 0.7583333333333333037, 0.7624999999999999556, 0.7666666666666667185, 0.7708333333333333703, 0.7750000000000000222, 0.7791666666666666741, 0.7833333333333333259, 0.7874999999999999778, 0.7916666666666666297, 0.7958333333333332815, 0.8000000000000000444, 0.8041666666666666963, 0.8083333333333333481, 0.8125000000000000000, 0.8166666666666666519, 0.8208333333333333037, 0.8249999999999999556, 0.8291666666666667185, 0.8333333333333333703, 0.8375000000000000222, 0.8416666666666666741, 0.8458333333333333259, 0.8499999999999999778, 0.8541666666666666297, 0.8583333333333332815, 0.8625000000000000444, 0.8666666666666666963, 0.8708333333333333481, 0.8750000000000000000, 0.8791666666666666519, 0.8833333333333333037, 0.8874999999999999556, 0.8916666666666667185, 0.8958333333333333703, 0.9000000000000000222, 0.9041666666666666741, 0.9083333333333333259, 0.9124999999999999778, 0.9166666666666666297, 0.9208333333333332815, 0.9250000000000000444, 0.9291666666666666963, 0.9333333333333333481, 0.9375000000000000000, 0.9416666666666666519, 0.9458333333333333037, 0.9499999999999999556, 0.9541666666666667185, 0.9583333333333333703, 0.9625000000000000222, 0.9666666666666666741, 0.9708333333333333259, 0.9749999999999999778, 0.9791666666666666297, 0.9833333333333332815, 0.9875000000000000444 ),
 .UNSPECIFIED. ) 
 GEOMETRIC_REPRESENTATION_ITEM ( )  RATIONAL_B_SPLINE_SURFACE ( (
 ( 1.000000000000000000, 0.9659258262890683122, 1.000000000000000000, 0.9659258262890683122, 1.000000000000000000, 0.9659258262890683122, 1.000000000000000000, 0.9659258262890683122, 1.000000000000000000, 0.9659258262890683122, 1.000000000000000000, 0.9659258262890683122, 1.000000000000000000, 0.9659258262890683122, 1.000000000000000000, 0.9659258262890683122, 1.000000000000000000, 0.9659258262890683122, 1.000000000000000000, 0.9659258262890683122, 1.000000000000000000, 0.9659258262890683122, 1.000000000000000000, 0.9659258262890683122, 1.000000000000000000, 0.9659258262890683122, 1.000000000000000000, 0.9659258262890683122, 1.000000000000000000, 0.9659258262890683122, 1.000000000000000000, 0.9659258262890683122, 1.000000000000000000, 0.9659258262890683122, 1.000000000000000000, 0.9659258262890683122, 1.000000000000000000, 0.9659258262890683122, 1.000000000000000000, 0.9659258262890683122, 1.000000000000000000, 0.9659258262890683122, 1.000000000000000000, 0.9659258262890683122, 1.000000000000000000, 0.9659258262890683122, 1.000000000000000000, 0.9659258262890683122, 1.000000000000000000, 0.9659258262890683122, 1.000000000000000000, 0.9659258262890683122, 1.000000000000000000, 0.9659258262890683122, 1.000000000000000000, 0.9659258262890683122, 1.000000000000000000, 0.9659258262890683122, 1.000000000000000000, 0.9659258262890683122, 1.000000000000000000, 0.9659258262890683122, 1.000000000000000000, 0.9659258262890683122, 1.000000000000000000, 0.9659258262890683122, 1.000000000000000000, 0.9659258262890683122, 1.000000000000000000, 0.9659258262890683122, 1.000000000000000000, 0.9659258262890683122, 1.000000000000000000, 0.9659258262890683122, 1.000000000000000000, 0.9659258262890683122, 1.000000000000000000, 0.9659258262890683122, 1.000000000000000000, 0.9659258262890683122, 1.000000000000000000, 0.9659258262890683122, 1.000000000000000000, 0.9659258262890683122, 1.000000000000000000, 0.9659258262890683122, 1.000000000000000000, 0.9659258262890683122, 1.000000000000000000, 0.9659258262890683122, 1.000000000000000000, 0.9659258262890683122, 1.000000000000000000, 0.9659258262890683122, 1.000000000000000000, 0.9659258262890683122, 1.000000000000000000, 0.9659258262890683122, 1.000000000000000000, 0.9659258262890683122, 1.000000000000000000, 0.9659258262890683122, 1.000000000000000000, 0.9659258262890683122, 1.000000000000000000, 0.9659258262890683122, 1.000000000000000000, 0.9659258262890683122, 1.000000000000000000, 0.9659258262890683122, 1.000000000000000000, 0.9659258262890683122, 1.000000000000000000, 0.9659258262890683122, 1.000000000000000000, 0.9659258262890683122, 1.000000000000000000, 0.9659258262890683122, 1.000000000000000000, 0.9659258262890683122, 1.000000000000000000, 0.9659258262890683122, 1.000000000000000000, 0.9659258262890683122, 1.000000000000000000, 0.9659258262890683122, 1.000000000000000000, 0.9659258262890683122, 1.000000000000000000, 0.9659258262890683122, 1.000000000000000000, 0.9659258262890683122, 1.000000000000000000, 0.9659258262890683122, 1.000000000000000000, 0.9659258262890683122, 1.000000000000000000, 0.9659258262890683122, 1.000000000000000000, 0.9659258262890683122, 1.000000000000000000, 0.9659258262890683122, 1.000000000000000000, 0.9659258262890683122, 1.000000000000000000, 0.9659258262890683122, 1.000000000000000000, 0.9659258262890683122, 1.000000000000000000, 0.9659258262890683122, 1.000000000000000000, 0.9659258262890683122, 1.000000000000000000, 0.9659258262890683122, 1.000000000000000000, 0.9659258262890683122, 1.000000000000000000, 0.9659258262890683122, 1.000000000000000000, 0.9659258262890683122, 1.000000000000000000, 0.9659258262890683122, 1.000000000000000000, 0.9659258262890683122, 1.000000000000000000, 0.9659258262890683122, 1.000000000000000000, 0.9659258262890683122, 1.000000000000000000, 0.9659258262890683122, 1.000000000000000000, 0.9659258262890683122, 1.000000000000000000, 0.9659258262890683122, 1.000000000000000000, 0.9659258262890683122, 1.000000000000000000, 0.9659258262890683122, 1.000000000000000000, 0.9659258262890683122, 1.000000000000000000, 0.9659258262890683122, 1.000000000000000000, 0.9659258262890683122, 1.000000000000000000, 0.9659258262890683122, 1.000000000000000000, 0.9659258262890683122, 1.000000000000000000, 0.9659258262890683122, 1.000000000000000000, 0.9659258262890683122, 1.000000000000000000, 0.9659258262890683122, 1.000000000000000000, 0.9659258262890683122, 1.000000000000000000, 0.9659258262890683122, 1.000000000000000000, 0.9659258262890683122, 1.000000000000000000, 0.9659258262890683122, 1.000000000000000000, 0.9659258262890683122, 1.000000000000000000, 0.9659258262890683122, 1.000000000000000000, 0.9659258262890683122, 1.000000000000000000, 0.9659258262890683122, 1.000000000000000000, 0.9659258262890683122, 1.000000000000000000, 0.9659258262890683122, 1.000000000000000000, 0.9659258262890683122, 1.000000000000000000, 0.9659258262890683122, 1.000000000000000000, 0.9659258262890683122, 1.000000000000000000, 0.9659258262890683122, 1.000000000000000000, 0.9659258262890683122, 1.000000000000000000, 0.9659258262890683122, 1.000000000000000000, 0.9659258262890683122, 1.000000000000000000, 0.9659258262890683122, 1.000000000000000000, 0.9659258262890683122, 1.000000000000000000, 0.9659258262890683122, 1.000000000000000000, 0.9659258262890683122, 1.000000000000000000, 0.9659258262890683122, 1.000000000000000000, 0.9659258262890683122, 1.000000000000000000, 0.9659258262890683122, 1.000000000000000000, 0.9659258262890683122, 1.000000000000000000, 0.9659258262890683122, 1.000000000000000000, 0.9659258262890683122, 1.000000000000000000, 0.9659258262890683122, 1.000000000000000000, 0.9659258262890683122, 1.000000000000000000, 0.9659258262890683122, 1.000000000000000000, 0.9659258262890683122, 1.000000000000000000, 0.9659258262890683122, 1.000000000000000000, 0.9659258262890683122, 1.000000000000000000, 0.9659258262890683122, 1.000000000000000000, 0.9659258262890683122, 1.000000000000000000, 0.9659258262890683122, 1.000000000000000000, 0.9659258262890683122, 1.000000000000000000, 0.9659258262890683122, 1.000000000000000000, 0.9659258262890683122, 1.000000000000000000, 0.9659258262890683122, 1.000000000000000000, 0.9659258262890683122, 1.000000000000000000, 0.9659258262890683122, 1.000000000000000000, 0.9659258262890683122, 1.000000000000000000, 0.9659258262890683122, 1.000000000000000000, 0.9659258262890683122, 1.000000000000000000, 0.9659258262890683122, 1.000000000000000000, 0.9659258262890683122, 1.000000000000000000, 0.9659258262890683122, 1.000000000000000000, 0.9659258262890683122, 1.000000000000000000, 0.9659258262890683122, 1.000000000000000000, 0.9659258262890683122, 1.000000000000000000, 0.9659258262890683122, 1.000000000000000000, 0.9659258262890683122, 1.000000000000000000, 0.9659258262890683122, 1.000000000000000000, 0.9659258262890683122, 1.000000000000000000, 0.9659258262890683122, 1.000000000000000000, 0.9659258262890683122, 1.000000000000000000, 0.9659258262890683122, 1.000000000000000000, 0.9659258262890683122, 1.000000000000000000, 0.9659258262890683122, 1.000000000000000000, 0.9659258262890683122, 1.000000000000000000, 0.9659258262890683122, 1.000000000000000000, 0.9659258262890683122, 1.000000000000000000, 0.9659258262890683122, 1.000000000000000000, 0.9659258262890683122, 1.000000000000000000, 0.9659258262890683122, 1.000000000000000000, 0.9659258262890683122, 1.000000000000000000, 0.9659258262890683122, 1.000000000000000000, 0.9659258262890683122, 1.000000000000000000, 0.9659258262890683122, 1.000000000000000000, 0.9659258262890683122, 1.000000000000000000, 0.9659258262890683122, 1.000000000000000000, 0.9659258262890683122, 1.000000000000000000, 0.9659258262890683122, 1.000000000000000000, 0.9659258262890683122, 1.000000000000000000, 0.9659258262890683122, 1.000000000000000000, 0.9659258262890683122, 1.000000000000000000, 0.9659258262890683122, 1.000000000000000000, 0.9659258262890683122, 1.000000000000000000, 0.9659258262890683122, 1.000000000000000000, 0.9659258262890683122, 1.000000000000000000, 0.9659258262890683122, 1.000000000000000000, 0.9659258262890683122, 1.000000000000000000, 0.9659258262890683122, 1.000000000000000000, 0.9659258262890683122, 1.000000000000000000, 0.9659258262890683122, 1.000000000000000000, 0.9659258262890683122, 1.000000000000000000, 0.9659258262890683122, 1.000000000000000000, 0.9659258262890683122, 1.000000000000000000, 0.9659258262890683122, 1.000000000000000000, 0.9659258262890683122, 1.000000000000000000, 0.9659258262890683122, 1.000000000000000000, 0.9659258262890683122, 1.000000000000000000, 0.9659258262890683122, 1.000000000000000000, 0.9659258262890683122, 1.000000000000000000, 0.9659258262890683122, 1.000000000000000000, 0.9659258262890683122, 1.000000000000000000, 0.9659258262890683122, 1.000000000000000000, 0.9659258262890683122, 1.000000000000000000, 0.9659258262890683122, 1.000000000000000000, 0.9659258262890683122, 1.000000000000000000, 0.9659258262890683122, 1.000000000000000000, 0.9659258262890683122, 1.000000000000000000, 0.9659258262890683122, 1.000000000000000000, 0.9659258262890683122, 1.000000000000000000, 0.9659258262890683122, 1.000000000000000000, 0.9659258262890683122, 1.000000000000000000, 0.9659258262890683122, 1.000000000000000000, 0.9659258262890683122, 1.000000000000000000, 0.9659258262890683122, 1.000000000000000000, 0.9659258262890683122, 1.000000000000000000, 0.9659258262890683122, 1.000000000000000000, 0.9659258262890683122, 1.000000000000000000, 0.9659258262890683122, 1.000000000000000000, 0.9659258262890683122, 1.000000000000000000, 0.9659258262890683122, 1.000000000000000000, 0.9659258262890683122, 1.000000000000000000, 0.9659258262890683122, 1.000000000000000000, 0.9659258262890683122, 1.000000000000000000, 0.9659258262890683122, 1.000000000000000000, 0.9659258262890683122, 1.000000000000000000, 0.9659258262890683122, 1.000000000000000000, 0.9659258262890683122, 1.000000000000000000, 0.9659258262890683122, 1.000000000000000000, 0.9659258262890683122, 1.000000000000000000, 0.9659258262890683122, 1.000000000000000000, 0.9659258262890683122, 1.000000000000000000, 0.9659258262890683122, 1.000000000000000000, 0.9659258262890683122, 1.000000000000000000, 0.9659258262890683122, 1.000000000000000000, 0.9659258262890683122, 1.000000000000000000, 0.9659258262890683122, 1.000000000000000000, 0.9659258262890683122, 1.000000000000000000, 0.9659258262890683122, 1.000000000000000000, 0.9659258262890683122, 1.000000000000000000, 0.9659258262890683122, 1.000000000000000000, 0.9659258262890683122, 1.000000000000000000, 0.9659258262890683122, 1.000000000000000000, 0.9659258262890683122, 1.000000000000000000, 0.9659258262890683122, 1.000000000000000000),
 ( 1.000000000000000000, 0.9659258262890683122, 1.000000000000000000, 0.9659258262890683122, 1.000000000000000000, 0.9659258262890683122, 1.000000000000000000, 0.9659258262890683122, 1.000000000000000000, 0.9659258262890683122, 1.000000000000000000, 0.9659258262890683122, 1.000000000000000000, 0.9659258262890683122, 1.000000000000000000, 0.9659258262890683122, 1.000000000000000000, 0.9659258262890683122, 1.000000000000000000, 0.9659258262890683122, 1.000000000000000000, 0.9659258262890683122, 1.000000000000000000, 0.9659258262890683122, 1.000000000000000000, 0.9659258262890683122, 1.000000000000000000, 0.9659258262890683122, 1.000000000000000000, 0.9659258262890683122, 1.000000000000000000, 0.9659258262890683122, 1.000000000000000000, 0.9659258262890683122, 1.000000000000000000, 0.9659258262890683122, 1.000000000000000000, 0.9659258262890683122, 1.000000000000000000, 0.9659258262890683122, 1.000000000000000000, 0.9659258262890683122, 1.000000000000000000, 0.9659258262890683122, 1.000000000000000000, 0.9659258262890683122, 1.000000000000000000, 0.9659258262890683122, 1.000000000000000000, 0.9659258262890683122, 1.000000000000000000, 0.9659258262890683122, 1.000000000000000000, 0.9659258262890683122, 1.000000000000000000, 0.9659258262890683122, 1.000000000000000000, 0.9659258262890683122, 1.000000000000000000, 0.9659258262890683122, 1.000000000000000000, 0.9659258262890683122, 1.000000000000000000, 0.9659258262890683122, 1.000000000000000000, 0.9659258262890683122, 1.000000000000000000, 0.9659258262890683122, 1.000000000000000000, 0.9659258262890683122, 1.000000000000000000, 0.9659258262890683122, 1.000000000000000000, 0.9659258262890683122, 1.000000000000000000, 0.9659258262890683122, 1.000000000000000000, 0.9659258262890683122, 1.000000000000000000, 0.9659258262890683122, 1.000000000000000000, 0.9659258262890683122, 1.000000000000000000, 0.9659258262890683122, 1.000000000000000000, 0.9659258262890683122, 1.000000000000000000, 0.9659258262890683122, 1.000000000000000000, 0.9659258262890683122, 1.000000000000000000, 0.9659258262890683122, 1.000000000000000000, 0.9659258262890683122, 1.000000000000000000, 0.9659258262890683122, 1.000000000000000000, 0.9659258262890683122, 1.000000000000000000, 0.9659258262890683122, 1.000000000000000000, 0.9659258262890683122, 1.000000000000000000, 0.9659258262890683122, 1.000000000000000000, 0.9659258262890683122, 1.000000000000000000, 0.9659258262890683122, 1.000000000000000000, 0.9659258262890683122, 1.000000000000000000, 0.9659258262890683122, 1.000000000000000000, 0.9659258262890683122, 1.000000000000000000, 0.9659258262890683122, 1.000000000000000000, 0.9659258262890683122, 1.000000000000000000, 0.9659258262890683122, 1.000000000000000000, 0.9659258262890683122, 1.000000000000000000, 0.9659258262890683122, 1.000000000000000000, 0.9659258262890683122, 1.000000000000000000, 0.9659258262890683122, 1.000000000000000000, 0.9659258262890683122, 1.000000000000000000, 0.9659258262890683122, 1.000000000000000000, 0.9659258262890683122, 1.000000000000000000, 0.9659258262890683122, 1.000000000000000000, 0.9659258262890683122, 1.000000000000000000, 0.9659258262890683122, 1.000000000000000000, 0.9659258262890683122, 1.000000000000000000, 0.9659258262890683122, 1.000000000000000000, 0.9659258262890683122, 1.000000000000000000, 0.9659258262890683122, 1.000000000000000000, 0.9659258262890683122, 1.000000000000000000, 0.9659258262890683122, 1.000000000000000000, 0.9659258262890683122, 1.000000000000000000, 0.9659258262890683122, 1.000000000000000000, 0.9659258262890683122, 1.000000000000000000, 0.9659258262890683122, 1.000000000000000000, 0.9659258262890683122, 1.000000000000000000, 0.9659258262890683122, 1.000000000000000000, 0.9659258262890683122, 1.000000000000000000, 0.9659258262890683122, 1.000000000000000000, 0.9659258262890683122, 1.000000000000000000, 0.9659258262890683122, 1.000000000000000000, 0.9659258262890683122, 1.000000000000000000, 0.9659258262890683122, 1.000000000000000000, 0.9659258262890683122, 1.000000000000000000, 0.9659258262890683122, 1.000000000000000000, 0.9659258262890683122, 1.000000000000000000, 0.9659258262890683122, 1.000000000000000000, 0.9659258262890683122, 1.000000000000000000, 0.9659258262890683122, 1.000000000000000000, 0.9659258262890683122, 1.000000000000000000, 0.9659258262890683122, 1.000000000000000000, 0.9659258262890683122, 1.000000000000000000, 0.9659258262890683122, 1.000000000000000000, 0.9659258262890683122, 1.000000000000000000, 0.9659258262890683122, 1.000000000000000000, 0.9659258262890683122, 1.000000000000000000, 0.9659258262890683122, 1.000000000000000000, 0.9659258262890683122, 1.000000000000000000, 0.9659258262890683122, 1.000000000000000000, 0.9659258262890683122, 1.000000000000000000, 0.9659258262890683122, 1.000000000000000000, 0.9659258262890683122, 1.000000000000000000, 0.9659258262890683122, 1.000000000000000000, 0.9659258262890683122, 1.000000000000000000, 0.9659258262890683122, 1.000000000000000000, 0.9659258262890683122, 1.000000000000000000, 0.9659258262890683122, 1.000000000000000000, 0.9659258262890683122, 1.000000000000000000, 0.9659258262890683122, 1.000000000000000000, 0.9659258262890683122, 1.000000000000000000, 0.9659258262890683122, 1.000000000000000000, 0.9659258262890683122, 1.000000000000000000, 0.9659258262890683122, 1.000000000000000000, 0.9659258262890683122, 1.000000000000000000, 0.9659258262890683122, 1.000000000000000000, 0.9659258262890683122, 1.000000000000000000, 0.9659258262890683122, 1.000000000000000000, 0.9659258262890683122, 1.000000000000000000, 0.9659258262890683122, 1.000000000000000000, 0.9659258262890683122, 1.000000000000000000, 0.9659258262890683122, 1.000000000000000000, 0.9659258262890683122, 1.000000000000000000, 0.9659258262890683122, 1.000000000000000000, 0.9659258262890683122, 1.000000000000000000, 0.9659258262890683122, 1.000000000000000000, 0.9659258262890683122, 1.000000000000000000, 0.9659258262890683122, 1.000000000000000000, 0.9659258262890683122, 1.000000000000000000, 0.9659258262890683122, 1.000000000000000000, 0.9659258262890683122, 1.000000000000000000, 0.9659258262890683122, 1.000000000000000000, 0.9659258262890683122, 1.000000000000000000, 0.9659258262890683122, 1.000000000000000000, 0.9659258262890683122, 1.000000000000000000, 0.9659258262890683122, 1.000000000000000000, 0.9659258262890683122, 1.000000000000000000, 0.9659258262890683122, 1.000000000000000000, 0.9659258262890683122, 1.000000000000000000, 0.9659258262890683122, 1.000000000000000000, 0.9659258262890683122, 1.000000000000000000, 0.9659258262890683122, 1.000000000000000000, 0.9659258262890683122, 1.000000000000000000, 0.9659258262890683122, 1.000000000000000000, 0.9659258262890683122, 1.000000000000000000, 0.9659258262890683122, 1.000000000000000000, 0.9659258262890683122, 1.000000000000000000, 0.9659258262890683122, 1.000000000000000000, 0.9659258262890683122, 1.000000000000000000, 0.9659258262890683122, 1.000000000000000000, 0.9659258262890683122, 1.000000000000000000, 0.9659258262890683122, 1.000000000000000000, 0.9659258262890683122, 1.000000000000000000, 0.9659258262890683122, 1.000000000000000000, 0.9659258262890683122, 1.000000000000000000, 0.9659258262890683122, 1.000000000000000000, 0.9659258262890683122, 1.000000000000000000, 0.9659258262890683122, 1.000000000000000000, 0.9659258262890683122, 1.000000000000000000, 0.9659258262890683122, 1.000000000000000000, 0.9659258262890683122, 1.000000000000000000, 0.9659258262890683122, 1.000000000000000000, 0.9659258262890683122, 1.000000000000000000, 0.9659258262890683122, 1.000000000000000000, 0.9659258262890683122, 1.000000000000000000, 0.9659258262890683122, 1.000000000000000000, 0.9659258262890683122, 1.000000000000000000, 0.9659258262890683122, 1.000000000000000000, 0.9659258262890683122, 1.000000000000000000, 0.9659258262890683122, 1.000000000000000000, 0.9659258262890683122, 1.000000000000000000, 0.9659258262890683122, 1.000000000000000000, 0.9659258262890683122, 1.000000000000000000, 0.9659258262890683122, 1.000000000000000000, 0.9659258262890683122, 1.000000000000000000, 0.9659258262890683122, 1.000000000000000000, 0.9659258262890683122, 1.000000000000000000, 0.9659258262890683122, 1.000000000000000000, 0.9659258262890683122, 1.000000000000000000, 0.9659258262890683122, 1.000000000000000000, 0.9659258262890683122, 1.000000000000000000, 0.9659258262890683122, 1.000000000000000000, 0.9659258262890683122, 1.000000000000000000, 0.9659258262890683122, 1.000000000000000000, 0.9659258262890683122, 1.000000000000000000, 0.9659258262890683122, 1.000000000000000000, 0.9659258262890683122, 1.000000000000000000, 0.9659258262890683122, 1.000000000000000000, 0.9659258262890683122, 1.000000000000000000, 0.9659258262890683122, 1.000000000000000000, 0.9659258262890683122, 1.000000000000000000, 0.9659258262890683122, 1.000000000000000000, 0.9659258262890683122, 1.000000000000000000, 0.9659258262890683122, 1.000000000000000000, 0.9659258262890683122, 1.000000000000000000, 0.9659258262890683122, 1.000000000000000000, 0.9659258262890683122, 1.000000000000000000, 0.9659258262890683122, 1.000000000000000000, 0.9659258262890683122, 1.000000000000000000, 0.9659258262890683122, 1.000000000000000000, 0.9659258262890683122, 1.000000000000000000, 0.9659258262890683122, 1.000000000000000000, 0.9659258262890683122, 1.000000000000000000, 0.9659258262890683122, 1.000000000000000000, 0.9659258262890683122, 1.000000000000000000, 0.9659258262890683122, 1.000000000000000000, 0.9659258262890683122, 1.000000000000000000, 0.9659258262890683122, 1.000000000000000000, 0.9659258262890683122, 1.000000000000000000, 0.9659258262890683122, 1.000000000000000000, 0.9659258262890683122, 1.000000000000000000, 0.9659258262890683122, 1.000000000000000000, 0.9659258262890683122, 1.000000000000000000, 0.9659258262890683122, 1.000000000000000000, 0.9659258262890683122, 1.000000000000000000, 0.9659258262890683122, 1.000000000000000000, 0.9659258262890683122, 1.000000000000000000, 0.9659258262890683122, 1.000000000000000000, 0.9659258262890683122, 1.000000000000000000, 0.9659258262890683122, 1.000000000000000000, 0.9659258262890683122, 1.000000000000000000, 0.9659258262890683122, 1.000000000000000000, 0.9659258262890683122, 1.000000000000000000, 0.9659258262890683122, 1.000000000000000000, 0.9659258262890683122, 1.000000000000000000, 0.9659258262890683122, 1.000000000000000000, 0.9659258262890683122, 1.000000000000000000, 0.9659258262890683122, 1.000000000000000000, 0.9659258262890683122, 1.000000000000000000, 0.9659258262890683122, 1.000000000000000000, 0.9659258262890683122, 1.000000000000000000, 0.9659258262890683122, 1.000000000000000000, 0.9659258262890683122, 1.000000000000000000) ) ) 
 REPRESENTATION_ITEM ( '' )  SURFACE ( )  );
#51461 = CARTESIAN_POINT ( 'NONE',  ( -0.2427821522309703550, -0.3162353388693405765, 0.4822834645669290543 ) ) ;
#51462 = CARTESIAN_POINT ( 'NONE',  ( -0.2690288713910754526, -0.5511811023622046335, 0.09757992244046803654 ) ) ;
#51463 = CARTESIAN_POINT ( 'NONE',  ( -1.496062992125983815, -0.1870078740157480601, -0.3641732283464567677 ) ) ;
#51464 = CARTESIAN_POINT ( 'NONE',  ( 0.8923884514435701520, -0.5023911411419708095, -0.1820866141732282451 ) ) ;
#51465 = CARTESIAN_POINT ( 'NONE',  ( 0.3740157480314966754, -0.5400638737290844871, 0.3530559997133364547 ) ) ;
#51466 = CARTESIAN_POINT ( 'NONE',  ( 1.351706036745407458, -0.4281496062992127816, -0.4176697321401328100 ) ) ;
#51467 = CARTESIAN_POINT ( 'NONE',  ( 0.6167979002624679463, 0.05413385826771626580, -0.4176697321401330321 ) ) ;
#51468 = CARTESIAN_POINT ( 'NONE',  ( 0.6758530183727039509, 0.1771653543307087075, -0.09757992244046823083 ) ) ;
#51469 = CARTESIAN_POINT ( 'NONE',  ( -1.594488188976377119, 0.1660481256975883668, -0.3530559997133364547 ) ) ;
#51470 = CARTESIAN_POINT ( 'NONE',  ( -1.122047244094487306, 0.1660481256975883668, -0.3530559997133364547 ) ) ;
#51471 = CARTESIAN_POINT ( 'NONE',  ( -0.3805774278215216522, -0.4281496062992127816, -0.4176697321401328100 ) ) ;
#51472 = CARTESIAN_POINT ( 'NONE',  ( 0.3460692066303959757, -0.1998031496062991907, -0.2624671916010499206 ) ) ;
#51473 = CARTESIAN_POINT ( 'NONE',  ( -0.3460692066303960313, 0.1998031496062989965, -2.622703412073490892 ) ) ;
#51474 = CARTESIAN_POINT ( 'NONE',  ( -0.05249343832020938322, -0.6046776061558809534, -0.2411417322834644161 ) ) ;
#51475 = CARTESIAN_POINT ( 'NONE',  ( 1.227034120734908917, -0.5511811023622046335, 0.09757992244046803654 ) ) ;
#51476 = CARTESIAN_POINT ( 'NONE',  ( -0.5577427821522301654, -0.3162353388693405765, 0.4822834645669290543 ) ) ;
#51477 = CARTESIAN_POINT ( 'NONE',  ( 0.4199475065616803948, -0.6046776061558809534, -0.2411417322834644161 ) ) ;
#51478 = CARTESIAN_POINT ( 'NONE',  ( -9.787531504996567848E-17, 0.3996062992125986035, -2.047244094488188892 ) ) ;
#51479 = CARTESIAN_POINT ( 'NONE',  ( -0.3420746716998661618, 0.1974969037888702206, -1.916010498687664043 ) ) ;
#51480 = CARTESIAN_POINT ( 'NONE',  ( -0.3917322834645671215, 0.1049643490035301469, -0.3398950131233596239 ) ) ;
#51481 = CARTESIAN_POINT ( 'NONE',  ( 0.2405786259268995197, -0.1712252042737591184, 5.748956133594166573 ) ) ;
#51482 = CARTESIAN_POINT ( 'NONE',  ( 4.797336870675656522E-17, -0.3917322834645670104, -1.015748031496062964 ) ) ;
#51483 = CARTESIAN_POINT ( 'NONE',  ( -0.8595800524934373854, -0.2845877964562161244, -0.3641732283464567121 ) ) ;
#51484 = CARTESIAN_POINT ( 'NONE',  ( -1.292650918635170010, -0.6692913385826771977, 0.1292274648535927661 ) ) ;
#51485 = CARTESIAN_POINT ( 'NONE',  ( 0.3420746716998660508, 0.1974969037888705814, -2.570209973753280863 ) ) ;
#51486 = CARTESIAN_POINT ( 'NONE',  ( 0.3149606299212606708, -0.1870078740157480879, -0.4822834645669291653 ) ) ;
#51487 = CARTESIAN_POINT ( 'NONE',  ( 1.391076115485564868, -0.6046776061558807314, 0.2411417322834647770 ) ) ;
#51488 = CARTESIAN_POINT ( 'NONE',  ( 0.7742782152230978099, -0.4281496062992124485, 0.4176697321401328655 ) ) ;
#51489 = CARTESIAN_POINT ( 'NONE',  ( -0.4724409448818898682, -8.678599364036362592E-17, -2.716535433070865757 ) ) ;
#51490 = CARTESIAN_POINT ( 'NONE',  ( -0.1070741851644056997, 0.3996062992125986035, -2.211286089238845065 ) ) ;
#51491 = CARTESIAN_POINT ( 'NONE',  ( -0.1049643490035302301, -0.3917322834645671770, -0.6988382134196345907 ) ) ;
#51492 = DIRECTION ( 'NONE',  ( 0.000000000000000000, 0.000000000000000000, -1.000000000000000000 ) ) ;
#51493 = CARTESIAN_POINT ( 'NONE',  ( 0.3412073490813655186, 0.2306618581243848609, 0.2411417322834645549 ) ) ;
#51494 = CARTESIAN_POINT ( 'NONE',  ( 0.3215223097112867578, -0.05778040916215522460, 0.4822834645669289988 ) ) ;
#51495 = CARTESIAN_POINT ( 'NONE',  ( 0.9580052493438326877, -0.004921259842519576551, 0.3153832671262227771 ) ) ;
#51496 = CARTESIAN_POINT ( 'NONE',  ( 1.286089238845145033, -0.6046776061558809534, -0.2411417322834644161 ) ) ;
#51497 = CARTESIAN_POINT ( 'NONE',  ( 0.2867679344610365999, -0.2867679344610365444, -0.1830708661417323746 ) ) ;
#51498 = CARTESIAN_POINT ( 'NONE',  ( 0.4396325459317590445, -0.6692913385826771977, 0.1292274648535927661 ) ) ;
#51499 = CARTESIAN_POINT ( 'NONE',  ( 1.187664041994751285, -0.05778040916215522460, 0.4822834645669289988 ) ) ;
#51500 = CARTESIAN_POINT ( 'NONE',  ( 0.4002624671916016896, -0.05778040916215522460, 0.4822834645669289988 ) ) ;
#51501 = CIRCLE ( 'NONE', #15271, 3.937007874015748143 ) ;
#51502 = CARTESIAN_POINT ( 'NONE',  ( 1.049868766404200349, 0.1283753931104748280, 0.1820866141732283561 ) ) ;
#51503 = CARTESIAN_POINT ( 'NONE',  ( -1.069553805774277722, 0.2952755905511811885, 0.1292274648535926551 ) ) ;
#51504 = CARTESIAN_POINT ( 'NONE',  ( -0.8595800524934373854, -0.3162353388693409650, -0.4822834645669289433 ) ) ;
#51505 = CARTESIAN_POINT ( 'NONE',  ( 1.207349081364829990, -0.6046776061558809534, -0.2411417322834644161 ) ) ;
#51506 = CARTESIAN_POINT ( 'NONE',  ( -0.3392501089628017219, -0.1958661417322836718, -0.7670603674540683592 ) ) ;
#51507 = CARTESIAN_POINT ( 'NONE',  ( -0.2867679344610364334, -0.2867679344610367109, -1.311023622047244430 ) ) ;
#51508 = CARTESIAN_POINT ( 'NONE',  ( -0.3917322834645669549, -0.1049643490035306603, -2.872703412073490448 ) ) ;
#51509 = VERTEX_POINT ( 'NONE', #30670 ) ;
#51510 = CARTESIAN_POINT ( 'NONE',  ( -0.1998031496062991907, -0.3460692066303959757, -0.2230971128608923992 ) ) ;
#51511 = EDGE_LOOP ( 'NONE', ( #70472, #40769, #71820, #63747 ) ) ;
#51512 = CARTESIAN_POINT ( 'NONE',  ( 1.371391076115485941, 0.2952755905511811885, 0.1292274648535926551 ) ) ;
#51513 = CARTESIAN_POINT ( 'NONE',  ( 0.8661417322834652488, -0.1870078740157480601, -0.3641732283464567677 ) ) ;
#51514 = CARTESIAN_POINT ( 'NONE',  ( -0.3460692066303958092, -0.1998031496062994683, -1.627296587926509330 ) ) ;
#51515 = CARTESIAN_POINT ( 'NONE',  ( 1.200787401574803681, 0.07958543189024085140, 0.2665933059059887866 ) ) ;
#51516 = CYLINDRICAL_SURFACE ( 'NONE', #33030, 0.5118110236220472231 ) ;
#51517 = DIRECTION ( 'NONE',  ( -0.000000000000000000, -1.000000000000000000, -0.000000000000000000 ) ) ;
#51518 = DIRECTION ( 'NONE',  ( 1.000000000000000000, 0.000000000000000000, 0.000000000000000000 ) ) ;
#51519 = CARTESIAN_POINT ( 'NONE',  ( -0.3917322834645671215, 0.1049643490035301469, -0.9048556430446195176 ) ) ;
#51520 = VECTOR ( 'NONE', #35704, 39.37007874015748854 ) ;
#51521 = CARTESIAN_POINT ( 'NONE',  ( -1.030183727034119867, -0.2845877964562159024, 0.3641732283464567677 ) ) ;
#51522 = CARTESIAN_POINT ( 'NONE',  ( -1.548556430446193399, 0.1283753931104748280, 0.1820866141732283561 ) ) ;
#51523 = CARTESIAN_POINT ( 'NONE',  ( -1.489501312335957062, -0.05778040916215522460, 0.4822834645669289988 ) ) ;
#51524 = CARTESIAN_POINT ( 'NONE',  ( -0.09186351706036689768, 0.05413385826771626580, -0.4176697321401330321 ) ) ;
#51525 = CARTESIAN_POINT ( 'NONE',  ( 1.555118110236221041, -0.5400638737290844871, 0.3530559997133364547 ) ) ;
#51526 = ORIENTED_EDGE ( 'NONE', *, *, #69760, .T. ) ;
#51527 = EDGE_CURVE ( 'NONE', #64262, #53376, #52621, .T. ) ;
#51528 = CARTESIAN_POINT ( 'NONE',  ( -1.115285832841460767, 1.079194095246727603, -0.1239054779398514883 ) ) ;
#51529 = CARTESIAN_POINT ( 'NONE',  ( 0.3458507752293908943, -0.3458507752293908943, -1.988188976377952777 ) ) ;
#51530 = FACE_OUTER_BOUND ( 'NONE', #31960, .T. ) ;
#51531 = CARTESIAN_POINT ( 'NONE',  ( -0.3030275874994723395, -1.146068349578384814E-15, 0.3627985898453523483 ) ) ;
#51532 = CARTESIAN_POINT ( 'NONE',  ( -0.7874015748031489847, -0.1870078740157480601, -0.3641732283464567677 ) ) ;
#51533 = CARTESIAN_POINT ( 'NONE',  ( -1.240157480314959759, -0.5400638737290845981, -0.3530559997133363437 ) ) ;
#51534 = CARTESIAN_POINT ( 'NONE',  ( 0.5839895013123367340, 0.2952755905511811885, 0.1292274648535926551 ) ) ;
#51535 = ORIENTED_EDGE ( 'NONE', *, *, #4017, .F. ) ;
#51537 = CARTESIAN_POINT ( 'NONE',  ( 0.6955380577427828781, 0.009842519685039144428, -0.3409548833797004797 ) ) ;
#51536 = CARTESIAN_POINT ( 'NONE',  ( -0.03443470937339728616, 0.2755905511811023723, -1.753551325310622078 ) ) ;
#51538 = CARTESIAN_POINT ( 'NONE',  ( 1.141732283464567788, -0.6692913385826771977, 8.415575281601705876E-17 ) ) ;
#51539 = CARTESIAN_POINT ( 'NONE',  ( -1.653543307086613234, -0.1870078740157480879, -0.4822834645669291653 ) ) ;
#51540 = CARTESIAN_POINT ( 'NONE',  ( -0.2867679344610364334, -0.2867679344610368219, -0.6115292406486071419 ) ) ;
#51541 = CARTESIAN_POINT ( 'NONE',  ( -0.5905511811023615998, 0.1771653543307087630, 0.000000000000000000 ) ) ;
#51542 = CARTESIAN_POINT ( 'NONE',  ( -1.141732283464566011, 0.1771653543307087630, 0.000000000000000000 ) ) ;
#51543 = CARTESIAN_POINT ( 'NONE',  ( 0.3917322834645670104, -0.1049643490035303273, -0.9835958005249345604 ) ) ;
#51544 = CARTESIAN_POINT ( 'NONE',  ( -0.7152230971128602510, -0.2845877964562159024, 0.3641732283464567677 ) ) ;
#51545 = CARTESIAN_POINT ( 'NONE',  ( 0.1246719160104994284, -0.5511811023622046335, 0.09757992244046803654 ) ) ;
#51546 = CARTESIAN_POINT ( 'NONE',  ( 0.1837270341207354329, 0.2306618581243848609, 0.2411417322834645549 ) ) ;
#51547 = CARTESIAN_POINT ( 'NONE',  ( -1.122047244094487306, 0.07958543189024071263, -0.2665933059059888421 ) ) ;
#51548 = CARTESIAN_POINT ( 'NONE',  ( -0.2867679344610365999, 0.2867679344610364889, -2.688976377952755570 ) ) ;
#51549 = CARTESIAN_POINT ( 'NONE',  ( 1.023622047244095112, -0.1870078740157480879, -0.4822834645669291653 ) ) ;
#51550 = ADVANCED_FACE ( 'NONE', ( #17642 ), #28782, .T. ) ;
#51551 = CARTESIAN_POINT ( 'NONE',  ( -1.391076115485563314, -0.6046776061558809534, -0.2411417322834644161 ) ) ;
#51552 = CARTESIAN_POINT ( 'NONE',  ( 0.4724409448818897572, -0.1265901696524988906, -1.133202099737532720 ) ) ;
#51553 = CARTESIAN_POINT ( 'NONE',  ( -0.3346456692913377662, -0.5400638737290844871, 0.3530559997133364547 ) ) ;
#51554 = CARTESIAN_POINT ( 'NONE',  ( -0.9645669291338575535, 0.1660481256975883668, -0.3530559997133364547 ) ) ;
#51555 = CARTESIAN_POINT ( 'NONE',  ( 0.9776902887139113929, -0.5511811023622048555, -0.09757992244046775898 ) ) ;
#51556 = CARTESIAN_POINT ( 'NONE',  ( -0.3477690288713905509, -0.5511811023622046335, 0.09757992244046803654 ) ) ;
#51557 = CARTESIAN_POINT ( 'NONE',  ( -0.5446194225721777693, -0.3162353388693409650, -0.4822834645669289433 ) ) ;
#51558 = CARTESIAN_POINT ( 'NONE',  ( -1.371391076115484609, -0.6692913385826771977, 0.1292274648535927661 ) ) ;
#51559 = CARTESIAN_POINT ( 'NONE',  ( -0.4061203303035118561, -2.613618158232546091E-15, -0.3464511005275220379 ) ) ;
#51560 = CARTESIAN_POINT ( 'NONE',  ( 1.082677165354331228, 0.07958543189024071263, -0.2665933059059888421 ) ) ;
#51561 = VECTOR ( 'NONE', #7019, 39.37007874015748854 ) ;
#51562 = CARTESIAN_POINT ( 'NONE',  ( -0.08530183727034056085, -0.3162353388693405765, 0.4822834645669290543 ) ) ;
#51563 = CARTESIAN_POINT ( 'NONE',  ( -1.594488188976377563, -0.5400638737290844871, 0.3530559997133364547 ) ) ;
#51564 = VERTEX_POINT ( 'NONE', #82843 ) ;
#51565 = CARTESIAN_POINT ( 'NONE',  ( -0.1070741851644051862, -0.3996062992125986590, -2.511154855643044748 ) ) ;
#51566 = CARTESIAN_POINT ( 'NONE',  ( -1.017060367454067249, -0.08942795157527998196, 0.3641732283464567121 ) ) ;
#51567 = CARTESIAN_POINT ( 'NONE',  ( 0.7020997375328090762, -0.05778040916215560624, -0.4822834645669293319 ) ) ;
#51568 = CARTESIAN_POINT ( 'NONE',  ( -0.9842519685039365918, -0.5511811023622047445, 6.969142054262312111E-17 ) ) ;
#51569 = CARTESIAN_POINT ( 'NONE',  ( -0.3996062992125984925, -0.1070741851644056858, -1.382545931758530022 ) ) ;
#51570 = CARTESIAN_POINT ( 'NONE',  ( -1.089238845144356427, 0.05413385826771666132, 0.4176697321401328100 ) ) ;
#51571 = CARTESIAN_POINT ( 'NONE',  ( 0.6889763779527566800, -0.5400638737290844871, 0.3530559997133364547 ) ) ;
#51572 = CARTESIAN_POINT ( 'NONE',  ( 0.5577427821522316087, -0.05778040916215522460, 0.4822834645669289988 ) ) ;
#51573 = CARTESIAN_POINT ( 'NONE',  ( -0.4724409448818898682, -8.678599364036362592E-17, -0.03937007874015747977 ) ) ;
#51574 = CARTESIAN_POINT ( 'NONE',  ( -1.469816272965878357, -0.5023911411419708095, -0.1820866141732282451 ) ) ;
#51575 = CARTESIAN_POINT ( 'NONE',  ( 0.3996062992125985480, 2.446882876249141654E-17, -0.8248031496062991907 ) ) ;
#51576 = CARTESIAN_POINT ( 'NONE',  ( -0.1070741851644056997, 0.3996062992125986035, -0.7939632545931758489 ) ) ;
#51577 = AXIS2_PLACEMENT_3D ( 'NONE', #8868, #73689, #34546 ) ;
#51578 = CARTESIAN_POINT ( 'NONE',  ( -0.2891555358219911054, 0.2891555358219909388, -0.4921259842519685179 ) ) ;
#51579 = CARTESIAN_POINT ( 'NONE',  ( 0.3534909051124875967, 1.220709699003109217, -1.724520491472795847 ) ) ;
#51580 = CARTESIAN_POINT ( 'NONE',  ( 1.023622047244095334, -0.1870078740157479769, 0.3641732283464567677 ) ) ;
#51581 = CARTESIAN_POINT ( 'NONE',  ( 0.2755905511811031494, -0.5511811023622047445, 6.969142054262312111E-17 ) ) ;
#51582 = CARTESIAN_POINT ( 'NONE',  ( 0.1115485564304467270, -0.6692913385826773087, -0.1292274648535924053 ) ) ;
#51583 = CARTESIAN_POINT ( 'NONE',  ( 1.404199475065617264, -0.4281496062992124485, 0.4176697321401328655 ) ) ;
#51584 = CARTESIAN_POINT ( 'NONE',  ( 0.3949938075777408852, 0.1058382717557500435, -1.146325459317585338 ) ) ;
#51585 = CARTESIAN_POINT ( 'NONE',  ( 0.4658792650918641698, -0.08942795157528024563, -0.3641732283464568787 ) ) ;
#51586 =( BOUNDED_CURVE ( )  B_SPLINE_CURVE ( 2, ( #36849, #4451, #24623, #67610, #30937, #50290, #18330, #81073, #54959, #75168, #48645, #49881, #9941 ),
 .UNSPECIFIED., .F., .F. ) 
 B_SPLINE_CURVE_WITH_KNOTS ( ( 3, 2, 2, 2, 2, 2, 3 ),
 ( 0.3125000000000000000, 0.3166666666666666519, 0.3208333333333333592, 0.3250000000000000111, 0.3291666666666666630, 0.3333333333333333148, 0.3375000000000000222 ),
 .UNSPECIFIED. ) 
 CURVE ( )  GEOMETRIC_REPRESENTATION_ITEM ( )  RATIONAL_B_SPLINE_CURVE ( ( 1.000000000000000000, 0.9659258262890683122, 1.000000000000000000, 0.9659258262890683122, 1.000000000000000000, 0.9659258262890683122, 1.000000000000000000, 0.9659258262890683122, 1.000000000000000000, 0.9659258262890683122, 1.000000000000000000, 0.9659258262890683122, 1.000000000000000000 ) ) 
 REPRESENTATION_ITEM ( '' )  );
#51587 = CARTESIAN_POINT ( 'NONE',  ( -0.6955380577427815458, 0.05413385826771666132, 0.4176697321401328100 ) ) ;
#51588 = CARTESIAN_POINT ( 'NONE',  ( -1.410761154855641575, -0.3162353388693409650, -0.4822834645669289433 ) ) ;
#51589 = CARTESIAN_POINT ( 'NONE',  ( 0.7545931758530189937, 0.2952755905511810774, -0.1292274648535930714 ) ) ;
#51590 = CARTESIAN_POINT ( 'NONE',  ( 0.1265901696524990294, -0.4724409448818896462, -1.502624671916010346 ) ) ;
#51591 = CARTESIAN_POINT ( 'NONE',  ( -0.7186703366786194591, -2.567464376874931580E-15, -0.4445507791589072832 ) ) ;
#51592 = VERTEX_POINT ( 'NONE', #62239 ) ;
#51593 = ORIENTED_EDGE ( 'NONE', *, *, #81282, .F. ) ;
#51594 = CARTESIAN_POINT ( 'NONE',  ( -1.266404199475064773, -0.3162353388693405765, 0.4822834645669290543 ) ) ;
#51595 = CARTESIAN_POINT ( 'NONE',  ( -0.4921259842519677963, 0.1660481256975883668, -0.3530559997133364547 ) ) ;
#51597 = CARTESIAN_POINT ( 'NONE',  ( -0.8070866141732276899, 0.1660481256975883668, -0.3530559997133364547 ) ) ;
#51596 = CARTESIAN_POINT ( 'NONE',  ( -0.5839895013123351797, -0.5511811023622046335, 0.09757992244046803654 ) ) ;
#51598 = CARTESIAN_POINT ( 'NONE',  ( 0.3392501089628018329, 0.1958661417322835052, -1.943550238023935561 ) ) ;
#51599 = CARTESIAN_POINT ( 'NONE',  ( 0.2087913723976025926, -0.2087913723976025926, 0.1248231986745540617 ) ) ;
#51600 = CARTESIAN_POINT ( 'NONE',  ( 1.627296587926509996, -0.6046776061558807314, 0.2411417322834647770 ) ) ;
#51601 = CARTESIAN_POINT ( 'NONE',  ( -1.207349081364828880, 0.2306618581243847221, -0.2411417322834647770 ) ) ;
#51602 = CARTESIAN_POINT ( 'NONE',  ( 0.2296587926509192634, -0.05778040916215560624, -0.4822834645669293319 ) ) ;
#51603 = CARTESIAN_POINT ( 'NONE',  ( -0.7742782152230962556, -0.4281496062992127816, -0.4176697321401328100 ) ) ;
#51604 = CARTESIAN_POINT ( 'NONE',  ( -0.3392501089628019995, 0.1958661417322832277, -1.593175853018372612 ) ) ;
#51605 = CARTESIAN_POINT ( 'NONE',  ( -0.9645669291338575535, 0.07958543189024071263, -0.2665933059059888421 ) ) ;
#51606 = ORIENTED_EDGE ( 'NONE', *, *, #40415, .T. ) ;
#51607 = CARTESIAN_POINT ( 'NONE',  ( 0.1058382717557500713, -0.3949938075777409408, -1.817585301837270739 ) ) ;
#51608 = ORIENTED_EDGE ( 'NONE', *, *, #41805, .T. ) ;
#51609 = DIRECTION ( 'NONE',  ( 0.000000000000000000, 0.000000000000000000, 1.000000000000000000 ) ) ;
#51610 = CARTESIAN_POINT ( 'NONE',  ( -1.266404199475064773, -0.3162353388693405765, 0.4822834645669290543 ) ) ;
#51611 = CARTESIAN_POINT ( 'NONE',  ( -0.7808398950131222316, -0.3162353388693409650, -0.4822834645669289433 ) ) ;
#51612 = CARTESIAN_POINT ( 'NONE',  ( 0.1998031496062994405, -0.3460692066303958092, -0.09186351706036746667 ) ) ;
#51613 = CARTESIAN_POINT ( 'NONE',  ( -0.9383202099737524282, -0.05778040916215522460, 0.4822834645669289988 ) ) ;
#51614 = CARTESIAN_POINT ( 'NONE',  ( -1.292650918635170010, -0.6692913385826771977, 0.1292274648535927661 ) ) ;
#51615 = CARTESIAN_POINT ( 'NONE',  ( -0.3817677560323433084, -4.005968212718139582E-15, 0.3627989612356165572 ) ) ;
#51616 = CARTESIAN_POINT ( 'NONE',  ( -0.8545558659330622087, 0.02791078216816064370, 0.4328096321851915285 ) ) ;
#51617 = CARTESIAN_POINT ( 'NONE',  ( 0.6102362204724416372, 0.07958543189024071263, -0.2665933059059888421 ) ) ;
#51618 = FACE_OUTER_BOUND ( 'NONE', #34278, .T. ) ;
#51619 = CARTESIAN_POINT ( 'NONE',  ( 0.3917322834645669549, 0.1049643490035304660, -0.3667979002624672802 ) ) ;
#51620 = CARTESIAN_POINT ( 'NONE',  ( -0.3543307086614165824, -0.5511811023622047445, 6.969142054262312111E-17 ) ) ;
#51621 = CARTESIAN_POINT ( 'NONE',  ( -0.6758530183727028406, 0.2952755905511811885, 0.1292274648535926551 ) ) ;
#51622 = CARTESIAN_POINT ( 'NONE',  ( 1.463254593175853824, 0.2952755905511810774, -0.1292274648535930714 ) ) ;
#51623 = CARTESIAN_POINT ( 'NONE',  ( -0.6758530183727028406, 0.2952755905511811885, 0.1292274648535926551 ) ) ;
#51624 = EDGE_CURVE ( 'NONE', #44566, #18339, #75747, .T. ) ;
#51625 = ORIENTED_EDGE ( 'NONE', *, *, #58543, .T. ) ;
#51626 = EDGE_LOOP ( 'NONE', ( #53657, #68428, #71735, #53783, #38168, #47302 ) ) ;
#51627 = CARTESIAN_POINT ( 'NONE',  ( -0.3996062992125986590, 0.1070741851644051723, -1.999343832020997525 ) ) ;
#51628 = CARTESIAN_POINT ( 'NONE',  ( -0.8727034120734901146, -0.3162353388693405765, 0.4822834645669290543 ) ) ;
#51629 = CARTESIAN_POINT ( 'NONE',  ( 1.384514435695538337, -0.6692913385826771977, 0.1292274648535927661 ) ) ;
#51630 = CARTESIAN_POINT ( 'NONE',  ( -1.233595800524933894, 0.1283753931104748280, 0.1820866141732283561 ) ) ;
#51631 = CARTESIAN_POINT ( 'NONE',  ( -1.371391076115484831, 0.2952755905511810774, -0.1292274648535930714 ) ) ;
#51632 = CARTESIAN_POINT ( 'NONE',  ( -0.2362204724409447953, -0.4091458600556404646, -0.8530183727034120755 ) ) ;
#51633 = CARTESIAN_POINT ( 'NONE',  ( 1.877095671717799341, 1.091897865355351271, 0.1662078246829481742 ) ) ;
#51634 = CARTESIAN_POINT ( 'NONE',  ( -0.1958661417322836718, 0.3392501089628017219, -0.1627296587926508609 ) ) ;
#51635 = CARTESIAN_POINT ( 'NONE',  ( 0.3917322834645670104, 2.398668435337828261E-17, -2.092519685039370358 ) ) ;
#51636 = CARTESIAN_POINT ( 'NONE',  ( -0.03937007874015669567, 0.2952755905511811885, 0.000000000000000000 ) ) ;
#51637 = CARTESIAN_POINT ( 'NONE',  ( -1.181102362204723644, -0.1870078740157479769, 0.3641732283464567677 ) ) ;
#51638 = CARTESIAN_POINT ( 'NONE',  ( -0.8005249343832013809, -0.4281496062992124485, 0.4176697321401328655 ) ) ;
#51639 = CARTESIAN_POINT ( 'NONE',  ( 0.2362204724409451007, -0.4091458600556402980, -2.688320209973753538 ) ) ;
#51640 = CARTESIAN_POINT ( 'NONE',  ( -1.213910761154854745, 0.2952755905511810774, -0.1292274648535930714 ) ) ;
#51641 = CARTESIAN_POINT ( 'NONE',  ( -0.8005249343832013809, -0.4281496062992124485, 0.4176697321401328655 ) ) ;
#51642 = CARTESIAN_POINT ( 'NONE',  ( -0.03937007874015669567, -0.6692913385826771977, 8.415575281601705876E-17 ) ) ;
#51643 = VECTOR ( 'NONE', #10238, 39.37007874015748143 ) ;
#51644 = CARTESIAN_POINT ( 'NONE',  ( 0.3420746716998660508, -0.1974969037888704149, -2.543963254593176071 ) ) ;
#51645 = CARTESIAN_POINT ( 'NONE',  ( 0.7152230971128614723, -0.2845877964562161244, -0.3641732283464567121 ) ) ;
#51646 = CARTESIAN_POINT ( 'NONE',  ( -0.7874015748031489847, -0.1870078740157479769, 0.3641732283464567677 ) ) ;
#51647 = CARTESIAN_POINT ( 'NONE',  ( -0.07506541128662616580, 1.068950050010701203, -1.458193486491603741 ) ) ;
#51648 = CARTESIAN_POINT ( 'NONE',  ( 0.8530183727034128527, -0.3690944881889763329, 0.3153832671262228327 ) ) ;
#51649 = CARTESIAN_POINT ( 'NONE',  ( 1.502624671916010790, -0.2845877964562161244, -0.3641732283464567121 ) ) ;
#51650 = CARTESIAN_POINT ( 'NONE',  ( 1.187664041994751285, -0.3162353388693409650, -0.4822834645669289433 ) ) ;
#51651 = CARTESIAN_POINT ( 'NONE',  ( -0.07217847769028787330, -0.08942795157527998196, 0.3641732283464567121 ) ) ;
#51652 = CARTESIAN_POINT ( 'NONE',  ( -0.3917322834645669549, -0.1049643490035306603, -1.297900262467191590 ) ) ;
#51653 = CARTESIAN_POINT ( 'NONE',  ( -1.049868766404198794, -0.6046776061558807314, 0.2411417322834647770 ) ) ;
#51654 = CARTESIAN_POINT ( 'NONE',  ( 1.036745406824147508, -0.4281496062992127816, -0.4176697321401328100 ) ) ;
#51655 = B_SPLINE_CURVE_WITH_KNOTS ( 'NONE', 3,
 ( #71745, #72576, #1052, #1876, #14923, #15342, #27952, #26706 ),
 .UNSPECIFIED., .F., .F.,
 ( 4, 2, 2, 4 ),
 ( 0.05656618697110752519, 0.05899478853696744213, 0.06020908931989741447, 0.06142339010282737988 ),
 .UNSPECIFIED. ) ;
#51656 = CARTESIAN_POINT ( 'NONE',  ( 0.3458507752293908943, 0.3458507752293908943, 0.1003937007874015769 ) ) ;
#51657 = CARTESIAN_POINT ( 'NONE',  ( -0.4199475065616791736, -0.5023911411419708095, 0.1820866141732285504 ) ) ;
#51658 = CARTESIAN_POINT ( 'NONE',  ( -0.4037097067573596210, -2.567464376874931580E-15, -0.4445507791589072832 ) ) ;
#51659 = CARTESIAN_POINT ( 'NONE',  ( 0.4790026246719168435, -0.3162353388693409650, -0.4822834645669289433 ) ) ;
#51660 = DIRECTION ( 'NONE',  ( 9.381338752702771457E-17, -0.6427876096865352551, 0.7660444431189814551 ) ) ;
#51661 = CARTESIAN_POINT ( 'NONE',  ( 0.8070866141732288002, 0.07958543189024085140, 0.2665933059059887866 ) ) ;
#51662 = CARTESIAN_POINT ( 'NONE',  ( 0.006561679790026889343, -0.08942795157527998196, 0.3641732283464567121 ) ) ;
#51663 = CARTESIAN_POINT ( 'NONE',  ( -0.08530183727034056085, -0.3162353388693405765, 0.4822834645669290543 ) ) ;
#51664 = CARTESIAN_POINT ( 'NONE',  ( -1.167979002624671470, -0.4281496062992127816, -0.4176697321401328100 ) ) ;
#51665 = CARTESIAN_POINT ( 'NONE',  ( -0.7874015748031489847, -0.1870078740157480601, -0.3641732283464567677 ) ) ;
#51666 = DIRECTION ( 'NONE',  ( -1.000000000000000000, 0.000000000000000000, 0.000000000000000000 ) ) ;
#51667 = B_SPLINE_CURVE_WITH_KNOTS ( 'NONE', 1,
 ( #42605, #16966 ),
 .UNSPECIFIED., .F., .F.,
 ( 2, 2 ),
 ( 0.0007499999999999989314, 0.002999999999999998328 ),
 .UNSPECIFIED. ) ;
#51668 = CARTESIAN_POINT ( 'NONE',  ( -1.010498687664041384, 0.05413385826771666132, 0.4176697321401328100 ) ) ;
#51669 = CARTESIAN_POINT ( 'NONE',  ( 0.2925321140481932369, -0.2925321140481931814, -0.9625984251968502381 ) ) ;
#51670 = CARTESIAN_POINT ( 'NONE',  ( -0.3917322834645669549, -0.1049643490035306603, -2.492782152230970993 ) ) ;
#51671 = CARTESIAN_POINT ( 'NONE',  ( 0.1968503937007881344, 0.1771653543307087630, 0.000000000000000000 ) ) ;
#51672 = CARTESIAN_POINT ( 'NONE',  ( -0.7283464566929126471, -0.5400638737290844871, 0.3530559997133364547 ) ) ;
#51673 = CARTESIAN_POINT ( 'NONE',  ( -1.148293963254592542, 0.2952755905511811885, 0.1292274648535926551 ) ) ;
#51674 = CARTESIAN_POINT ( 'NONE',  ( -1.102362204724408601, -0.1870078740157480601, -0.3641732283464567677 ) ) ;
#51675 = CARTESIAN_POINT ( 'NONE',  ( 1.653543307086614789, -0.1870078740157479769, 0.4822834645669291653 ) ) ;
#51676 = EDGE_CURVE ( 'NONE', #29291, #31839, #38137, .T. ) ;
#51677 = CARTESIAN_POINT ( 'NONE',  ( -0.8989501312335946848, -0.5511811023622046335, 0.09757992244046803654 ) ) ;
#51678 = CARTESIAN_POINT ( 'NONE',  ( -1.443569553805773564, -0.5023911411419708095, 0.1820866141732285504 ) ) ;
#51679 = CARTESIAN_POINT ( 'NONE',  ( 1.443569553805774897, 0.2306618581243848609, 0.2411417322834645549 ) ) ;
#51680 = CARTESIAN_POINT ( 'NONE',  ( -0.4744094488189005698, 1.553452312607695118, 1.016821367227982442 ) ) ;
#51681 = CARTESIAN_POINT ( 'NONE',  ( 0.3392501089628018329, 0.1958661417322835607, -2.017735851214910170 ) ) ;
#51682 = ORIENTED_EDGE ( 'NONE', *, *, #3380, .T. ) ;
#51683 = ADVANCED_FACE ( 'NONE', ( #57562 ), #46066, .T. ) ;
#51684 = CARTESIAN_POINT ( 'NONE',  ( -0.2258813529811895260, -1.094630224652485432E-15, 0.4281993546915541238 ) ) ;
#51685 = CARTESIAN_POINT ( 'NONE',  ( -1.646981627296586703, -0.3162353388693409650, -0.4822834645669289433 ) ) ;
#51686 = CARTESIAN_POINT ( 'NONE',  ( -1.384514435695537005, 0.2952755905511811885, 0.1292274648535926551 ) ) ;
#51687 = CARTESIAN_POINT ( 'NONE',  ( 1.102362204724410155, -0.1870078740157479769, 0.4822834645669291653 ) ) ;
#51688 = CARTESIAN_POINT ( 'NONE',  ( -0.1049643490035302024, -0.3917322834645671215, -1.889107611548556109 ) ) ;
#51689 = CARTESIAN_POINT ( 'NONE',  ( 1.660104986876641320, -0.08942795157527998196, 0.3641732283464567121 ) ) ;
#51690 = CARTESIAN_POINT ( 'NONE',  ( 0.7020997375328090762, -0.3162353388693405765, 0.4822834645669290543 ) ) ;
#51691 = CARTESIAN_POINT ( 'NONE',  ( -0.07217847769028787330, -0.05778040916215522460, 0.4822834645669289988 ) ) ;
#51692 = CARTESIAN_POINT ( 'NONE',  ( 2.795275590551181466, 2.204724409448820310, 0.000000000000000000 ) ) ;
#51693 = CARTESIAN_POINT ( 'NONE',  ( 0.1070741851644054637, -0.3996062992125984925, -2.681758530183727451 ) ) ;
#51694 = CARTESIAN_POINT ( 'NONE',  ( 0.7611548556430451917, -0.5023911411419708095, 0.1820866141732285504 ) ) ;
#51695 = CARTESIAN_POINT ( 'NONE',  ( -0.2925321140481930704, -0.2925321140481933480, -1.318897637795275690 ) ) ;
#51696 = ORIENTED_EDGE ( 'NONE', *, *, #40336, .T. ) ;
#51698 = CARTESIAN_POINT ( 'NONE',  ( 4.797336870675656522E-17, -0.3917322834645670659, -0.07547863336714100146 ) ) ;
#51697 = VECTOR ( 'NONE', #50291, 39.37007874015748143 ) ;
#51699 = ORIENTED_EDGE ( 'NONE', *, *, #39798, .T. ) ;
#51700 = CARTESIAN_POINT ( 'NONE',  ( -0.09186351706036689768, 0.05413385826771626580, -0.4176697321401330321 ) ) ;
#51701 = CARTESIAN_POINT ( 'NONE',  ( -1.502624671916009680, -0.3162353388693405765, 0.4822834645669290543 ) ) ;
#51702 = CARTESIAN_POINT ( 'NONE',  ( 0.7480314960629927956, 0.2952755905511811885, 0.000000000000000000 ) ) ;
#51703 = CARTESIAN_POINT ( 'NONE',  ( 1.332020997375329197, -0.3162353388693405765, 0.4822834645669290543 ) ) ;
#51704 = CARTESIAN_POINT ( 'NONE',  ( 1.305774278215223960, 0.2952755905511810774, -0.1292274648535930714 ) ) ;
#51705 = CARTESIAN_POINT ( 'NONE',  ( -0.6036745406824141069, -0.6046776061558809534, -0.2411417322834644161 ) ) ;
#51706 = CARTESIAN_POINT ( 'NONE',  ( 0.06561679790026316017, 0.05413385826771626580, -0.4176697321401330321 ) ) ;
#51707 = CARTESIAN_POINT ( 'NONE',  ( 1.423884514435696191, -0.05778040916215522460, 0.4822834645669289988 ) ) ;
#51708 = CARTESIAN_POINT ( 'NONE',  ( 1.496062992125984703, -0.1870078740157480879, -0.4822834645669291653 ) ) ;
#51709 = EDGE_CURVE ( 'NONE', #83292, #49627, #8491, .T. ) ;
#51710 = CARTESIAN_POINT ( 'NONE',  ( 1.194225721784777594, 0.05413385826771666132, 0.4176697321401328100 ) ) ;
#51711 = CARTESIAN_POINT ( 'NONE',  ( -0.1706036745406816491, -0.4281496062992124485, 0.4176697321401328655 ) ) ;
#51712 = CARTESIAN_POINT ( 'NONE',  ( 0.2867679344610365999, 0.2867679344610365999, -0.1299212598425196485 ) ) ;
#51713 = CARTESIAN_POINT ( 'NONE',  ( 0.5708661417322842269, 0.07958543189024085140, 0.2665933059059887866 ) ) ;
#51714 = VERTEX_POINT ( 'NONE', #59475 ) ;
#51715 = CARTESIAN_POINT ( 'NONE',  ( 0.1974969037888706369, -0.3420746716998659953, -0.5643044619422573627 ) ) ;
#51716 = VERTEX_POINT ( 'NONE', #19507 ) ;
#51717 = CARTESIAN_POINT ( 'NONE',  ( -0.6036745406824141069, 0.1283753931104748280, 0.1820866141732283561 ) ) ;
#51718 = CARTESIAN_POINT ( 'NONE',  ( 0.6299212598425341092, 2.165354330708662012, -3.937007874015759690 ) ) ;
#51719 = CARTESIAN_POINT ( 'NONE',  ( 0.1246719160104994284, -0.6692913385826771977, 0.1292274648535927661 ) ) ;
#51720 = CARTESIAN_POINT ( 'NONE',  ( -0.04593175853018302557, -0.6692913385826773087, -0.1292274648535924053 ) ) ;
#51721 = CARTESIAN_POINT ( 'NONE',  ( -1.023622047244094002, -0.1870078740157480879, -0.4822834645669291653 ) ) ;
#51722 = EDGE_CURVE ( 'NONE', #52853, #34044, #71278, .T. ) ;
#51723 = CARTESIAN_POINT ( 'NONE',  ( -0.1049643490035307158, 0.3917322834645670104, -1.578103305283151681 ) ) ;
#51724 = CARTESIAN_POINT ( 'NONE',  ( -1.286089238845143479, 0.2306618581243847221, -0.2411417322834647770 ) ) ;
#51725 = CARTESIAN_POINT ( 'NONE',  ( 0.04852021190738116385, 1.072605569307989226, 0.2413719949950524080 ) ) ;
#51726 = CARTESIAN_POINT ( 'NONE',  ( 0.8530183727034126306, -0.004921259842519870586, -0.3153832671262229437 ) ) ;
#51727 = CARTESIAN_POINT ( 'NONE',  ( 0.3215223097112867578, -0.3162353388693409650, -0.4822834645669289433 ) ) ;
#51728 = CARTESIAN_POINT ( 'NONE',  ( 0.5577427821522316087, -0.05778040916215522460, 0.4822834645669289988 ) ) ;
#51729 = CARTESIAN_POINT ( 'NONE',  ( -0.3460692066303960868, 0.1998031496062990242, -1.128608923884514503 ) ) ;
#51730 = LINE ( 'NONE', #1668, #11699 ) ;
#51731 = CARTESIAN_POINT ( 'NONE',  ( -0.1998031496062991630, -0.3460692066303959202, -0.7723097112860892732 ) ) ;
#51732 = CARTESIAN_POINT ( 'NONE',  ( -0.1998031496062991630, -0.3460692066303959202, -0.2998687664041995160 ) ) ;
#51733 = CARTESIAN_POINT ( 'NONE',  ( -0.006561679790025524116, -0.3162353388693405765, 0.4822834645669290543 ) ) ;
#51734 = CARTESIAN_POINT ( 'NONE',  ( -0.2925321140481932924, 0.2925321140481931814, -2.854330708661417138 ) ) ;
#51735 = ADVANCED_FACE ( 'NONE', ( #26234 ), #56990, .F. ) ;
#51736 = CARTESIAN_POINT ( 'NONE',  ( -0.3917322834645671215, 0.1049643490035301469, -2.007217847769029007 ) ) ;
#51737 = CARTESIAN_POINT ( 'NONE',  ( -1.391076115485563314, -0.5023911411419708095, -0.1820866141732282451 ) ) ;
#51738 = CARTESIAN_POINT ( 'NONE',  ( 1.404199475065617264, -0.4281496062992124485, 0.4176697321401328655 ) ) ;
#51739 = CARTESIAN_POINT ( 'NONE',  ( 1.522309711286089939, 0.2306618581243848609, 0.2411417322834645549 ) ) ;
#51740 = CARTESIAN_POINT ( 'NONE',  ( 0.3871391076115493490, -0.2845877964562159024, 0.3641732283464567677 ) ) ;
#51741 = CARTESIAN_POINT ( 'NONE',  ( 0.6036745406824153282, -0.6046776061558807314, 0.2411417322834647770 ) ) ;
#51742 = CARTESIAN_POINT ( 'NONE',  ( 5.785732909357575061E-17, -0.4724409448818898682, -1.572834645669291431 ) ) ;
#51743 = CARTESIAN_POINT ( 'NONE',  ( 0.5118110236220480003, -0.5511811023622047445, 6.969142054262312111E-17 ) ) ;
#51744 = CARTESIAN_POINT ( 'NONE',  ( 0.07874015748031558404, -0.1870078740157480879, -0.4822834645669291653 ) ) ;
#51745 = CARTESIAN_POINT ( 'NONE',  ( -0.3420746716998662729, 0.1974969037888702206, -1.362860892388451539 ) ) ;
#51746 = CARTESIAN_POINT ( 'NONE',  ( -1.286089238845143479, -0.6046776061558807314, 0.2411417322834647770 ) ) ;
#51747 = CARTESIAN_POINT ( 'NONE',  ( 0.4527559055118117182, -0.4536011799217367080, 0.2665933059059888421 ) ) ;
#51748 = CARTESIAN_POINT ( 'NONE',  ( 0.3277333542595164406, 0.004960608223778823628, 0.3437734562760190182 ) ) ;
#51749 = CARTESIAN_POINT ( 'NONE',  ( -0.6233595800524928121, -0.05778040916215522460, 0.4822834645669289988 ) ) ;
#51750 = CARTESIAN_POINT ( 'NONE',  ( -0.3215223097112853146, -0.08942795157528024563, -0.3641732283464568787 ) ) ;
#51751 = CARTESIAN_POINT ( 'NONE',  ( 0.1181102362204724254, 0.04921259842519689481, -0.08523872084492506440 ) ) ;
#51752 = CARTESIAN_POINT ( 'NONE',  ( -0.7349081364829390672, 0.2306618581243847221, -0.2411417322834647770 ) ) ;
#51753 = CARTESIAN_POINT ( 'NONE',  ( -0.06561679790026180015, 0.05413385826771666132, 0.4176697321401328100 ) ) ;
#51754 = CARTESIAN_POINT ( 'NONE',  ( 0.2821522309711292364, -0.5511811023622046335, 0.09757992244046803654 ) ) ;
#51755 = CARTESIAN_POINT ( 'NONE',  ( -9.787531504996566615E-17, 0.3996062992125985480, -1.966535433070866201 ) ) ;
#51756 = CARTESIAN_POINT ( 'NONE',  ( 0.03937007874015833325, -0.6692913385826771977, 8.415575281601705876E-17 ) ) ;
#51757 = CARTESIAN_POINT ( 'NONE',  ( 0.3917322834645669549, 2.398668435337827645E-17, -1.930426878443882943 ) ) ;
#51758 = VECTOR ( 'NONE', #21164, 39.37007874015748143 ) ;
#51759 = CARTESIAN_POINT ( 'NONE',  ( 0.7217847769028878924, -0.004921259842519576551, 0.3153832671262227771 ) ) ;
#51760 = CARTESIAN_POINT ( 'NONE',  ( 1.535433070866142335, -0.6692913385826771977, 8.415575281601705876E-17 ) ) ;
#51761 = CARTESIAN_POINT ( 'NONE',  ( -0.9908136482939626788, -0.5511811023622048555, -0.09757992244046775898 ) ) ;
#51762 = VECTOR ( 'NONE', #83198, 39.37007874015748143 ) ;
#51763 = CARTESIAN_POINT ( 'NONE',  ( -1.305774278215222184, -0.5511811023622048555, -0.09757992244046775898 ) ) ;
#51764 = CARTESIAN_POINT ( 'NONE',  ( -0.6102362204724400829, -0.5400638737290845981, -0.3530559997133363437 ) ) ;
#51765 = CARTESIAN_POINT ( 'NONE',  ( -0.2427821522309703550, -0.05778040916215560624, -0.4822834645669293319 ) ) ;
#51766 = CARTESIAN_POINT ( 'NONE',  ( 0.5643044619422579178, -0.004921259842519576551, 0.3153832671262227771 ) ) ;
#51767 = CARTESIAN_POINT ( 'NONE',  ( -0.1265901696524993347, 0.4724409448818896462, -2.368766404199475151 ) ) ;
#51768 = CARTESIAN_POINT ( 'NONE',  ( 1.108923884514436242, -0.08942795157527998196, 0.3641732283464567121 ) ) ;
#51769 = CARTESIAN_POINT ( 'NONE',  ( 0.6561679790026253567, -0.6046776061558809534, -0.2411417322834644161 ) ) ;
#51770 = CARTESIAN_POINT ( 'NONE',  ( -0.3996062992125986590, 0.1070741851644051723, 0.2053805774278214813 ) ) ;
#51771 = CARTESIAN_POINT ( 'NONE',  ( -0.2821522309711278487, 0.2952755905511811885, 0.1292274648535926551 ) ) ;
#51772 = CARTESIAN_POINT ( 'NONE',  ( 0.2867679344610365999, -0.2867679344610365444, -1.285433070866141669 ) ) ;
#51773 = CARTESIAN_POINT ( 'NONE',  ( 1.312335958005249825, 0.1283753931104746893, -0.1820866141732285504 ) ) ;
#51774 = CARTESIAN_POINT ( 'NONE',  ( 0.4855643044619430415, -0.4281496062992127816, -0.4176697321401328100 ) ) ;
#51775 = CARTESIAN_POINT ( 'NONE',  ( -0.04593175853018302557, 0.2952755905511811885, 0.1292274648535926551 ) ) ;
#51776 = CARTESIAN_POINT ( 'NONE',  ( -0.3983403474834782965, -0.03178304480584832892, -1.220472440944881942 ) ) ;
#51777 = CARTESIAN_POINT ( 'NONE',  ( 0.4593175853018380828, -0.004921259842519870586, -0.3153832671262229437 ) ) ;
#51778 = CARTESIAN_POINT ( 'NONE',  ( 0.6758530183727039509, -0.6692913385826771977, 0.1292274648535927661 ) ) ;
#51779 = EDGE_CURVE ( 'NONE', #65845, #14996, #5749, .T. ) ;
#51780 = CARTESIAN_POINT ( 'NONE',  ( -0.3083989501312330295, -0.08942795157527998196, 0.3641732283464567121 ) ) ;
#51781 = CARTESIAN_POINT ( 'NONE',  ( -0.8005249343832011588, 0.05413385826771626580, -0.4176697321401330321 ) ) ;
#51782 = CARTESIAN_POINT ( 'NONE',  ( 0.8464566929133864326, 0.1660481256975883391, -0.3530559997133364547 ) ) ;
#51783 = CARTESIAN_POINT ( 'NONE',  ( -0.3018372703412066094, 0.05413385826771666132, 0.4176697321401328100 ) ) ;
#51784 = CARTESIAN_POINT ( 'NONE',  ( -1.213910761154854745, -0.6692913385826771977, 0.1292274648535927661 ) ) ;
#51785 = CARTESIAN_POINT ( 'NONE',  ( -0.8792650918635160906, -0.004921259842519870586, -0.3153832671262229437 ) ) ;
#51786 = CARTESIAN_POINT ( 'NONE',  ( 0.5446194225721792126, -0.05778040916215560624, -0.4822834645669293319 ) ) ;
#51787 = CARTESIAN_POINT ( 'NONE',  ( -1.181102362204723644, -0.1870078740157480879, -0.4822834645669291653 ) ) ;
#51788 = CARTESIAN_POINT ( 'NONE',  ( -0.2755905511811015396, -0.6692913385826771977, 8.415575281601705876E-17 ) ) ;
#51789 = DIRECTION ( 'NONE',  ( 1.000000000000000000, -0.000000000000000000, -0.000000000000000000 ) ) ;
#51791 = CARTESIAN_POINT ( 'NONE',  ( 1.371391076115485719, -0.6692913385826773087, -0.1292274648535924053 ) ) ;
#51790 = CARTESIAN_POINT ( 'NONE',  ( 1.660104986876641320, -0.05778040916215522460, 0.4822834645669289988 ) ) ;
#51792 = CARTESIAN_POINT ( 'NONE',  ( 1.233595800524935227, 0.2306618581243847221, -0.2411417322834647770 ) ) ;
#51793 = CARTESIAN_POINT ( 'NONE',  ( -0.1958661417322836718, 0.3392501089628017219, -2.524934383202099397 ) ) ;
#51794 = CARTESIAN_POINT ( 'NONE',  ( 0.5314960629921294810, 0.000000000000000000, -0.9881811337016621621 ) ) ;
#51795 = CARTESIAN_POINT ( 'NONE',  ( -1.456692913385826182, -0.6692913385826771977, 8.415575281601705876E-17 ) ) ;
#51796 = CARTESIAN_POINT ( 'NONE',  ( -0.1265901696524993347, 0.4724409448818895907, -0.6364829396325458744 ) ) ;
#51797 = CARTESIAN_POINT ( 'NONE',  ( 0.3996062992125986035, 2.446882876249141962E-17, 0.03937007874015746589 ) ) ;
#51798 = ORIENTED_EDGE ( 'NONE', *, *, #28945, .F. ) ;
#51799 = CARTESIAN_POINT ( 'NONE',  ( 0.01968503937007957949, -0.4536011799217368745, -0.2665933059059886201 ) ) ;
#51800 = CARTESIAN_POINT ( 'NONE',  ( 0.1958661417322834775, 0.3392501089628018884, -1.711286089238845287 ) ) ;
#51801 = ORIENTED_EDGE ( 'NONE', *, *, #57736, .T. ) ;
#51802 = CARTESIAN_POINT ( 'NONE',  ( 0.3149606299212603933, -0.1870078740157479769, 0.4822834645669291653 ) ) ;
#51803 = CARTESIAN_POINT ( 'NONE',  ( 0.4593175853018379162, -0.4281496062992124485, 0.4176697321401328655 ) ) ;
#51804 = CARTESIAN_POINT ( 'NONE',  ( 0.09156050430091122738, 0.3808816823641256732, -2.755905511811024056 ) ) ;
#51805 = CARTESIAN_POINT ( 'NONE',  ( 0.000000000000000000, 0.000000000000000000, 0.000000000000000000 ) ) ;
#51806 = CARTESIAN_POINT ( 'NONE',  ( -0.3477690288713902178, 0.1771653543307087075, -0.09757992244046823083 ) ) ;
#51807 = CARTESIAN_POINT ( 'NONE',  ( -3.937007874015748143, 1.724409448818897905, 0.6299212598425196763 ) ) ;
#51808 = CARTESIAN_POINT ( 'NONE',  ( 0.7611548556430454138, 0.2306618581243847221, -0.2411417322834647770 ) ) ;
#51809 = CARTESIAN_POINT ( 'NONE',  ( 1.043307086614173818, -0.4536011799217368745, -0.2665933059059886201 ) ) ;
#51810 = CARTESIAN_POINT ( 'NONE',  ( -0.2296587926509179312, -0.05778040916215522460, 0.4822834645669289988 ) ) ;
#51811 = CARTESIAN_POINT ( 'NONE',  ( 0.1049643490035304522, -0.3917322834645668994, -1.267697219651231499 ) ) ;
#51812 = CARTESIAN_POINT ( 'NONE',  ( -0.8595800524934373854, -0.05778040916215522460, 0.4822834645669289988 ) ) ;
#51813 = CARTESIAN_POINT ( 'NONE',  ( -1.128608923884513837, -0.5023911411419708095, 0.1820866141732285504 ) ) ;
#51814 = CARTESIAN_POINT ( 'NONE',  ( -1.036745406824146176, 0.05413385826771626580, -0.4176697321401330321 ) ) ;
#51815 = CARTESIAN_POINT ( 'NONE',  ( 1.364829396325460076, 0.2306618581243848609, 0.2411417322834645549 ) ) ;
#51816 = CARTESIAN_POINT ( 'NONE',  ( 0.4847769261806181285, 1.968503937007873850, -0.4915354330708656128 ) ) ;
#51817 = EDGE_LOOP ( 'NONE', ( #25134, #2877, #48655, #37564, #75030 ) ) ;
#51818 = CARTESIAN_POINT ( 'NONE',  ( 0.1049643490035304799, -0.3917322834645670104, -2.601725352527246127 ) ) ;
#51819 = CARTESIAN_POINT ( 'NONE',  ( 0.05905511811023709395, -0.5400638737290844871, 0.3530559997133364547 ) ) ;
#51820 = VERTEX_POINT ( 'NONE', #34227 ) ;
#51821 = CIRCLE ( 'NONE', #18263, 3.543307086614173151 ) ;
#51822 = CARTESIAN_POINT ( 'NONE',  ( -0.9645669291338575535, -0.5400638737290844871, 0.3530559997133364547 ) ) ;
#51823 = CARTESIAN_POINT ( 'NONE',  ( 1.528871391076116026, -0.6692913385826773087, -0.1292274648535924053 ) ) ;
#51824 = CARTESIAN_POINT ( 'NONE',  ( 1.391076115485564868, -0.6046776061558807314, 0.2411417322834647770 ) ) ;
#51825 = CARTESIAN_POINT ( 'NONE',  ( 0.3543307086614179147, 0.2952755905511811885, 0.000000000000000000 ) ) ;
#51826 = CARTESIAN_POINT ( 'NONE',  ( 0.02624671916010564918, -0.6046776061558809534, -0.2411417322834644161 ) ) ;
#51827 = CARTESIAN_POINT ( 'NONE',  ( 0.1958661417322836440, -0.3392501089628017219, -1.908792650918635259 ) ) ;
#51828 = CARTESIAN_POINT ( 'NONE',  ( -1.279527559055116948, -0.5400638737290844871, 0.3530559997133364547 ) ) ;
#51829 = CARTESIAN_POINT ( 'NONE',  ( -0.1246719160104980823, -0.6692913385826773087, -0.1292274648535924053 ) ) ;
#51830 = CARTESIAN_POINT ( 'NONE',  ( -0.2952755905511803003, -0.4536011799217368745, -0.2665933059059886201 ) ) ;
#51831 = CARTESIAN_POINT ( 'NONE',  ( -1.614173228346457378, 0.7166040191147894367, 0.1372047244094476981 ) ) ;
#51832 = CARTESIAN_POINT ( 'NONE',  ( 1.364829396325460076, 0.2306618581243848609, 0.2411417322834645549 ) ) ;
#51833 = CARTESIAN_POINT ( 'NONE',  ( -0.6692913385826764205, -0.6692913385826771977, 8.415575281601705876E-17 ) ) ;
#51834 = CARTESIAN_POINT ( 'NONE',  ( -0.5314960629921393620, 2.755905511811024056, 3.821484228344191880 ) ) ;
#51835 = B_SPLINE_CURVE_WITH_KNOTS ( 'NONE', 3,
 ( #10202, #35871, #55204, #80912 ),
 .UNSPECIFIED., .F., .F.,
 ( 4, 4 ),
 ( 3.593986969189856268E-07, 0.001287825409103294464 ),
 .UNSPECIFIED. ) ;
#51836 = CARTESIAN_POINT ( 'NONE',  ( 1.207349081364829990, -0.6046776061558809534, -0.2411417322834644161 ) ) ;
#51837 = PLANE ( 'NONE',  #40204 ) ;
#51838 = ORIENTED_EDGE ( 'NONE', *, *, #19393, .F. ) ;
#51839 = ORIENTED_EDGE ( 'NONE', *, *, #13707, .T. ) ;
#51840 = CARTESIAN_POINT ( 'NONE',  ( 0.3871391076115493490, -0.3162353388693405765, 0.4822834645669290543 ) ) ;
#51841 = CARTESIAN_POINT ( 'NONE',  ( -0.4855643044619415427, -0.3690944881889763329, 0.3153832671262228327 ) ) ;
#51843 = CARTESIAN_POINT ( 'NONE',  ( 0.5314960629921324786, 2.716535433070866645, -1.854472803289050509 ) ) ;
#51842 = CARTESIAN_POINT ( 'NONE',  ( 1.535433070866142558, 0.1771653543307087630, 0.000000000000000000 ) ) ;
#51844 = CARTESIAN_POINT ( 'NONE',  ( -0.4091458600556405756, 0.2362204724409446288, -0.4179790026246719137 ) ) ;
#51845 = CARTESIAN_POINT ( 'NONE',  ( 1.627296587926509996, -0.5023911411419708095, 0.1820866141732285504 ) ) ;
#51846 = CARTESIAN_POINT ( 'NONE',  ( 1.332020997375328974, -0.05778040916215560624, -0.4822834645669293319 ) ) ;
#51847 = CARTESIAN_POINT ( 'NONE',  ( 0.1974969037888706092, -0.3420746716998660508, -0.3261154855643044748 ) ) ;
#51848 = CARTESIAN_POINT ( 'NONE',  ( 0.07874015748031558404, -0.1870078740157480879, -0.4822834645669291653 ) ) ;
#51849 = CARTESIAN_POINT ( 'NONE',  ( 0.1474713956048451791, 8.471767977567108961E-16, -0.4445507791589058955 ) ) ;
#51850 = CARTESIAN_POINT ( 'NONE',  ( -1.443569553805773564, -0.6046776061558807314, 0.2411417322834647770 ) ) ;
#51851 = CARTESIAN_POINT ( 'NONE',  ( 0.06561679790026316017, 0.05413385826771626580, -0.4176697321401330321 ) ) ;
#51852 = CARTESIAN_POINT ( 'NONE',  ( -9.674558042662122972E-17, 0.3949938075777409963, -0.07677165354330710290 ) ) ;
#51853 = CARTESIAN_POINT ( 'NONE',  ( 1.561679790026247350, 0.05413385826771626580, -0.4176697321401330321 ) ) ;
#51854 = CARTESIAN_POINT ( 'NONE',  ( 0.3477690288713918276, 0.2952755905511811885, 0.1292274648535926551 ) ) ;
#51855 = CARTESIAN_POINT ( 'NONE',  ( 0.9120734908136490793, 0.1771653543307087075, -0.09757992244046823083 ) ) ;
#51856 = DIRECTION ( 'NONE',  ( 0.000000000000000000, 0.000000000000000000, 1.000000000000000000 ) ) ;
#51857 = CARTESIAN_POINT ( 'NONE',  ( 0.6496062992125991586, -0.4536011799217368745, -0.2665933059059886201 ) ) ;
#51858 = CARTESIAN_POINT ( 'NONE',  ( -1.227034120734907141, -0.6692913385826773087, -0.1292274648535924053 ) ) ;
#51859 = CARTESIAN_POINT ( 'NONE',  ( 0.2925321140481932369, 0.2925321140481932369, -0.8444881889763780070 ) ) ;
#51860 = CARTESIAN_POINT ( 'NONE',  ( 1.266404199475066328, -0.3162353388693409650, -0.4822834645669289433 ) ) ;
#51861 = CARTESIAN_POINT ( 'NONE',  ( -9.594673741351313045E-17, 0.3917322834645670104, -0.7795275590551180578 ) ) ;
#51862 = CIRCLE ( 'NONE', #19603, 0.1771653543307085410 ) ;
#51863 = TOROIDAL_SURFACE ( 'NONE', #42444, 3.858267716535433323, 0.07874015748031495954 ) ;
#51865 = CARTESIAN_POINT ( 'NONE',  ( 0.3458507752293908943, -0.3458507752293908943, -0.4901574803149605919 ) ) ;
#51864 = CARTESIAN_POINT ( 'NONE',  ( 0.7611548556430454138, 0.2306618581243847221, -0.2411417322834647770 ) ) ;
#51866 = LINE ( 'NONE', #59033, #32141 ) ;
#51867 = CARTESIAN_POINT ( 'NONE',  ( 0.3018372703412079971, -0.3690944881889763329, 0.3153832671262228327 ) ) ;
#51868 = CARTESIAN_POINT ( 'NONE',  ( 0.4527559055118117182, 0.1660481256975883668, -0.3530559997133364547 ) ) ;
#51869 = CARTESIAN_POINT ( 'NONE',  ( -0.2087913723976025926, 0.2087913723976025371, 0.1248231986745539646 ) ) ;
#51870 = CARTESIAN_POINT ( 'NONE',  ( -1.102362204724408601, -0.1870078740157479769, 0.3641732283464567677 ) ) ;
#51871 = CARTESIAN_POINT ( 'NONE',  ( -1.082677165354329896, 0.1660481256975885056, 0.3530559997133364547 ) ) ;
#51872 = CARTESIAN_POINT ( 'NONE',  ( 1.023622047244095334, -0.1870078740157479769, 0.4822834645669291653 ) ) ;
#51873 = CARTESIAN_POINT ( 'NONE',  ( -0.9317585301837263412, 0.05413385826771666132, 0.4176697321401328100 ) ) ;
#51874 = CARTESIAN_POINT ( 'NONE',  ( 0.9514435695538062676, -0.3162353388693409650, -0.4822834645669289433 ) ) ;
#51875 = CARTESIAN_POINT ( 'NONE',  ( -1.476377952755905110, 0.07958543189024085140, 0.2665933059059887866 ) ) ;
#51876 = CARTESIAN_POINT ( 'NONE',  ( 1.057016155527769508, 1.247622337477865440, -0.3768861415345499677 ) ) ;
#51877 = CARTESIAN_POINT ( 'NONE',  ( 0.8989501312335963501, -0.6692913385826773087, -0.1292274648535924053 ) ) ;
#51878 = CARTESIAN_POINT ( 'NONE',  ( 0.1265901696524989462, 0.4724409448818897572, -2.432414698162729039 ) ) ;
#51879 = CIRCLE ( 'NONE', #53205, 0.3149606299212598381 ) ;
#51880 = CARTESIAN_POINT ( 'NONE',  ( -0.08907927694006900765, -1.283732188437465593E-15, -0.4281993546915538462 ) ) ;
#51881 = CARTESIAN_POINT ( 'NONE',  ( 1.548556430446194954, 0.2306618581243847221, -0.2411417322834647770 ) ) ;
#51882 = CARTESIAN_POINT ( 'NONE',  ( -0.9645669291338575535, -0.4536011799217367080, 0.2665933059059888421 ) ) ;
#51883 = CARTESIAN_POINT ( 'NONE',  ( 1.469816272965879911, -0.5023911411419708095, 0.1820866141732285504 ) ) ;
#51884 = CARTESIAN_POINT ( 'NONE',  ( -1.437007874015747477, 0.07958543189024071263, -0.2665933059059888421 ) ) ;
#51885 = CARTESIAN_POINT ( 'NONE',  ( -0.2624671916010490880, -0.5023911411419708095, 0.1820866141732285504 ) ) ;
#51886 = ADVANCED_FACE ( 'NONE', ( #78859 ), #71697, .F. ) ;
#51887 = CARTESIAN_POINT ( 'NONE',  ( 0.6299212598425341092, 1.724409448818898127, -3.937007874015759690 ) ) ;
#51888 = CARTESIAN_POINT ( 'NONE',  ( 1.030183727034121421, -0.2845877964562161244, -0.3641732283464567121 ) ) ;
#51889 = CARTESIAN_POINT ( 'NONE',  ( 0.6889763779527566800, -0.5400638737290844871, 0.3530559997133364547 ) ) ;
#51890 = CARTESIAN_POINT ( 'NONE',  ( 1.115485564304462551, 0.05413385826771666132, 0.4176697321401328100 ) ) ;
#51891 = CARTESIAN_POINT ( 'NONE',  ( 0.01968503937007957949, -0.5400638737290845981, -0.3530559997133363437 ) ) ;
#51892 = CARTESIAN_POINT ( 'NONE',  ( 0.5708661417322841158, -0.4536011799217368745, -0.2665933059059886201 ) ) ;
#51893 = CARTESIAN_POINT ( 'NONE',  ( -1.430446194225720724, 0.05413385826771626580, -0.4176697321401330321 ) ) ;
#51894 = CARTESIAN_POINT ( 'NONE',  ( -1.509186351706035767, -0.4281496062992124485, 0.4176697321401328655 ) ) ;
#51895 = CARTESIAN_POINT ( 'NONE',  ( -0.7217847769028863381, 0.05413385826771626580, -0.4176697321401330321 ) ) ;
#51896 = CARTESIAN_POINT ( 'NONE',  ( 0.3996062992125986035, -0.1070741851644053111, -0.2690288713910761187 ) ) ;
#51897 = CARTESIAN_POINT ( 'NONE',  ( -0.09842519685039295696, 0.1660481256975883668, -0.3530559997133364547 ) ) ;
#51898 = CARTESIAN_POINT ( 'NONE',  ( -0.4396325459317577122, -0.6692913385826773087, -0.1292274648535924053 ) ) ;
#51899 = CARTESIAN_POINT ( 'NONE',  ( 0.4330708661417329575, -0.6692913385826771977, 8.415575281601705876E-17 ) ) ;
#51900 = CARTESIAN_POINT ( 'NONE',  ( -0.3996062992125986035, -7.340648628747425578E-17, -2.716535433070865757 ) ) ;
#51901 = CARTESIAN_POINT ( 'NONE',  ( -0.3949938075777409408, -0.1058382717557502933, -2.093175853018372834 ) ) ;
#51902 = CARTESIAN_POINT ( 'NONE',  ( 0.1049643490035304938, -0.3917322834645669549, -0.3923884514435695414 ) ) ;
#51903 = CARTESIAN_POINT ( 'NONE',  ( 0.000000000000000000, 2.755905511811024056, 0.000000000000000000 ) ) ;
#51904 = CARTESIAN_POINT ( 'NONE',  ( 0.1958661417322834775, 0.3392501089628018884, -1.081364829396325389 ) ) ;
#51905 = CARTESIAN_POINT ( 'NONE',  ( -1.036745406824146176, -0.004921259842519870586, -0.3153832671262229437 ) ) ;
#51906 = CARTESIAN_POINT ( 'NONE',  ( -0.3917322834645671215, 0.1049643490035301469, -0.9698162729658791337 ) ) ;
#51907 = CARTESIAN_POINT ( 'NONE',  ( -1.069553805774277722, 0.2952755905511811885, 0.1292274648535926551 ) ) ;
#51908 = CARTESIAN_POINT ( 'NONE',  ( -0.1958661417322834497, -0.3392501089628018884, 0.1693106543645162554 ) ) ;
#51909 = CARTESIAN_POINT ( 'NONE',  ( 0.3937007874015754361, -0.1870078740157479769, 0.4822834645669291653 ) ) ;
#51910 = CARTESIAN_POINT ( 'NONE',  ( -0.01312335958005186876, -0.3690944881889763329, 0.3153832671262228327 ) ) ;
#51911 = CARTESIAN_POINT ( 'NONE',  ( 1.299212598425197429, 0.2952755905511811885, 0.000000000000000000 ) ) ;
#51912 = CARTESIAN_POINT ( 'NONE',  ( 0.2952755905511816326, -0.5400638737290844871, 0.3530559997133364547 ) ) ;
#51913 = DIRECTION ( 'NONE',  ( 0.8660254037844361541, 0.000000000000000000, 0.5000000000000043299 ) ) ;
#51914 = CARTESIAN_POINT ( 'NONE',  ( -0.3460692066303958092, -0.1998031496062994683, -2.414698162729658648 ) ) ;
#51915 = CARTESIAN_POINT ( 'NONE',  ( -0.3917322834645671770, 0.1049643490035302024, -1.289389394521996968 ) ) ;
#51916 = CARTESIAN_POINT ( 'NONE',  ( 1.456692913385827515, -0.6692913385826771977, 8.415575281601705876E-17 ) ) ;
#51917 = AXIS2_PLACEMENT_3D ( 'NONE', #68218, #23573, #28659 ) ;
#51918 = AXIS2_PLACEMENT_3D ( 'NONE', #80166, #41423, #21647 ) ;
#51919 = CARTESIAN_POINT ( 'NONE',  ( 0.5905511811023629321, -0.6692913385826771977, 8.415575281601705876E-17 ) ) ;
#51920 = CARTESIAN_POINT ( 'NONE',  ( 0.2559055118110243332, -0.5400638737290845981, -0.3530559997133363437 ) ) ;
#51921 = CARTESIAN_POINT ( 'NONE',  ( 0.8202099737532813073, 0.1771653543307087630, 0.09757992244046791164 ) ) ;
#51922 = CARTESIAN_POINT ( 'NONE',  ( 1.482939632545932307, -0.4281496062992124485, 0.4176697321401328655 ) ) ;
#51923 = CARTESIAN_POINT ( 'NONE',  ( -0.2867679344610365999, 0.2867679344610364889, -0.5767716535433071723 ) ) ;
#51924 = CARTESIAN_POINT ( 'NONE',  ( 0.1968503937007881344, 0.2952755905511811885, 0.000000000000000000 ) ) ;
#51925 = CARTESIAN_POINT ( 'NONE',  ( 0.8727034120734913358, -0.05778040916215522460, 0.4822834645669289988 ) ) ;
#51926 = CARTESIAN_POINT ( 'NONE',  ( 0.3477690288713918276, -0.6692913385826773087, -0.1292274648535924053 ) ) ;
#51927 = CARTESIAN_POINT ( 'NONE',  ( 1.253280839895013710, -0.08942795157528024563, -0.3641732283464568787 ) ) ;
#51928 = CARTESIAN_POINT ( 'NONE',  ( -0.7677165354330699465, 0.1660481256975885056, 0.3530559997133364547 ) ) ;
#51929 = CARTESIAN_POINT ( 'NONE',  ( -1.220472440944881054, 0.2952755905511811885, 0.000000000000000000 ) ) ;
#51930 = CARTESIAN_POINT ( 'NONE',  ( 1.056430446194226436, -0.6692913385826773087, -0.1292274648535924053 ) ) ;
#51931 = CARTESIAN_POINT ( 'NONE',  ( 0.1265901696524989184, 0.4724409448818898127, -0.5426509186351704539 ) ) ;
#51932 = CARTESIAN_POINT ( 'NONE',  ( 0.3917322834645669549, 0.1049643490035304660, -2.006561679790026531 ) ) ;
#51933 = CARTESIAN_POINT ( 'NONE',  ( 1.607611548556431069, -0.6692913385826773087, -0.1292274648535924053 ) ) ;
#51934 = EDGE_LOOP ( 'NONE', ( #9934, #80737, #16994, #32370 ) ) ;
#51935 = CARTESIAN_POINT ( 'NONE',  ( 0.1998031496062992740, 0.3460692066303959757, -0.1443569553805774397 ) ) ;
#51936 = ORIENTED_EDGE ( 'NONE', *, *, #35126, .F. ) ;
#51937 = CARTESIAN_POINT ( 'NONE',  ( 1.561679790026247350, 0.05413385826771626580, -0.4176697321401330321 ) ) ;
#51938 = AXIS2_PLACEMENT_3D ( 'NONE', #69780, #25144, #23502 ) ;
#51939 = CARTESIAN_POINT ( 'NONE',  ( 0.7611548556430451917, -0.5023911411419708095, 0.1820866141732285504 ) ) ;
#51940 = CARTESIAN_POINT ( 'NONE',  ( -0.08520949344212035148, 1.070405622666591228, 2.867149795802078849 ) ) ;
#51941 = DIRECTION ( 'NONE',  ( -0.000000000000000000, 1.000000000000000000, 0.000000000000000000 ) ) ;
#51942 = CARTESIAN_POINT ( 'NONE',  ( 0.3392501089628018329, 0.1958661417322835607, -0.6883202099737534274 ) ) ;
#51943 = CARTESIAN_POINT ( 'NONE',  ( -0.9842519685039360366, 0.1771653543307087630, 0.000000000000000000 ) ) ;
#51944 = CARTESIAN_POINT ( 'NONE',  ( -1.574803149606298636, -0.1870078740157479769, 0.3641732283464567677 ) ) ;
#51945 = CARTESIAN_POINT ( 'NONE',  ( -0.3941128856533543945, -0.02500110684012597437, -1.929133858266767865 ) ) ;
#51946 = CARTESIAN_POINT ( 'NONE',  ( -0.1902887139107604098, -0.6692913385826771977, 0.1292274648535927661 ) ) ;
#51947 = CARTESIAN_POINT ( 'NONE',  ( 1.482939632545932307, 0.05413385826771626580, -0.4176697321401330321 ) ) ;
#51948 = ORIENTED_EDGE ( 'NONE', *, *, #14046, .F. ) ;
#51949 = DIRECTION ( 'NONE',  ( 0.000000000000000000, 0.000000000000000000, -1.000000000000000000 ) ) ;
#51950 = CARTESIAN_POINT ( 'NONE',  ( 3.523619145740947811, 3.916330350904249524, 3.611108355172080397 ) ) ;
#51951 = LINE ( 'NONE', #635, #37112 ) ;
#51952 = CARTESIAN_POINT ( 'NONE',  ( -0.03443470937339728616, 0.2755905511811023723, -1.656110380428732265 ) ) ;
#51953 = CARTESIAN_POINT ( 'NONE',  ( -1.108923884514435132, -0.08942795157528024563, -0.3641732283464568787 ) ) ;
#51954 = CARTESIAN_POINT ( 'NONE',  ( -1.437007874015747477, 0.1660481256975883668, -0.3530559997133364547 ) ) ;
#51955 = CARTESIAN_POINT ( 'NONE',  ( 0.6496062992125991586, -0.5400638737290845981, -0.3530559997133363437 ) ) ;
#51956 = ORIENTED_EDGE ( 'NONE', *, *, #31518, .T. ) ;
#51957 = CARTESIAN_POINT ( 'NONE',  ( -0.2362204724409447953, -0.4091458600556404646, -2.504593175853018661 ) ) ;
#51958 =( BOUNDED_SURFACE ( )  B_SPLINE_SURFACE ( 1, 2, ( 
 ( #69257, #16270, #23388, #48644, #74338, #16685, #42324, #41915, #67609, #4039, #30533, #56197, #11604, #60861, #17512, #29704, #81072, #74755, #68434, #3215, #10774, #4450, #30115, #81485, #23801, #49474, #5272, #30936, #18329, #45207, #25438, #13258, #56603, #24622, #43969, #82303, #50289, #75987, #83120, #44781, #57835, #69666, #50699, #51104, #12417, #37263, #12009, #37663, #63341, #62939, #70478, #5676, #31344, #70063, #57010, #76801, #82706, #25026, #31765, #64587, #57426, #76397, #19132, #18729, #12835, #38493, #44371, #38075, #64176, #6510, #32180, #63751, #6090, #203, #25855, #51515, #77219, #19548, #70907, #38907, #4296, #23647, #42993, #49728, #37515, #69099, #82155, #68688, #80514, #11030, #42592, #75426, #3892, #29959, #18176, #10212, #29552, #55215, #80922, #61549, #35880, #23237, #43400, #36687, #17768, #17365, #22829, #75019, #11447, #62362, #37103, #56040, #48906, #4700, #62788, #5122, #30373, #81748, #74607, #30789, #10628, #81333, #55624, #24059, #36284, #56453, #67874, #16950, #11862, #54810, #24470, #49318, #61957, #50137, #75835, #43809, #68292, #69513, #63190, #29144, #48488, #74189, #16535, #42180, #56735, #12141, #69795, #37798, #63067, #36977, #12550, #18858, #55909, #38208, #31066, #76118, #82432, #69386, #44506, #23934, #81621, #5810, #24750, #18050, #19264, #49602, #75296, #17640, #18459, #56329, #63883, #44102, #50418, #11740, #43272, #5404, #31480, #76936, #51237, #44917, #75709, #70614, #68969, #63475, #11318, #57141, #6221, #31897, #25160, #82838, #50828, #62657, #76530, #57558, #38626, #4998, #30666, #82028, #24342, #50011, #83249, #70195, #25572, #12969, #43683, #37395, #4575, #30246, #58826, #65982, #27666, #71041, #39889, #13386, #65576, #64723, #20946, #7062, #39038, #33571, #15054, #58398, #32731, #758, #33986, #53332, #59233, #14229, #79041, #7910, #21360, #72707, #71459, #39465, #1183, #78201, #1594, #64304, #46603, #59648, #20531, #32310, #46183, #77779, #27249, #26419, #65151, #47013, #45345, #52072, #20113, #45760, #13806, #7488, #33157, #78622, #71880, #52908, #52492, #57973, #26834, #72299, #14645, #40302, #8320, #2004, #6638, #338, #25994, #51651, #77356, #19687, #16716, #22188, #9562, #41543, #67643, #47845, #35646, #79448, #66821, #23420, #66395, #23009, #60896, #73551, #15895, #42356, #61730, #73123, #41130, #48677, #67232, #22602, #61307, #68054, #4067, #80288, #49086, #3248, #35233, #28911, #74786, #54575, #48262, #10401, #36058, #21768, #73959, #16305, #60071, #2426, #41948, #81103, #40710, #9977, #3664, #29327, #54988, #80696, #8733, #74372, #29734, #55397, #34403, #28082, #54156, #53740, #15473, #47430, #9154, #34827, #60485, #2835, #28498, #79871, #23836, #75197, #31377, #82334, #37696, #5307, #10803, #62969, #82736, #30966, #63371, #44003, #68870, #76017, #5706, #50730, #56633, #24652, #43173, #76429, #81929, #69287, #17949, #69696, #24240, #12040, #55808, #11218, #83149, #42769, #25055, #37294, #49913, #75611, #18757, #38106, #49504, #17541, #44401, #43586, #50320, #57042, #70093, #63782, #18359, #25469, #12447, #11634, #6121, #51135, #31793, #57456, #17137, #68465, #81515, #36463, #62138, #4477, #30147, #36878, #62556, #4891, #30566, #56231, #51968, #13699, #57869, #33044, #27143, #27563, #38523, #12866, #6540, #13285, #19580, #20841, #59132, #77676, #59547, #77251, #64618, #71353, #38937, #39355, #78517, #40198, #235, #52385, #25887, #78094, #45240, #33470, #70940, #51547, #46078, #76830, #6955, #32625, #58288, #46493, #65881, #71771, #26731, #8217, #653, #72189, #1490, #20006, #1902, #26310, #45657, #65039, #7376, #58713, #14546, #33881, #1078, #20425, #14124, #39777, #65471, #52807, #7805, #19162, #44812, #70508, #64206, #32210, #53638, #22905, #42256, #48163, #3145, #16614, #28808, #10294, #61630, #60382, #28392, #47741, #67125, #73858, #3972, #9873, #48573, #9455, #21255, #35128, #66714, #16199, #27979, #54051, #67951, #34302, #79345, #21666, #47325, #2319, #59963, #73016, #67536, #60792, #41846, #41441, #46909, #15789, #35542, #54472, #61203, #80185, #15367, #22500, #3560, #29225, #54892 ),
 ( #73439, #2731, #79765, #80597, #74270, #41028, #9047, #35961, #22082, #53222, #78932, #72604, #14951, #40609, #66292, #8631, #34722, #75512, #38008, #43485, #69181, #31279, #82641, #10709, #24141, #11532, #48989, #74687, #17033, #56125, #5611, #37597, #50222, #4785, #49812, #36366, #37189, #63271, #63686, #42672, #68371, #62040, #49403, #17851, #81831, #11116, #69596, #4377, #81005, #30869, #62869, #43075, #44307, #23319, #30045, #55707, #5205, #81416, #56944, #56535, #82237, #36773, #23732, #30462, #24556, #18662, #76332, #69997, #17445, #12352, #75097, #75918, #68772, #62449, #18257, #43899, #11943, #24954, #50627, #29636, #55296, #39683, #78421, #20327, #25790, #19486, #51451, #6858, #59041, #33377, #7280, #26212, #6024, #32950, #45562, #83050, #57354, #12768, #20749, #64940, #72092, #25373, #19067, #64107, #51036, #76737, #38425, #39258, #26639, #65375, #70412, #38841, #58616, #51874, #31695, #6442, #44715, #32114, #40102, #64520, #57772, #7710, #135, #71675, #77154, #45139, #983, #46399, #70843, #1395, #13604, #14451, #77998, #77580, #27050, #52709, #14026, #13192, #32527, #52293, #71258, #45979, #58191, #559, #19912, #33789, #79254, #16519, #16100, #79669, #72920, #2220, #61110, #41349, #15272, #34624, #15691, #60288, #54795, #65790, #2638, #73343, #47648, #67030, #40932, #14858, #73765, #80086, #59452, #41745, #8948, #67440, #21987, #28295, #47231, #21162, #66612, #9362, #80498, #29127, #22814, #53546, #48471, #46818, #53957, #27886, #8537, #66199, #21569, #1805, #72509, #27467, #9773, #35445, #3462, #74173, #22406, #35033, #60698, #3047, #28713, #8123, #53125, #54376, #48063, #78836, #40520, #34204, #59867, #10196, #48889, #57984, #17752, #26006, #35865, #55198, #16934, #61530, #3876, #74590, #75406, #63894, #19276, #23219, #75002, #43381, #62346, #42164, #42574, #80906, #29535, #77367, #17349, #67858, #44928, #68276, #25583, #61937, #10611, #38219, #349, #36268, #38637, #49712, #32322, #31908, #4684, #12981, #70625, #51247, #4280, #76949, #69082, #81732, #24041, #29941, #68672, #30355, #55606, #81317, #23630, #64315, #56024, #49301, #42976, #6649, #12561, #11011, #36670, #6232, #57569, #51663, #83261, #71891, #27260, #1604, #52920, #78212, #52082, #27680, #33998, #71053, #53345, #46196, #7921, #14242, #1195, #59660, #39050, #13397, #20958, #39900, #33169, #34416, #64735, #7073, #32743, #33582, #71470, #13818, #20124, #45771, #72719, #8745, #14658, #78634, #66408, #46616, #60084, #28096, #26844, #20544, #65588, #59245, #40315, #53752, #2016, #15066, #72311, #58410, #65994, #58837, #8332, #77791, #79055, #2438, #769, #39477, #65164, #7500, #52503, #26431, #21372, #47027, #40722, #19699, #45356, #73135, #41960, #61740, #67653, #42368, #23020, #47856, #54998, #68067, #29744, #35656, #9990, #22200, #55408, #60907, #48272, #80298, #48687, #3259, #74384, #34837, #73561, #62148, #21779, #4077, #16315, #28920, #54588, #81114, #17147, #28510, #79882, #23432, #22612, #61319, #16727, #49096, #42779, #3674, #4489, #29337, #73970, #80706, #30157, #10411, #36068, #74800, #68475, #60497, #10813, #36473, #15485, #41142, #66832, #79462, #47441, #9165, #2846, #54167, #15905, #41554, #67242, #9573, #35243, #17551, #75207, #68880, #75621, #81939, #83160, #38118, #56643, #38535, #56242, #43596, #50331, #17959, #76028, #57466, #19174, #62566, #31387, #4905, #57053, #24250, #12457, #49923, #30576, #25067, #6550, #82344, #18373, #23847, #69298, #55819, #6131, #69707, #62979, #11647, #51146, #82746, #5318, #24662, #5717, #44013, #44822, #81527, #12051, #63381, #37708, #50741, #30976, #37305, #63793, #70105, #49514, #31806, #76439, #18768, #44411, #25479, #76840, #43183, #11229, #70520, #12876, #64216, #36890, #25898, #246, #51558, #20437, #666, #40211, #46091, #78106, #13713, #70950, #7390, #59146, #21268, #78950, #72616, #20017, #46923, #13295, #71783, #77687, #58300, #32637, #71364, #77262, #38947, #19591, #65894, #8229, #33893, #14964, #46506, #51982, #45668, #39367, #33058, #1914, #59559, #33483, #52397, #32221, #1503, #14138, #45253, #64630, #6966, #40621 ) ),
 .UNSPECIFIED., .F., .F., .F. ) 
 B_SPLINE_SURFACE_WITH_KNOTS ( ( 2, 2 ),
 ( 3, 2, 2, 2, 2, 2, 2, 2, 2, 2, 2, 2, 2, 2, 2, 2, 2, 2, 2, 2, 2, 2, 2, 2, 2, 2, 2, 2, 2, 2, 2, 2, 2, 2, 2, 2, 2, 2, 2, 2, 2, 2, 2, 2, 2, 2, 2, 2, 2, 2, 2, 2, 2, 2, 2, 2, 2, 2, 2, 2, 2, 2, 2, 2, 2, 2, 2, 2, 2, 2, 2, 2, 2, 2, 2, 2, 2, 2, 2, 2, 2, 2, 2, 2, 2, 2, 2, 2, 2, 2, 2, 2, 2, 2, 2, 2, 2, 2, 2, 2, 2, 2, 2, 2, 2, 2, 2, 2, 2, 2, 2, 2, 2, 2, 2, 2, 2, 2, 2, 2, 2, 2, 2, 2, 2, 2, 2, 2, 2, 2, 2, 2, 2, 2, 2, 2, 2, 2, 2, 2, 2, 2, 2, 2, 2, 2, 2, 2, 2, 2, 2, 2, 2, 2, 2, 2, 2, 2, 2, 2, 2, 2, 2, 2, 2, 2, 2, 2, 2, 2, 2, 2, 2, 2, 2, 2, 2, 2, 2, 2, 2, 2, 2, 2, 2, 2, 2, 2, 2, 2, 2, 2, 2, 2, 2, 2, 2, 2, 2, 2, 2, 2, 2, 2, 2, 2, 2, 2, 2, 2, 2, 2, 2, 2, 2, 2, 2, 2, 2, 2, 2, 2, 2, 2, 2, 2, 2, 2, 2, 2, 2, 2, 2, 2, 2, 2, 2, 2, 2, 2, 2, 2, 2, 2, 2, 2, 2, 2, 2, 2, 2, 2, 2, 2, 2, 3 ),
 ( 0.000000000000000000, 1.000000000000000000 ),
 ( 0.000000000000000000, 0.003787878787878787984, 0.007575757575757575968, 0.01136363636363636395, 0.01515151515151515194, 0.01893939393939393992, 0.02272727272727272790, 0.02651515151515151589, 0.03030303030303030387, 0.03409090909090908839, 0.03787878787878787984, 0.04166666666666666435, 0.04545454545454545581, 0.04924242424242424032, 0.05303030303030303177, 0.05681818181818181629, 0.06060606060606060774, 0.06439393939393939226, 0.06818181818181817677, 0.07196969696969697516, 0.07575757575757575968, 0.07954545454545454419, 0.08333333333333332871, 0.08712121212121212710, 0.09090909090909091161, 0.09469696969696969613, 0.09848484848484848064, 0.1022727272727272790, 0.1060606060606060635, 0.1098484848484848481, 0.1136363636363636326, 0.1174242424242424310, 0.1212121212121212155, 0.1250000000000000000, 0.1287878787878787845, 0.1325757575757575690, 0.1363636363636363535, 0.1401515151515151381, 0.1439393939393939503, 0.1477272727272727348, 0.1515151515151515194, 0.1553030303030303039, 0.1590909090909090884, 0.1628787878787878729, 0.1666666666666666574, 0.1704545454545454419, 0.1742424242424242542, 0.1780303030303030387, 0.1818181818181818232, 0.1856060606060606077, 0.1893939393939393923, 0.1931818181818181768, 0.1969696969696969613, 0.2007575757575757458, 0.2045454545454545581, 0.2083333333333333426, 0.2121212121212121271, 0.2159090909090909116, 0.2196969696969696961, 0.2234848484848484806, 0.2272727272727272652, 0.2310606060606060497, 0.2348484848484848619, 0.2386363636363636465, 0.2424242424242424310, 0.2462121212121212155, 0.2500000000000000000, 0.2537878787878787845, 0.2575757575757575690, 0.2613636363636363535, 0.2651515151515151381, 0.2689393939393939226, 0.2727272727272727071, 0.2765151515151514916, 0.2803030303030302761, 0.2840909090909091161, 0.2878787878787879007, 0.2916666666666666852, 0.2954545454545454697, 0.2992424242424242542, 0.3030303030303030387, 0.3068181818181818232, 0.3106060606060606077, 0.3143939393939393923, 0.3181818181818181768, 0.3219696969696969613, 0.3257575757575757458, 0.3295454545454545303, 0.3333333333333333148, 0.3371212121212120993, 0.3409090909090908839, 0.3446969696969697239, 0.3484848484848485084, 0.3522727272727272929, 0.3560606060606060774, 0.3598484848484848619, 0.3636363636363636465, 0.3674242424242424310, 0.3712121212121212155, 0.3750000000000000000, 0.3787878787878787845, 0.3825757575757575690, 0.3863636363636363535, 0.3901515151515151381, 0.3939393939393939226, 0.3977272727272727071, 0.4015151515151514916, 0.4053030303030302761, 0.4090909090909091161, 0.4128787878787879007, 0.4166666666666666852, 0.4204545454545454697, 0.4242424242424242542, 0.4280303030303030387, 0.4318181818181818232, 0.4356060606060606077, 0.4393939393939393923, 0.4431818181818181768, 0.4469696969696969613, 0.4507575757575757458, 0.4545454545454545303, 0.4583333333333333148, 0.4621212121212120993, 0.4659090909090908839, 0.4696969696969697239, 0.4734848484848485084, 0.4772727272727272929, 0.4810606060606060774, 0.4848484848484848619, 0.4886363636363636465, 0.4924242424242424310, 0.4962121212121212155, 0.5000000000000000000, 0.5037878787878787845, 0.5075757575757575690, 0.5113636363636363535, 0.5151515151515151381, 0.5189393939393939226, 0.5227272727272727071, 0.5265151515151514916, 0.5303030303030302761, 0.5340909090909090606, 0.5378787878787878451, 0.5416666666666666297, 0.5454545454545454142, 0.5492424242424241987, 0.5530303030303029832, 0.5568181818181817677, 0.5606060606060605522, 0.5643939393939394478, 0.5681818181818182323, 0.5719696969696970168, 0.5757575757575758013, 0.5795454545454545858, 0.5833333333333333703, 0.5871212121212121549, 0.5909090909090909394, 0.5946969696969697239, 0.5984848484848485084, 0.6022727272727272929, 0.6060606060606060774, 0.6098484848484848619, 0.6136363636363636465, 0.6174242424242424310, 0.6212121212121212155, 0.6250000000000000000, 0.6287878787878787845, 0.6325757575757575690, 0.6363636363636363535, 0.6401515151515151381, 0.6439393939393939226, 0.6477272727272727071, 0.6515151515151514916, 0.6553030303030302761, 0.6590909090909090606, 0.6628787878787878451, 0.6666666666666666297, 0.6704545454545454142, 0.6742424242424241987, 0.6780303030303029832, 0.6818181818181817677, 0.6856060606060605522, 0.6893939393939394478, 0.6931818181818182323, 0.6969696969696970168, 0.7007575757575758013, 0.7045454545454545858, 0.7083333333333333703, 0.7121212121212121549, 0.7159090909090909394, 0.7196969696969697239, 0.7234848484848485084, 0.7272727272727272929, 0.7310606060606060774, 0.7348484848484848619, 0.7386363636363636465, 0.7424242424242424310, 0.7462121212121212155, 0.7500000000000000000, 0.7537878787878787845, 0.7575757575757575690, 0.7613636363636363535, 0.7651515151515151381, 0.7689393939393939226, 0.7727272727272727071, 0.7765151515151514916, 0.7803030303030302761, 0.7840909090909090606, 0.7878787878787878451, 0.7916666666666666297, 0.7954545454545454142, 0.7992424242424241987, 0.8030303030303029832, 0.8068181818181817677, 0.8106060606060605522, 0.8143939393939394478, 0.8181818181818182323, 0.8219696969696970168, 0.8257575757575758013, 0.8295454545454545858, 0.8333333333333333703, 0.8371212121212121549, 0.8409090909090909394, 0.8446969696969697239, 0.8484848484848485084, 0.8522727272727272929, 0.8560606060606060774, 0.8598484848484848619, 0.8636363636363636465, 0.8674242424242424310, 0.8712121212121212155, 0.8750000000000000000, 0.8787878787878787845, 0.8825757575757575690, 0.8863636363636363535, 0.8901515151515151381, 0.8939393939393939226, 0.8977272727272727071, 0.9015151515151514916, 0.9053030303030302761, 0.9090909090909090606, 0.9128787878787878451, 0.9166666666666666297, 0.9204545454545454142, 0.9242424242424241987, 0.9280303030303029832, 0.9318181818181817677, 0.9356060606060605522, 0.9393939393939394478, 0.9431818181818182323, 0.9469696969696970168, 0.9507575757575758013, 0.9545454545454545858, 0.9583333333333333703, 0.9621212121212121549, 0.9659090909090909394 ),
 .UNSPECIFIED. ) 
 GEOMETRIC_REPRESENTATION_ITEM ( )  RATIONAL_B_SPLINE_SURFACE ( (
 ( 1.000000000000000000, 0.9659258262890683122, 1.000000000000000000, 0.9659258262890683122, 1.000000000000000000, 0.9659258262890683122, 1.000000000000000000, 0.9659258262890683122, 1.000000000000000000, 0.9659258262890683122, 1.000000000000000000, 0.9659258262890683122, 1.000000000000000000, 0.9659258262890683122, 1.000000000000000000, 0.9659258262890683122, 1.000000000000000000, 0.9659258262890683122, 1.000000000000000000, 0.9659258262890683122, 1.000000000000000000, 0.9659258262890683122, 1.000000000000000000, 0.9659258262890683122, 1.000000000000000000, 0.9659258262890683122, 1.000000000000000000, 0.9659258262890683122, 1.000000000000000000, 0.9659258262890683122, 1.000000000000000000, 0.9659258262890683122, 1.000000000000000000, 0.9659258262890683122, 1.000000000000000000, 0.9659258262890683122, 1.000000000000000000, 0.9659258262890683122, 1.000000000000000000, 0.9659258262890683122, 1.000000000000000000, 0.9659258262890683122, 1.000000000000000000, 0.9659258262890683122, 1.000000000000000000, 0.9659258262890683122, 1.000000000000000000, 0.9659258262890683122, 1.000000000000000000, 0.9659258262890683122, 1.000000000000000000, 0.9659258262890683122, 1.000000000000000000, 0.9659258262890683122, 1.000000000000000000, 0.9659258262890683122, 1.000000000000000000, 0.9659258262890683122, 1.000000000000000000, 0.9659258262890683122, 1.000000000000000000, 0.9659258262890683122, 1.000000000000000000, 0.9659258262890683122, 1.000000000000000000, 0.9659258262890683122, 1.000000000000000000, 0.9659258262890683122, 1.000000000000000000, 0.9659258262890683122, 1.000000000000000000, 0.9659258262890683122, 1.000000000000000000, 0.9659258262890683122, 1.000000000000000000, 0.9659258262890683122, 1.000000000000000000, 0.9659258262890683122, 1.000000000000000000, 0.9659258262890683122, 1.000000000000000000, 0.9659258262890683122, 1.000000000000000000, 0.9659258262890683122, 1.000000000000000000, 0.9659258262890683122, 1.000000000000000000, 0.9659258262890683122, 1.000000000000000000, 0.9659258262890683122, 1.000000000000000000, 0.9659258262890683122, 1.000000000000000000, 0.9659258262890683122, 1.000000000000000000, 0.9659258262890683122, 1.000000000000000000, 0.9659258262890683122, 1.000000000000000000, 0.9659258262890683122, 1.000000000000000000, 0.9659258262890683122, 1.000000000000000000, 0.9659258262890683122, 1.000000000000000000, 0.9659258262890683122, 1.000000000000000000, 0.9659258262890683122, 1.000000000000000000, 0.9659258262890683122, 1.000000000000000000, 0.9659258262890683122, 1.000000000000000000, 0.9659258262890683122, 1.000000000000000000, 0.9659258262890683122, 1.000000000000000000, 0.9659258262890683122, 1.000000000000000000, 0.9659258262890683122, 1.000000000000000000, 0.9659258262890683122, 1.000000000000000000, 0.9659258262890683122, 1.000000000000000000, 0.9659258262890683122, 1.000000000000000000, 0.9659258262890683122, 1.000000000000000000, 0.9659258262890683122, 1.000000000000000000, 0.9659258262890683122, 1.000000000000000000, 0.9659258262890683122, 1.000000000000000000, 0.9659258262890683122, 1.000000000000000000, 0.9659258262890683122, 1.000000000000000000, 0.9659258262890683122, 1.000000000000000000, 0.9659258262890683122, 1.000000000000000000, 0.9659258262890683122, 1.000000000000000000, 0.9659258262890683122, 1.000000000000000000, 0.9659258262890683122, 1.000000000000000000, 0.9659258262890683122, 1.000000000000000000, 0.9659258262890683122, 1.000000000000000000, 0.9659258262890683122, 1.000000000000000000, 0.9659258262890683122, 1.000000000000000000, 0.9659258262890683122, 1.000000000000000000, 0.9659258262890683122, 1.000000000000000000, 0.9659258262890683122, 1.000000000000000000, 0.9659258262890683122, 1.000000000000000000, 0.9659258262890683122, 1.000000000000000000, 0.9659258262890683122, 1.000000000000000000, 0.9659258262890683122, 1.000000000000000000, 0.9659258262890683122, 1.000000000000000000, 0.9659258262890683122, 1.000000000000000000, 0.9659258262890683122, 1.000000000000000000, 0.9659258262890683122, 1.000000000000000000, 0.9659258262890683122, 1.000000000000000000, 0.9659258262890683122, 1.000000000000000000, 0.9659258262890683122, 1.000000000000000000, 0.9659258262890683122, 1.000000000000000000, 0.9659258262890683122, 1.000000000000000000, 0.9659258262890683122, 1.000000000000000000, 0.9659258262890683122, 1.000000000000000000, 0.9659258262890683122, 1.000000000000000000, 0.9659258262890683122, 1.000000000000000000, 0.9659258262890683122, 1.000000000000000000, 0.9659258262890683122, 1.000000000000000000, 0.9659258262890683122, 1.000000000000000000, 0.9659258262890683122, 1.000000000000000000, 0.9659258262890683122, 1.000000000000000000, 0.9659258262890683122, 1.000000000000000000, 0.9659258262890683122, 1.000000000000000000, 0.9659258262890683122, 1.000000000000000000, 0.9659258262890683122, 1.000000000000000000, 0.9659258262890683122, 1.000000000000000000, 0.9659258262890683122, 1.000000000000000000, 0.9659258262890683122, 1.000000000000000000, 0.9659258262890683122, 1.000000000000000000, 0.9659258262890683122, 1.000000000000000000, 0.9659258262890683122, 1.000000000000000000, 0.9659258262890683122, 1.000000000000000000, 0.9659258262890683122, 1.000000000000000000, 0.9659258262890683122, 1.000000000000000000, 0.9659258262890683122, 1.000000000000000000, 0.9659258262890683122, 1.000000000000000000, 0.9659258262890683122, 1.000000000000000000, 0.9659258262890683122, 1.000000000000000000, 0.9659258262890683122, 1.000000000000000000, 0.9659258262890683122, 1.000000000000000000, 0.9659258262890683122, 1.000000000000000000, 0.9659258262890683122, 1.000000000000000000, 0.9659258262890683122, 1.000000000000000000, 0.9659258262890683122, 1.000000000000000000, 0.9659258262890683122, 1.000000000000000000, 0.9659258262890683122, 1.000000000000000000, 0.9659258262890683122, 1.000000000000000000, 0.9659258262890683122, 1.000000000000000000, 0.9659258262890683122, 1.000000000000000000, 0.9659258262890683122, 1.000000000000000000, 0.9659258262890683122, 1.000000000000000000, 0.9659258262890683122, 1.000000000000000000, 0.9659258262890683122, 1.000000000000000000, 0.9659258262890683122, 1.000000000000000000, 0.9659258262890683122, 1.000000000000000000, 0.9659258262890683122, 1.000000000000000000, 0.9659258262890683122, 1.000000000000000000, 0.9659258262890683122, 1.000000000000000000, 0.9659258262890683122, 1.000000000000000000, 0.9659258262890683122, 1.000000000000000000, 0.9659258262890683122, 1.000000000000000000, 0.9659258262890683122, 1.000000000000000000, 0.9659258262890683122, 1.000000000000000000, 0.9659258262890683122, 1.000000000000000000, 0.9659258262890683122, 1.000000000000000000, 0.9659258262890683122, 1.000000000000000000, 0.9659258262890683122, 1.000000000000000000, 0.9659258262890683122, 1.000000000000000000, 0.9659258262890683122, 1.000000000000000000, 0.9659258262890683122, 1.000000000000000000, 0.9659258262890683122, 1.000000000000000000, 0.9659258262890683122, 1.000000000000000000, 0.9659258262890683122, 1.000000000000000000, 0.9659258262890683122, 1.000000000000000000, 0.9659258262890683122, 1.000000000000000000, 0.9659258262890683122, 1.000000000000000000, 0.9659258262890683122, 1.000000000000000000, 0.9659258262890683122, 1.000000000000000000, 0.9659258262890683122, 1.000000000000000000, 0.9659258262890683122, 1.000000000000000000, 0.9659258262890683122, 1.000000000000000000, 0.9659258262890683122, 1.000000000000000000, 0.9659258262890683122, 1.000000000000000000, 0.9659258262890683122, 1.000000000000000000, 0.9659258262890683122, 1.000000000000000000, 0.9659258262890683122, 1.000000000000000000, 0.9659258262890683122, 1.000000000000000000, 0.9659258262890683122, 1.000000000000000000, 0.9659258262890683122, 1.000000000000000000, 0.9659258262890683122, 1.000000000000000000, 0.9659258262890683122, 1.000000000000000000, 0.9659258262890683122, 1.000000000000000000, 0.9659258262890683122, 1.000000000000000000, 0.9659258262890683122, 1.000000000000000000, 0.9659258262890683122, 1.000000000000000000, 0.9659258262890683122, 1.000000000000000000, 0.9659258262890683122, 1.000000000000000000, 0.9659258262890683122, 1.000000000000000000, 0.9659258262890683122, 1.000000000000000000, 0.9659258262890683122, 1.000000000000000000, 0.9659258262890683122, 1.000000000000000000, 0.9659258262890683122, 1.000000000000000000, 0.9659258262890683122, 1.000000000000000000, 0.9659258262890683122, 1.000000000000000000, 0.9659258262890683122, 1.000000000000000000, 0.9659258262890683122, 1.000000000000000000, 0.9659258262890683122, 1.000000000000000000, 0.9659258262890683122, 1.000000000000000000, 0.9659258262890683122, 1.000000000000000000, 0.9659258262890683122, 1.000000000000000000, 0.9659258262890683122, 1.000000000000000000, 0.9659258262890683122, 1.000000000000000000, 0.9659258262890683122, 1.000000000000000000, 0.9659258262890683122, 1.000000000000000000, 0.9659258262890683122, 1.000000000000000000, 0.9659258262890683122, 1.000000000000000000, 0.9659258262890683122, 1.000000000000000000, 0.9659258262890683122, 1.000000000000000000, 0.9659258262890683122, 1.000000000000000000, 0.9659258262890683122, 1.000000000000000000, 0.9659258262890683122, 1.000000000000000000, 0.9659258262890683122, 1.000000000000000000, 0.9659258262890683122, 1.000000000000000000, 0.9659258262890683122, 1.000000000000000000, 0.9659258262890683122, 1.000000000000000000, 0.9659258262890683122, 1.000000000000000000, 0.9659258262890683122, 1.000000000000000000, 0.9659258262890683122, 1.000000000000000000, 0.9659258262890683122, 1.000000000000000000, 0.9659258262890683122, 1.000000000000000000, 0.9659258262890683122, 1.000000000000000000, 0.9659258262890683122, 1.000000000000000000, 0.9659258262890683122, 1.000000000000000000, 0.9659258262890683122, 1.000000000000000000, 0.9659258262890683122, 1.000000000000000000, 0.9659258262890683122, 1.000000000000000000, 0.9659258262890683122, 1.000000000000000000, 0.9659258262890683122, 1.000000000000000000, 0.9659258262890683122, 1.000000000000000000, 0.9659258262890683122, 1.000000000000000000, 0.9659258262890683122, 1.000000000000000000, 0.9659258262890683122, 1.000000000000000000, 0.9659258262890683122, 1.000000000000000000, 0.9659258262890683122, 1.000000000000000000, 0.9659258262890683122, 1.000000000000000000, 0.9659258262890683122, 1.000000000000000000, 0.9659258262890683122, 1.000000000000000000, 0.9659258262890683122, 1.000000000000000000, 0.9659258262890683122, 1.000000000000000000, 0.9659258262890683122, 1.000000000000000000, 0.9659258262890683122, 1.000000000000000000, 0.9659258262890683122, 1.000000000000000000, 0.9659258262890683122, 1.000000000000000000, 0.9659258262890683122, 1.000000000000000000, 0.9659258262890683122, 1.000000000000000000, 0.9659258262890683122, 1.000000000000000000, 0.9659258262890683122, 1.000000000000000000, 0.9659258262890683122, 1.000000000000000000, 0.9659258262890683122, 1.000000000000000000, 0.9659258262890683122, 1.000000000000000000, 0.9659258262890683122, 1.000000000000000000, 0.9659258262890683122, 1.000000000000000000, 0.9659258262890683122, 1.000000000000000000, 0.9659258262890683122, 1.000000000000000000, 0.9659258262890683122, 1.000000000000000000, 0.9659258262890683122, 1.000000000000000000, 0.9659258262890683122, 1.000000000000000000, 0.9659258262890683122, 1.000000000000000000, 0.9659258262890683122, 1.000000000000000000, 0.9659258262890683122, 1.000000000000000000, 0.9659258262890683122, 1.000000000000000000, 0.9659258262890683122, 1.000000000000000000, 0.9659258262890683122, 1.000000000000000000),
 ( 1.000000000000000000, 0.9659258262890683122, 1.000000000000000000, 0.9659258262890683122, 1.000000000000000000, 0.9659258262890683122, 1.000000000000000000, 0.9659258262890683122, 1.000000000000000000, 0.9659258262890683122, 1.000000000000000000, 0.9659258262890683122, 1.000000000000000000, 0.9659258262890683122, 1.000000000000000000, 0.9659258262890683122, 1.000000000000000000, 0.9659258262890683122, 1.000000000000000000, 0.9659258262890683122, 1.000000000000000000, 0.9659258262890683122, 1.000000000000000000, 0.9659258262890683122, 1.000000000000000000, 0.9659258262890683122, 1.000000000000000000, 0.9659258262890683122, 1.000000000000000000, 0.9659258262890683122, 1.000000000000000000, 0.9659258262890683122, 1.000000000000000000, 0.9659258262890683122, 1.000000000000000000, 0.9659258262890683122, 1.000000000000000000, 0.9659258262890683122, 1.000000000000000000, 0.9659258262890683122, 1.000000000000000000, 0.9659258262890683122, 1.000000000000000000, 0.9659258262890683122, 1.000000000000000000, 0.9659258262890683122, 1.000000000000000000, 0.9659258262890683122, 1.000000000000000000, 0.9659258262890683122, 1.000000000000000000, 0.9659258262890683122, 1.000000000000000000, 0.9659258262890683122, 1.000000000000000000, 0.9659258262890683122, 1.000000000000000000, 0.9659258262890683122, 1.000000000000000000, 0.9659258262890683122, 1.000000000000000000, 0.9659258262890683122, 1.000000000000000000, 0.9659258262890683122, 1.000000000000000000, 0.9659258262890683122, 1.000000000000000000, 0.9659258262890683122, 1.000000000000000000, 0.9659258262890683122, 1.000000000000000000, 0.9659258262890683122, 1.000000000000000000, 0.9659258262890683122, 1.000000000000000000, 0.9659258262890683122, 1.000000000000000000, 0.9659258262890683122, 1.000000000000000000, 0.9659258262890683122, 1.000000000000000000, 0.9659258262890683122, 1.000000000000000000, 0.9659258262890683122, 1.000000000000000000, 0.9659258262890683122, 1.000000000000000000, 0.9659258262890683122, 1.000000000000000000, 0.9659258262890683122, 1.000000000000000000, 0.9659258262890683122, 1.000000000000000000, 0.9659258262890683122, 1.000000000000000000, 0.9659258262890683122, 1.000000000000000000, 0.9659258262890683122, 1.000000000000000000, 0.9659258262890683122, 1.000000000000000000, 0.9659258262890683122, 1.000000000000000000, 0.9659258262890683122, 1.000000000000000000, 0.9659258262890683122, 1.000000000000000000, 0.9659258262890683122, 1.000000000000000000, 0.9659258262890683122, 1.000000000000000000, 0.9659258262890683122, 1.000000000000000000, 0.9659258262890683122, 1.000000000000000000, 0.9659258262890683122, 1.000000000000000000, 0.9659258262890683122, 1.000000000000000000, 0.9659258262890683122, 1.000000000000000000, 0.9659258262890683122, 1.000000000000000000, 0.9659258262890683122, 1.000000000000000000, 0.9659258262890683122, 1.000000000000000000, 0.9659258262890683122, 1.000000000000000000, 0.9659258262890683122, 1.000000000000000000, 0.9659258262890683122, 1.000000000000000000, 0.9659258262890683122, 1.000000000000000000, 0.9659258262890683122, 1.000000000000000000, 0.9659258262890683122, 1.000000000000000000, 0.9659258262890683122, 1.000000000000000000, 0.9659258262890683122, 1.000000000000000000, 0.9659258262890683122, 1.000000000000000000, 0.9659258262890683122, 1.000000000000000000, 0.9659258262890683122, 1.000000000000000000, 0.9659258262890683122, 1.000000000000000000, 0.9659258262890683122, 1.000000000000000000, 0.9659258262890683122, 1.000000000000000000, 0.9659258262890683122, 1.000000000000000000, 0.9659258262890683122, 1.000000000000000000, 0.9659258262890683122, 1.000000000000000000, 0.9659258262890683122, 1.000000000000000000, 0.9659258262890683122, 1.000000000000000000, 0.9659258262890683122, 1.000000000000000000, 0.9659258262890683122, 1.000000000000000000, 0.9659258262890683122, 1.000000000000000000, 0.9659258262890683122, 1.000000000000000000, 0.9659258262890683122, 1.000000000000000000, 0.9659258262890683122, 1.000000000000000000, 0.9659258262890683122, 1.000000000000000000, 0.9659258262890683122, 1.000000000000000000, 0.9659258262890683122, 1.000000000000000000, 0.9659258262890683122, 1.000000000000000000, 0.9659258262890683122, 1.000000000000000000, 0.9659258262890683122, 1.000000000000000000, 0.9659258262890683122, 1.000000000000000000, 0.9659258262890683122, 1.000000000000000000, 0.9659258262890683122, 1.000000000000000000, 0.9659258262890683122, 1.000000000000000000, 0.9659258262890683122, 1.000000000000000000, 0.9659258262890683122, 1.000000000000000000, 0.9659258262890683122, 1.000000000000000000, 0.9659258262890683122, 1.000000000000000000, 0.9659258262890683122, 1.000000000000000000, 0.9659258262890683122, 1.000000000000000000, 0.9659258262890683122, 1.000000000000000000, 0.9659258262890683122, 1.000000000000000000, 0.9659258262890683122, 1.000000000000000000, 0.9659258262890683122, 1.000000000000000000, 0.9659258262890683122, 1.000000000000000000, 0.9659258262890683122, 1.000000000000000000, 0.9659258262890683122, 1.000000000000000000, 0.9659258262890683122, 1.000000000000000000, 0.9659258262890683122, 1.000000000000000000, 0.9659258262890683122, 1.000000000000000000, 0.9659258262890683122, 1.000000000000000000, 0.9659258262890683122, 1.000000000000000000, 0.9659258262890683122, 1.000000000000000000, 0.9659258262890683122, 1.000000000000000000, 0.9659258262890683122, 1.000000000000000000, 0.9659258262890683122, 1.000000000000000000, 0.9659258262890683122, 1.000000000000000000, 0.9659258262890683122, 1.000000000000000000, 0.9659258262890683122, 1.000000000000000000, 0.9659258262890683122, 1.000000000000000000, 0.9659258262890683122, 1.000000000000000000, 0.9659258262890683122, 1.000000000000000000, 0.9659258262890683122, 1.000000000000000000, 0.9659258262890683122, 1.000000000000000000, 0.9659258262890683122, 1.000000000000000000, 0.9659258262890683122, 1.000000000000000000, 0.9659258262890683122, 1.000000000000000000, 0.9659258262890683122, 1.000000000000000000, 0.9659258262890683122, 1.000000000000000000, 0.9659258262890683122, 1.000000000000000000, 0.9659258262890683122, 1.000000000000000000, 0.9659258262890683122, 1.000000000000000000, 0.9659258262890683122, 1.000000000000000000, 0.9659258262890683122, 1.000000000000000000, 0.9659258262890683122, 1.000000000000000000, 0.9659258262890683122, 1.000000000000000000, 0.9659258262890683122, 1.000000000000000000, 0.9659258262890683122, 1.000000000000000000, 0.9659258262890683122, 1.000000000000000000, 0.9659258262890683122, 1.000000000000000000, 0.9659258262890683122, 1.000000000000000000, 0.9659258262890683122, 1.000000000000000000, 0.9659258262890683122, 1.000000000000000000, 0.9659258262890683122, 1.000000000000000000, 0.9659258262890683122, 1.000000000000000000, 0.9659258262890683122, 1.000000000000000000, 0.9659258262890683122, 1.000000000000000000, 0.9659258262890683122, 1.000000000000000000, 0.9659258262890683122, 1.000000000000000000, 0.9659258262890683122, 1.000000000000000000, 0.9659258262890683122, 1.000000000000000000, 0.9659258262890683122, 1.000000000000000000, 0.9659258262890683122, 1.000000000000000000, 0.9659258262890683122, 1.000000000000000000, 0.9659258262890683122, 1.000000000000000000, 0.9659258262890683122, 1.000000000000000000, 0.9659258262890683122, 1.000000000000000000, 0.9659258262890683122, 1.000000000000000000, 0.9659258262890683122, 1.000000000000000000, 0.9659258262890683122, 1.000000000000000000, 0.9659258262890683122, 1.000000000000000000, 0.9659258262890683122, 1.000000000000000000, 0.9659258262890683122, 1.000000000000000000, 0.9659258262890683122, 1.000000000000000000, 0.9659258262890683122, 1.000000000000000000, 0.9659258262890683122, 1.000000000000000000, 0.9659258262890683122, 1.000000000000000000, 0.9659258262890683122, 1.000000000000000000, 0.9659258262890683122, 1.000000000000000000, 0.9659258262890683122, 1.000000000000000000, 0.9659258262890683122, 1.000000000000000000, 0.9659258262890683122, 1.000000000000000000, 0.9659258262890683122, 1.000000000000000000, 0.9659258262890683122, 1.000000000000000000, 0.9659258262890683122, 1.000000000000000000, 0.9659258262890683122, 1.000000000000000000, 0.9659258262890683122, 1.000000000000000000, 0.9659258262890683122, 1.000000000000000000, 0.9659258262890683122, 1.000000000000000000, 0.9659258262890683122, 1.000000000000000000, 0.9659258262890683122, 1.000000000000000000, 0.9659258262890683122, 1.000000000000000000, 0.9659258262890683122, 1.000000000000000000, 0.9659258262890683122, 1.000000000000000000, 0.9659258262890683122, 1.000000000000000000, 0.9659258262890683122, 1.000000000000000000, 0.9659258262890683122, 1.000000000000000000, 0.9659258262890683122, 1.000000000000000000, 0.9659258262890683122, 1.000000000000000000, 0.9659258262890683122, 1.000000000000000000, 0.9659258262890683122, 1.000000000000000000, 0.9659258262890683122, 1.000000000000000000, 0.9659258262890683122, 1.000000000000000000, 0.9659258262890683122, 1.000000000000000000, 0.9659258262890683122, 1.000000000000000000, 0.9659258262890683122, 1.000000000000000000, 0.9659258262890683122, 1.000000000000000000, 0.9659258262890683122, 1.000000000000000000, 0.9659258262890683122, 1.000000000000000000, 0.9659258262890683122, 1.000000000000000000, 0.9659258262890683122, 1.000000000000000000, 0.9659258262890683122, 1.000000000000000000, 0.9659258262890683122, 1.000000000000000000, 0.9659258262890683122, 1.000000000000000000, 0.9659258262890683122, 1.000000000000000000, 0.9659258262890683122, 1.000000000000000000, 0.9659258262890683122, 1.000000000000000000, 0.9659258262890683122, 1.000000000000000000, 0.9659258262890683122, 1.000000000000000000, 0.9659258262890683122, 1.000000000000000000, 0.9659258262890683122, 1.000000000000000000, 0.9659258262890683122, 1.000000000000000000, 0.9659258262890683122, 1.000000000000000000, 0.9659258262890683122, 1.000000000000000000, 0.9659258262890683122, 1.000000000000000000, 0.9659258262890683122, 1.000000000000000000, 0.9659258262890683122, 1.000000000000000000, 0.9659258262890683122, 1.000000000000000000, 0.9659258262890683122, 1.000000000000000000, 0.9659258262890683122, 1.000000000000000000, 0.9659258262890683122, 1.000000000000000000, 0.9659258262890683122, 1.000000000000000000, 0.9659258262890683122, 1.000000000000000000, 0.9659258262890683122, 1.000000000000000000, 0.9659258262890683122, 1.000000000000000000, 0.9659258262890683122, 1.000000000000000000, 0.9659258262890683122, 1.000000000000000000, 0.9659258262890683122, 1.000000000000000000, 0.9659258262890683122, 1.000000000000000000, 0.9659258262890683122, 1.000000000000000000, 0.9659258262890683122, 1.000000000000000000, 0.9659258262890683122, 1.000000000000000000, 0.9659258262890683122, 1.000000000000000000, 0.9659258262890683122, 1.000000000000000000, 0.9659258262890683122, 1.000000000000000000, 0.9659258262890683122, 1.000000000000000000, 0.9659258262890683122, 1.000000000000000000, 0.9659258262890683122, 1.000000000000000000, 0.9659258262890683122, 1.000000000000000000, 0.9659258262890683122, 1.000000000000000000, 0.9659258262890683122, 1.000000000000000000, 0.9659258262890683122, 1.000000000000000000, 0.9659258262890683122, 1.000000000000000000, 0.9659258262890683122, 1.000000000000000000, 0.9659258262890683122, 1.000000000000000000, 0.9659258262890683122, 1.000000000000000000, 0.9659258262890683122, 1.000000000000000000, 0.9659258262890683122, 1.000000000000000000, 0.9659258262890683122, 1.000000000000000000, 0.9659258262890683122, 1.000000000000000000, 0.9659258262890683122, 1.000000000000000000) ) ) 
 REPRESENTATION_ITEM ( '' )  SURFACE ( )  );
#51959 = CARTESIAN_POINT ( 'NONE',  ( 1.318897637795276356, -0.5400638737290844871, 0.3530559997133364547 ) ) ;
#51960 = CARTESIAN_POINT ( 'NONE',  ( -1.568241469816272105, -0.05778040916215522460, 0.4822834645669289988 ) ) ;
#51961 = CARTESIAN_POINT ( 'NONE',  ( 0.1958661417322834497, 0.3392501089628018329, -0.8543113928795783574 ) ) ;
#51962 = CARTESIAN_POINT ( 'NONE',  ( -0.1837270341207343505, -0.5023911411419708095, 0.1820866141732285504 ) ) ;
#51963 = CARTESIAN_POINT ( 'NONE',  ( -1.515748031496062076, -0.4536011799217367080, 0.2665933059059888421 ) ) ;
#51964 = CARTESIAN_POINT ( 'NONE',  ( 0.4531182788721080934, 1.535433070866141447, -0.5309055118110237448 ) ) ;
#51965 = CARTESIAN_POINT ( 'NONE',  ( -0.5314960629921250401, 0.07958543189024085140, 0.2665933059059887866 ) ) ;
#51966 = CARTESIAN_POINT ( 'NONE',  ( 0.08530183727034192087, -0.2845877964562161244, -0.3641732283464567121 ) ) ;
#51967 = CARTESIAN_POINT ( 'NONE',  ( 0.02624671916010564918, 0.2306618581243848609, 0.2411417322834645549 ) ) ;
#51968 = CARTESIAN_POINT ( 'NONE',  ( -0.9317585301837263412, -0.3690944881889765550, -0.3153832671262227771 ) ) ;
#51969 = CARTESIAN_POINT ( 'NONE',  ( -0.1958661417322836995, 0.3392501089628017219, -0.009861835466878533449 ) ) ;
#51970 = CARTESIAN_POINT ( 'NONE',  ( 0.8858267716535438430, -0.5400638737290845981, -0.3530559997133363437 ) ) ;
#51971 = EDGE_CURVE ( 'NONE', #79084, #63914, #55616, .T. ) ;
#51972 = CARTESIAN_POINT ( 'NONE',  ( -1.528871391076114250, -0.6692913385826771977, 0.1292274648535927661 ) ) ;
#51973 = CIRCLE ( 'NONE', #22450, 1.929133858267716661 ) ;
#51974 = CARTESIAN_POINT ( 'NONE',  ( 0.3458507752293908943, -0.3458507752293908943, -1.120078740157480324 ) ) ;
#51975 = VECTOR ( 'NONE', #64142, 39.37007874015749564 ) ;
#51976 = CARTESIAN_POINT ( 'NONE',  ( -0.3740157480314953431, -0.5400638737290845981, -0.3530559997133363437 ) ) ;
#51977 = CARTESIAN_POINT ( 'NONE',  ( 0.3346456692913390985, 0.07958543189024085140, 0.2665933059059887866 ) ) ;
#51978 = CARTESIAN_POINT ( 'NONE',  ( -0.9186351706036736120, -0.6046776061558809534, -0.2411417322834644161 ) ) ;
#51979 = CARTESIAN_POINT ( 'NONE',  ( 0.9711286089238851948, -0.5023911411419708095, -0.1820866141732282451 ) ) ;
#51980 = CARTESIAN_POINT ( 'NONE',  ( -0.4527559055118102749, 0.07958543189024085140, 0.2665933059059887866 ) ) ;
#51981 = CARTESIAN_POINT ( 'NONE',  ( -0.5314960629921254842, -0.5400638737290845981, -0.3530559997133363437 ) ) ;
#51982 = CARTESIAN_POINT ( 'NONE',  ( -1.561679790026246017, -0.4281496062992127816, -0.4176697321401328100 ) ) ;
#51983 = CARTESIAN_POINT ( 'NONE',  ( 0.000000000000000000, 0.000000000000000000, -1.220472440944881942 ) ) ;
#51984 = CARTESIAN_POINT ( 'NONE',  ( 1.371391076115485941, 0.1771653543307087630, 0.09757992244046791164 ) ) ;
#51985 = CARTESIAN_POINT ( 'NONE',  ( 0.5118110236220480003, -0.6692913385826771977, 8.415575281601705876E-17 ) ) ;
#51986 = CARTESIAN_POINT ( 'NONE',  ( -1.371391076115484609, -0.6692913385826771977, 0.1292274648535927661 ) ) ;
#51987 = CARTESIAN_POINT ( 'NONE',  ( -1.489501312335957062, -0.3162353388693409650, -0.4822834645669289433 ) ) ;
#51988 = VERTEX_POINT ( 'NONE', #2242 ) ;
#51989 = CARTESIAN_POINT ( 'NONE',  ( -0.2925321140481932369, 0.2925321140481931259, -2.458661417322834719 ) ) ;
#51990 = CARTESIAN_POINT ( 'NONE',  ( -1.036745406824146176, -0.3690944881889763329, 0.3153832671262228327 ) ) ;
#51991 = CARTESIAN_POINT ( 'NONE',  ( 0.5971128608923890191, -0.6692913385826771977, 0.1292274648535927661 ) ) ;
#51992 = CARTESIAN_POINT ( 'NONE',  ( -1.161417322834644716, -0.4536011799217368745, -0.2665933059059886201 ) ) ;
#51993 = CARTESIAN_POINT ( 'NONE',  ( -0.3460692066303957537, -0.1998031496062994405, -1.861548556430446366 ) ) ;
#51994 = CARTESIAN_POINT ( 'NONE',  ( -1.187664041994750175, -0.05778040916215560624, -0.4822834645669293319 ) ) ;
#51995 = CARTESIAN_POINT ( 'NONE',  ( 0.9251968503937015864, 0.1660481256975883668, -0.3530559997133364547 ) ) ;
#51996 = CARTESIAN_POINT ( 'NONE',  ( 0.4002624671916016896, -0.05778040916215522460, 0.4822834645669289988 ) ) ;
#51997 = CARTESIAN_POINT ( 'NONE',  ( -1.220472440944881054, 0.000000000000000000, 0.5309055118110237448 ) ) ;
#51998 = CARTESIAN_POINT ( 'NONE',  ( -1.666666666666665853, -0.004921259842519870586, -0.3153832671262229437 ) ) ;
#51999 = CARTESIAN_POINT ( 'NONE',  ( 0.3996062992125985480, 2.446882876249141654E-17, -0.9822834645669291653 ) ) ;
#52000 = CARTESIAN_POINT ( 'NONE',  ( 4.893765752498283924E-17, -0.3996062992125986035, -1.181102362204724310 ) ) ;
#52001 = CARTESIAN_POINT ( 'NONE',  ( 0.2891555358219910499, 0.2891555358219910499, -0.6102362204724410821 ) ) ;
#52002 = CARTESIAN_POINT ( 'NONE',  ( 1.016821367227983552, 1.537401574803149984, 0.4744094488188975722 ) ) ;
#52003 = CARTESIAN_POINT ( 'NONE',  ( 0.7020997375328090762, -0.2845877964562159024, 0.3641732283464567677 ) ) ;
#52004 = CARTESIAN_POINT ( 'NONE',  ( 0.4527559055118117182, -0.4536011799217367080, 0.2665933059059888421 ) ) ;
#52005 = CARTESIAN_POINT ( 'NONE',  ( 0.2230971128608929543, 0.05413385826771626580, -0.4176697321401330321 ) ) ;
#52006 = CARTESIAN_POINT ( 'NONE',  ( 1.207349081364829990, -0.6046776061558809534, -0.2411417322834644161 ) ) ;
#52007 = CARTESIAN_POINT ( 'NONE',  ( 0.1974969037888706092, -0.3420746716998660508, -1.585958005249344493 ) ) ;
#52008 = CARTESIAN_POINT ( 'NONE',  ( 0.5314960629921267055, -0.4536011799217367080, 0.2665933059059888421 ) ) ;
#52009 = CARTESIAN_POINT ( 'NONE',  ( -0.9186351706036736120, -0.6046776061558809534, -0.2411417322834644161 ) ) ;
#52010 = CARTESIAN_POINT ( 'NONE',  ( -1.240157480314959759, -0.5400638737290845981, -0.3530559997133363437 ) ) ;
#52011 = CARTESIAN_POINT ( 'NONE',  ( 1.030183727034121421, -0.05778040916215522460, 0.4822834645669289988 ) ) ;
#52012 = CARTESIAN_POINT ( 'NONE',  ( -0.2362204724409451284, 0.4091458600556402425, -1.430446194225721834 ) ) ;
#52013 = CARTESIAN_POINT ( 'NONE',  ( 0.3330030935778962586, -0.2065800153021633556, -2.755905511811022723 ) ) ;
#52014 = ORIENTED_EDGE ( 'NONE', *, *, #61781, .F. ) ;
#52015 = ORIENTED_EDGE ( 'NONE', *, *, #62252, .F. ) ;
#52016 = CARTESIAN_POINT ( 'NONE',  ( -1.253280839895012377, -0.05778040916215522460, 0.4822834645669289988 ) ) ;
#52017 = CARTESIAN_POINT ( 'NONE',  ( -0.5052493438320203589, 0.2952755905511810774, -0.1292274648535930714 ) ) ;
#52019 = CARTESIAN_POINT ( 'NONE',  ( -0.9514435695538050464, -0.05778040916215560624, -0.4822834645669293319 ) ) ;
#52018 = CARTESIAN_POINT ( 'NONE',  ( -0.9580052493438311334, -0.004921259842519870586, -0.3153832671262229437 ) ) ;
#52020 = CARTESIAN_POINT ( 'NONE',  ( 0.3917322834645668994, -0.1049643490035303134, -2.081345513614486276 ) ) ;
#52021 = DIRECTION ( 'NONE',  ( 1.047444401652940007E-14, -0.000000000000000000, -1.000000000000000000 ) ) ;
#52022 = CARTESIAN_POINT ( 'NONE',  ( 1.561679790026247350, 0.05413385826771626580, -0.4176697321401330321 ) ) ;
#52023 = CARTESIAN_POINT ( 'NONE',  ( -1.174540682414697335, -0.3162353388693409650, -0.4822834645669289433 ) ) ;
#52024 = CARTESIAN_POINT ( 'NONE',  ( 0.4658792650918640033, -0.3162353388693405765, 0.4822834645669290543 ) ) ;
#52025 = CARTESIAN_POINT ( 'NONE',  ( -0.8858267716535425107, -0.5400638737290844871, 0.3530559997133364547 ) ) ;
#52026 = CARTESIAN_POINT ( 'NONE',  ( 0.6233595800524939223, -0.3162353388693405765, 0.4822834645669290543 ) ) ;
#52027 = CARTESIAN_POINT ( 'NONE',  ( -0.3392501089628017219, -0.1958661417322836718, -1.461942257217847763 ) ) ;
#52028 = CARTESIAN_POINT ( 'NONE',  ( -0.7086614173228339419, -0.1870078740157479769, 0.3641732283464567677 ) ) ;
#52029 = ORIENTED_EDGE ( 'NONE', *, *, #40826, .F. ) ;
#52030 = CARTESIAN_POINT ( 'NONE',  ( 0.2891555358219910499, -0.2891555358219909944, -1.830708661417323135 ) ) ;
#52031 = AXIS2_PLACEMENT_3D ( 'NONE', #26426, #44512, #13392 ) ;
#52032 = ORIENTED_EDGE ( 'NONE', *, *, #79015, .F. ) ;
#52033 = CARTESIAN_POINT ( 'NONE',  ( -1.633858267716534529, -0.4536011799217368745, -0.2665933059059886201 ) ) ;
#52034 = MECHANICAL_DESIGN_GEOMETRIC_PRESENTATION_REPRESENTATION (  '', ( #30554 ), #39995 ) ;
#52035 = CARTESIAN_POINT ( 'NONE',  ( -1.279527559055116948, -0.5400638737290844871, 0.3530559997133364547 ) ) ;
#52036 = CARTESIAN_POINT ( 'NONE',  ( -1.377952755905511140, -0.6692913385826771977, 8.415575281601705876E-17 ) ) ;
#52037 = CARTESIAN_POINT ( 'NONE',  ( 0.2925321140481932369, 0.2925321140481932369, -0.6102362204724409711 ) ) ;
#52038 = CARTESIAN_POINT ( 'NONE',  ( -1.292650918635170010, -0.6692913385826771977, 0.1292274648535927661 ) ) ;
#52039 = CARTESIAN_POINT ( 'NONE',  ( -1.318897637795274802, -0.5400638737290845981, -0.3530559997133363437 ) ) ;
#52040 = CARTESIAN_POINT ( 'NONE',  ( -1.614173228346455824, 0.2952755905511811885, 0.000000000000000000 ) ) ;
#52041 = PLANE ( 'NONE',  #50928 ) ;
#52042 = CARTESIAN_POINT ( 'NONE',  ( 0.2690288713910767848, 0.1771653543307087630, 0.09757992244046791164 ) ) ;
#52043 = DIRECTION ( 'NONE',  ( 0.000000000000000000, 0.000000000000000000, -1.000000000000000000 ) ) ;
#52044 = CARTESIAN_POINT ( 'NONE',  ( 0.1049643490035304938, -0.3917322834645669549, -0.4849081364829396779 ) ) ;
#52045 = CARTESIAN_POINT ( 'NONE',  ( -0.4133858267716528645, 0.07958543189024071263, -0.2665933059059888421 ) ) ;
#52046 = CARTESIAN_POINT ( 'NONE',  ( -0.6167979002624665030, -0.4281496062992127816, -0.4176697321401328100 ) ) ;
#52047 = CARTESIAN_POINT ( 'NONE',  ( 1.502624671916010790, -0.3162353388693409650, -0.4822834645669289433 ) ) ;
#52048 = CARTESIAN_POINT ( 'NONE',  ( -0.3674540682414689785, 0.2306618581243848609, 0.2411417322834645549 ) ) ;
#52049 = EDGE_LOOP ( 'NONE', ( #34698, #8263, #11717, #20171 ) ) ;
#52050 = ORIENTED_EDGE ( 'NONE', *, *, #60654, .T. ) ;
#52051 = CARTESIAN_POINT ( 'NONE',  ( 0.3460692066303959202, -0.1998031496062991630, -1.914041994750656395 ) ) ;
#52052 = CARTESIAN_POINT ( 'NONE',  ( -0.8792650918635160906, -0.4281496062992124485, 0.4176697321401328655 ) ) ;
#52053 = CARTESIAN_POINT ( 'NONE',  ( 1.358267716535433323, -0.5400638737290845981, -0.3530559997133363437 ) ) ;
#52054 = CARTESIAN_POINT ( 'NONE',  ( -1.476377952755905110, -0.4536011799217368745, -0.2665933059059886201 ) ) ;
#52055 = CARTESIAN_POINT ( 'NONE',  ( -0.4724409448818898682, -8.678599364036362592E-17, -0.6692913385826770867 ) ) ;
#52056 = CARTESIAN_POINT ( 'NONE',  ( 1.939486441909066494, 1.160811571118570695, 0.2889173282905437290 ) ) ;
#52057 = CARTESIAN_POINT ( 'NONE',  ( -0.3917322834645669549, -0.1049643490035306603, -0.3530183727034120755 ) ) ;
#52058 = CARTESIAN_POINT ( 'NONE',  ( -0.2867679344610364334, -0.2867679344610367109, -2.033464566929133799 ) ) ;
#52059 = CARTESIAN_POINT ( 'NONE',  ( -0.4068241469816264999, -0.4281496062992124485, 0.4176697321401328655 ) ) ;
#52060 = CARTESIAN_POINT ( 'NONE',  ( -1.489501312335957062, -0.08942795157527998196, 0.3641732283464567121 ) ) ;
#52061 = CARTESIAN_POINT ( 'NONE',  ( -0.5774278215223089816, 0.2306618581243847221, -0.2411417322834647770 ) ) ;
#52062 = CARTESIAN_POINT ( 'NONE',  ( -0.3458507752293909498, 0.3458507752293907833, -2.616141732283464805 ) ) ;
#52063 = CARTESIAN_POINT ( 'NONE',  ( -1.391076115485563758, 0.2306618581243848609, 0.2411417322834645549 ) ) ;
#52064 = CARTESIAN_POINT ( 'NONE',  ( -0.9908136482939626788, -0.6692913385826773087, -0.1292274648535924053 ) ) ;
#52065 = CARTESIAN_POINT ( 'NONE',  ( -0.5380577427821514602, -0.4281496062992127816, -0.4176697321401328100 ) ) ;
#52066 = CARTESIAN_POINT ( 'NONE',  ( 0.3949938075777408852, 0.1058382717557500435, -2.721128608923885306 ) ) ;
#52067 = CARTESIAN_POINT ( 'NONE',  ( 1.082677165354331228, -0.4536011799217367080, 0.2665933059059888421 ) ) ;
#52068 = DIRECTION ( 'NONE',  ( -3.096699300667737957E-16, 1.000000000000000000, -0.000000000000000000 ) ) ;
#52069 = CARTESIAN_POINT ( 'NONE',  ( 0.5774278215223104249, 0.1283753931104748280, 0.1820866141732283561 ) ) ;
#52070 = CARTESIAN_POINT ( 'NONE',  ( 1.272965879265092637, -0.004921259842519576551, 0.3153832671262227771 ) ) ;
#52071 = CARTESIAN_POINT ( 'NONE',  ( 1.364829396325459854, -0.6046776061558809534, -0.2411417322834644161 ) ) ;
#52072 = CARTESIAN_POINT ( 'NONE',  ( 0.05905511811023709395, -0.4536011799217367080, 0.2665933059059888421 ) ) ;
#52073 = CARTESIAN_POINT ( 'NONE',  ( -0.3917322834645671215, 0.1049643490035301469, -1.599737532808399143 ) ) ;
#52074 = CARTESIAN_POINT ( 'NONE',  ( -0.9842519685039360366, 0.2952755905511811885, 0.000000000000000000 ) ) ;
#52075 = CARTESIAN_POINT ( 'NONE',  ( 1.102362204724410155, -0.1870078740157479769, 0.4822834645669291653 ) ) ;
#52076 = CARTESIAN_POINT ( 'NONE',  ( 0.4091458600556403535, 0.2362204724409449896, 0.1069553805774278027 ) ) ;
#52077 = CARTESIAN_POINT ( 'NONE',  ( -0.5643044619422565855, -0.3690944881889763329, 0.3153832671262228327 ) ) ;
#52078 = CARTESIAN_POINT ( 'NONE',  ( -0.4396325459317579343, 0.2952755905511811885, 0.1292274648535926551 ) ) ;
#52079 = CARTESIAN_POINT ( 'NONE',  ( 0.2559055118110243332, 0.1660481256975885056, 0.3530559997133364547 ) ) ;
#52080 = CARTESIAN_POINT ( 'NONE',  ( 1.030183727034121421, -0.2845877964562161244, -0.3641732283464567121 ) ) ;
#52081 = CARTESIAN_POINT ( 'NONE',  ( 0.05905511811023681640, 0.07958543189024071263, -0.2665933059059888421 ) ) ;
#52082 = CARTESIAN_POINT ( 'NONE',  ( -0.1312335958005241554, -0.6046776061558809534, -0.2411417322834644161 ) ) ;
#52083 = CARTESIAN_POINT ( 'NONE',  ( -1.509186351706035767, 0.05413385826771626580, -0.4176697321401330321 ) ) ;
#52084 = CARTESIAN_POINT ( 'NONE',  ( -0.8070866141732276899, 0.07958543189024071263, -0.2665933059059888421 ) ) ;
#52085 = CARTESIAN_POINT ( 'NONE',  ( -1.586052503253846169, 1.850393700787402729, 0.1653254495020583248 ) ) ;
#52086 = CARTESIAN_POINT ( 'NONE',  ( 0.7349081364829403995, 0.2306618581243848609, 0.2411417322834645549 ) ) ;
#52087 = CARTESIAN_POINT ( 'NONE',  ( -1.036745406824146176, -0.4281496062992124485, 0.4176697321401328655 ) ) ;
#52088 = CARTESIAN_POINT ( 'NONE',  ( -0.1070741851644056997, 0.3996062992125984925, -1.028215223097112663 ) ) ;
#52089 =( BOUNDED_CURVE ( )  B_SPLINE_CURVE ( 2, ( #21043, #34505, #41637, #53839, #10076, #29007, #27766, #42047, #9250, #22285, #53431, #53005, #34084 ),
 .UNSPECIFIED., .F., .F. ) 
 B_SPLINE_CURVE_WITH_KNOTS ( ( 3, 2, 2, 2, 2, 2, 3 ),
 ( 0.7875000000000000888, 0.7916666666666667407, 0.7958333333333333925, 0.8000000000000000444, 0.8041666666666666963, 0.8083333333333333481, 0.8125000000000000000 ),
 .UNSPECIFIED. ) 
 CURVE ( )  GEOMETRIC_REPRESENTATION_ITEM ( )  RATIONAL_B_SPLINE_CURVE ( ( 0.9999999999999991118, 0.9659258262890692004, 1.000000000000000000, 0.9659258262890683122, 1.000000000000000000, 0.9659258262890683122, 1.000000000000000000, 0.9659258262890683122, 1.000000000000000000, 0.9659258262890683122, 1.000000000000000000, 0.9659258262890683122, 1.000000000000000000 ) ) 
 REPRESENTATION_ITEM ( '' )  );
#52090 = CARTESIAN_POINT ( 'NONE',  ( -0.3392501089628017219, -0.1958661417322836718, -2.656824146981627166 ) ) ;
#52091 = CARTESIAN_POINT ( 'NONE',  ( 0.2230971128608929543, -0.004921259842519870586, -0.3153832671262229437 ) ) ;
#52093 = CIRCLE ( 'NONE', #64246, 0.5118110236220471121 ) ;
#52092 = CARTESIAN_POINT ( 'NONE',  ( -0.8923884514435688198, -0.6046776061558807314, 0.2411417322834647770 ) ) ;
#52094 = CARTESIAN_POINT ( 'NONE',  ( -1.154855643044618851, 0.2306618581243848609, 0.2411417322834645549 ) ) ;
#52095 = CARTESIAN_POINT ( 'NONE',  ( -1.266404199475064773, -0.08942795157528024563, -0.3641732283464568787 ) ) ;
#52096 = DIRECTION ( 'NONE',  ( 0.000000000000000000, 0.000000000000000000, -1.000000000000000000 ) ) ;
#52097 = CARTESIAN_POINT ( 'NONE',  ( -0.9908136482939626788, 0.1771653543307087630, 0.09757992244046791164 ) ) ;
#52098 = CARTESIAN_POINT ( 'NONE',  ( -1.430446194225721390, -0.3690944881889763329, 0.3153832671262228327 ) ) ;
#52099 = CARTESIAN_POINT ( 'NONE',  ( 1.279527559055118724, 0.1660481256975885056, 0.3530559997133364547 ) ) ;
#52100 = CARTESIAN_POINT ( 'NONE',  ( 0.1181102362204724254, -0.04921259842519686706, -0.08523872084492506440 ) ) ;
#52101 = CARTESIAN_POINT ( 'NONE',  ( -0.3917322834645670659, -7.196005306013484475E-17, -2.555793593997062629 ) ) ;
#52102 = ORIENTED_EDGE ( 'NONE', *, *, #76299, .T. ) ;
#52103 = CARTESIAN_POINT ( 'NONE',  ( -0.2262115530851587786, -2.191421614605370878E-15, 0.4445507791589071167 ) ) ;
#52104 = EDGE_CURVE ( 'NONE', #15218, #14378, #54564, .T. ) ;
#52105 = CARTESIAN_POINT ( 'NONE',  ( 1.601049868766404982, 0.1283753931104748280, 0.1820866141732283561 ) ) ;
#52106 = CARTESIAN_POINT ( 'NONE',  ( -1.240157480314959759, 0.1660481256975885056, 0.3530559997133364547 ) ) ;
#52107 = CARTESIAN_POINT ( 'NONE',  ( 1.437007874015748810, 0.1660481256975885056, 0.3530559997133364547 ) ) ;
#52108 = CARTESIAN_POINT ( 'NONE',  ( -0.1049643490035307020, 0.3917322834645669549, -1.823490813648294129 ) ) ;
#52109 = FACE_OUTER_BOUND ( 'NONE', #13679, .T. ) ;
#52110 = EDGE_CURVE ( 'NONE', #70238, #44445, #14405, .T. ) ;
#52111 = CARTESIAN_POINT ( 'NONE',  ( 0.6364829396325465405, -0.3162353388693409650, -0.4822834645669289433 ) ) ;
#52112 = CARTESIAN_POINT ( 'NONE',  ( -0.1574803149606292529, -0.1870078740157480879, -0.4822834645669291653 ) ) ;
#52113 = CARTESIAN_POINT ( 'NONE',  ( 0.2372349296589321144, 1.126275035012231918, -3.929877705396449539 ) ) ;
#52114 = CARTESIAN_POINT ( 'NONE',  ( -0.7233831536534669482, 2.176714048050446326, -0.5048085489442492024 ) ) ;
#52115 = CARTESIAN_POINT ( 'NONE',  ( 0.9055118110236227702, -0.5511811023622047445, 6.969142054262312111E-17 ) ) ;
#52116 = CARTESIAN_POINT ( 'NONE',  ( -0.1998031496062991907, -0.3460692066303959757, -1.325459317585301777 ) ) ;
#52117 = ORIENTED_EDGE ( 'NONE', *, *, #51302, .T. ) ;
#52118 = CARTESIAN_POINT ( 'NONE',  ( -0.3917322834645671770, 0.1049643490035302024, 0.1279334401236726371 ) ) ;
#52119 = ORIENTED_EDGE ( 'NONE', *, *, #23584, .T. ) ;
#52120 = CARTESIAN_POINT ( 'NONE',  ( 0.1181102362204730916, -0.6692913385826771977, 8.415575281601705876E-17 ) ) ;
#52121 = CARTESIAN_POINT ( 'NONE',  ( 1.141732283464567566, 0.2952755905511811885, 0.000000000000000000 ) ) ;
#52122 = CARTESIAN_POINT ( 'NONE',  ( 0.8464566929133866546, -0.5400638737290844871, 0.3530559997133364547 ) ) ;
#52123 = CARTESIAN_POINT ( 'NONE',  ( 1.397637795275591177, 0.1660481256975883668, -0.3530559997133364547 ) ) ;
#52124 = CARTESIAN_POINT ( 'NONE',  ( -0.6889763779527552368, 0.1660481256975885056, 0.3530559997133364547 ) ) ;
#52125 = CARTESIAN_POINT ( 'NONE',  ( 0.07217847769028949700, -0.05778040916215560624, -0.4822834645669293319 ) ) ;
#52126 = CARTESIAN_POINT ( 'NONE',  ( 1.391076115485564868, -0.6046776061558807314, 0.2411417322834647770 ) ) ;
#52127 = CARTESIAN_POINT ( 'NONE',  ( 1.200787401574803681, -0.5400638737290845981, -0.3530559997133363437 ) ) ;
#52128 = CARTESIAN_POINT ( 'NONE',  ( 1.305774278215223960, -0.6692913385826771977, 0.1292274648535927661 ) ) ;
#52129 = CARTESIAN_POINT ( 'NONE',  ( 5.463695987328526437E-16, -0.1870078740157479769, 0.4822834645669291653 ) ) ;
#52130 = EDGE_CURVE ( 'NONE', #38353, #81379, #30094, .T. ) ;
#52131 = CARTESIAN_POINT ( 'NONE',  ( -0.3392501089628019995, 0.1958661417322832277, -0.3333333333333333148 ) ) ;
#52132 = CARTESIAN_POINT ( 'NONE',  ( 0.3477690288713918276, -0.5511811023622048555, -0.09757992244046775898 ) ) ;
#52133 = ORIENTED_EDGE ( 'NONE', *, *, #16548, .T. ) ;
#52134 = CARTESIAN_POINT ( 'NONE',  ( -0.1974969037888706647, 0.3420746716998658843, -0.4855643044619423754 ) ) ;
#52135 = EDGE_LOOP ( 'NONE', ( #44855, #83114, #31223, #39013 ) ) ;
#52136 = CARTESIAN_POINT ( 'NONE',  ( -0.5708661417322828946, 0.07958543189024071263, -0.2665933059059888421 ) ) ;
#52137 = CARTESIAN_POINT ( 'NONE',  ( -0.006561679790025524116, -0.05778040916215560624, -0.4822834645669293319 ) ) ;
#52138 = CARTESIAN_POINT ( 'NONE',  ( -0.4724409448818899238, 0.1265901696524986964, -0.1902887139107611314 ) ) ;
#52139 = CARTESIAN_POINT ( 'NONE',  ( 0.1509186351706042484, -0.3162353388693405765, 0.4822834645669290543 ) ) ;
#52140 = CARTESIAN_POINT ( 'NONE',  ( 0.1312335958005255154, -0.6046776061558807314, 0.2411417322834647770 ) ) ;
#52141 = EDGE_CURVE ( 'NONE', #50999, #4208, #37572, .T. ) ;
#52142 = CARTESIAN_POINT ( 'NONE',  ( -1.115485564304461219, -0.4281496062992124485, 0.4176697321401328655 ) ) ;
#52143 = CARTESIAN_POINT ( 'NONE',  ( 1.292650918635171564, -0.5511811023622048555, -0.09757992244046775898 ) ) ;
#52144 = CARTESIAN_POINT ( 'NONE',  ( -1.601049868766403650, 0.2306618581243847221, -0.2411417322834647770 ) ) ;
#52145 = CARTESIAN_POINT ( 'NONE',  ( 0.5314960629921349211, 2.716535433070866645, -2.543486866223387377 ) ) ;
#52146 = CARTESIAN_POINT ( 'NONE',  ( 1.069553805774278610, -0.5511811023622046335, 0.09757992244046803654 ) ) ;
#52147 = CARTESIAN_POINT ( 'NONE',  ( 0.3477690288713918276, -0.6692913385826773087, -0.1292274648535924053 ) ) ;
#52148 = CARTESIAN_POINT ( 'NONE',  ( 0.7283464566929143125, 0.1660481256975885056, 0.3530559997133364547 ) ) ;
#52149 = CARTESIAN_POINT ( 'NONE',  ( -9.787531504996567848E-17, 0.3996062992125986035, -1.417322834645669216 ) ) ;
#52150 = DIRECTION ( 'NONE',  ( -0.4043106043482678214, -0.6467352376403849856, 0.6467352376403909808 ) ) ;
#52151 = CARTESIAN_POINT ( 'NONE',  ( -0.1998031496062994405, 0.3460692066303957537, -0.7198162729658792447 ) ) ;
#52152 = CARTESIAN_POINT ( 'NONE',  ( -9.787531504996566615E-17, 0.3996062992125985480, 0.08070866141732281618 ) ) ;
#52153 = CARTESIAN_POINT ( 'NONE',  ( -0.08530183727034056085, -0.05778040916215560624, -0.4822834645669293319 ) ) ;
#52154 = B_SPLINE_CURVE_WITH_KNOTS ( 'NONE', 3,
 ( #83121, #30938, #36850, #10776 ),
 .UNSPECIFIED., .F., .F.,
 ( 4, 4 ),
 ( 0.2172790356422210356, 0.2186919052326019575 ),
 .UNSPECIFIED. ) ;
#52155 = CARTESIAN_POINT ( 'NONE',  ( 0.3460692066303959757, -0.1998031496062991907, -2.624671916010498762 ) ) ;
#52156 = CARTESIAN_POINT ( 'NONE',  ( -0.3392501089628019995, 0.1958661417322832277, -2.000656167979002920 ) ) ;
#52157 = CARTESIAN_POINT ( 'NONE',  ( -1.036745406824146176, -0.3690944881889763329, 0.3153832671262228327 ) ) ;
#52158 = CARTESIAN_POINT ( 'NONE',  ( 1.292650918635171564, 0.2952755905511811885, 0.1292274648535926551 ) ) ;
#52159 = AXIS2_PLACEMENT_3D ( 'NONE', #71903, #58422, #52933 ) ;
#52160 = CARTESIAN_POINT ( 'NONE',  ( 1.397637795275591177, 0.1660481256975883668, -0.3530559997133364547 ) ) ;
#52161 = CARTESIAN_POINT ( 'NONE',  ( -0.4330708661417315697, -0.5511811023622047445, 6.969142054262312111E-17 ) ) ;
#52162 = CARTESIAN_POINT ( 'NONE',  ( 0.6299212598425204535, -0.1870078740157479769, 0.4822834645669291653 ) ) ;
#52163 = CARTESIAN_POINT ( 'NONE',  ( -1.157146581871515012E-16, 0.4724409448818898682, -1.651574803149606474 ) ) ;
#52164 = CARTESIAN_POINT ( 'NONE',  ( 0.4265091863517067594, 0.1771653543307087630, 0.09757992244046791164 ) ) ;
#52165 = CARTESIAN_POINT ( 'NONE',  ( -0.1574803149606292529, -0.1870078740157479769, 0.4822834645669291653 ) ) ;
#52166 = CARTESIAN_POINT ( 'NONE',  ( -0.1058382717557497660, -0.3949938075777411073, -1.408792650918635259 ) ) ;
#52167 = CARTESIAN_POINT ( 'NONE',  ( -1.030183727034119867, -0.05778040916215560624, -0.4822834645669293319 ) ) ;
#52168 = CARTESIAN_POINT ( 'NONE',  ( 0.3149606299212603933, -0.1870078740157479769, 0.3641732283464567677 ) ) ;
#52169 = EDGE_CURVE ( 'NONE', #13953, #71224, #79692, .T. ) ;
#52170 = CARTESIAN_POINT ( 'NONE',  ( -1.171093442848938793, -2.191421614605370878E-15, 0.4445507791589071167 ) ) ;
#52171 = CARTESIAN_POINT ( 'NONE',  ( -0.8267716535433065062, -0.6692913385826771977, 8.415575281601705876E-17 ) ) ;
#52172 = CARTESIAN_POINT ( 'NONE',  ( -0.4330708661417315697, -0.5511811023622047445, 6.969142054262312111E-17 ) ) ;
#52173 = CARTESIAN_POINT ( 'NONE',  ( -0.03443470937339728616, 0.2755905511811023723, -1.656110380428732265 ) ) ;
#52174 = CARTESIAN_POINT ( 'NONE',  ( -0.5905511811023615998, 0.2952755905511811885, 0.000000000000000000 ) ) ;
#52175 = CARTESIAN_POINT ( 'NONE',  ( -0.3215223097112853146, -0.05778040916215560624, -0.4822834645669293319 ) ) ;
#52176 = CARTESIAN_POINT ( 'NONE',  ( 0.2099737532808405305, 0.1283753931104746893, -0.1820866141732285504 ) ) ;
#52177 = CARTESIAN_POINT ( 'NONE',  ( -0.3996062992125984925, -0.1070741851644056858, -2.169947506561679340 ) ) ;
#52178 = CARTESIAN_POINT ( 'NONE',  ( -0.04593175853018302557, 0.2952755905511811885, 0.1292274648535926551 ) ) ;
#52179 = CARTESIAN_POINT ( 'NONE',  ( 0.3917322834645668994, -0.1049643490035303134, -2.081345513614486276 ) ) ;
#52180 = CARTESIAN_POINT ( 'NONE',  ( -1.725721784776902190, -0.08942795157527998196, 0.3641732283464567121 ) ) ;
#52181 = CARTESIAN_POINT ( 'NONE',  ( 0.7152230971128616943, -0.08942795157527998196, 0.3641732283464567121 ) ) ;
#52182 = CARTESIAN_POINT ( 'NONE',  ( 1.522309711286089939, -0.6046776061558809534, -0.2411417322834644161 ) ) ;
#52183 = CARTESIAN_POINT ( 'NONE',  ( -0.7677165354330699465, 0.07958543189024085140, 0.2665933059059887866 ) ) ;
#52184 = CARTESIAN_POINT ( 'NONE',  ( -1.115485564304461219, -0.3690944881889763329, 0.3153832671262228327 ) ) ;
#52185 = CARTESIAN_POINT ( 'NONE',  ( -0.6167979002624665030, -0.4281496062992127816, -0.4176697321401328100 ) ) ;
#52186 = CARTESIAN_POINT ( 'NONE',  ( -0.01968503937007793844, -0.5400638737290844871, 0.3530559997133364547 ) ) ;
#52187 = CARTESIAN_POINT ( 'NONE',  ( 0.5052493438320218022, -0.5511811023622048555, -0.09757992244046775898 ) ) ;
#52188 = CARTESIAN_POINT ( 'NONE',  ( -0.2524317427257168345, 0.1533591454305971991, 5.791393970467346719 ) ) ;
#52189 = CARTESIAN_POINT ( 'NONE',  ( 0.9448818897637802916, -0.1870078740157479769, 0.3641732283464567677 ) ) ;
#52190 = EDGE_CURVE ( 'NONE', #58992, #28368, #6414, .T. ) ;
#52191 = CARTESIAN_POINT ( 'NONE',  ( 0.4199475065616805614, 0.2306618581243848609, 0.2411417322834645549 ) ) ;
#52192 = CARTESIAN_POINT ( 'NONE',  ( 0.3996062992125985480, 2.446882876249141654E-17, -0.03740157480314962313 ) ) ;
#52193 = CARTESIAN_POINT ( 'NONE',  ( -0.8792650918635160906, 0.05413385826771626580, -0.4176697321401330321 ) ) ;
#52194 = CARTESIAN_POINT ( 'NONE',  ( -0.3917322834645669549, -0.1049643490035306603, -1.390419947506561504 ) ) ;
#52195 = CARTESIAN_POINT ( 'NONE',  ( 1.535433070866142335, -0.5511811023622047445, 6.969142054262312111E-17 ) ) ;
#52196 = CARTESIAN_POINT ( 'NONE',  ( 0.4461942257217856311, 0.2306618581243847221, -0.2411417322834647770 ) ) ;
#52197 = CARTESIAN_POINT ( 'NONE',  ( 0.1706036745406830368, -0.4281496062992127816, -0.4176697321401328100 ) ) ;
#52198 = CARTESIAN_POINT ( 'NONE',  ( 0.4744094488189052328, 1.537401574803149984, -2.170146923806634653 ) ) ;
#52199 = CARTESIAN_POINT ( 'NONE',  ( -0.02624671916010428221, 0.1283753931104746893, -0.1820866141732285504 ) ) ;
#52200 = CARTESIAN_POINT ( 'NONE',  ( 0.9514435695538062676, -0.3162353388693409650, -0.4822834645669289433 ) ) ;
#52201 = CARTESIAN_POINT ( 'NONE',  ( -0.1377952755905504645, 0.07958543189024085140, 0.2665933059059887866 ) ) ;
#52202 = CARTESIAN_POINT ( 'NONE',  ( -0.6102362204724400829, -0.5400638737290845981, -0.3530559997133363437 ) ) ;
#52203 = CARTESIAN_POINT ( 'NONE',  ( 5.785732909357575061E-17, -0.4724409448818898682, -2.598425196850393970 ) ) ;
#52204 = CARTESIAN_POINT ( 'NONE',  ( -0.2821522309711278487, 0.2952755905511811885, 0.1292274648535926551 ) ) ;
#52205 = ORIENTED_EDGE ( 'NONE', *, *, #49228, .T. ) ;
#52206 = CARTESIAN_POINT ( 'NONE',  ( -1.095800524934382292, -0.3162353388693409650, -0.4822834645669289433 ) ) ;
#52207 = CARTESIAN_POINT ( 'NONE',  ( -0.5249343832020990641, -0.5023911411419708095, -0.1820866141732282451 ) ) ;
#52208 = CARTESIAN_POINT ( 'NONE',  ( 0.03937007874015806264, 0.2952755905511811885, 0.000000000000000000 ) ) ;
#52209 = CARTESIAN_POINT ( 'NONE',  ( -1.154855643044618851, -0.6046776061558809534, -0.2411417322834644161 ) ) ;
#52210 = CARTESIAN_POINT ( 'NONE',  ( -0.8595800524934373854, -0.05778040916215522460, 0.4822834645669289988 ) ) ;
#52211 = ADVANCED_FACE ( 'NONE', ( #48083 ), #9987, .T. ) ;
#52212 = CARTESIAN_POINT ( 'NONE',  ( -0.3503937007874015630, -0.3051181102362204856, -0.01968503937007903132 ) ) ;
#52214 = CARTESIAN_POINT ( 'NONE',  ( 0.8202099737532813073, 0.2952755905511811885, 0.1292274648535926551 ) ) ;
#52213 = CARTESIAN_POINT ( 'NONE',  ( 1.666666666666667185, 0.05413385826771666132, 0.4176697321401328100 ) ) ;
#52215 = CARTESIAN_POINT ( 'NONE',  ( 1.246719160104987623, 0.05413385826771626580, -0.4176697321401330321 ) ) ;
#52216 = CARTESIAN_POINT ( 'NONE',  ( -0.3392501089628019995, 0.1958661417322832277, -2.380577427821522374 ) ) ;
#52217 = CARTESIAN_POINT ( 'NONE',  ( -1.548556430446193399, -0.6046776061558809534, -0.2411417322834644161 ) ) ;
#52218 = CARTESIAN_POINT ( 'NONE',  ( -1.417322834645668772, -0.1870078740157479769, 0.4822834645669291653 ) ) ;
#52219 = CARTESIAN_POINT ( 'NONE',  ( 0.1265901696524990294, -0.4724409448818896462, -0.5577427821522309426 ) ) ;
#52220 = CARTESIAN_POINT ( 'NONE',  ( -0.3996062992125986035, -7.340648628747425578E-17, -0.1968503937007874405 ) ) ;
#52221 = ORIENTED_EDGE ( 'NONE', *, *, #17674, .T. ) ;
#52222 = CARTESIAN_POINT ( 'NONE',  ( -0.06561679790026180015, -0.004921259842519576551, 0.3153832671262227771 ) ) ;
#52223 = CARTESIAN_POINT ( 'NONE',  ( 4.797336870675656522E-17, -0.3917322834645670104, -1.645669291338582640 ) ) ;
#52224 = ORIENTED_EDGE ( 'NONE', *, *, #64962, .T. ) ;
#52225 = CARTESIAN_POINT ( 'NONE',  ( 0.1181102362204730916, -0.6692913385826771977, 8.415575281601705876E-17 ) ) ;
#52226 = CARTESIAN_POINT ( 'NONE',  ( 0.2099737532808405305, 0.2306618581243847221, -0.2411417322834647770 ) ) ;
#52227 = CARTESIAN_POINT ( 'NONE',  ( -0.1990279662527743021, 0.1990279662527742188, 0.1112963449492363477 ) ) ;
#52228 = DIRECTION ( 'NONE',  ( 0.000000000000000000, 0.000000000000000000, -1.000000000000000000 ) ) ;
#52229 = CARTESIAN_POINT ( 'NONE',  ( -0.7545931758530176614, -0.5511811023622048555, -0.09757992244046775898 ) ) ;
#52230 = CARTESIAN_POINT ( 'NONE',  ( -0.2087913723976026203, -0.2087913723976025926, 0.1248231986745540339 ) ) ;
#52231 = CARTESIAN_POINT ( 'NONE',  ( 0.7808398950131241190, -0.05778040916215560624, -0.4822834645669293319 ) ) ;
#52232 = CARTESIAN_POINT ( 'NONE',  ( 1.135170603674541256, 0.1771653543307087630, 0.09757992244046791164 ) ) ;
#52233 = CARTESIAN_POINT ( 'NONE',  ( -0.3871391076115476282, -0.05778040916215522460, 0.4822834645669289988 ) ) ;
#52234 = CARTESIAN_POINT ( 'NONE',  ( 4.797336870675655290E-17, -0.3917322834645669549, -1.261135539861205412 ) ) ;
#52235 = CARTESIAN_POINT ( 'NONE',  ( -0.6233595800524928121, -0.3162353388693409650, -0.4822834645669289433 ) ) ;
#52236 = CARTESIAN_POINT ( 'NONE',  ( 2.795275590551181910, 1.726086921369709426, 0.000000000000000000 ) ) ;
#52237 = CARTESIAN_POINT ( 'NONE',  ( 1.174540682414699111, -0.3162353388693405765, 0.4822834645669290543 ) ) ;
#52238 = DIRECTION ( 'NONE',  ( -1.000000000000000000, -0.000000000000000000, -0.000000000000000000 ) ) ;
#52239 = ORIENTED_EDGE ( 'NONE', *, *, #24452, .F. ) ;
#52240 = CARTESIAN_POINT ( 'NONE',  ( 0.2867679344610366554, -0.2867679344610365999, -2.614848712107298745 ) ) ;
#52241 = CARTESIAN_POINT ( 'NONE',  ( 0.1706036745406830368, -0.4281496062992127816, -0.4176697321401328100 ) ) ;
#52242 = ORIENTED_EDGE ( 'NONE', *, *, #77894, .T. ) ;
#52243 = CARTESIAN_POINT ( 'NONE',  ( -0.6692913385826764205, -0.6692913385826771977, 8.415575281601705876E-17 ) ) ;
#52244 = CARTESIAN_POINT ( 'NONE',  ( 1.227034120734908917, -0.6692913385826771977, 0.1292274648535927661 ) ) ;
#52245 = CARTESIAN_POINT ( 'NONE',  ( 1.253280839895013710, -0.3162353388693405765, 0.4822834645669290543 ) ) ;
#52246 = CARTESIAN_POINT ( 'NONE',  ( 0.4461942257217855201, -0.6046776061558807314, 0.2411417322834647770 ) ) ;
#52247 = CARTESIAN_POINT ( 'NONE',  ( -0.2296587926509179312, -0.05778040916215522460, 0.4822834645669289988 ) ) ;
#52248 = CARTESIAN_POINT ( 'NONE',  ( 0.3917322834645670104, -0.1049643490035303411, -1.928477690288713742 ) ) ;
#52249 = CARTESIAN_POINT ( 'NONE',  ( -1.148293963254592542, -0.6692913385826773087, -0.1292274648535924053 ) ) ;
#52250 = CARTESIAN_POINT ( 'NONE',  ( 0.01312335958005323398, -0.4281496062992127816, -0.4176697321401328100 ) ) ;
#52251 = CARTESIAN_POINT ( 'NONE',  ( 0.01312335958005323398, -0.3690944881889765550, -0.3153832671262227771 ) ) ;
#52252 = CARTESIAN_POINT ( 'NONE',  ( 1.581364829396326277, -0.3162353388693409650, -0.4822834645669289433 ) ) ;
#52253 = CARTESIAN_POINT ( 'NONE',  ( 1.318897637795276356, -0.5400638737290844871, 0.3530559997133364547 ) ) ;
#52254 = CARTESIAN_POINT ( 'NONE',  ( -0.4199475065616791736, 0.2306618581243847221, -0.2411417322834647770 ) ) ;
#52255 = CARTESIAN_POINT ( 'NONE',  ( -0.5314960629921197111, 2.755905511811024056, -1.813482582612295557 ) ) ;
#52256 = CARTESIAN_POINT ( 'NONE',  ( 1.043307086614173818, -0.5400638737290845981, -0.3530559997133363437 ) ) ;
#52257 = DIRECTION ( 'NONE',  ( 0.000000000000000000, 0.000000000000000000, 1.000000000000000000 ) ) ;
#52258 = ORIENTED_EDGE ( 'NONE', *, *, #2422, .T. ) ;
#52259 = CARTESIAN_POINT ( 'NONE',  ( 0.3018372703412079971, 0.05413385826771626580, -0.4176697321401330321 ) ) ;
#52260 = CARTESIAN_POINT ( 'NONE',  ( -0.09842519685039295696, 0.07958543189024071263, -0.2665933059059888421 ) ) ;
#52262 = CARTESIAN_POINT ( 'NONE',  ( -0.9055118110236215490, 0.2066929133858268208, 0.000000000000000000 ) ) ;
#52261 = CARTESIAN_POINT ( 'NONE',  ( 1.391076115485564868, 0.1283753931104746893, -0.1820866141732285504 ) ) ;
#52263 = CARTESIAN_POINT ( 'NONE',  ( 5.785732909357575061E-17, -0.4724409448818898682, -0.3129921259842520231 ) ) ;
#52264 = CARTESIAN_POINT ( 'NONE',  ( 1.535433070866142558, 0.1771653543307087630, 0.000000000000000000 ) ) ;
#52265 = EDGE_CURVE ( 'NONE', #30219, #29058, #20743, .T. ) ;
#52266 = CARTESIAN_POINT ( 'NONE',  ( 1.076115485564305141, -0.6046776061558807314, 0.2411417322834647770 ) ) ;
#52267 = CARTESIAN_POINT ( 'NONE',  ( -0.3420746716998660508, -0.1974969037888706924, 0.02821522309711286050 ) ) ;
#52268 = CARTESIAN_POINT ( 'NONE',  ( 0.1377952755905518800, -0.5400638737290844871, 0.3530559997133364547 ) ) ;
#52269 = DIRECTION ( 'NONE',  ( 0.000000000000000000, -1.000000000000000000, 0.000000000000000000 ) ) ;
#52270 = CARTESIAN_POINT ( 'NONE',  ( -1.620734908136482577, -0.6692913385826773087, -0.1292274648535924053 ) ) ;
#52271 = CARTESIAN_POINT ( 'NONE',  ( -0.1837270341207343505, -0.6046776061558807314, 0.2411417322834647770 ) ) ;
#52272 = EDGE_CURVE ( 'NONE', #11553, #5025, #48492, .T. ) ;
#52273 = CARTESIAN_POINT ( 'NONE',  ( 0.1058382717557500852, -0.3949938075777408852, -0.1620734908136483021 ) ) ;
#52274 = CARTESIAN_POINT ( 'NONE',  ( 1.509186351706037543, 0.05413385826771666132, 0.4176697321401328100 ) ) ;
#52275 = CARTESIAN_POINT ( 'NONE',  ( 0.6824146981627303710, 0.2306618581243847221, -0.2411417322834647770 ) ) ;
#52276 = CARTESIAN_POINT ( 'NONE',  ( 1.069553805774278832, 0.1771653543307087075, -0.09757992244046823083 ) ) ;
#52277 = CARTESIAN_POINT ( 'NONE',  ( -0.05905511811023545637, 0.1660481256975885056, 0.3530559997133364547 ) ) ;
#52278 = CARTESIAN_POINT ( 'NONE',  ( 0.8595800524934390507, -0.2845877964562159024, 0.3641732283464567677 ) ) ;
#52279 = CARTESIAN_POINT ( 'NONE',  ( -1.253280839895012377, -0.3162353388693409650, -0.4822834645669289433 ) ) ;
#52280 = CARTESIAN_POINT ( 'NONE',  ( 4.893765752498283308E-17, -0.3996062992125985480, -1.100393700787401619 ) ) ;
#52281 = CARTESIAN_POINT ( 'NONE',  ( 1.056430446194226658, 0.2952755905511811885, 0.1292274648535926551 ) ) ;
#52282 = CARTESIAN_POINT ( 'NONE',  ( 0.1958661417322834775, 0.3392501089628018884, -0.7664041994750655507 ) ) ;
#52284 = DIRECTION ( 'NONE',  ( 0.000000000000000000, -1.460819769243627131E-15, -1.000000000000000000 ) ) ;
#52283 = CARTESIAN_POINT ( 'NONE',  ( 0.5511811023622055217, -0.1870078740157479769, 0.4822834645669291653 ) ) ;
#52285 = DIRECTION ( 'NONE',  ( 0.000000000000000000, 0.000000000000000000, 1.000000000000000000 ) ) ;
#52286 = CARTESIAN_POINT ( 'NONE',  ( 0.6496062992125991586, 0.07958543189024085140, 0.2665933059059887866 ) ) ;
#52287 = B_SPLINE_CURVE_WITH_KNOTS ( 'NONE', 3,
 ( #54504, #74303, #67162, #55743 ),
 .UNSPECIFIED., .F., .F.,
 ( 4, 4 ),
 ( 3.210432057682506253E-07, 0.001287787053612018777 ),
 .UNSPECIFIED. ) ;
#52288 = CARTESIAN_POINT ( 'NONE',  ( 0.6692913385826778638, -0.6692913385826771977, 8.415575281601705876E-17 ) ) ;
#52289 = CARTESIAN_POINT ( 'NONE',  ( 1.653543307086614789, -0.1870078740157479769, 0.3641732283464567677 ) ) ;
#52290 = CARTESIAN_POINT ( 'NONE',  ( -0.8989501312335946848, 0.1771653543307087075, -0.09757992244046823083 ) ) ;
#52291 = CARTESIAN_POINT ( 'NONE',  ( -0.8267716535433065062, -0.6692913385826771977, 8.415575281601705876E-17 ) ) ;
#52292 = CARTESIAN_POINT ( 'NONE',  ( -1.437007874015747477, -0.5400638737290844871, 0.3530559997133364547 ) ) ;
#52293 = CARTESIAN_POINT ( 'NONE',  ( 0.7808398950131241190, -0.05778040916215560624, -0.4822834645669293319 ) ) ;
#52294 = CARTESIAN_POINT ( 'NONE',  ( -1.555118110236219930, -0.4536011799217368745, -0.2665933059059886201 ) ) ;
#52295 = CARTESIAN_POINT ( 'NONE',  ( 1.018615313942585976, 1.475001671837482542, -0.4705483627597061846 ) ) ;
#52296 = CARTESIAN_POINT ( 'NONE',  ( 1.023622047244095112, -0.1870078740157480879, -0.4822834645669291653 ) ) ;
#52297 = CARTESIAN_POINT ( 'NONE',  ( 4.893765752498283308E-17, -0.3996062992125985480, 0.1594488188976377896 ) ) ;
#52298 = CARTESIAN_POINT ( 'NONE',  ( 0.2098209183887521645, 1.111631239983235098, 3.931436657694179715 ) ) ;
#52299 = CARTESIAN_POINT ( 'NONE',  ( 1.489501312335958172, -0.3162353388693405765, 0.4822834645669290543 ) ) ;
#52300 = CARTESIAN_POINT ( 'NONE',  ( -1.377952755905511140, 0.1771653543307087630, 0.000000000000000000 ) ) ;
#52301 = CARTESIAN_POINT ( 'NONE',  ( 1.043307086614173818, 0.07958543189024085140, 0.2665933059059887866 ) ) ;
#52302 = CARTESIAN_POINT ( 'NONE',  ( -1.102362204724408601, -0.1870078740157480601, -0.3641732283464567677 ) ) ;
#52303 = CARTESIAN_POINT ( 'NONE',  ( -0.6036745406824141069, -0.5023911411419708095, -0.1820866141732282451 ) ) ;
#52304 = LINE ( 'NONE', #52721, #78938 ) ;
#52305 = CARTESIAN_POINT ( 'NONE',  ( 0.7414698162729663755, -0.5511811023622048555, -0.09757992244046775898 ) ) ;
#52306 = CARTESIAN_POINT ( 'NONE',  ( 0.4921259842519691285, -0.5400638737290845981, -0.3530559997133363437 ) ) ;
#52307 = CARTESIAN_POINT ( 'NONE',  ( 1.194225721784777594, -0.4281496062992127816, -0.4176697321401328100 ) ) ;
#52308 = CARTESIAN_POINT ( 'NONE',  ( -0.09842519685039295696, -0.5400638737290844871, 0.3530559997133364547 ) ) ;
#52309 = CARTESIAN_POINT ( 'NONE',  ( 0.7217847769028878924, -0.3690944881889765550, -0.3153832671262227771 ) ) ;
#52310 = CARTESIAN_POINT ( 'NONE',  ( 1.233595800524935227, -0.6046776061558807314, 0.2411417322834647770 ) ) ;
#52311 = FACE_OUTER_BOUND ( 'NONE', #67587, .T. ) ;
#52312 = CARTESIAN_POINT ( 'NONE',  ( -0.3608923884514428360, -0.6692913385826773087, -0.1292274648535924053 ) ) ;
#52313 = CARTESIAN_POINT ( 'NONE',  ( -0.1070741851644051862, -0.3996062992125986590, -0.5446194225721784354 ) ) ;
#52314 = CARTESIAN_POINT ( 'NONE',  ( 0.4724409448818897017, 0.1265901696524990294, -1.146325459317585116 ) ) ;
#52315 = CARTESIAN_POINT ( 'NONE',  ( 0.07217847769028949700, -0.05778040916215560624, -0.4822834645669293319 ) ) ;
#52316 = CARTESIAN_POINT ( 'NONE',  ( -0.2952755905511803003, -0.5400638737290845981, -0.3530559997133363437 ) ) ;
#52318 = AXIS2_PLACEMENT_3D ( 'NONE', #24130, #49799, #8115 ) ;
#52317 = CARTESIAN_POINT ( 'NONE',  ( -0.1443569553805768291, 0.05413385826771666132, 0.4176697321401328100 ) ) ;
#52319 = CARTESIAN_POINT ( 'NONE',  ( -0.3996062992125986035, -0.1070741851644056997, -2.565616797900262647 ) ) ;
#52320 = CARTESIAN_POINT ( 'NONE',  ( 0.3949938075777411073, -0.1058382717557499464, -2.001312335958005395 ) ) ;
#52321 = CARTESIAN_POINT ( 'NONE',  ( -0.2867679344610364334, -0.2867679344610367109, -0.6811023622047243098 ) ) ;
#52322 = DIRECTION ( 'NONE',  ( -0.000000000000000000, -1.000000000000000000, -0.000000000000000000 ) ) ;
#52323 = CARTESIAN_POINT ( 'NONE',  ( 0.2867679344610366554, 0.2867679344610366554, -1.074803149606299080 ) ) ;
#52324 = CARTESIAN_POINT ( 'NONE',  ( -1.089238845144356427, -0.004921259842519576551, 0.3153832671262227771 ) ) ;
#52325 = CARTESIAN_POINT ( 'NONE',  ( -0.3392501089628019995, 0.1958661417322832277, -0.9632545931758529356 ) ) ;
#52326 = CARTESIAN_POINT ( 'NONE',  ( -1.036745406824146176, 0.05413385826771626580, -0.4176697321401330321 ) ) ;
#52327 = CARTESIAN_POINT ( 'NONE',  ( -0.3949938075777409963, -7.255918531996591613E-17, -2.793307086614173151 ) ) ;
#52328 = CARTESIAN_POINT ( 'NONE',  ( 0.2296587926509192634, -0.3162353388693405765, 0.4822834645669290543 ) ) ;
#52329 = CARTESIAN_POINT ( 'NONE',  ( -0.5380577427821514602, -0.3690944881889765550, -0.3153832671262227771 ) ) ;
#52330 = CARTESIAN_POINT ( 'NONE',  ( 1.135170603674541256, 0.2952755905511811885, 0.1292274648535926551 ) ) ;
#52331 = CARTESIAN_POINT ( 'NONE',  ( 0.4133858267716541968, -0.5400638737290845981, -0.3530559997133363437 ) ) ;
#52332 = CARTESIAN_POINT ( 'NONE',  ( 0.3568790343112974717, 1.224452473450301060, 1.063829662821178745 ) ) ;
#52333 = CARTESIAN_POINT ( 'NONE',  ( -0.3460692066303960868, 0.1998031496062990242, -2.388451443569553856 ) ) ;
#52334 = CARTESIAN_POINT ( 'NONE',  ( 0.2867679344610366554, 0.2867679344610366554, -1.236895956201786717 ) ) ;
#52335 = CARTESIAN_POINT ( 'NONE',  ( 1.299212598425197429, -0.6692913385826771977, 8.415575281601705876E-17 ) ) ;
#52336 = CARTESIAN_POINT ( 'NONE',  ( 0.6364829396325465405, -0.05778040916215522460, 0.4822834645669289988 ) ) ;
#52337 = CARTESIAN_POINT ( 'NONE',  ( 0.2427821522309716595, -0.3162353388693409650, -0.4822834645669289433 ) ) ;
#52338 = CARTESIAN_POINT ( 'NONE',  ( 1.312335958005249825, 0.2306618581243847221, -0.2411417322834647770 ) ) ;
#52339 = CARTESIAN_POINT ( 'NONE',  ( 0.9448818897637802916, -0.1870078740157480879, -0.4822834645669291653 ) ) ;
#52340 = CARTESIAN_POINT ( 'NONE',  ( 0.1958661417322836440, -0.3392501089628017219, -0.4914698162729659869 ) ) ;
#52341 = CARTESIAN_POINT ( 'NONE',  ( -0.1049868766404193215, 0.2306618581243847221, -0.2411417322834647770 ) ) ;
#52342 = CARTESIAN_POINT ( 'NONE',  ( 0.9120734908136490793, 0.2952755905511810774, -0.1292274648535930714 ) ) ;
#52343 = CARTESIAN_POINT ( 'NONE',  ( 0.3937007874015754361, -0.1870078740157479769, 0.4822834645669291653 ) ) ;
#52344 = CARTESIAN_POINT ( 'NONE',  ( 0.9580052493438327987, -0.3690944881889765550, -0.3153832671262227771 ) ) ;
#52345 = CARTESIAN_POINT ( 'NONE',  ( -0.8398950131233589023, -0.6046776061558809534, -0.2411417322834644161 ) ) ;
#52346 = CARTESIAN_POINT ( 'NONE',  ( -1.332020997375327642, -0.3162353388693409650, -0.4822834645669289433 ) ) ;
#52347 = CARTESIAN_POINT ( 'NONE',  ( 0.6692913385826777528, 0.2952755905511811885, 0.000000000000000000 ) ) ;
#52348 = CARTESIAN_POINT ( 'NONE',  ( -0.1002886991216605655, -0.3788256970794443568, -1.929133858267718882 ) ) ;
#52349 = CARTESIAN_POINT ( 'NONE',  ( -0.3917322834645669549, -0.1049643490035306603, -2.085301837270341352 ) ) ;
#52350 = ORIENTED_EDGE ( 'NONE', *, *, #45382, .F. ) ;
#52351 = CARTESIAN_POINT ( 'NONE',  ( -0.2925321140481932924, 0.2925321140481931814, -0.1771653543307087075 ) ) ;
#52352 = ORIENTED_EDGE ( 'NONE', *, *, #67169, .F. ) ;
#52353 = CARTESIAN_POINT ( 'NONE',  ( 1.581364829396326277, -0.3162353388693409650, -0.4822834645669289433 ) ) ;
#52354 = CARTESIAN_POINT ( 'NONE',  ( 0.9776902887139113929, 0.1771653543307087630, 0.09757992244046791164 ) ) ;
#52355 = CARTESIAN_POINT ( 'NONE',  ( -0.6575345472709128725, 1.929133858267715773, -0.5309055118110235227 ) ) ;
#52356 = CARTESIAN_POINT ( 'NONE',  ( -0.06850640440391347896, 1.067651707476379830, 2.869699202025107532 ) ) ;
#52357 = CARTESIAN_POINT ( 'NONE',  ( -0.4744094488188880798, 1.537401574803149984, -2.554262525012305218 ) ) ;
#52358 = CARTESIAN_POINT ( 'NONE',  ( -0.3917322834645669549, -0.1049643490035306603, -0.7604986876640419391 ) ) ;
#52359 = ADVANCED_FACE ( 'NONE', ( #15712 ), #23366, .T. ) ;
#52360 = CARTESIAN_POINT ( 'NONE',  ( -1.010498687664041384, -0.004921259842519576551, 0.3153832671262227771 ) ) ;
#52361 = CARTESIAN_POINT ( 'NONE',  ( -1.620734908136482577, -0.5511811023622048555, -0.09757992244046775898 ) ) ;
#52362 = CARTESIAN_POINT ( 'NONE',  ( -0.3917864676224234177, -0.04037479286093467734, -1.929133858266767865 ) ) ;
#52363 = CARTESIAN_POINT ( 'NONE',  ( -0.4461942257217840213, 0.2306618581243848609, 0.2411417322834645549 ) ) ;
#52364 = CARTESIAN_POINT ( 'NONE',  ( 1.207349081364829990, -0.6046776061558809534, -0.2411417322834644161 ) ) ;
#52365 = ORIENTED_EDGE ( 'NONE', *, *, #3407, .F. ) ;
#52366 = CARTESIAN_POINT ( 'NONE',  ( -1.574803149606298636, -0.1870078740157479769, 0.4822834645669291653 ) ) ;
#52367 = FACE_OUTER_BOUND ( 'NONE', #17375, .T. ) ;
#52368 = CARTESIAN_POINT ( 'NONE',  ( 1.614173228346456712, 1.267785121476991517, 0.1372047244094478646 ) ) ;
#52369 = CARTESIAN_POINT ( 'NONE',  ( -0.8661417322834640276, -0.1870078740157479769, 0.3641732283464567677 ) ) ;
#52370 = CARTESIAN_POINT ( 'NONE',  ( 1.614173228346456712, 0.9921945702958890889, 0.1372047244094478646 ) ) ;
#52371 = CARTESIAN_POINT ( 'NONE',  ( 0.5380577427821529035, -0.4281496062992124485, 0.4176697321401328655 ) ) ;
#52372 = ORIENTED_EDGE ( 'NONE', *, *, #52141, .F. ) ;
#52374 = CARTESIAN_POINT ( 'NONE',  ( 4.218763579739897660E-16, 0.000000000000000000, 3.444881889763779625 ) ) ;
#52373 = FACE_OUTER_BOUND ( 'NONE', #47707, .T. ) ;
#52375 = CARTESIAN_POINT ( 'NONE',  ( 1.351706036745407680, 0.05413385826771666132, 0.4176697321401328100 ) ) ;
#52376 = CARTESIAN_POINT ( 'NONE',  ( -1.686351706036744558, 0.2952755905511810774, -0.1292274648535930714 ) ) ;
#52377 = CARTESIAN_POINT ( 'NONE',  ( -0.3917322834645668994, -0.1049643490035306742, -0.7558861960291846094 ) ) ;
#52378 = CARTESIAN_POINT ( 'NONE',  ( -1.003937007874015297, -0.4536011799217368745, -0.2665933059059886201 ) ) ;
#52379 = CARTESIAN_POINT ( 'NONE',  ( -1.404199475065615932, -0.3690944881889765550, -0.3153832671262227771 ) ) ;
#52380 = CARTESIAN_POINT ( 'NONE',  ( -0.4724409448818899238, 0.1265901696524986964, -0.8202099737532806412 ) ) ;
#52381 = CARTESIAN_POINT ( 'NONE',  ( 0.2887139107611556010, -0.6046776061558807314, 0.2411417322834647770 ) ) ;
#52382 = CARTESIAN_POINT ( 'NONE',  ( -1.115485564304461219, -0.004921259842519870586, -0.3153832671262229437 ) ) ;
#52383 = CARTESIAN_POINT ( 'NONE',  ( -0.02624671916010428221, -0.5023911411419708095, 0.1820866141732285504 ) ) ;
#52384 = CARTESIAN_POINT ( 'NONE',  ( -0.4855643044619415427, -0.4281496062992124485, 0.4176697321401328655 ) ) ;
#52385 = CARTESIAN_POINT ( 'NONE',  ( -1.082677165354329896, -0.4536011799217368745, -0.2665933059059886201 ) ) ;
#52386 = CARTESIAN_POINT ( 'NONE',  ( -0.2867679344610367109, 0.2867679344610365444, -0.1739038302175346939 ) ) ;
#52387 = CARTESIAN_POINT ( 'NONE',  ( 0.7742782152230978099, -0.4281496062992124485, 0.4176697321401328655 ) ) ;
#52388 = CARTESIAN_POINT ( 'NONE',  ( -1.351706036745406347, -0.4281496062992124485, 0.4176697321401328655 ) ) ;
#52389 = CARTESIAN_POINT ( 'NONE',  ( -0.1265901696524993347, 0.4724409448818895907, -1.343175853018372834 ) ) ;
#52390 = CARTESIAN_POINT ( 'NONE',  ( -0.6036745406824141069, 0.2306618581243848609, 0.2411417322834645549 ) ) ;
#52391 = CARTESIAN_POINT ( 'NONE',  ( -0.1115485564304456306, 0.1771653543307087075, -0.09757992244046823083 ) ) ;
#52392 = CARTESIAN_POINT ( 'NONE',  ( -1.240157480314959759, -0.5400638737290845981, -0.3530559997133363437 ) ) ;
#52393 = CARTESIAN_POINT ( 'NONE',  ( 0.8398950131233602345, -0.5023911411419708095, 0.1820866141732285504 ) ) ;
#52394 = CARTESIAN_POINT ( 'NONE',  ( -0.2821522309711278487, 0.1771653543307087630, 0.09757992244046791164 ) ) ;
#52395 = CARTESIAN_POINT ( 'NONE',  ( -0.6955380577427815458, -0.4281496062992127816, -0.4176697321401328100 ) ) ;
#52396 = CARTESIAN_POINT ( 'NONE',  ( -1.056430446194224881, 0.2952755905511810774, -0.1292274648535930714 ) ) ;
#52397 = CARTESIAN_POINT ( 'NONE',  ( -1.607611548556429737, 0.2952755905511810774, -0.1292274648535930714 ) ) ;
#52398 = CARTESIAN_POINT ( 'NONE',  ( 0.3458507752293908943, 0.3458507752293908943, -2.104330708661417138 ) ) ;
#52399 = CARTESIAN_POINT ( 'NONE',  ( 1.358267716535433323, 0.07958543189024085140, 0.2665933059059887866 ) ) ;
#52400 = CARTESIAN_POINT ( 'NONE',  ( 0.2362204724409456558, -0.1870078740157479769, 0.4822834645669291653 ) ) ;
#52401 = CARTESIAN_POINT ( 'NONE',  ( -1.377952755905511140, -0.6692913385826771977, 8.415575281601705876E-17 ) ) ;
#52402 = CARTESIAN_POINT ( 'NONE',  ( -1.686351706036744558, 0.2952755905511810774, -0.1292274648535930714 ) ) ;
#52403 = EDGE_LOOP ( 'NONE', ( #27729, #45390, #41091, #44947 ) ) ;
#52404 = CARTESIAN_POINT ( 'NONE',  ( 0.1070741851644053388, 0.3996062992125986035, -2.589895013123359568 ) ) ;
#52405 = CARTESIAN_POINT ( 'NONE',  ( -1.076115485564303809, -0.5023911411419708095, -0.1820866141732282451 ) ) ;
#52406 = CARTESIAN_POINT ( 'NONE',  ( 0.7939632545931766261, -0.05778040916215522460, 0.4822834645669289988 ) ) ;
#52407 = CARTESIAN_POINT ( 'NONE',  ( -1.233595800524933894, 0.1283753931104748280, 0.1820866141732283561 ) ) ;
#52408 = CARTESIAN_POINT ( 'NONE',  ( -9.787531504996566615E-17, 0.3996062992125985480, -1.809055118110236560 ) ) ;
#52409 = CARTESIAN_POINT ( 'NONE',  ( -1.220472440944881054, 0.2952755905511811885, 0.000000000000000000 ) ) ;
#52410 = CARTESIAN_POINT ( 'NONE',  ( 0.8464566929133866546, -0.5400638737290844871, 0.3530559997133364547 ) ) ;
#52411 = CARTESIAN_POINT ( 'NONE',  ( 0.4658792650918641698, -0.05778040916215560624, -0.4822834645669293319 ) ) ;
#52412 = CARTESIAN_POINT ( 'NONE',  ( 1.187664041994751285, -0.3162353388693409650, -0.4822834645669289433 ) ) ;
#52413 = CARTESIAN_POINT ( 'NONE',  ( -1.607611548556429737, -0.5511811023622046335, 0.09757992244046803654 ) ) ;
#52414 = CARTESIAN_POINT ( 'NONE',  ( 0.1070741851644054637, -0.3996062992125984925, -1.106955380577427706 ) ) ;
#52415 = CARTESIAN_POINT ( 'NONE',  ( -0.2925321140481930704, -0.2925321140481933480, -1.161417322834645383 ) ) ;
#52416 = CARTESIAN_POINT ( 'NONE',  ( 0.1058382717557499880, 0.3949938075777411073, -0.7808398950131234528 ) ) ;
#52417 = LINE ( 'NONE', #13314, #69482 ) ;
#52418 = CARTESIAN_POINT ( 'NONE',  ( 0.9514435695538062676, -0.2845877964562161244, -0.3641732283464567121 ) ) ;
#52419 = CARTESIAN_POINT ( 'NONE',  ( 0.1509186351706042484, -0.2845877964562159024, 0.3641732283464567677 ) ) ;
#52420 = CARTESIAN_POINT ( 'NONE',  ( 0.1181102362204730916, -0.6692913385826771977, 8.415575281601705876E-17 ) ) ;
#52421 = CARTESIAN_POINT ( 'NONE',  ( 1.128608923884514947, 0.2306618581243848609, 0.2411417322834645549 ) ) ;
#52422 = CARTESIAN_POINT ( 'NONE',  ( -0.1058382717557503072, 0.3949938075777408852, -1.658136482939632339 ) ) ;
#52423 = CARTESIAN_POINT ( 'NONE',  ( 0.2099737532808405305, -0.5023911411419708095, 0.1820866141732285504 ) ) ;
#52424 = CARTESIAN_POINT ( 'NONE',  ( -0.5839895013123351797, -0.6692913385826771977, 0.1292274648535927661 ) ) ;
#52425 = CARTESIAN_POINT ( 'NONE',  ( -1.476377952755905110, 0.1660481256975885056, 0.3530559997133364547 ) ) ;
#52426 = CARTESIAN_POINT ( 'NONE',  ( 0.7808398950131241190, -0.05778040916215560624, -0.4822834645669293319 ) ) ;
#52427 = CARTESIAN_POINT ( 'NONE',  ( 0.1265901696524989462, 0.4724409448818897572, -2.040682414698162361 ) ) ;
#52428 = DIRECTION ( 'NONE',  ( 0.000000000000000000, 1.000000000000000000, 0.000000000000000000 ) ) ;
#52429 = ORIENTED_EDGE ( 'NONE', *, *, #64406, .F. ) ;
#52430 = ORIENTED_EDGE ( 'NONE', *, *, #41383, .F. ) ;
#52431 = CARTESIAN_POINT ( 'NONE',  ( -1.240157480314959759, 0.1660481256975885056, 0.3530559997133364547 ) ) ;
#52432 = CIRCLE ( 'NONE', #49927, 0.5118110236220472231 ) ;
#52434 = CARTESIAN_POINT ( 'NONE',  ( -1.240157480314959759, -0.5400638737290845981, -0.3530559997133363437 ) ) ;
#52433 = CARTESIAN_POINT ( 'NONE',  ( -0.8858267716535425107, -0.4536011799217367080, 0.2665933059059888421 ) ) ;
#52435 = CARTESIAN_POINT ( 'NONE',  ( 0.1958661417322836162, -0.3392501089628018329, -2.376621104165667298 ) ) ;
#52436 = CARTESIAN_POINT ( 'NONE',  ( 0.1998031496062992463, 0.3460692066303959202, -2.740813648293963567 ) ) ;
#52437 = CARTESIAN_POINT ( 'NONE',  ( 1.620734908136483465, -0.6692913385826771977, 0.1292274648535927661 ) ) ;
#52438 = CARTESIAN_POINT ( 'NONE',  ( -1.286089238845143479, -0.6046776061558807314, 0.2411417322834647770 ) ) ;
#52439 = CARTESIAN_POINT ( 'NONE',  ( 0.2887139107611556010, -0.6046776061558807314, 0.2411417322834647770 ) ) ;
#52440 = CARTESIAN_POINT ( 'NONE',  ( -1.122047244094487306, 0.1660481256975883668, -0.3530559997133364547 ) ) ;
#52441 = CARTESIAN_POINT ( 'NONE',  ( -0.3917322834645669549, -7.196005306013483243E-17, -2.639088295766717884 ) ) ;
#52442 = EDGE_CURVE ( 'NONE', #74617, #24203, #32801, .T. ) ;
#52443 = CARTESIAN_POINT ( 'NONE',  ( 0.4790026246719167324, -0.05778040916215522460, 0.4822834645669289988 ) ) ;
#52444 = CARTESIAN_POINT ( 'NONE',  ( -0.3917322834645670104, -7.196005306013484475E-17, -2.078740157480314821 ) ) ;
#52445 = CARTESIAN_POINT ( 'NONE',  ( -0.7414698162729651543, -0.5511811023622046335, 0.09757992244046803654 ) ) ;
#52446 = ORIENTED_EDGE ( 'NONE', *, *, #25189, .T. ) ;
#52447 = CARTESIAN_POINT ( 'NONE',  ( 0.1974969037888706369, -0.3420746716998659953, -1.981627296587926690 ) ) ;
#52448 = VERTEX_POINT ( 'NONE', #9383 ) ;
#52449 = CARTESIAN_POINT ( 'NONE',  ( -0.6418543022643059537, 1.311896022878452671E-15, -0.3627985898453513491 ) ) ;
#52450 = CARTESIAN_POINT ( 'NONE',  ( -1.312335958005248715, -0.6046776061558809534, -0.2411417322834644161 ) ) ;
#52451 = CARTESIAN_POINT ( 'NONE',  ( -1.161417322834644716, 0.1660481256975885056, 0.3530559997133364547 ) ) ;
#52452 = CARTESIAN_POINT ( 'NONE',  ( 0.1070741851644054915, -0.3996062992125986035, -0.4002624671916010235 ) ) ;
#52453 = CARTESIAN_POINT ( 'NONE',  ( -1.574803149606298636, -0.1870078740157479769, 0.4822834645669291653 ) ) ;
#52454 = CARTESIAN_POINT ( 'NONE',  ( -1.266404199475064773, -0.3162353388693405765, 0.4822834645669290543 ) ) ;
#52455 = CARTESIAN_POINT ( 'NONE',  ( -1.253280839895012377, -0.3162353388693409650, -0.4822834645669289433 ) ) ;
#52457 = CARTESIAN_POINT ( 'NONE',  ( 0.1938976377952755792, 0.1938976377952755792, 0.07874015748031495954 ) ) ;
#52456 = B_SPLINE_CURVE_WITH_KNOTS ( 'NONE', 3,
 ( #39929, #65618, #73585, #59687, #3698, #35268, #48298, #9189 ),
 .UNSPECIFIED., .F., .F.,
 ( 4, 2, 2, 4 ),
 ( 0.000000000000000000, 0.002428728328773748467, 0.003643092493160610991, 0.004857456657547474382 ),
 .UNSPECIFIED. ) ;
#52458 = CYLINDRICAL_SURFACE ( 'NONE', #75188, 0.2165354330708661457 ) ;
#52459 = ADVANCED_FACE ( 'NONE', ( #35053, #63195 ), #11453, .F. ) ;
#52460 = CARTESIAN_POINT ( 'NONE',  ( 0.01968503937007957949, -0.4536011799217368745, -0.2665933059059886201 ) ) ;
#52461 = CARTESIAN_POINT ( 'NONE',  ( 0.5419760673063064305, 1.535433070866141447, -0.4915354330708657793 ) ) ;
#52462 = CARTESIAN_POINT ( 'NONE',  ( -9.594673741351313045E-17, 0.3917322834645670104, -0.5570866141732284671 ) ) ;
#52463 = CARTESIAN_POINT ( 'NONE',  ( -0.3346456692913377662, -0.4536011799217367080, 0.2665933059059888421 ) ) ;
#52464 = CARTESIAN_POINT ( 'NONE',  ( -0.9908136482939626788, 0.2952755905511811885, 0.1292274648535926551 ) ) ;
#52465 = CARTESIAN_POINT ( 'NONE',  ( 0.8136482939632553313, 0.2306618581243848609, 0.2411417322834645549 ) ) ;
#52466 = CARTESIAN_POINT ( 'NONE',  ( -0.6627296587926501115, 0.2952755905511810774, -0.1292274648535930714 ) ) ;
#52467 = VERTEX_POINT ( 'NONE', #64022 ) ;
#52468 = ORIENTED_EDGE ( 'NONE', *, *, #37540, .T. ) ;
#52469 = CARTESIAN_POINT ( 'NONE',  ( -0.2925321140481930149, -0.2925321140481933480, -1.868110236220472453 ) ) ;
#52470 = CARTESIAN_POINT ( 'NONE',  ( -0.9448818897637790704, -0.1870078740157480879, -0.4822834645669291653 ) ) ;
#52471 = CARTESIAN_POINT ( 'NONE',  ( 1.036745406824147508, -0.4281496062992127816, -0.4176697321401328100 ) ) ;
#52472 = CARTESIAN_POINT ( 'NONE',  ( 0.000000000000000000, 0.000000000000000000, 0.000000000000000000 ) ) ;
#52473 = CARTESIAN_POINT ( 'NONE',  ( -1.725721784776902190, -0.05778040916215522460, 0.4822834645669289988 ) ) ;
#52474 = CARTESIAN_POINT ( 'NONE',  ( 0.3458507752293908943, 0.3458507752293908943, -1.082677165354330562 ) ) ;
#52475 = CARTESIAN_POINT ( 'NONE',  ( 1.392101432702376629, 0.1377952755905511861, 0.9507481457704560768 ) ) ;
#52476 = CARTESIAN_POINT ( 'NONE',  ( 0.1049643490035304938, -0.3917322834645669549, -0.2349081364829396223 ) ) ;
#52477 = CARTESIAN_POINT ( 'NONE',  ( -0.3917322834645671215, 0.1049643490035301469, -2.637139107611548461 ) ) ;
#52478 = CARTESIAN_POINT ( 'NONE',  ( -0.4658792650918627265, -0.3162353388693409650, -0.4822834645669289433 ) ) ;
#52479 = CARTESIAN_POINT ( 'NONE',  ( -1.364829396325458521, -0.5023911411419708095, 0.1820866141732285504 ) ) ;
#52480 = CARTESIAN_POINT ( 'NONE',  ( -0.8792650918635160906, 0.05413385826771626580, -0.4176697321401330321 ) ) ;
#52481 = CARTESIAN_POINT ( 'NONE',  ( 0.1070741851644053388, 0.3996062992125986035, -0.2276902887139107545 ) ) ;
#52483 = LINE ( 'NONE', #1585, #6206 ) ;
#52482 = CARTESIAN_POINT ( 'NONE',  ( -1.351706036745406347, 0.05413385826771626580, -0.4176697321401330321 ) ) ;
#52484 = CARTESIAN_POINT ( 'NONE',  ( -0.8070866141732276899, -0.5400638737290844871, 0.3530559997133364547 ) ) ;
#52485 = CARTESIAN_POINT ( 'NONE',  ( -0.2230971128608915943, -0.4281496062992127816, -0.4176697321401328100 ) ) ;
#52486 = CARTESIAN_POINT ( 'NONE',  ( 0.3949938075777409963, 2.418639510665530743E-17, -2.557086614173228689 ) ) ;
#52487 = CARTESIAN_POINT ( 'NONE',  ( 0.7808398950131240079, -0.2845877964562159024, 0.3641732283464567677 ) ) ;
#52488 = DIRECTION ( 'NONE',  ( 0.000000000000000000, 0.000000000000000000, 1.000000000000000000 ) ) ;
#52489 = CARTESIAN_POINT ( 'NONE',  ( 0.2952755905511819101, 0.07958543189024071263, -0.2665933059059888421 ) ) ;
#52490 = CARTESIAN_POINT ( 'NONE',  ( 1.423884514435696191, -0.08942795157527998196, 0.3641732283464567121 ) ) ;
#52491 = CARTESIAN_POINT ( 'NONE',  ( 1.528871391076116026, -0.6692913385826773087, -0.1292274648535924053 ) ) ;
#52492 = CARTESIAN_POINT ( 'NONE',  ( 8.195543980992789655E-16, -0.1870078740157480601, -0.3641732283464567677 ) ) ;
#52493 = CARTESIAN_POINT ( 'NONE',  ( 4.797336870675656522E-17, -0.3917322834645670104, -1.803149606299212726 ) ) ;
#52494 = CARTESIAN_POINT ( 'NONE',  ( -1.417322834645668772, -0.1870078740157480879, -0.4822834645669291653 ) ) ;
#52495 = CARTESIAN_POINT ( 'NONE',  ( 1.233595800524935227, -0.6046776061558807314, 0.2411417322834647770 ) ) ;
#52496 = CARTESIAN_POINT ( 'NONE',  ( 0.4091458600556404646, -0.2362204724409448231, -0.02427821522309711946 ) ) ;
#52497 = CARTESIAN_POINT ( 'NONE',  ( -0.4002624671916004129, -0.2845877964562159024, 0.3641732283464567677 ) ) ;
#52498 = PLANE ( 'NONE',  #17121 ) ;
#52499 = CARTESIAN_POINT ( 'NONE',  ( 0.2624671916010504757, 0.2306618581243848609, 0.2411417322834645549 ) ) ;
#52500 = CARTESIAN_POINT ( 'NONE',  ( -1.019868997598491145, 1.617710314158373519, -0.4678352644680017214 ) ) ;
#52501 = CARTESIAN_POINT ( 'NONE',  ( 0.9186351706036751663, -0.5023911411419708095, 0.1820866141732285504 ) ) ;
#52502 = CARTESIAN_POINT ( 'NONE',  ( 0.1968503937007881344, 0.1771653543307087630, 0.000000000000000000 ) ) ;
#52503 = CARTESIAN_POINT ( 'NONE',  ( -0.4724409448818890911, -0.1870078740157480879, -0.4822834645669291653 ) ) ;
#52504 = CARTESIAN_POINT ( 'NONE',  ( -1.620734908136482577, -0.6692913385826773087, -0.1292274648535924053 ) ) ;
#52505 = CARTESIAN_POINT ( 'NONE',  ( -0.7742782152230962556, -0.3690944881889765550, -0.3153832671262227771 ) ) ;
#52506 = CARTESIAN_POINT ( 'NONE',  ( 0.000000000000000000, 2.755905511811024056, 0.000000000000000000 ) ) ;
#52507 = CARTESIAN_POINT ( 'NONE',  ( 0.4986876640419954376, -0.6046776061558809534, -0.2411417322834644161 ) ) ;
#52508 = VECTOR ( 'NONE', #4135, 39.37007874015748143 ) ;
#52509 = CARTESIAN_POINT ( 'NONE',  ( -0.9317585301837263412, -0.4281496062992127816, -0.4176697321401328100 ) ) ;
#52510 = CARTESIAN_POINT ( 'NONE',  ( 0.3460692066303958092, 0.1998031496062993018, -1.152887139107611425 ) ) ;
#52511 = CARTESIAN_POINT ( 'NONE',  ( -0.1958661417322836718, 0.3392501089628017219, -2.617454068241469756 ) ) ;
#52512 = CARTESIAN_POINT ( 'NONE',  ( 0.3083989501312343062, -0.2845877964562159024, 0.3641732283464567677 ) ) ;
#52513 = CARTESIAN_POINT ( 'NONE',  ( -0.7611548556430438595, -0.6046776061558809534, -0.2411417322834644161 ) ) ;
#52514 = CARTESIAN_POINT ( 'NONE',  ( -0.9973753280839886548, 0.2306618581243848609, 0.2411417322834645549 ) ) ;
#52515 = CARTESIAN_POINT ( 'NONE',  ( -1.338582677165353729, -0.1870078740157479769, 0.3641732283464567677 ) ) ;
#52516 = CARTESIAN_POINT ( 'NONE',  ( 1.220472440944881942, 0.000000000000000000, -0.5309055118110238558 ) ) ;
#52517 = CARTESIAN_POINT ( 'NONE',  ( -0.9383202099737524282, -0.2845877964562161244, -0.3641732283464567121 ) ) ;
#52518 = CARTESIAN_POINT ( 'NONE',  ( -1.604771003085129655, 1.871396828306225002, 0.1466069496707748665 ) ) ;
#52519 = CARTESIAN_POINT ( 'NONE',  ( 1.482939632545932307, 0.05413385826771626580, -0.4176697321401330321 ) ) ;
#52520 = CARTESIAN_POINT ( 'NONE',  ( -0.2925321140481932924, 0.2925321140481931814, -0.01968503937007875029 ) ) ;
#52521 = CARTESIAN_POINT ( 'NONE',  ( -0.3917322834645671770, 0.1049643490035302024, -2.391751599246406457 ) ) ;
#52522 = ADVANCED_FACE ( 'NONE', ( #49734 ), #5128, .T. ) ;
#52523 = ORIENTED_EDGE ( 'NONE', *, *, #78534, .F. ) ;
#52524 = VECTOR ( 'NONE', #14267, 39.37007874015748143 ) ;
#52525 = CARTESIAN_POINT ( 'NONE',  ( 0.4724922890202770676, 1.580837543196284223, -2.558946168779563823 ) ) ;
#52526 = CARTESIAN_POINT ( 'NONE',  ( 1.469816272965879911, 0.1283753931104746893, -0.1820866141732285504 ) ) ;
#52527 = CARTESIAN_POINT ( 'NONE',  ( -1.299212598425196097, -0.6692913385826771977, 8.415575281601705876E-17 ) ) ;
#52528 = CARTESIAN_POINT ( 'NONE',  ( 1.194225721784777594, -0.4281496062992127816, -0.4176697321401328100 ) ) ;
#52529 = CARTESIAN_POINT ( 'NONE',  ( -0.3917322834645671215, 0.1049643490035301469, -2.322178477690288734 ) ) ;
#52530 = CARTESIAN_POINT ( 'NONE',  ( 1.666666666666667185, -0.004921259842519576551, 0.3153832671262227771 ) ) ;
#52531 = CARTESIAN_POINT ( 'NONE',  ( 0.6102362204724416372, 0.1660481256975883668, -0.3530559997133364547 ) ) ;
#52532 = CARTESIAN_POINT ( 'NONE',  ( -0.2296587926509179312, -0.05778040916215522460, 0.4822834645669289988 ) ) ;
#52533 = CARTESIAN_POINT ( 'NONE',  ( -0.6975637601868556192, 5.991678263669262536E-15, 0.3954985857520036951 ) ) ;
#52534 = DIRECTION ( 'NONE',  ( 0.000000000000000000, 0.000000000000000000, 1.000000000000000000 ) ) ;
#52535 = CARTESIAN_POINT ( 'NONE',  ( 0.7086614173228352742, -0.1870078740157480601, -0.3641732283464567677 ) ) ;
#52536 = CARTESIAN_POINT ( 'NONE',  ( -0.1998031496062991907, -0.3460692066303959757, -1.482939632545931863 ) ) ;
#52537 = ORIENTED_EDGE ( 'NONE', *, *, #30658, .T. ) ;
#52538 = CARTESIAN_POINT ( 'NONE',  ( -0.3392501089628019995, 0.1958661417322831999, 0.1344951199136988906 ) ) ;
#52539 = ORIENTED_EDGE ( 'NONE', *, *, #73492, .F. ) ;
#52540 = CARTESIAN_POINT ( 'NONE',  ( -0.03280839895013062252, -0.6692913385826771977, 0.1292274648535927661 ) ) ;
#52541 = CARTESIAN_POINT ( 'NONE',  ( 1.443569553805774897, 0.2306618581243848609, 0.2411417322834645549 ) ) ;
#52542 = CARTESIAN_POINT ( 'NONE',  ( 0.4265091863517067594, 0.2952755905511811885, 0.1292274648535926551 ) ) ;
#52543 = CARTESIAN_POINT ( 'NONE',  ( 1.253280839895013710, -0.05778040916215560624, -0.4822834645669293319 ) ) ;
#52544 = CARTESIAN_POINT ( 'NONE',  ( -0.5577427821522301654, -0.3162353388693405765, 0.4822834645669290543 ) ) ;
#52545 = CARTESIAN_POINT ( 'NONE',  ( 0.1115485564304467270, -0.6692913385826773087, -0.1292274648535924053 ) ) ;
#52546 = CARTESIAN_POINT ( 'NONE',  ( 1.476377952755906220, 0.1660481256975883668, -0.3530559997133364547 ) ) ;
#52547 = CARTESIAN_POINT ( 'NONE',  ( 1.194225721784777594, -0.4281496062992127816, -0.4176697321401328100 ) ) ;
#52548 = CARTESIAN_POINT ( 'NONE',  ( 1.253280839895013710, -0.05778040916215560624, -0.4822834645669293319 ) ) ;
#52549 = CARTESIAN_POINT ( 'NONE',  ( -0.3392501089628019995, 0.1958661417322832277, -0.6482939632545930975 ) ) ;
#52550 = CARTESIAN_POINT ( 'NONE',  ( 0.4593175853018380828, -0.004921259842519870586, -0.3153832671262229437 ) ) ;
#52551 = ORIENTED_EDGE ( 'NONE', *, *, #43383, .T. ) ;
#52552 = CARTESIAN_POINT ( 'NONE',  ( 0.2891555358219910499, -0.2891555358219909944, -0.5708661417322835607 ) ) ;
#52553 = ORIENTED_EDGE ( 'NONE', *, *, #69619, .F. ) ;
#52554 = CARTESIAN_POINT ( 'NONE',  ( -0.5577427821522301654, -0.08942795157528024563, -0.3641732283464568787 ) ) ;
#52555 = CARTESIAN_POINT ( 'NONE',  ( -0.1968503937007867743, 0.2952755905511811885, 0.000000000000000000 ) ) ;
#52556 = CARTESIAN_POINT ( 'NONE',  ( 2.558801921129982837, 1.494646310179101878, 0.4725519687354816090 ) ) ;
#52557 = CARTESIAN_POINT ( 'NONE',  ( 0.2362204724409456558, -0.1870078740157480879, -0.4822834645669291653 ) ) ;
#52558 = CARTESIAN_POINT ( 'NONE',  ( 0.1640419947506569498, -0.05778040916215522460, 0.4822834645669289988 ) ) ;
#52559 = CARTESIAN_POINT ( 'NONE',  ( -0.6955380577427815458, 0.05413385826771666132, 0.4176697321401328100 ) ) ;
#52560 = CARTESIAN_POINT ( 'NONE',  ( -0.7939632545931754048, -0.3162353388693405765, 0.4822834645669290543 ) ) ;
#52561 = CARTESIAN_POINT ( 'NONE',  ( 1.443569553805774897, -0.5023911411419708095, -0.1820866141732282451 ) ) ;
#52562 = CARTESIAN_POINT ( 'NONE',  ( -1.437007874015747477, 0.1660481256975883668, -0.3530559997133364547 ) ) ;
#52563 = CARTESIAN_POINT ( 'NONE',  ( 0.06049490571020648549, 1.070753598490859382, 0.2444952571283235676 ) ) ;
#52564 = CARTESIAN_POINT ( 'NONE',  ( 1.017060367454068581, -0.08942795157528024563, -0.3641732283464568787 ) ) ;
#52565 = CARTESIAN_POINT ( 'NONE',  ( 0.6364829396325465405, -0.3162353388693409650, -0.4822834645669289433 ) ) ;
#52566 = CARTESIAN_POINT ( 'NONE',  ( 0.7414698162729663755, 0.2952755905511811885, 0.1292274648535926551 ) ) ;
#52567 = STYLED_ITEM ( 'NONE', ( #58361 ), #31714 ) ;
#52568 = CARTESIAN_POINT ( 'NONE',  ( 0.3996062992125986035, 0.1070741851644054776, -1.227034120734908029 ) ) ;
#52569 = CARTESIAN_POINT ( 'NONE',  ( 0.3264567959345339720, 2.726622551019859153E-15, 0.3791475997938225095 ) ) ;
#52570 = CARTESIAN_POINT ( 'NONE',  ( -0.3996062992125986590, 0.1070741851644051723, -0.8969816272965877024 ) ) ;
#52571 = CARTESIAN_POINT ( 'NONE',  ( 0.1070741851644053388, 0.3996062992125986035, 0.08727034120734902811 ) ) ;
#52572 = CARTESIAN_POINT ( 'NONE',  ( -0.4396325459317579898, 0.2952755905511811885, 0.1292274648535926551 ) ) ;
#52573 = CARTESIAN_POINT ( 'NONE',  ( -0.1070741851644056997, 0.3996062992125986035, -2.841207349081364963 ) ) ;
#52574 = CARTESIAN_POINT ( 'NONE',  ( 0.2867679344610365999, 0.2867679344610365999, -2.112204724409449064 ) ) ;
#52575 = CARTESIAN_POINT ( 'NONE',  ( -1.286089238845143479, 0.1283753931104746893, -0.1820866141732285504 ) ) ;
#52576 = CARTESIAN_POINT ( 'NONE',  ( 1.364829396325459854, -0.6046776061558809534, -0.2411417322834644161 ) ) ;
#52577 = CARTESIAN_POINT ( 'NONE',  ( 1.056430446194226658, 0.2952755905511811885, 0.1292274648535926551 ) ) ;
#52578 = CARTESIAN_POINT ( 'NONE',  ( -0.08530183727034056085, -0.2845877964562159024, 0.3641732283464567677 ) ) ;
#52579 = CARTESIAN_POINT ( 'NONE',  ( 0.6364829396325465405, -0.05778040916215522460, 0.4822834645669289988 ) ) ;
#52580 = CARTESIAN_POINT ( 'NONE',  ( 0.3458507752293908943, -0.3458507752293908943, -1.907480314960629197 ) ) ;
#52581 = CARTESIAN_POINT ( 'NONE',  ( -0.01312335958005186876, -0.004921259842519870586, -0.3153832671262229437 ) ) ;
#52582 = CARTESIAN_POINT ( 'NONE',  ( 0.01968503937007930540, 0.1660481256975885056, 0.3530559997133364547 ) ) ;
#52583 = CARTESIAN_POINT ( 'NONE',  ( -0.1974969037888704149, -0.3420746716998661063, -1.402230971128609172 ) ) ;
#52584 = CARTESIAN_POINT ( 'NONE',  ( -1.167979002624671470, -0.4281496062992127816, -0.4176697321401328100 ) ) ;
#52585 = CARTESIAN_POINT ( 'NONE',  ( 0.5380577427821529035, -0.004921259842519870586, -0.3153832671262229437 ) ) ;
#52586 = CONICAL_SURFACE ( 'NONE', #28390, 1.244489337948955221, 0.7853981633974452814 ) ;
#52587 = CARTESIAN_POINT ( 'NONE',  ( 0.3477690288713918276, 0.2066929133858267931, 0.1054918080437490802 ) ) ;
#52589 = EDGE_CURVE ( 'NONE', #14913, #39936, #69192, .T. ) ;
#52588 = CARTESIAN_POINT ( 'NONE',  ( -0.7808398950131225646, -0.05778040916215522460, 0.4822834645669289988 ) ) ;
#52590 = CARTESIAN_POINT ( 'NONE',  ( -0.09842519685039295696, -0.4536011799217367080, 0.2665933059059888421 ) ) ;
#52591 = CARTESIAN_POINT ( 'NONE',  ( 3.224202737261815166, 2.716535433070866645, 0.5314960629921260393 ) ) ;
#52592 = CARTESIAN_POINT ( 'NONE',  ( -0.7939632545931754048, -0.3162353388693405765, 0.4822834645669290543 ) ) ;
#52593 = CARTESIAN_POINT ( 'NONE',  ( -0.7939632545931750718, -0.05778040916215560624, -0.4822834645669293319 ) ) ;
#52594 = CARTESIAN_POINT ( 'NONE',  ( 0.06561679790026316017, -0.4281496062992124485, 0.4176697321401328655 ) ) ;
#52595 = CARTESIAN_POINT ( 'NONE',  ( 0.1070741851644054776, -0.3996062992125984925, -2.366797900262467280 ) ) ;
#52596 = ADVANCED_FACE ( 'NONE', ( #79181 ), #79879, .T. ) ;
#52597 = CARTESIAN_POINT ( 'NONE',  ( 0.2867679344610365999, 0.2867679344610365999, -2.265072547735221153 ) ) ;
#52598 = CARTESIAN_POINT ( 'NONE',  ( -1.627296587926508442, -0.5023911411419708095, -0.1820866141732282451 ) ) ;
#52599 = CARTESIAN_POINT ( 'NONE',  ( 0.5839895013123367340, 0.1771653543307087630, 0.09757992244046791164 ) ) ;
#52600 = CARTESIAN_POINT ( 'NONE',  ( 1.325459317585302665, 0.05413385826771626580, -0.4176697321401330321 ) ) ;
#52601 = CARTESIAN_POINT ( 'NONE',  ( -0.9317585301837263412, -0.004921259842519576551, 0.3153832671262227771 ) ) ;
#52602 = CARTESIAN_POINT ( 'NONE',  ( -1.017060367454067249, -0.2845877964562161244, -0.3641732283464567121 ) ) ;
#52603 = CARTESIAN_POINT ( 'NONE',  ( -0.7677165354330699465, -0.5400638737290845981, -0.3530559997133363437 ) ) ;
#52604 = CARTESIAN_POINT ( 'NONE',  ( -0.2690288713910754526, 0.2952755905511810774, -0.1292274648535930714 ) ) ;
#52605 = CARTESIAN_POINT ( 'NONE',  ( 0.6561679790026253567, -0.5023911411419708095, -0.1820866141732282451 ) ) ;
#52606 = CARTESIAN_POINT ( 'NONE',  ( -0.2635551335312363852, 0.1334335510540912706, 5.584872361112683592 ) ) ;
#52607 = CARTESIAN_POINT ( 'NONE',  ( 0.9383202099737536495, -0.2845877964562159024, 0.3641732283464567677 ) ) ;
#52608 = EDGE_CURVE ( 'NONE', #32285, #30272, #66405, .T. ) ;
#52609 = CARTESIAN_POINT ( 'NONE',  ( 0.2559055118110243332, 0.1660481256975885056, 0.3530559997133364547 ) ) ;
#52610 = EDGE_CURVE ( 'NONE', #18339, #50999, #62797, .T. ) ;
#52611 = CARTESIAN_POINT ( 'NONE',  ( -0.1998031496062994405, 0.3460692066303957537, -0.08989501312335958227 ) ) ;
#52612 = CARTESIAN_POINT ( 'NONE',  ( -0.8661417322834640276, -0.1870078740157480879, -0.4822834645669291653 ) ) ;
#52613 = CARTESIAN_POINT ( 'NONE',  ( -0.2867679344610365999, 0.2867679344610364889, -1.521653543307086354 ) ) ;
#52614 = CARTESIAN_POINT ( 'NONE',  ( 1.325459317585302665, -0.004921259842519870586, -0.3153832671262229437 ) ) ;
#52615 = CARTESIAN_POINT ( 'NONE',  ( 0.2952755905511819101, 0.1660481256975883668, -0.3530559997133364547 ) ) ;
#52616 = CARTESIAN_POINT ( 'NONE',  ( 0.2362204724409456558, -0.1870078740157479769, 0.4822834645669291653 ) ) ;
#52617 = CARTESIAN_POINT ( 'NONE',  ( 0.03280839895013198948, -0.5511811023622048555, -0.09757992244046775898 ) ) ;
#52618 = CARTESIAN_POINT ( 'NONE',  ( -0.1938976377952756625, 0.2726377952755905665, 0.1574803149606299191 ) ) ;
#52619 = CARTESIAN_POINT ( 'NONE',  ( 0.09186351706036827158, -0.004921259842519576551, 0.3153832671262227771 ) ) ;
#52620 = CARTESIAN_POINT ( 'NONE',  ( 0.7611548556430454138, 0.2306618581243847221, -0.2411417322834647770 ) ) ;
#52621 = B_SPLINE_CURVE_WITH_KNOTS ( 'NONE', 3,
 ( #44105, #5407, #82030, #56331 ),
 .UNSPECIFIED., .F., .F.,
 ( 4, 4 ),
 ( 0.1331161126011577434, 0.1345277053022641001 ),
 .UNSPECIFIED. ) ;
#52622 = CARTESIAN_POINT ( 'NONE',  ( -0.9383202099737524282, -0.08942795157527998196, 0.3641732283464567121 ) ) ;
#52623 = CARTESIAN_POINT ( 'NONE',  ( -0.6299212598425188991, -0.1870078740157480879, -0.4822834645669291653 ) ) ;
#52624 = DIRECTION ( 'NONE',  ( 0.000000000000000000, 0.000000000000000000, -1.000000000000000000 ) ) ;
#52625 = ORIENTED_EDGE ( 'NONE', *, *, #32904, .T. ) ;
#52626 = CARTESIAN_POINT ( 'NONE',  ( -1.023622047244093558, -0.1870078740157479769, 0.4822834645669291653 ) ) ;
#52627 = CARTESIAN_POINT ( 'NONE',  ( -0.9251968503937002541, 0.07958543189024085140, 0.2665933059059887866 ) ) ;
#52628 = CIRCLE ( 'NONE', #57970, 0.09842519685039351207 ) ;
#52629 = CARTESIAN_POINT ( 'NONE',  ( -0.06561679790026180015, -0.4281496062992127816, -0.4176697321401328100 ) ) ;
#52630 = CARTESIAN_POINT ( 'NONE',  ( -1.541994750656167090, 0.2952755905511811885, 0.1292274648535926551 ) ) ;
#52631 = CARTESIAN_POINT ( 'NONE',  ( -0.9448818897637790704, -0.1870078740157480879, -0.4822834645669291653 ) ) ;
#52632 = LINE ( 'NONE', #20246, #6815 ) ;
#52634 = CARTESIAN_POINT ( 'NONE',  ( 1.095800524934383846, -0.3162353388693405765, 0.4822834645669290543 ) ) ;
#52633 = CARTESIAN_POINT ( 'NONE',  ( 0.6299212598425100174, 1.724409448818897905, 0.9285414500055780840 ) ) ;
#52635 = CARTESIAN_POINT ( 'NONE',  ( 1.200787401574803681, 0.1660481256975885056, 0.3530559997133364547 ) ) ;
#52636 = CARTESIAN_POINT ( 'NONE',  ( -0.3917322834645669549, -0.1049643490035306603, -2.557742782152230721 ) ) ;
#52637 = CARTESIAN_POINT ( 'NONE',  ( -1.604771003085130321, 1.320215725944019258, 0.1466069496707743391 ) ) ;
#52638 = CARTESIAN_POINT ( 'NONE',  ( -1.345144356955379816, -0.05778040916215560624, -0.4822834645669293319 ) ) ;
#52639 = CARTESIAN_POINT ( 'NONE',  ( -0.4724409448818895907, -0.1265901696524993070, -0.8333333333333332593 ) ) ;
#52640 = CARTESIAN_POINT ( 'NONE',  ( -0.3460692066303960868, 0.1998031496062990242, 0.1312335958005249048 ) ) ;
#52641 = VERTEX_POINT ( 'NONE', #3800 ) ;
#52642 = CARTESIAN_POINT ( 'NONE',  ( -0.2821522309711278487, -0.5511811023622048555, -0.09757992244046775898 ) ) ;
#52643 = CARTESIAN_POINT ( 'NONE',  ( 0.1958661417322834775, 0.3392501089628018884, -1.868766404199474929 ) ) ;
#52644 = EDGE_LOOP ( 'NONE', ( #36520, #60758, #2896, #82886 ) ) ;
#52645 = CARTESIAN_POINT ( 'NONE',  ( 0.3346456692913390985, 0.1660481256975885056, 0.3530559997133364547 ) ) ;
#52646 = CARTESIAN_POINT ( 'NONE',  ( 0.09842519685039434474, -0.5400638737290845981, -0.3530559997133363437 ) ) ;
#52647 = CARTESIAN_POINT ( 'NONE',  ( -0.7283464566929126471, -0.5400638737290844871, 0.3530559997133364547 ) ) ;
#52648 = DIRECTION ( 'NONE',  ( 0.000000000000000000, 0.000000000000000000, 1.000000000000000000 ) ) ;
#52649 = CARTESIAN_POINT ( 'NONE',  ( -0.7020997375328074108, -0.08942795157527998196, 0.3641732283464567121 ) ) ;
#52650 = CARTESIAN_POINT ( 'NONE',  ( 0.5905511811023629321, 0.2952755905511811885, 0.000000000000000000 ) ) ;
#52651 = CARTESIAN_POINT ( 'NONE',  ( 0.4265091863517067039, -0.5511811023622048555, -0.09757992244046775898 ) ) ;
#52652 = CARTESIAN_POINT ( 'NONE',  ( -0.4921259842519677963, 0.1660481256975883668, -0.3530559997133364547 ) ) ;
#52653 = CARTESIAN_POINT ( 'NONE',  ( 0.3917322834645668994, -0.1049643490035303134, -1.136463623850706650 ) ) ;
#52654 = CARTESIAN_POINT ( 'NONE',  ( -0.7152230971128602510, -0.3162353388693405765, 0.4822834645669290543 ) ) ;
#52655 = DIRECTION ( 'NONE',  ( 0.000000000000000000, 0.000000000000000000, 1.000000000000000000 ) ) ;
#52656 = CARTESIAN_POINT ( 'NONE',  ( 1.469816272965879911, -0.6046776061558807314, 0.2411417322834647770 ) ) ;
#52657 = CARTESIAN_POINT ( 'NONE',  ( 1.581364829396326277, -0.2845877964562161244, -0.3641732283464567121 ) ) ;
#52658 = VERTEX_POINT ( 'NONE', #54721 ) ;
#52659 = CARTESIAN_POINT ( 'NONE',  ( 0.1049643490035303967, 0.3917322834645670659, -2.667342150427508773 ) ) ;
#52660 = CARTESIAN_POINT ( 'NONE',  ( -0.1902887139107604098, 0.2952755905511810774, -0.1292274648535930714 ) ) ;
#52661 = ORIENTED_EDGE ( 'NONE', *, *, #23107, .T. ) ;
#52662 = CARTESIAN_POINT ( 'NONE',  ( -1.332020997375327642, -0.3162353388693409650, -0.4822834645669289433 ) ) ;
#52663 = CARTESIAN_POINT ( 'NONE',  ( 1.286089238845145033, 0.2306618581243848609, 0.2411417322834645549 ) ) ;
#52664 = CARTESIAN_POINT ( 'NONE',  ( 1.272965879265092637, 0.05413385826771666132, 0.4176697321401328100 ) ) ;
#52665 = CARTESIAN_POINT ( 'NONE',  ( 0.1443569553805781891, -0.4281496062992124485, 0.4176697321401328655 ) ) ;
#52666 = CARTESIAN_POINT ( 'NONE',  ( -0.3149606299212590610, -0.1870078740157480879, -0.4822834645669291653 ) ) ;
#52667 = CARTESIAN_POINT ( 'NONE',  ( -9.594673741351313045E-17, 0.3917322834645670104, -1.659448818897637734 ) ) ;
#52668 = CARTESIAN_POINT ( 'NONE',  ( -1.023622047244094002, -0.1870078740157480879, -0.4822834645669291653 ) ) ;
#52669 = CARTESIAN_POINT ( 'NONE',  ( -0.4921259842519677963, 0.1660481256975883668, -0.3530559997133364547 ) ) ;
#52670 = CARTESIAN_POINT ( 'NONE',  ( 0.01968503937007957949, -0.4536011799217368745, -0.2665933059059886201 ) ) ;
#52671 = CARTESIAN_POINT ( 'NONE',  ( -0.03757601356356682354, 0.4709442531824372113, -2.755905511811023612 ) ) ;
#52672 = CARTESIAN_POINT ( 'NONE',  ( -0.3215223097112853146, -0.3162353388693405765, 0.4822834645669290543 ) ) ;
#52673 = PLANE ( 'NONE',  #53372 ) ;
#52674 = EDGE_CURVE ( 'NONE', #20402, #60445, #66504, .T. ) ;
#52675 = CARTESIAN_POINT ( 'NONE',  ( 0.6824146981627303710, 0.2306618581243847221, -0.2411417322834647770 ) ) ;
#52676 = CARTESIAN_POINT ( 'NONE',  ( 3.918940769308645322, 1.247921457474008511, -0.3771434222490559485 ) ) ;
#52677 = CARTESIAN_POINT ( 'NONE',  ( -0.1377952755905504645, -0.5400638737290845981, -0.3530559997133363437 ) ) ;
#52678 = CARTESIAN_POINT ( 'NONE',  ( -0.3477690288713905509, -0.5511811023622046335, 0.09757992244046803654 ) ) ;
#52680 = CARTESIAN_POINT ( 'NONE',  ( -1.854472803289052507, 2.716535433070866645, -0.5314960629921260393 ) ) ;
#52679 = CARTESIAN_POINT ( 'NONE',  ( 1.122047244094488860, -0.4536011799217368745, -0.2665933059059886201 ) ) ;
#52681 = CARTESIAN_POINT ( 'NONE',  ( -0.2362204724409447953, -0.4091458600556404646, -0.1423884514435695414 ) ) ;
#52682 = CARTESIAN_POINT ( 'NONE',  ( 1.496062992125985147, -0.1870078740157479769, 0.3641732283464567677 ) ) ;
#52683 = CARTESIAN_POINT ( 'NONE',  ( 1.135170603674541256, 0.2952755905511811885, 0.1292274648535926551 ) ) ;
#52684 = CARTESIAN_POINT ( 'NONE',  ( -0.3949938075777408852, -0.1058382717557502933, -0.1227034120734908501 ) ) ;
#52685 = CARTESIAN_POINT ( 'NONE',  ( 0.1706036745406830368, 0.05413385826771666132, 0.4176697321401328100 ) ) ;
#52686 = CARTESIAN_POINT ( 'NONE',  ( -1.450131233595799651, 0.2952755905511810774, -0.1292274648535930714 ) ) ;
#52687 = CARTESIAN_POINT ( 'NONE',  ( -1.528871391076114250, 0.2952755905511810774, -0.1292274648535930714 ) ) ;
#52688 = CARTESIAN_POINT ( 'NONE',  ( -0.2099737532808391705, -0.6046776061558809534, -0.2411417322834644161 ) ) ;
#52689 = CARTESIAN_POINT ( 'NONE',  ( -0.1974969037888704149, -0.3420746716998661063, -0.1423884514435695414 ) ) ;
#52690 = CARTESIAN_POINT ( 'NONE',  ( -1.476377952755905110, 0.07958543189024085140, 0.2665933059059887866 ) ) ;
#52691 = CARTESIAN_POINT ( 'NONE',  ( 0.5314960629921264834, 0.1660481256975883668, -0.3530559997133364547 ) ) ;
#52692 = AXIS2_PLACEMENT_3D ( 'NONE', #3066, #16953, #49321 ) ;
#52693 = CARTESIAN_POINT ( 'NONE',  ( 1.148293963254593875, -0.5511811023622046335, 0.09757992244046803654 ) ) ;
#52694 = CARTESIAN_POINT ( 'NONE',  ( 0.2390676544208471532, 1.098169981481509350, 0.2023185670810682124 ) ) ;
#52695 = CARTESIAN_POINT ( 'NONE',  ( 0.4855643044619430415, -0.3690944881889765550, -0.3153832671262227771 ) ) ;
#52696 = CARTESIAN_POINT ( 'NONE',  ( -1.194225721784776262, -0.4281496062992124485, 0.4176697321401328655 ) ) ;
#52697 = CARTESIAN_POINT ( 'NONE',  ( -0.3996062992125984925, -0.1070741851644056858, -0.7526246719160103460 ) ) ;
#52698 = CARTESIAN_POINT ( 'NONE',  ( 1.312335958005250269, -0.6046776061558807314, 0.2411417322834647770 ) ) ;
#52699 = CARTESIAN_POINT ( 'NONE',  ( -0.3392501089628017219, -0.1958661417322836718, -0.5170603674540682482 ) ) ;
#52701 = DIRECTION ( 'NONE',  ( 0.000000000000000000, 0.000000000000000000, 1.000000000000000000 ) ) ;
#52700 = CARTESIAN_POINT ( 'NONE',  ( 0.9120734908136490793, 0.2952755905511810774, -0.1292274648535930714 ) ) ;
#52702 = CARTESIAN_POINT ( 'NONE',  ( -0.7998211177050861265, -2.609869883881465018E-15, -0.3464511005275220379 ) ) ;
#52703 = CARTESIAN_POINT ( 'NONE',  ( 0.3937007874015754361, -0.1870078740157480601, -0.3641732283464567677 ) ) ;
#52704 = CARTESIAN_POINT ( 'NONE',  ( 0.7283464566929143125, 0.1660481256975885056, 0.3530559997133364547 ) ) ;
#52705 = CARTESIAN_POINT ( 'NONE',  ( 1.620734908136483465, -0.5511811023622046335, 0.09757992244046803654 ) ) ;
#52706 = CARTESIAN_POINT ( 'NONE',  ( -0.7414698162729651543, 0.1771653543307087075, -0.09757992244046823083 ) ) ;
#52707 = CARTESIAN_POINT ( 'NONE',  ( -0.8464566929133852113, -0.5400638737290845981, -0.3530559997133363437 ) ) ;
#52708 = CARTESIAN_POINT ( 'NONE',  ( -1.633858267716534529, -0.5400638737290845981, -0.3530559997133363437 ) ) ;
#52709 = CARTESIAN_POINT ( 'NONE',  ( 0.8070866141732289112, -0.5400638737290845981, -0.3530559997133363437 ) ) ;
#52710 = CARTESIAN_POINT ( 'NONE',  ( 1.692913385826772421, 0.2952755905511811885, 0.000000000000000000 ) ) ;
#52711 = CARTESIAN_POINT ( 'NONE',  ( -0.3893108287682406909, 0.05073257145186435557, -1.220472440944881276 ) ) ;
#52712 = CARTESIAN_POINT ( 'NONE',  ( 0.7086614173228352742, -0.1870078740157480879, -0.4822834645669291653 ) ) ;
#52713 = B_SPLINE_CURVE_WITH_KNOTS ( 'NONE', 3,
 ( #75085, #62028, #4364, #55695 ),
 .UNSPECIFIED., .F., .F.,
 ( 4, 4 ),
 ( 0.05917802304550456166, 0.06118368893514435081 ),
 .UNSPECIFIED. ) ;
#52714 = CARTESIAN_POINT ( 'NONE',  ( -1.157146581871515012E-16, 0.4724409448818898682, -2.753937007874015741 ) ) ;
#52715 = CARTESIAN_POINT ( 'NONE',  ( 0.3858508372531669339, 1.260953067117916326, 3.918063942240381792 ) ) ;
#52716 = CARTESIAN_POINT ( 'NONE',  ( 1.364829396325460076, 0.2306618581243848609, 0.2411417322834645549 ) ) ;
#52717 = CARTESIAN_POINT ( 'NONE',  ( -1.541994750656167090, 0.1771653543307087630, 0.09757992244046791164 ) ) ;
#52718 = CARTESIAN_POINT ( 'NONE',  ( 1.391076115485564868, 0.1283753931104746893, -0.1820866141732285504 ) ) ;
#52719 = CARTESIAN_POINT ( 'NONE',  ( -1.338582677165353729, -0.1870078740157479769, 0.3641732283464567677 ) ) ;
#52720 = CARTESIAN_POINT ( 'NONE',  ( -0.6364829396325453192, -0.08942795157528024563, -0.3641732283464568787 ) ) ;
#52721 = CARTESIAN_POINT ( 'NONE',  ( 3.937007874015748143, 1.537401574803149984, 0.4744094488188975722 ) ) ;
#52722 = CARTESIAN_POINT ( 'NONE',  ( 0.4921259842519691285, 0.07958543189024085140, 0.2665933059059887866 ) ) ;
#52723 = CARTESIAN_POINT ( 'NONE',  ( 0.6036745406824154392, 0.2306618581243847221, -0.2411417322834647770 ) ) ;
#52724 = CARTESIAN_POINT ( 'NONE',  ( 1.017060367454068581, -0.05778040916215560624, -0.4822834645669293319 ) ) ;
#52725 = CARTESIAN_POINT ( 'NONE',  ( -0.01968503937007793844, 0.1660481256975883668, -0.3530559997133364547 ) ) ;
#52726 = CARTESIAN_POINT ( 'NONE',  ( -0.01968503937007793844, -0.4536011799217367080, 0.2665933059059888421 ) ) ;
#52728 = CARTESIAN_POINT ( 'NONE',  ( 1.108923884514436242, -0.05778040916215522460, 0.4822834645669289988 ) ) ;
#52727 = B_SPLINE_CURVE_WITH_KNOTS ( 'NONE', 3,
 ( #59261, #60099, #39491, #45786 ),
 .UNSPECIFIED., .F., .F.,
 ( 4, 4 ),
 ( 2.857347768991906607E-07, 0.001436604392377180406 ),
 .UNSPECIFIED. ) ;
#52729 = CARTESIAN_POINT ( 'NONE',  ( -1.646981627296586703, -0.05778040916215522460, 0.4822834645669289988 ) ) ;
#52730 = CARTESIAN_POINT ( 'NONE',  ( -0.3871391076115479057, -0.3162353388693409650, -0.4822834645669289433 ) ) ;
#52731 = CARTESIAN_POINT ( 'NONE',  ( -0.3996062992125986590, 0.1070741851644051862, -0.9776902887139107268 ) ) ;
#52732 = CARTESIAN_POINT ( 'NONE',  ( 0.03280839895013198948, 0.2066929133858267931, 0.1054918080437490802 ) ) ;
#52733 = CARTESIAN_POINT ( 'NONE',  ( 0.2362204724409456558, -0.1870078740157480879, -0.4822834645669291653 ) ) ;
#52734 = CARTESIAN_POINT ( 'NONE',  ( -0.7283464566929126471, -0.5400638737290844871, 0.3530559997133364547 ) ) ;
#52735 = CARTESIAN_POINT ( 'NONE',  ( -0.03937007874015669567, -0.6692913385826771977, 8.415575281601705876E-17 ) ) ;
#52736 = ADVANCED_FACE ( 'NONE', ( #41272 ), #55121, .F. ) ;
#52737 = CARTESIAN_POINT ( 'NONE',  ( -0.3460692066303958092, -0.1998031496062994683, -2.572178477690288734 ) ) ;
#52738 = CARTESIAN_POINT ( 'NONE',  ( 0.3420746716998660508, -0.1974969037888703871, -1.837270341207348556 ) ) ;
#52740 = CARTESIAN_POINT ( 'NONE',  ( 4.797336870675656522E-17, -0.3917322834645670104, -0.5433070866141732624 ) ) ;
#52739 = AXIS2_PLACEMENT_3D ( 'NONE', #11201, #18740, #44382 ) ;
#52741 = FACE_OUTER_BOUND ( 'NONE', #82256, .T. ) ;
#52742 = EDGE_CURVE ( 'NONE', #39419, #15857, #40860, .T. ) ;
#52743 = CARTESIAN_POINT ( 'NONE',  ( -0.7808398950131225646, -0.08942795157527998196, 0.3641732283464567121 ) ) ;
#52744 = CARTESIAN_POINT ( 'NONE',  ( -0.1958661417322836718, 0.3392501089628017219, -1.265091863517060489 ) ) ;
#52745 = CARTESIAN_POINT ( 'NONE',  ( -1.660104986876639543, -0.05778040916215560624, -0.4822834645669293319 ) ) ;
#52746 = AXIS2_PLACEMENT_3D ( 'NONE', #74608, #49320, #10630 ) ;
#52747 = CARTESIAN_POINT ( 'NONE',  ( 0.3392501089628018329, -0.1958661417322834497, -0.02753973933627114692 ) ) ;
#52748 = CARTESIAN_POINT ( 'NONE',  ( 0.4986876640419954376, -0.6046776061558809534, -0.2411417322834644161 ) ) ;
#52749 = CARTESIAN_POINT ( 'NONE',  ( -0.6824146981627291497, -0.5023911411419708095, -0.1820866141732282451 ) ) ;
#52750 = CARTESIAN_POINT ( 'NONE',  ( 1.240157480314961314, -0.5400638737290844871, 0.3530559997133364547 ) ) ;
#52751 = CARTESIAN_POINT ( 'NONE',  ( 0.3215223097112867578, -0.05778040916215522460, 0.4822834645669289988 ) ) ;
#52752 = CARTESIAN_POINT ( 'NONE',  ( 0.1265901696524989184, 0.4724409448818898127, -0.07020997375328084933 ) ) ;
#52753 = CARTESIAN_POINT ( 'NONE',  ( 0.1998031496062994405, -0.3460692066303958092, -2.769028871391076230 ) ) ;
#52754 = CARTESIAN_POINT ( 'NONE',  ( 0.3917322834645670659, -0.1049643490035303273, -1.210649237041681703 ) ) ;
#52755 = CARTESIAN_POINT ( 'NONE',  ( 1.384514435695538559, 0.2952755905511810774, -0.1292274648535930714 ) ) ;
#52756 = CARTESIAN_POINT ( 'NONE',  ( 0.6824146981627303710, 0.2306618581243847221, -0.2411417322834647770 ) ) ;
#52757 = CARTESIAN_POINT ( 'NONE',  ( 0.2034120734908142214, 0.2952755905511810774, -0.1292274648535930714 ) ) ;
#52758 = CARTESIAN_POINT ( 'NONE',  ( -1.653543307086613234, -0.1870078740157479769, 0.4822834645669291653 ) ) ;
#52759 = CARTESIAN_POINT ( 'NONE',  ( 0.7480314960629927956, 0.2952755905511811885, 0.000000000000000000 ) ) ;
#52760 = CARTESIAN_POINT ( 'NONE',  ( -0.3392501089628017219, -0.1958661417322836718, -0.6095800524934383846 ) ) ;
#52761 = CARTESIAN_POINT ( 'NONE',  ( 0.04593175853018440641, 0.2952755905511810774, -0.1292274648535930714 ) ) ;
#52762 = CARTESIAN_POINT ( 'NONE',  ( 1.220472440944882608, 0.2952755905511811885, 0.000000000000000000 ) ) ;
#52763 = CARTESIAN_POINT ( 'NONE',  ( 0.2952755905511819101, 0.1660481256975883668, -0.3530559997133364547 ) ) ;
#52764 = CARTESIAN_POINT ( 'NONE',  ( 0.9383202099737538715, -0.08942795157528024563, -0.3641732283464568787 ) ) ;
#52765 = CARTESIAN_POINT ( 'NONE',  ( -1.496062992125983815, -0.1870078740157480879, -0.4822834645669291653 ) ) ;
#52766 = CARTESIAN_POINT ( 'NONE',  ( -1.561679790026246017, 0.05413385826771666132, 0.4176697321401328100 ) ) ;
#52767 = CARTESIAN_POINT ( 'NONE',  ( 0.8595800524934390507, -0.05778040916215560624, -0.4822834645669293319 ) ) ;
#52768 = CARTESIAN_POINT ( 'NONE',  ( 0.09865214182602936865, -0.3796925558542994517, -1.929133858267717549 ) ) ;
#52769 = EDGE_CURVE ( 'NONE', #40470, #12202, #43535, .T. ) ;
#52770 = CARTESIAN_POINT ( 'NONE',  ( -0.1049643490035307020, 0.3917322834645669549, -1.888451443569553412 ) ) ;
#52771 = ORIENTED_EDGE ( 'NONE', *, *, #18921, .T. ) ;
#52772 = CARTESIAN_POINT ( 'NONE',  ( -0.3996062992125986035, -7.340648628747425578E-17, -0.5118110236220472231 ) ) ;
#52773 = ORIENTED_EDGE ( 'NONE', *, *, #81291, .F. ) ;
#52774 = CARTESIAN_POINT ( 'NONE',  ( 1.253280839895013710, -0.05778040916215560624, -0.4822834645669293319 ) ) ;
#52775 = CARTESIAN_POINT ( 'NONE',  ( 0.8923884514435701520, -0.5023911411419708095, -0.1820866141732282451 ) ) ;
#52776 = CARTESIAN_POINT ( 'NONE',  ( -1.614173228346457378, 1.330640075373402897, 0.1372047244094476981 ) ) ;
#52777 = CARTESIAN_POINT ( 'NONE',  ( -0.3234312996134343088, 1.189126250296157261, 2.759783988742167349 ) ) ;
#52778 = CARTESIAN_POINT ( 'NONE',  ( -0.3458507752293906723, -0.3458507752293910609, -1.161417322834645605 ) ) ;
#52779 = CARTESIAN_POINT ( 'NONE',  ( -0.1049643490035307020, 0.3917322834645669549, -0.7211286089238846397 ) ) ;
#52780 = EDGE_CURVE ( 'NONE', #70804, #29875, #47571, .T. ) ;
#52781 = CARTESIAN_POINT ( 'NONE',  ( 1.358267716535433323, -0.5400638737290845981, -0.3530559997133363437 ) ) ;
#52782 = FACE_OUTER_BOUND ( 'NONE', #4711, .T. ) ;
#52783 = CARTESIAN_POINT ( 'NONE',  ( -0.4921259842519677963, -0.5400638737290844871, 0.3530559997133364547 ) ) ;
#52784 = CARTESIAN_POINT ( 'NONE',  ( 0.9580052493438326877, 0.05413385826771666132, 0.4176697321401328100 ) ) ;
#52785 = ORIENTED_EDGE ( 'NONE', *, *, #42363, .T. ) ;
#52786 = CARTESIAN_POINT ( 'NONE',  ( -1.463254593175852492, -0.6692913385826773087, -0.1292274648535924053 ) ) ;
#52787 = CARTESIAN_POINT ( 'NONE',  ( -0.7205944486920646819, -4.754953748228849300E-15, -0.3627989612356167237 ) ) ;
#52788 = DIRECTION ( 'NONE',  ( -3.491481338843133355E-15, -6.123233995736767268E-17, 1.000000000000000000 ) ) ;
#52789 = CARTESIAN_POINT ( 'NONE',  ( 1.522309711286089939, 0.1283753931104748280, 0.1820866141732283561 ) ) ;
#52790 = DIRECTION ( 'NONE',  ( 0.000000000000000000, 0.000000000000000000, 1.000000000000000000 ) ) ;
#52791 = CARTESIAN_POINT ( 'NONE',  ( -1.010498687664041384, -0.004921259842519576551, 0.3153832671262227771 ) ) ;
#52792 = CARTESIAN_POINT ( 'NONE',  ( 0.8789144566217211851, 0.004960608223779470680, 0.3437734562760185741 ) ) ;
#52793 = CARTESIAN_POINT ( 'NONE',  ( 0.7742782152230979209, 0.05413385826771626580, -0.4176697321401330321 ) ) ;
#52794 = ORIENTED_EDGE ( 'NONE', *, *, #82467, .F. ) ;
#52796 = CARTESIAN_POINT ( 'NONE',  ( -0.4199475065616791736, 0.1539470093639521697, -0.1968503937007875793 ) ) ;
#52795 = CARTESIAN_POINT ( 'NONE',  ( 1.080276388343102000E-18, 0.000000000000000000, -0.1771653543307086798 ) ) ;
#52797 = CARTESIAN_POINT ( 'NONE',  ( 0.6955380577427828781, -0.4281496062992124485, 0.4176697321401328655 ) ) ;
#52798 = CARTESIAN_POINT ( 'NONE',  ( -1.555118110236219930, 0.1660481256975885056, 0.3530559997133364547 ) ) ;
#52799 = CARTESIAN_POINT ( 'NONE',  ( -0.1958661417322834497, -0.3392501089628018884, -0.6180909204386334510 ) ) ;
#52800 = VECTOR ( 'NONE', #80614, 39.37007874015748143 ) ;
#52801 = CARTESIAN_POINT ( 'NONE',  ( -0.6889763779527552368, -0.4536011799217368745, -0.2665933059059886201 ) ) ;
#52802 = CARTESIAN_POINT ( 'NONE',  ( 1.653543307086614789, -0.1870078740157479769, 0.4822834645669291653 ) ) ;
#52803 = CARTESIAN_POINT ( 'NONE',  ( 0.4330708661417329575, -0.6692913385826771977, 8.415575281601705876E-17 ) ) ;
#52804 = CARTESIAN_POINT ( 'NONE',  ( -1.135170603674539924, 0.1771653543307087075, -0.09757992244046823083 ) ) ;
#52805 = CARTESIAN_POINT ( 'NONE',  ( 0.06561679790026316017, -0.004921259842519870586, -0.3153832671262229437 ) ) ;
#52806 = CARTESIAN_POINT ( 'NONE',  ( -0.2887139107611542133, 0.2306618581243848609, 0.2411417322834645549 ) ) ;
#52807 = CARTESIAN_POINT ( 'NONE',  ( -1.305774278215222184, 0.1771653543307087630, 0.09757992244046791164 ) ) ;
#52808 = CARTESIAN_POINT ( 'NONE',  ( -0.1049643490035307158, 0.3917322834645670104, -0.1607804706374822146 ) ) ;
#52809 = CARTESIAN_POINT ( 'NONE',  ( 0.6102362204724416372, -0.5400638737290844871, 0.3530559997133364547 ) ) ;
#52810 = CARTESIAN_POINT ( 'NONE',  ( 5.785732909357575061E-17, -0.4724409448818898682, -0.2362204724409449064 ) ) ;
#52811 = CARTESIAN_POINT ( 'NONE',  ( -0.2362204724409447953, -0.4091458600556404646, -1.559711286089238591 ) ) ;
#52812 = CARTESIAN_POINT ( 'NONE',  ( -0.9251968503937002541, 0.1660481256975885056, 0.3530559997133364547 ) ) ;
#52813 = CARTESIAN_POINT ( 'NONE',  ( -0.05905511811023545637, -0.4536011799217368745, -0.2665933059059886201 ) ) ;
#52814 = CARTESIAN_POINT ( 'NONE',  ( -1.404199475065615932, -0.4281496062992127816, -0.4176697321401328100 ) ) ;
#52815 = CARTESIAN_POINT ( 'NONE',  ( 0.8267716535433078384, -0.5511811023622047445, 6.969142054262312111E-17 ) ) ;
#52816 = CARTESIAN_POINT ( 'NONE',  ( -0.6496062992125976043, -0.4536011799217367080, 0.2665933059059888421 ) ) ;
#52817 = CARTESIAN_POINT ( 'NONE',  ( -0.9055118110236215490, 0.2952755905511811885, 0.000000000000000000 ) ) ;
#52818 = CARTESIAN_POINT ( 'NONE',  ( -1.095800524934382292, -0.05778040916215522460, 0.4822834645669289988 ) ) ;
#52819 = CARTESIAN_POINT ( 'NONE',  ( 1.646981627296588035, -0.3162353388693405765, 0.4822834645669290543 ) ) ;
#52820 = CARTESIAN_POINT ( 'NONE',  ( 1.524059884292195765E-16, 0.04488074079120789317, 1.244489337948954555 ) ) ;
#52821 = CARTESIAN_POINT ( 'NONE',  ( 0.8070866141732289112, -0.4536011799217368745, -0.2665933059059886201 ) ) ;
#52822 = CARTESIAN_POINT ( 'NONE',  ( 0.2034120734908144990, -0.6692913385826771977, 0.1292274648535927661 ) ) ;
#52823 = CARTESIAN_POINT ( 'NONE',  ( -1.496062992125983815, -0.1870078740157479769, 0.4822834645669291653 ) ) ;
#52824 = CARTESIAN_POINT ( 'NONE',  ( -1.338582677165353729, -0.1870078740157480879, -0.4822834645669291653 ) ) ;
#52825 = EDGE_LOOP ( 'NONE', ( #4035, #12579, #46041, #47390, #31456, #57083 ) ) ;
#52826 = CARTESIAN_POINT ( 'NONE',  ( -0.2925321140481930149, -0.2925321140481933480, -2.655511811023622215 ) ) ;
#52827 = CARTESIAN_POINT ( 'NONE',  ( -1.154855643044618851, 0.1283753931104748280, 0.1820866141732283561 ) ) ;
#52828 = CARTESIAN_POINT ( 'NONE',  ( -0.5380577427821514602, 0.05413385826771666132, 0.4176697321401328100 ) ) ;
#52829 = CARTESIAN_POINT ( 'NONE',  ( 0.5380577427821529035, 0.05413385826771626580, -0.4176697321401330321 ) ) ;
#52830 = CARTESIAN_POINT ( 'NONE',  ( -1.305774278215222184, -0.5511811023622048555, -0.09757992244046775898 ) ) ;
#52831 = CARTESIAN_POINT ( 'NONE',  ( -0.3996062992125986590, 0.1070741851644051723, -1.999343832020997525 ) ) ;
#52832 = CARTESIAN_POINT ( 'NONE',  ( -1.587926509186350810, -0.4281496062992124485, 0.4176697321401328655 ) ) ;
#52833 = CARTESIAN_POINT ( 'NONE',  ( 0.8333333333333340365, -0.6692913385826771977, 0.1292274648535927661 ) ) ;
#52834 = CARTESIAN_POINT ( 'NONE',  ( 0.4133858267716541968, 0.1660481256975885056, 0.3530559997133364547 ) ) ;
#52835 = CARTESIAN_POINT ( 'NONE',  ( 1.043307086614173818, -0.5400638737290845981, -0.3530559997133363437 ) ) ;
#52837 = ADVANCED_FACE ( 'NONE', ( #3387 ), #34961, .F. ) ;
#52836 = CARTESIAN_POINT ( 'NONE',  ( 4.893765752498283308E-17, -0.3996062992125985480, -1.100393700787401619 ) ) ;
#52838 = CARTESIAN_POINT ( 'NONE',  ( -0.1998031496062991907, -0.3460692066303959757, -1.482939632545931863 ) ) ;
#52839 = CARTESIAN_POINT ( 'NONE',  ( -0.3949938075777411628, 0.1058382717557497937, -0.6627296587926508886 ) ) ;
#52840 = AXIS2_PLACEMENT_3D ( 'NONE', #6872, #75527, #32541 ) ;
#52841 = DIRECTION ( 'NONE',  ( -3.096699300667737957E-16, 1.000000000000000000, -0.000000000000000000 ) ) ;
#52842 = CARTESIAN_POINT ( 'NONE',  ( 0.1181102362204730916, -0.5511811023622047445, 6.969142054262312111E-17 ) ) ;
#52843 = CARTESIAN_POINT ( 'NONE',  ( 0.2559055118110243332, -0.5400638737290845981, -0.3530559997133363437 ) ) ;
#52844 = CARTESIAN_POINT ( 'NONE',  ( 1.187664041994751285, -0.3162353388693409650, -0.4822834645669289433 ) ) ;
#52845 = CARTESIAN_POINT ( 'NONE',  ( 4.837279021331061486E-17, -0.3949938075777409963, -1.572834645669291875 ) ) ;
#52846 = CARTESIAN_POINT ( 'NONE',  ( 0.4593175853018380828, -0.004921259842519870586, -0.3153832671262229437 ) ) ;
#52847 = CARTESIAN_POINT ( 'NONE',  ( -0.6824146981627288167, 0.2306618581243848609, 0.2411417322834645549 ) ) ;
#52848 = CARTESIAN_POINT ( 'NONE',  ( -1.614173228346455824, 0.2952755905511811885, 0.000000000000000000 ) ) ;
#52849 = CARTESIAN_POINT ( 'NONE',  ( 0.4593175853018380828, 0.05413385826771626580, -0.4176697321401330321 ) ) ;
#52850 = CARTESIAN_POINT ( 'NONE',  ( -0.3458507752293906723, -0.3458507752293910609, -1.948818897637795144 ) ) ;
#52851 = CARTESIAN_POINT ( 'NONE',  ( 0.1614515132151791432, -0.3594585737333411690, -2.755905511811025388 ) ) ;
#52852 = ORIENTED_EDGE ( 'NONE', *, *, #23429, .F. ) ;
#52853 = VERTEX_POINT ( 'NONE', #28640 ) ;
#52854 = AXIS2_PLACEMENT_3D ( 'NONE', #5431, #11766, #44532 ) ;
#52855 = CARTESIAN_POINT ( 'NONE',  ( -1.706036745406823485, 0.2306618581243848609, 0.2411417322834645549 ) ) ;
#52857 = CARTESIAN_POINT ( 'NONE',  ( -1.194225721784776262, -0.4281496062992124485, 0.4176697321401328655 ) ) ;
#52856 = CARTESIAN_POINT ( 'NONE',  ( -1.371391076115484609, -0.5511811023622046335, 0.09757992244046803654 ) ) ;
#52858 = CARTESIAN_POINT ( 'NONE',  ( -0.3917322834645668994, -0.1049643490035306742, -2.330689345635483356 ) ) ;
#52859 = CARTESIAN_POINT ( 'NONE',  ( 0.000000000000000000, 0.000000000000000000, 0.000000000000000000 ) ) ;
#52860 = CARTESIAN_POINT ( 'NONE',  ( 1.679790026246720025, 0.2306618581243848609, 0.2411417322834645549 ) ) ;
#52861 = CARTESIAN_POINT ( 'NONE',  ( -1.213910761154854745, 0.2952755905511810774, -0.1292274648535930714 ) ) ;
#52862 = CARTESIAN_POINT ( 'NONE',  ( 0.4986876640419954376, 0.2306618581243848609, 0.2411417322834645549 ) ) ;
#52863 = CARTESIAN_POINT ( 'NONE',  ( -1.141732283464566011, 0.2952755905511811885, 0.000000000000000000 ) ) ;
#52864 = CARTESIAN_POINT ( 'NONE',  ( 0.2867679344610365999, -0.2867679344610365999, -2.855623728837584085 ) ) ;
#52865 = CARTESIAN_POINT ( 'NONE',  ( 0.6889763779527563470, 0.1660481256975883668, -0.3530559997133364547 ) ) ;
#52866 = CARTESIAN_POINT ( 'NONE',  ( -9.594673741351313045E-17, 0.3917322834645670104, -1.881889763779527769 ) ) ;
#52867 = CARTESIAN_POINT ( 'NONE',  ( -1.384514435695537005, -0.5511811023622048555, -0.09757992244046775898 ) ) ;
#52868 = ORIENTED_EDGE ( 'NONE', *, *, #23484, .T. ) ;
#52869 = CARTESIAN_POINT ( 'NONE',  ( 0.3949938075777409408, 0.1058382717557500574, -2.171916010498687655 ) ) ;
#52870 = ORIENTED_EDGE ( 'NONE', *, *, #76757, .T. ) ;
#52871 = CARTESIAN_POINT ( 'NONE',  ( -1.699475065616797398, 0.1771653543307087630, 0.09757992244046791164 ) ) ;
#52872 = CARTESIAN_POINT ( 'NONE',  ( -1.181102362204723644, -0.1870078740157480879, -0.4822834645669291653 ) ) ;
#52873 = CARTESIAN_POINT ( 'NONE',  ( -1.272965879265091305, 0.05413385826771626580, -0.4176697321401330321 ) ) ;
#52874 = CARTESIAN_POINT ( 'NONE',  ( 0.3996062992125986590, -0.1070741851644053111, -0.7414698162729659314 ) ) ;
#52875 = CARTESIAN_POINT ( 'NONE',  ( -1.410761154855642463, -0.05778040916215522460, 0.4822834645669289988 ) ) ;
#52876 = CARTESIAN_POINT ( 'NONE',  ( -1.620734908136482577, -0.6692913385826773087, -0.1292274648535924053 ) ) ;
#52877 = CARTESIAN_POINT ( 'NONE',  ( -1.437007874015747477, 0.1660481256975883668, -0.3530559997133364547 ) ) ;
#52878 = CARTESIAN_POINT ( 'NONE',  ( -0.8398950131233585692, 0.2306618581243848609, 0.2411417322834645549 ) ) ;
#52879 = CARTESIAN_POINT ( 'NONE',  ( 0.03937007874015833325, -0.5511811023622047445, 6.969142054262312111E-17 ) ) ;
#52880 = CARTESIAN_POINT ( 'NONE',  ( 0.4417575354491365958, 1.710976477253062233, 2.103512204792471252 ) ) ;
#52881 = CARTESIAN_POINT ( 'NONE',  ( -0.1958661417322836718, 0.3392501089628017219, -0.5702099737532808632 ) ) ;
#52882 = CARTESIAN_POINT ( 'NONE',  ( -0.8464566929133852113, -0.4536011799217368745, -0.2665933059059886201 ) ) ;
#52883 = CARTESIAN_POINT ( 'NONE',  ( -0.8464566929133852113, 0.1660481256975885056, 0.3530559997133364547 ) ) ;
#52884 = CARTESIAN_POINT ( 'NONE',  ( 0.7939632545931766261, -0.05778040916215522460, 0.4822834645669289988 ) ) ;
#52885 = CARTESIAN_POINT ( 'NONE',  ( -0.8661417322834640276, -0.1870078740157479769, 0.4822834645669291653 ) ) ;
#52886 = VERTEX_POINT ( 'NONE', #80830 ) ;
#52887 = VERTEX_POINT ( 'NONE', #48397 ) ;
#52888 = CARTESIAN_POINT ( 'NONE',  ( -1.128608923884513837, 0.2306618581243847221, -0.2411417322834647770 ) ) ;
#52889 = CARTESIAN_POINT ( 'NONE',  ( 0.8989501312335963501, -0.6692913385826773087, -0.1292274648535924053 ) ) ;
#52890 = CARTESIAN_POINT ( 'NONE',  ( -1.496062992125983815, -0.1870078740157480601, -0.3641732283464567677 ) ) ;
#52891 = CARTESIAN_POINT ( 'NONE',  ( 0.4724409448818897572, -0.1265901696524988906, -1.213910761154855189 ) ) ;
#52892 = CARTESIAN_POINT ( 'NONE',  ( 1.973869084197717116, 1.199841186584411190, 0.3336616047370207783 ) ) ;
#52893 = CARTESIAN_POINT ( 'NONE',  ( 0.2867679344610365999, -0.2867679344610365444, -0.2480314960629920740 ) ) ;
#52894 = CARTESIAN_POINT ( 'NONE',  ( 0.1049643490035303689, 0.3917322834645670104, -2.282808398950130879 ) ) ;
#52895 = CARTESIAN_POINT ( 'NONE',  ( -0.4396325459317577122, -0.6692913385826773087, -0.1292274648535924053 ) ) ;
#52896 = CARTESIAN_POINT ( 'NONE',  ( -1.482939632545930975, -0.004921259842519576551, 0.3153832671262227771 ) ) ;
#52897 = CARTESIAN_POINT ( 'NONE',  ( -0.1998031496062994405, 0.3460692066303957537, -0.2473753280839895152 ) ) ;
#52899 = CARTESIAN_POINT ( 'NONE',  ( -0.6627296587926501115, 0.2066929133858267098, -0.1054918080437494132 ) ) ;
#52898 = CARTESIAN_POINT ( 'NONE',  ( -1.417322834645668772, -0.1870078740157479769, 0.4822834645669291653 ) ) ;
#52900 = CARTESIAN_POINT ( 'NONE',  ( -1.587926509186350810, -0.4281496062992124485, 0.4176697321401328655 ) ) ;
#52901 = CARTESIAN_POINT ( 'NONE',  ( -0.5446194225721777693, -0.3162353388693409650, -0.4822834645669289433 ) ) ;
#52902 = CARTESIAN_POINT ( 'NONE',  ( 0.2891555358219910499, -0.2891555358219909944, -2.852362204724409267 ) ) ;
#52903 = CARTESIAN_POINT ( 'NONE',  ( 0.4658792650918640033, -0.2845877964562159024, 0.3641732283464567677 ) ) ;
#52904 = CARTESIAN_POINT ( 'NONE',  ( -0.1049643490035307020, 0.3917322834645669549, -0.09120734908136493568 ) ) ;
#52905 = CARTESIAN_POINT ( 'NONE',  ( 0.4461942257217856311, 0.1283753931104746893, -0.1820866141732285504 ) ) ;
#52906 = CARTESIAN_POINT ( 'NONE',  ( 1.266404199475066328, -0.08942795157527998196, 0.3641732283464567121 ) ) ;
#52907 = CARTESIAN_POINT ( 'NONE',  ( 1.148293963254593653, 0.2952755905511810774, -0.1292274648535930714 ) ) ;
#52908 = CARTESIAN_POINT ( 'NONE',  ( 0.006561679790026889343, -0.2845877964562161244, -0.3641732283464567121 ) ) ;
#52909 = CARTESIAN_POINT ( 'NONE',  ( 0.1958661417322834775, 0.3392501089628018884, -1.711286089238845287 ) ) ;
#52910 = CARTESIAN_POINT ( 'NONE',  ( -1.089238845144356427, -0.4281496062992127816, -0.4176697321401328100 ) ) ;
#52911 = CARTESIAN_POINT ( 'NONE',  ( -0.2493438320209966919, -0.004921259842519870586, -0.3153832671262229437 ) ) ;
#52912 = CARTESIAN_POINT ( 'NONE',  ( -0.4724409448818898682, -8.678599364036362592E-17, -0.2736220472440945017 ) ) ;
#52913 = CARTESIAN_POINT ( 'NONE',  ( -0.3805774278215216522, -0.004921259842519576551, 0.3153832671262227771 ) ) ;
#52914 = CARTESIAN_POINT ( 'NONE',  ( -0.4744094488188934089, 1.537401574803149984, -1.016821367227985551 ) ) ;
#52915 = CARTESIAN_POINT ( 'NONE',  ( -0.09186351706036663400, -0.4281496062992124485, 0.4176697321401328655 ) ) ;
#52916 = DIRECTION ( 'NONE',  ( -0.000000000000000000, -1.000000000000000000, -0.000000000000000000 ) ) ;
#52917 = CIRCLE ( 'NONE', #77081, 0.1771653543307088186 ) ;
#52918 = CARTESIAN_POINT ( 'NONE',  ( 1.102362204724410155, -0.1870078740157479769, 0.3641732283464567677 ) ) ;
#52919 = CARTESIAN_POINT ( 'NONE',  ( -0.3674540682414692561, -0.5023911411419708095, -0.1820866141732282451 ) ) ;
#52920 = CARTESIAN_POINT ( 'NONE',  ( -0.1181102362204717315, -0.6692913385826771977, 8.415575281601705876E-17 ) ) ;
#52921 = DIRECTION ( 'NONE',  ( -1.000000000000000000, 0.000000000000000000, 0.000000000000000000 ) ) ;
#52922 = CARTESIAN_POINT ( 'NONE',  ( -1.312335958005248715, 0.1283753931104748280, 0.1820866141732283561 ) ) ;
#52923 = DIRECTION ( 'NONE',  ( 0.000000000000000000, 0.000000000000000000, -1.000000000000000000 ) ) ;
#52924 = CARTESIAN_POINT ( 'NONE',  ( 0.5839895013123367340, 0.2952755905511811885, 0.1292274648535926551 ) ) ;
#52925 = CARTESIAN_POINT ( 'NONE',  ( -0.9383202099737524282, -0.3162353388693409650, -0.4822834645669289433 ) ) ;
#52926 = CARTESIAN_POINT ( 'NONE',  ( 0.3996062992125984925, 0.1070741851644054637, -1.146325459317585116 ) ) ;
#52927 = EDGE_CURVE ( 'NONE', #5969, #55042, #77293, .T. ) ;
#52928 = CARTESIAN_POINT ( 'NONE',  ( 0.3392501089628018329, 0.1958661417322835607, -2.735564304461941987 ) ) ;
#52929 = CARTESIAN_POINT ( 'NONE',  ( 0.4002624671916016896, -0.2845877964562161244, -0.3641732283464567121 ) ) ;
#52930 = CARTESIAN_POINT ( 'NONE',  ( -0.6036745406824141069, -0.6046776061558809534, -0.2411417322834644161 ) ) ;
#52931 = CARTESIAN_POINT ( 'NONE',  ( -1.299212598425196097, 0.2952755905511811885, 0.000000000000000000 ) ) ;
#52932 = CARTESIAN_POINT ( 'NONE',  ( -1.167979002624671470, -0.004921259842519576551, 0.3153832671262227771 ) ) ;
#52933 = DIRECTION ( 'NONE',  ( -1.000000000000000000, 0.000000000000000000, 0.000000000000000000 ) ) ;
#52934 = CARTESIAN_POINT ( 'NONE',  ( -0.7808398950131222316, -0.2845877964562161244, -0.3641732283464567121 ) ) ;
#52935 = CYLINDRICAL_SURFACE ( 'NONE', #57376, 0.3051181102362204856 ) ;
#52936 = CARTESIAN_POINT ( 'NONE',  ( 0.9383202099737536495, -0.3162353388693405765, 0.4822834645669290543 ) ) ;
#52937 = CARTESIAN_POINT ( 'NONE',  ( 0.3996062992125986035, 0.1070741851644054776, -0.1246719160104987068 ) ) ;
#52938 = CARTESIAN_POINT ( 'NONE',  ( 0.1049643490035303967, 0.3917322834645670659, -2.667342150427508773 ) ) ;
#52939 = LINE ( 'NONE', #46216, #8252 ) ;
#52940 = CARTESIAN_POINT ( 'NONE',  ( -1.607611548556429737, -0.6692913385826771977, 0.1292274648535927661 ) ) ;
#52941 = CARTESIAN_POINT ( 'NONE',  ( -1.450131233595799651, -0.6692913385826771977, 0.1292274648535927661 ) ) ;
#52942 = CARTESIAN_POINT ( 'NONE',  ( 1.200787401574803681, -0.5400638737290845981, -0.3530559997133363437 ) ) ;
#52943 = CARTESIAN_POINT ( 'NONE',  ( 0.3392501089628018329, 0.1958661417322835607, -2.578083989501311901 ) ) ;
#52944 = CARTESIAN_POINT ( 'NONE',  ( 1.594488188976378673, -0.4536011799217368745, -0.2665933059059886201 ) ) ;
#52945 = CARTESIAN_POINT ( 'NONE',  ( 0.3871391076115493490, -0.3162353388693405765, 0.4822834645669290543 ) ) ;
#52946 = CARTESIAN_POINT ( 'NONE',  ( -0.2755905511811015396, -0.6692913385826771977, 8.415575281601705876E-17 ) ) ;
#52947 = CARTESIAN_POINT ( 'NONE',  ( -0.6979622409133203753, 5.991678263669262536E-15, 0.4118484887281945728 ) ) ;
#52948 = CARTESIAN_POINT ( 'NONE',  ( -0.3996062992125986035, -7.340648628747425578E-17, -2.086614173228346303 ) ) ;
#52949 = CARTESIAN_POINT ( 'NONE',  ( 0.5905511811023629321, -0.5511811023622047445, 6.969142054262312111E-17 ) ) ;
#52950 = CARTESIAN_POINT ( 'NONE',  ( -0.1070741851644051862, -0.3996062992125987146, -1.646981627296587591 ) ) ;
#52951 = ORIENTED_EDGE ( 'NONE', *, *, #70822, .T. ) ;
#52952 = CARTESIAN_POINT ( 'NONE',  ( -0.3917322834645670659, -7.196005306013484475E-17, -0.1935888695876134269 ) ) ;
#52953 = VERTEX_POINT ( 'NONE', #4204 ) ;
#52954 = CARTESIAN_POINT ( 'NONE',  ( 0.006561679790026889343, -0.05778040916215522460, 0.4822834645669289988 ) ) ;
#52955 = CARTESIAN_POINT ( 'NONE',  ( 1.292650918635171564, 0.2952755905511811885, 0.1292274648535926551 ) ) ;
#52956 = CARTESIAN_POINT ( 'NONE',  ( 0.1837270341207357105, -0.6046776061558809534, -0.2411417322834644161 ) ) ;
#52957 = CARTESIAN_POINT ( 'NONE',  ( -0.5643044619422565855, -0.3690944881889763329, 0.3153832671262228327 ) ) ;
#52958 = VECTOR ( 'NONE', #14607, 39.37007874015748143 ) ;
#52959 = CARTESIAN_POINT ( 'NONE',  ( 1.299212598425197429, -0.6692913385826771977, 8.415575281601705876E-17 ) ) ;
#52960 = CARTESIAN_POINT ( 'NONE',  ( -0.2952755905511803003, -0.5400638737290845981, -0.3530559997133363437 ) ) ;
#52961 = CARTESIAN_POINT ( 'NONE',  ( -0.1771653543307080136, -0.5400638737290844871, 0.3530559997133364547 ) ) ;
#52962 = CARTESIAN_POINT ( 'NONE',  ( -1.548556430446193399, -0.6046776061558809534, -0.2411417322834644161 ) ) ;
#52963 = CARTESIAN_POINT ( 'NONE',  ( 0.7020997375328090762, -0.05778040916215560624, -0.4822834645669293319 ) ) ;
#52964 = CARTESIAN_POINT ( 'NONE',  ( 1.167979002624672580, -0.4281496062992124485, 0.4176697321401328655 ) ) ;
#52965 = CARTESIAN_POINT ( 'NONE',  ( 0.1958661417322834775, 0.3392501089628018884, -0.7664041994750655507 ) ) ;
#52966 = CARTESIAN_POINT ( 'NONE',  ( 0.3740157480314966754, -0.4536011799217367080, 0.2665933059059888421 ) ) ;
#52967 = EDGE_LOOP ( 'NONE', ( #63219, #1213 ) ) ;
#52968 = CARTESIAN_POINT ( 'NONE',  ( -0.3949938075777409963, -7.255918531996591613E-17, -0.6692913385826770867 ) ) ;
#52969 = ORIENTED_EDGE ( 'NONE', *, *, #56716, .T. ) ;
#52970 = CARTESIAN_POINT ( 'NONE',  ( -0.6430446194225716283, -0.3690944881889763329, 0.3153832671262228327 ) ) ;
#52971 = CARTESIAN_POINT ( 'NONE',  ( -0.09186351706036663400, -0.4281496062992124485, 0.4176697321401328655 ) ) ;
#52972 = CARTESIAN_POINT ( 'NONE',  ( -1.424355216557543713, 1.172051041393591619, 0.3026866195246171176 ) ) ;
#52973 = CARTESIAN_POINT ( 'NONE',  ( -0.2493438320209966919, 0.05413385826771626580, -0.4176697321401330321 ) ) ;
#52974 = CARTESIAN_POINT ( 'NONE',  ( 0.1574803149606306130, -0.1870078740157479769, 0.4822834645669291653 ) ) ;
#52975 = CARTESIAN_POINT ( 'NONE',  ( -0.8005249343832011588, 0.05413385826771626580, -0.4176697321401330321 ) ) ;
#52976 = CARTESIAN_POINT ( 'NONE',  ( -1.154855643044618851, -0.6046776061558809534, -0.2411417322834644161 ) ) ;
#52977 = VECTOR ( 'NONE', #11356, 39.37007874015748143 ) ;
#52978 = CARTESIAN_POINT ( 'NONE',  ( 1.371391076115485941, 0.1771653543307087630, 0.09757992244046791164 ) ) ;
#52979 = DIRECTION ( 'NONE',  ( 0.000000000000000000, 0.000000000000000000, 1.000000000000000000 ) ) ;
#52980 = CARTESIAN_POINT ( 'NONE',  ( -0.1265901696524986964, -0.4724409448818899238, -2.749343832020996636 ) ) ;
#52981 = CARTESIAN_POINT ( 'NONE',  ( 0.8202099737532813073, 0.1771653543307087630, 0.09757992244046791164 ) ) ;
#52982 = CARTESIAN_POINT ( 'NONE',  ( 0.5643044619422579178, 0.05413385826771666132, 0.4176697321401328100 ) ) ;
#52983 = CARTESIAN_POINT ( 'NONE',  ( 0.4855643044619430415, -0.4281496062992127816, -0.4176697321401328100 ) ) ;
#52984 = CARTESIAN_POINT ( 'NONE',  ( 0.1070741851644053527, 0.3996062992125986590, -1.095800524934382958 ) ) ;
#52985 = CARTESIAN_POINT ( 'NONE',  ( -2.565525098582201124, 1.606100245667705373, 0.4697171261335973402 ) ) ;
#52986 = CARTESIAN_POINT ( 'NONE',  ( 0.2925321140481932369, 0.2925321140481932369, -0.6870078740157479213 ) ) ;
#52987 = CARTESIAN_POINT ( 'NONE',  ( -9.787531504996566615E-17, 0.3996062992125985480, -0.7066929133858268486 ) ) ;
#52988 = CARTESIAN_POINT ( 'NONE',  ( -0.3412073490813641308, -0.6046776061558807314, 0.2411417322834647770 ) ) ;
#52989 = CARTESIAN_POINT ( 'NONE',  ( 0.3460692066303959757, -0.1998031496062991907, -2.939632545931758489 ) ) ;
#52990 = CARTESIAN_POINT ( 'NONE',  ( -9.594673741351313045E-17, 0.3917322834645670104, -2.131889763779527769 ) ) ;
#52991 = CARTESIAN_POINT ( 'NONE',  ( -1.003937007874014853, 0.07958543189024085140, 0.2665933059059887866 ) ) ;
#52992 = CARTESIAN_POINT ( 'NONE',  ( 0.9317585301837276734, -0.4281496062992124485, 0.4176697321401328655 ) ) ;
#52993 = CARTESIAN_POINT ( 'NONE',  ( 0.9055118110236227702, 0.2952755905511811885, 0.000000000000000000 ) ) ;
#52994 = CARTESIAN_POINT ( 'NONE',  ( -0.2427821522309703550, -0.2845877964562159024, 0.3641732283464567677 ) ) ;
#52995 = CARTESIAN_POINT ( 'NONE',  ( 0.6758530183727039509, 0.2952755905511810774, -0.1292274648535930714 ) ) ;
#52996 = CARTESIAN_POINT ( 'NONE',  ( -0.1265901696524986964, -0.4724409448818899238, -1.723753280839894986 ) ) ;
#52997 = CARTESIAN_POINT ( 'NONE',  ( 0.07217847769028949700, -0.2845877964562159024, 0.3641732283464567677 ) ) ;
#52998 = CARTESIAN_POINT ( 'NONE',  ( -0.1837270341207343505, -0.6046776061558807314, 0.2411417322834647770 ) ) ;
#52999 = CARTESIAN_POINT ( 'NONE',  ( 0.3949938075777408852, 0.1058382717557500435, -1.303805774278215424 ) ) ;
#53000 = CARTESIAN_POINT ( 'NONE',  ( -1.476377952755905110, -0.5400638737290845981, -0.3530559997133363437 ) ) ;
#53001 = CARTESIAN_POINT ( 'NONE',  ( 0.3674540682414705883, 0.1283753931104746893, -0.1820866141732285504 ) ) ;
#53002 = CARTESIAN_POINT ( 'NONE',  ( 1.410761154855643795, -0.08942795157528024563, -0.3641732283464568787 ) ) ;
#53003 = CARTESIAN_POINT ( 'NONE',  ( -0.9186351706036736120, 0.2306618581243848609, 0.2411417322834645549 ) ) ;
#53004 = CARTESIAN_POINT ( 'NONE',  ( -0.6955380577427815458, -0.004921259842519576551, 0.3153832671262227771 ) ) ;
#53005 = CARTESIAN_POINT ( 'NONE',  ( -0.4724409448818899238, 0.1265901696524986964, -2.314304461942256808 ) ) ;
#53006 = CARTESIAN_POINT ( 'NONE',  ( -0.5839895013123351797, 0.2952755905511810774, -0.1292274648535930714 ) ) ;
#53007 = CARTESIAN_POINT ( 'NONE',  ( -0.5511811023622038563, -0.1870078740157479769, 0.4822834645669291653 ) ) ;
#53008 = CARTESIAN_POINT ( 'NONE',  ( -0.1574803149606292529, -0.1870078740157480879, -0.4822834645669291653 ) ) ;
#53009 = CARTESIAN_POINT ( 'NONE',  ( 0.3996062992125984925, 0.1070741851644054637, -2.721128608923884418 ) ) ;
#53010 =( BOUNDED_CURVE ( )  B_SPLINE_CURVE ( 1, ( #78798, #52671 ),
 .UNSPECIFIED., .F., .F. ) 
 B_SPLINE_CURVE_WITH_KNOTS ( ( 2, 2 ),
 ( 0.000000000000000000, 0.001849999999999999648 ),
 .UNSPECIFIED. ) 
 CURVE ( )  GEOMETRIC_REPRESENTATION_ITEM ( )  RATIONAL_B_SPLINE_CURVE ( ( 0.9911642120908024101, 0.9911642120908024101 ) ) 
 REPRESENTATION_ITEM ( '' )  );
#53011 = CARTESIAN_POINT ( 'NONE',  ( -0.1958661417322834497, -0.3392501089628018884, -1.877933440123672471 ) ) ;
#53012 = CARTESIAN_POINT ( 'NONE',  ( -0.5314960629921124946, 2.687524476698321507, -3.900447471620232864 ) ) ;
#53013 = CARTESIAN_POINT ( 'NONE',  ( 0.5511811023622055217, -0.1870078740157479769, 0.3641732283464567677 ) ) ;
#53014 = CARTESIAN_POINT ( 'NONE',  ( 1.200787401574803681, -0.5400638737290845981, -0.3530559997133363437 ) ) ;
#53015 = CARTESIAN_POINT ( 'NONE',  ( -1.345144356955379816, -0.08942795157528024563, -0.3641732283464568787 ) ) ;
#53016 = CARTESIAN_POINT ( 'NONE',  ( -1.259842519685038686, -0.1870078740157479769, 0.3641732283464567677 ) ) ;
#53017 = CARTESIAN_POINT ( 'NONE',  ( -0.6889763779527552368, -0.5400638737290845981, -0.3530559997133363437 ) ) ;
#53018 = CARTESIAN_POINT ( 'NONE',  ( 0.4133858267716541968, 0.07958543189024085140, 0.2665933059059887866 ) ) ;
#53019 = CARTESIAN_POINT ( 'NONE',  ( -0.2746814661183892281, 0.1088119808354341828, 5.842252906343563978 ) ) ;
#53020 = CARTESIAN_POINT ( 'NONE',  ( 1.194225721784777594, -0.3690944881889765550, -0.3153832671262227771 ) ) ;
#53021 = VECTOR ( 'NONE', #21122, 39.37007874015748143 ) ;
#53022 = CARTESIAN_POINT ( 'NONE',  ( 0.3937007874015754361, -0.1870078740157479769, 0.4822834645669291653 ) ) ;
#53023 = CARTESIAN_POINT ( 'NONE',  ( 6.265965269058076312E-17, 1.062992125984252745, -1.850393700787401619 ) ) ;
#53024 = EDGE_CURVE ( 'NONE', #8617, #1453, #14020, .T. ) ;
#53025 = CARTESIAN_POINT ( 'NONE',  ( -0.6758530183727028406, -0.6692913385826773087, -0.1292274648535924053 ) ) ;
#53026 = CARTESIAN_POINT ( 'NONE',  ( -0.1958661417322836718, 0.3392501089628017219, -1.515091863517060489 ) ) ;
#53027 = CARTESIAN_POINT ( 'NONE',  ( 1.430446194225722500, -0.004921259842519576551, 0.3153832671262227771 ) ) ;
#53028 = CARTESIAN_POINT ( 'NONE',  ( 0.5380577427821529035, -0.4281496062992124485, 0.4176697321401328655 ) ) ;
#53029 = CARTESIAN_POINT ( 'NONE',  ( 0.08530183727034192087, -0.05778040916215522460, 0.4822834645669289988 ) ) ;
#53030 = CARTESIAN_POINT ( 'NONE',  ( 8.195543980992789655E-16, -0.1870078740157480601, -0.3641732283464567677 ) ) ;
#53031 = DIRECTION ( 'NONE',  ( 1.000000000000000000, 0.000000000000000000, 0.000000000000000000 ) ) ;
#53032 = CARTESIAN_POINT ( 'NONE',  ( -0.2099737532808391705, 0.1283753931104748280, 0.1820866141732283561 ) ) ;
#53033 = CARTESIAN_POINT ( 'NONE',  ( 0.9383202099737538715, -0.05778040916215560624, -0.4822834645669293319 ) ) ;
#53034 = CARTESIAN_POINT ( 'NONE',  ( -0.8070866141732276899, -0.4536011799217367080, 0.2665933059059888421 ) ) ;
#53036 = CARTESIAN_POINT ( 'NONE',  ( 0.2925321140481932369, -0.2925321140481931814, -0.8051181102362205966 ) ) ;
#53035 = AXIS2_PLACEMENT_3D ( 'NONE', #39628, #52238, #26155 ) ;
#53037 = CARTESIAN_POINT ( 'NONE',  ( -0.9645669291338575535, 0.1660481256975883668, -0.3530559997133364547 ) ) ;
#53038 = CARTESIAN_POINT ( 'NONE',  ( -0.8542087009142328435, -4.039970415760091124E-15, 0.3627989612356165572 ) ) ;
#53039 = VERTEX_POINT ( 'NONE', #50866 ) ;
#53040 = CARTESIAN_POINT ( 'NONE',  ( -1.358267716535432434, -0.5400638737290844871, 0.3530559997133364547 ) ) ;
#53041 = CARTESIAN_POINT ( 'NONE',  ( -1.141732283464566011, -0.5511811023622047445, 6.969142054262312111E-17 ) ) ;
#53042 = CARTESIAN_POINT ( 'NONE',  ( -0.1574803149606292529, -0.1870078740157479769, 0.4822834645669291653 ) ) ;
#53043 = FACE_OUTER_BOUND ( 'NONE', #47806, .T. ) ;
#53044 = CARTESIAN_POINT ( 'NONE',  ( -0.8398950131233585692, 0.2306618581243848609, 0.2411417322834645549 ) ) ;
#53045 = CARTESIAN_POINT ( 'NONE',  ( -1.854472803289052507, 2.716535433070866645, 0.5314960629921260393 ) ) ;
#53047 = CARTESIAN_POINT ( 'NONE',  ( 0.7808398950131240079, -0.3162353388693405765, 0.4822834645669290543 ) ) ;
#53046 = CARTESIAN_POINT ( 'NONE',  ( -0.8761506516392493227, -2.567464376874931580E-15, -0.4445507791589072832 ) ) ;
#53048 = CARTESIAN_POINT ( 'NONE',  ( 0.9383202099737538715, -0.05778040916215560624, -0.4822834645669293319 ) ) ;
#53049 = CARTESIAN_POINT ( 'NONE',  ( -9.594673741351313045E-17, 0.3917322834645670104, -2.511811023622047223 ) ) ;
#53050 = CARTESIAN_POINT ( 'NONE',  ( 1.509186351706037543, -0.4281496062992127816, -0.4176697321401328100 ) ) ;
#53051 = CARTESIAN_POINT ( 'NONE',  ( -1.161417322834644716, -0.5400638737290845981, -0.3530559997133363437 ) ) ;
#53052 = CARTESIAN_POINT ( 'NONE',  ( -0.1070741851644056997, 0.3996062992125986035, -0.6364829396325458744 ) ) ;
#53053 = ORIENTED_EDGE ( 'NONE', *, *, #63775, .F. ) ;
#53054 = CARTESIAN_POINT ( 'NONE',  ( -0.6889763779527552368, 0.07958543189024085140, 0.2665933059059887866 ) ) ;
#53055 = CARTESIAN_POINT ( 'NONE',  ( -0.2867679344610364334, -0.2867679344610367109, -1.940944881889763884 ) ) ;
#53056 = EDGE_LOOP ( 'NONE', ( #1327, #58445 ) ) ;
#53057 = CARTESIAN_POINT ( 'NONE',  ( 0.3543307086614179147, 0.2952755905511811885, 0.000000000000000000 ) ) ;
#53058 = CARTESIAN_POINT ( 'NONE',  ( -0.06561679790026180015, -0.4281496062992127816, -0.4176697321401328100 ) ) ;
#53059 = CARTESIAN_POINT ( 'NONE',  ( -0.7939632545931750718, -0.05778040916215560624, -0.4822834645669293319 ) ) ;
#53060 = CARTESIAN_POINT ( 'NONE',  ( 1.601049868766404982, -0.6046776061558809534, -0.2411417322834644161 ) ) ;
#53061 = CARTESIAN_POINT ( 'NONE',  ( -0.8267716535433065062, 0.1771653543307087630, 0.000000000000000000 ) ) ;
#53062 = FACE_OUTER_BOUND ( 'NONE', #64869, .T. ) ;
#53063 = CARTESIAN_POINT ( 'NONE',  ( 0.6496062992125991586, -0.5400638737290845981, -0.3530559997133363437 ) ) ;
#53064 = EDGE_CURVE ( 'NONE', #51397, #10785, #18495, .T. ) ;
#53065 = CARTESIAN_POINT ( 'NONE',  ( 0.4921259842519691285, 0.07958543189024085140, 0.2665933059059887866 ) ) ;
#53066 = CARTESIAN_POINT ( 'NONE',  ( -0.4265091863517051496, -0.6692913385826771977, 0.1292274648535927661 ) ) ;
#53067 = CARTESIAN_POINT ( 'NONE',  ( 0.1958661417322834497, 0.3392501089628018329, -1.011791707840208332 ) ) ;
#53068 = CARTESIAN_POINT ( 'NONE',  ( -0.9645669291338575535, 0.1660481256975883668, -0.3530559997133364547 ) ) ;
#53069 = CARTESIAN_POINT ( 'NONE',  ( -1.679790026246718693, 0.1283753931104746893, -0.1820866141732285504 ) ) ;
#53070 = CARTESIAN_POINT ( 'NONE',  ( 1.541994750656168645, 0.2952755905511810774, -0.1292274648535930714 ) ) ;
#53071 = CARTESIAN_POINT ( 'NONE',  ( 0.000000000000000000, 2.559055118110236560, 0.000000000000000000 ) ) ;
#53072 = ORIENTED_EDGE ( 'NONE', *, *, #26135, .T. ) ;
#53073 = CARTESIAN_POINT ( 'NONE',  ( -9.594673741351313045E-17, 0.3917322834645670659, -2.673903830217533972 ) ) ;
#53074 = CARTESIAN_POINT ( 'NONE',  ( 0.07874015748031558404, -0.1870078740157479769, 0.4822834645669291653 ) ) ;
#53075 = ORIENTED_EDGE ( 'NONE', *, *, #46886, .F. ) ;
#53076 = CARTESIAN_POINT ( 'NONE',  ( -1.003937007874015297, -0.5400638737290845981, -0.3530559997133363437 ) ) ;
#53077 = CARTESIAN_POINT ( 'NONE',  ( 1.154855643044620184, 0.2306618581243847221, -0.2411417322834647770 ) ) ;
#53078 = CARTESIAN_POINT ( 'NONE',  ( 1.305774278215223960, 0.2952755905511810774, -0.1292274648535930714 ) ) ;
#53079 = CARTESIAN_POINT ( 'NONE',  ( 0.4396325459317590445, -0.6692913385826771977, 0.1292274648535927661 ) ) ;
#53080 = CARTESIAN_POINT ( 'NONE',  ( -0.1837270341207340729, 0.2306618581243847221, -0.2411417322834647770 ) ) ;
#53081 = CARTESIAN_POINT ( 'NONE',  ( -0.3917322834645671215, 0.1049643490035301469, -2.007217847769029007 ) ) ;
#53082 = CARTESIAN_POINT ( 'NONE',  ( -1.345144356955379816, -0.05778040916215560624, -0.4822834645669293319 ) ) ;
#53083 = CARTESIAN_POINT ( 'NONE',  ( -0.6889763779527552368, 0.1660481256975885056, 0.3530559997133364547 ) ) ;
#53084 = PRODUCT_DEFINITION_FORMATION_WITH_SPECIFIED_SOURCE ( 'ANY', '', #72209, .NOT_KNOWN. ) ;
#53085 = CARTESIAN_POINT ( 'NONE',  ( -0.6364829396325453192, -0.08942795157528024563, -0.3641732283464568787 ) ) ;
#53086 = CARTESIAN_POINT ( 'NONE',  ( -1.614173228346456712, 0.7166040191147899918, -0.1372047244094478091 ) ) ;
#53087 = CARTESIAN_POINT ( 'NONE',  ( -0.6364829396325453192, -0.3162353388693405765, 0.4822834645669290543 ) ) ;
#53088 = CARTESIAN_POINT ( 'NONE',  ( -1.192688228555125685, 0.02791078216816347476, -0.4328096321851898631 ) ) ;
#53089 = CARTESIAN_POINT ( 'NONE',  ( 0.6955380577427828781, 0.05413385826771626580, -0.4176697321401330321 ) ) ;
#53090 = CARTESIAN_POINT ( 'NONE',  ( -0.3996062992125987146, 0.1070741851644051862, -1.922572178477689908 ) ) ;
#53091 = CARTESIAN_POINT ( 'NONE',  ( 3.931468625396333572, 1.111233271792932520, -0.2107404457489559235 ) ) ;
#53092 = EDGE_CURVE ( 'NONE', #29367, #55042, #25200, .T. ) ;
#53093 =( BOUNDED_SURFACE ( )  B_SPLINE_SURFACE ( 1, 2, ( 
 ( #68295, #10632, #36287, #75023, #17771, #29963, #17369, #68692, #474, #13519, #64020, #6361, #70757, #32033, #24879, #25291, #58108, #11866, #19831, #18585, #50141, #19405, #38761, #37930, #37519, #50547, #56865, #64859, #82560, #39175, #43812, #13108, #45480, #63194, #31613, #51368, #63607, #51791, #24475, #45056, #26129, #44634, #58537, #76251, #69918, #25708, #5534, #12272, #57692, #31199, #75838, #7197, #77071, #64438, #6774, #50957, #44228, #32869, #5944, #18180, #69517, #12687, #32446, #57274, #82972, #76654, #18987, #38346, #70331, #54, #77495, #71177, #46742, #47153, #27809, #7631, #26969, #46323, #72844, #52634, #53469, #34126, #40440, #1320, #66120, #903, #40029, #61338, #78339, #42386, #23038, #45897, #59787, #29356, #33302, #41978, #8456, #3691, #74403, #2141, #79179, #16335, #21494, #20670, #1730, #55015, #14784, #67672, #10008, #35673, #72016, #48704, #16747, #68085, #14372, #71594, #80724, #65292, #10430, #36087, #26560, #52214, #65717, #8048, #27386, #33710, #59371, #53047, #77917, #20248, #78758, #58963, #13946, #21083, #39603, #72434, #18393, #29764, #82768, #49532, #12072, #68493, #69318, #11669, #4507, #75641, #12479, #76464, #74820, #44035, #24272, #24684, #5338, #10833, #30175, #23865, #50351, #55838, #30997, #37327, #17980, #62168, #43617, #61758, #17570, #37730, #81547, #18790, #25090, #23450, #62999, #5739, #36492, #69727, #56665, #63403, #50763, #82365, #76049, #31410, #57074, #75226, #62585, #44435, #70128, #4096, #55426, #81134, #43203, #49115, #17165, #42799, #68898, #11251, #36909, #4927, #30595, #56261, #81957, #49943, #32244, #45277, #38970, #70972, #64238, #57904, #59167, #52843, #13317, #44846, #20879, #19197, #52005, #78554, #78130, #6154, #1525, #25924, #71810, #70544, #45691, #71388, #14161, #25503, #33505, #269, #63815, #33085, #52420, #51582, #51169, #38558, #12899, #46531, #6573, #27179, #57489, #1114, #72231, #76865, #64653, #65077, #77284, #65506, #38143, #58752, #39817, #58326, #31828, #19615, #6991, #39393, #32659, #688, #13737, #26344, #83182, #77710, #7415, #26765, #20463, #20040, #46116, #7838, #60003, #8253, #80633, #2771, #15832, #28014, #3597, #40645, #73482, #41883, #46946, #54507, #22121, #73895, #29262, #54090, #79805, #60829, #47780, #14987, #15405, #67576, #28431, #41480, #9495, #48200, #66329, #61243, #54926, #22944, #53674, #1939, #67165, #78972, #80221, #48612, #9908, #14580, #8667, #21701, #41065, #47364, #34338, #2358, #35580, #40233, #73055, #21293, #65916, #72638, #35168, #33917, #22537, #59582, #27601, #79382, #16235, #66754, #3181, #28845, #53261, #9088, #34760, #60420, #16653, #69222, #5241, #4415, #61667, #74723, #23356, #31315, #49027, #63310, #10335, #37229, #11979, #4008, #81454, #17887, #30084, #18295, #74306, #11570, #50259, #11155, #24994, #17072, #36402, #75547, #29672, #62077, #81867, #55334, #42293, #5648, #43524, #62906, #30905, #17481, #42709, #56980, #55746, #67990, #82677, #62489, #56572, #23771, #35997, #68405, #10745, #4823, #81043, #49442, #75136, #82273, #36813, #24591, #75957, #43112, #68808, #30501, #43940, #56164, #69634, #24179, #49848, #37634, #32562, #50668, #6479, #26671, #51072, #7745, #71708, #12387, #32148, #78032, #76368, #71291, #52326, #70878, #1427, #76771, #12804, #51907, #6061, #38459, #58225, #63721, #18701, #65407, #77614, #45597, #13638, #77187, #19102, #33410, #64145, #44343, #59072, #38877, #19947, #57805, #39716, #44751, #70447, #64555, #70034, #38045, #31732, #32983, #13227, #39291, #64977, #57397, #171, #25824, #7314, #51484, #58651, #592, #6893, #19519, #26248, #83087, #45172, #20362, #1018, #25409, #14062, #46012, #2672, #54409, #59486, #67063, #34660, #3083, #16134, #66650, #8986, #73376, #60323, #27500, #27918, #80120, #40968, #53993, #22021, #60731, #53156, #73797, #41780, #67473, #40550, #14483, #28331, #8155, #9395, #9807, #22438, #61143, #21194, #34239, #53577, #59900, #78868, #46848, #48098, #35479, #2253, #33820, #27083, #1840, #79705, #52745, #35066, #78453, #20779, #14890, #28747, #72543, #47681, #15726, #46433, #40137, #72125 ),
 ( #65822, #41381, #66231, #8569, #79286, #21604, #47264, #72954, #15305, #24491, #18196, #36301, #10230, #69533, #67893, #17383, #43830, #43421, #54830, #50158, #74625, #37124, #35897, #11049, #36707, #62808, #74206, #82175, #80940, #29160, #81768, #17786, #16969, #16553, #3910, #61567, #11883, #29571, #75854, #22846, #49747, #37535, #42197, #10646, #30393, #42608, #30807, #3495, #24078, #5142, #23665, #80535, #55233, #48925, #4719, #23255, #68309, #62382, #61977, #48507, #4314, #56058, #75448, #69118, #29979, #55642, #81353, #49337, #75037, #43013, #68708, #11467, #56472, #52232, #5960, #31630, #77090, #13965, #77935, #76268, #45498, #25725, #26148, #6792, #69934, #57290, #25309, #51809, #82988, #32464, #13128, #19422, #63623, #45074, #63211, #19003, #39194, #50973, #20265, #922, #24895, #38779, #7216, #12290, #19849, #70777, #64877, #45915, #64456, #58126, #77514, #493, #76670, #64038, #32887, #71195, #13537, #58556, #26579, #44652, #71613, #5551, #31215, #70348, #50564, #56883, #44245, #82576, #18602, #37946, #12703, #38362, #6377, #32049, #57709, #71, #51385, #1337, #41287, #21927, #27826, #79196, #21512, #21100, #72033, #73282, #65733, #7650, #15630, #40458, #53486, #33727, #47588, #14389, #40047, #66137, #39621, #65311, #20688, #60228, #8475, #40871, #47170, #8066, #59389, #1747, #66553, #27404, #72862, #15211, #2160, #53065, #8886, #33320, #78776, #53896, #46759, #58982, #26987, #72452, #34563, #52651, #14801, #79610, #2578, #78356, #46339, #34144, #59805, #28237, #13396, #31907, #32321, #1194, #45355, #58409, #26430, #65163, #57568, #78211, #20543, #71890, #44927, #18867, #39049, #12560, #13817, #46195, #26843, #65587, #25582, #38636, #57983, #64314, #83260, #51246, #52502, #14241, #6648, #38218, #39899, #63893, #71052, #31489, #71469, #82849, #57150, #19275, #7499, #6231, #64734, #7072, #33168, #44516, #25170, #76948, #50839, #52081, #45770, #70624, #70203, #12980, #348, #76539, #26005, #51662, #77366, #77790, #19698, #32742, #768, #20123, #39476, #58836, #7920, #28509, #67241, #28095, #41959, #8331, #8744, #60906, #21778, #34836, #2845, #41553, #33997, #54587, #80297, #48271, #21371, #78633, #15484, #72310, #73560, #22611, #3258, #33581, #2015, #15065, #34415, #40721, #59659, #27679, #28919, #73969, #66407, #14657, #16314, #40314, #47440, #59244, #47855, #1603, #27259, #79054, #9572, #65993, #41141, #66831, #35242, #20957, #52919, #53344, #46615, #54166, #22198, #47026, #72718, #60083, #2437, #53751, #79461, #73134, #9164, #79881, #60496, #15904, #54601, #41155, #67665, #29350, #66843, #8345, #40736, #53358, #60098, #79893, #66420, #22625, #34432, #34011, #73572, #41565, #8756, #3271, #60920, #15078, #54180, #79475, #80310, #9177, #2452, #47868, #47039, #79068, #48285, #34848, #48698, #59673, #60511, #21384, #2028, #2859, #73982, #28110, #72732, #35256, #35667, #16328, #15917, #22211, #27694, #67254, #28523, #21791, #9587, #41972, #28932, #10002, #61331, #66007, #3685, #53764, #47454, #55009, #73148, #80717, #15497, #23032, #74396, #40328, #10423, #23859, #30989, #43197, #44027, #36081, #5331, #56657, #23444, #30588, #43609, #55420, #5731, #82358, #17564, #69720, #31402, #68892, #68079, #17159, #29757, #36486, #56254, #42792, #24676, #10826, #61752, #49936, #17972, #68487, #62992, #37320, #74814, #81950, #55832, #50344, #11242, #62161, #24263, #49108, #81127, #76041, #36902, #25082, #4089, #62578, #4502, #30169, #4920, #18386, #81540, #49526, #11661, #12064, #37722, #75634, #69311, #75219, #63396, #57067, #82761, #50756, #16740, #42380, #58318, #70965, #18783, #71801, #31821, #44427, #681, #32237, #14154, #70121, #262, #19607, #40953, #12472, #25915, #7408, #45269, #60309, #78122, #76857, #8970, #19189, #66633, #12892, #51574, #83175, #38551, #58745, #1107, #34644, #38134, #64231, #77277, #57481, #26758, #13730, #25495, #6565, #44838, #2658, #28317, #51161, #76456, #57895, #63808, #52413, #13310, #6147, #26337, #70536, #38962, #64646, #6983, #32652, #51998, #77703, #20033, #20455, #45684, #71380, #39384, #65069, #46108, #33078, #23239 ) ),
 .UNSPECIFIED., .F., .F., .F. ) 
 B_SPLINE_SURFACE_WITH_KNOTS ( ( 2, 2 ),
 ( 3, 2, 2, 2, 2, 2, 2, 2, 2, 2, 2, 2, 2, 2, 2, 2, 2, 2, 2, 2, 2, 2, 2, 2, 2, 2, 2, 2, 2, 2, 2, 2, 2, 2, 2, 2, 2, 2, 2, 2, 2, 2, 2, 2, 2, 2, 2, 2, 2, 2, 2, 2, 2, 2, 2, 2, 2, 2, 2, 2, 2, 2, 2, 2, 2, 2, 2, 2, 2, 2, 2, 2, 2, 2, 2, 2, 2, 2, 2, 2, 2, 2, 2, 2, 2, 2, 2, 2, 2, 2, 2, 2, 2, 2, 2, 2, 2, 2, 2, 2, 2, 2, 2, 2, 2, 2, 2, 2, 2, 2, 2, 2, 2, 2, 2, 2, 2, 2, 2, 2, 2, 2, 2, 2, 2, 2, 2, 2, 2, 2, 2, 2, 2, 2, 2, 2, 2, 2, 2, 2, 2, 2, 2, 2, 2, 2, 2, 2, 2, 2, 2, 2, 2, 2, 2, 2, 2, 2, 2, 2, 2, 2, 2, 2, 2, 2, 2, 2, 2, 2, 2, 2, 2, 2, 2, 2, 2, 2, 2, 2, 2, 2, 2, 2, 2, 2, 2, 2, 2, 2, 2, 2, 2, 2, 2, 2, 2, 2, 2, 2, 2, 2, 2, 2, 2, 2, 2, 2, 2, 2, 2, 2, 2, 2, 2, 2, 2, 2, 2, 2, 2, 2, 2, 2, 2, 2, 2, 2, 2, 2, 2, 2, 2, 2, 2, 2, 2, 2, 2, 2, 2, 2, 2, 2, 2, 2, 2, 2, 2, 2, 2, 2, 2, 2, 2, 3 ),
 ( 0.000000000000000000, 1.000000000000000000 ),
 ( 0.000000000000000000, 0.003787878787878787984, 0.007575757575757575968, 0.01136363636363636395, 0.01515151515151515194, 0.01893939393939393992, 0.02272727272727272790, 0.02651515151515151589, 0.03030303030303030387, 0.03409090909090908839, 0.03787878787878787984, 0.04166666666666666435, 0.04545454545454545581, 0.04924242424242424032, 0.05303030303030303177, 0.05681818181818181629, 0.06060606060606060774, 0.06439393939393939226, 0.06818181818181817677, 0.07196969696969697516, 0.07575757575757575968, 0.07954545454545454419, 0.08333333333333332871, 0.08712121212121212710, 0.09090909090909091161, 0.09469696969696969613, 0.09848484848484848064, 0.1022727272727272790, 0.1060606060606060635, 0.1098484848484848481, 0.1136363636363636326, 0.1174242424242424310, 0.1212121212121212155, 0.1250000000000000000, 0.1287878787878787845, 0.1325757575757575690, 0.1363636363636363535, 0.1401515151515151381, 0.1439393939393939503, 0.1477272727272727348, 0.1515151515151515194, 0.1553030303030303039, 0.1590909090909090884, 0.1628787878787878729, 0.1666666666666666574, 0.1704545454545454419, 0.1742424242424242542, 0.1780303030303030387, 0.1818181818181818232, 0.1856060606060606077, 0.1893939393939393923, 0.1931818181818181768, 0.1969696969696969613, 0.2007575757575757458, 0.2045454545454545581, 0.2083333333333333426, 0.2121212121212121271, 0.2159090909090909116, 0.2196969696969696961, 0.2234848484848484806, 0.2272727272727272652, 0.2310606060606060497, 0.2348484848484848619, 0.2386363636363636465, 0.2424242424242424310, 0.2462121212121212155, 0.2500000000000000000, 0.2537878787878787845, 0.2575757575757575690, 0.2613636363636363535, 0.2651515151515151381, 0.2689393939393939226, 0.2727272727272727071, 0.2765151515151514916, 0.2803030303030302761, 0.2840909090909091161, 0.2878787878787879007, 0.2916666666666666852, 0.2954545454545454697, 0.2992424242424242542, 0.3030303030303030387, 0.3068181818181818232, 0.3106060606060606077, 0.3143939393939393923, 0.3181818181818181768, 0.3219696969696969613, 0.3257575757575757458, 0.3295454545454545303, 0.3333333333333333148, 0.3371212121212120993, 0.3409090909090908839, 0.3446969696969697239, 0.3484848484848485084, 0.3522727272727272929, 0.3560606060606060774, 0.3598484848484848619, 0.3636363636363636465, 0.3674242424242424310, 0.3712121212121212155, 0.3750000000000000000, 0.3787878787878787845, 0.3825757575757575690, 0.3863636363636363535, 0.3901515151515151381, 0.3939393939393939226, 0.3977272727272727071, 0.4015151515151514916, 0.4053030303030302761, 0.4090909090909091161, 0.4128787878787879007, 0.4166666666666666852, 0.4204545454545454697, 0.4242424242424242542, 0.4280303030303030387, 0.4318181818181818232, 0.4356060606060606077, 0.4393939393939393923, 0.4431818181818181768, 0.4469696969696969613, 0.4507575757575757458, 0.4545454545454545303, 0.4583333333333333148, 0.4621212121212120993, 0.4659090909090908839, 0.4696969696969697239, 0.4734848484848485084, 0.4772727272727272929, 0.4810606060606060774, 0.4848484848484848619, 0.4886363636363636465, 0.4924242424242424310, 0.4962121212121212155, 0.5000000000000000000, 0.5037878787878787845, 0.5075757575757575690, 0.5113636363636363535, 0.5151515151515151381, 0.5189393939393939226, 0.5227272727272727071, 0.5265151515151514916, 0.5303030303030302761, 0.5340909090909090606, 0.5378787878787878451, 0.5416666666666666297, 0.5454545454545454142, 0.5492424242424241987, 0.5530303030303029832, 0.5568181818181817677, 0.5606060606060605522, 0.5643939393939394478, 0.5681818181818182323, 0.5719696969696970168, 0.5757575757575758013, 0.5795454545454545858, 0.5833333333333333703, 0.5871212121212121549, 0.5909090909090909394, 0.5946969696969697239, 0.5984848484848485084, 0.6022727272727272929, 0.6060606060606060774, 0.6098484848484848619, 0.6136363636363636465, 0.6174242424242424310, 0.6212121212121212155, 0.6250000000000000000, 0.6287878787878787845, 0.6325757575757575690, 0.6363636363636363535, 0.6401515151515151381, 0.6439393939393939226, 0.6477272727272727071, 0.6515151515151514916, 0.6553030303030302761, 0.6590909090909090606, 0.6628787878787878451, 0.6666666666666666297, 0.6704545454545454142, 0.6742424242424241987, 0.6780303030303029832, 0.6818181818181817677, 0.6856060606060605522, 0.6893939393939394478, 0.6931818181818182323, 0.6969696969696970168, 0.7007575757575758013, 0.7045454545454545858, 0.7083333333333333703, 0.7121212121212121549, 0.7159090909090909394, 0.7196969696969697239, 0.7234848484848485084, 0.7272727272727272929, 0.7310606060606060774, 0.7348484848484848619, 0.7386363636363636465, 0.7424242424242424310, 0.7462121212121212155, 0.7500000000000000000, 0.7537878787878787845, 0.7575757575757575690, 0.7613636363636363535, 0.7651515151515151381, 0.7689393939393939226, 0.7727272727272727071, 0.7765151515151514916, 0.7803030303030302761, 0.7840909090909090606, 0.7878787878787878451, 0.7916666666666666297, 0.7954545454545454142, 0.7992424242424241987, 0.8030303030303029832, 0.8068181818181817677, 0.8106060606060605522, 0.8143939393939394478, 0.8181818181818182323, 0.8219696969696970168, 0.8257575757575758013, 0.8295454545454545858, 0.8333333333333333703, 0.8371212121212121549, 0.8409090909090909394, 0.8446969696969697239, 0.8484848484848485084, 0.8522727272727272929, 0.8560606060606060774, 0.8598484848484848619, 0.8636363636363636465, 0.8674242424242424310, 0.8712121212121212155, 0.8750000000000000000, 0.8787878787878787845, 0.8825757575757575690, 0.8863636363636363535, 0.8901515151515151381, 0.8939393939393939226, 0.8977272727272727071, 0.9015151515151514916, 0.9053030303030302761, 0.9090909090909090606, 0.9128787878787878451, 0.9166666666666666297, 0.9204545454545454142, 0.9242424242424241987, 0.9280303030303029832, 0.9318181818181817677, 0.9356060606060605522, 0.9393939393939394478, 0.9431818181818182323, 0.9469696969696970168, 0.9507575757575758013, 0.9545454545454545858, 0.9583333333333333703, 0.9621212121212121549, 0.9659090909090909394 ),
 .UNSPECIFIED. ) 
 GEOMETRIC_REPRESENTATION_ITEM ( )  RATIONAL_B_SPLINE_SURFACE ( (
 ( 1.000000000000000000, 0.9659258262890683122, 1.000000000000000000, 0.9659258262890683122, 1.000000000000000000, 0.9659258262890683122, 1.000000000000000000, 0.9659258262890683122, 1.000000000000000000, 0.9659258262890683122, 1.000000000000000000, 0.9659258262890683122, 1.000000000000000000, 0.9659258262890683122, 1.000000000000000000, 0.9659258262890683122, 1.000000000000000000, 0.9659258262890683122, 1.000000000000000000, 0.9659258262890683122, 1.000000000000000000, 0.9659258262890683122, 1.000000000000000000, 0.9659258262890683122, 1.000000000000000000, 0.9659258262890683122, 1.000000000000000000, 0.9659258262890683122, 1.000000000000000000, 0.9659258262890683122, 1.000000000000000000, 0.9659258262890683122, 1.000000000000000000, 0.9659258262890683122, 1.000000000000000000, 0.9659258262890683122, 1.000000000000000000, 0.9659258262890683122, 1.000000000000000000, 0.9659258262890683122, 1.000000000000000000, 0.9659258262890683122, 1.000000000000000000, 0.9659258262890683122, 1.000000000000000000, 0.9659258262890683122, 1.000000000000000000, 0.9659258262890683122, 1.000000000000000000, 0.9659258262890683122, 1.000000000000000000, 0.9659258262890683122, 1.000000000000000000, 0.9659258262890683122, 1.000000000000000000, 0.9659258262890683122, 1.000000000000000000, 0.9659258262890683122, 1.000000000000000000, 0.9659258262890683122, 1.000000000000000000, 0.9659258262890683122, 1.000000000000000000, 0.9659258262890683122, 1.000000000000000000, 0.9659258262890683122, 1.000000000000000000, 0.9659258262890683122, 1.000000000000000000, 0.9659258262890683122, 1.000000000000000000, 0.9659258262890683122, 1.000000000000000000, 0.9659258262890683122, 1.000000000000000000, 0.9659258262890683122, 1.000000000000000000, 0.9659258262890683122, 1.000000000000000000, 0.9659258262890683122, 1.000000000000000000, 0.9659258262890683122, 1.000000000000000000, 0.9659258262890683122, 1.000000000000000000, 0.9659258262890683122, 1.000000000000000000, 0.9659258262890683122, 1.000000000000000000, 0.9659258262890683122, 1.000000000000000000, 0.9659258262890683122, 1.000000000000000000, 0.9659258262890683122, 1.000000000000000000, 0.9659258262890683122, 1.000000000000000000, 0.9659258262890683122, 1.000000000000000000, 0.9659258262890683122, 1.000000000000000000, 0.9659258262890683122, 1.000000000000000000, 0.9659258262890683122, 1.000000000000000000, 0.9659258262890683122, 1.000000000000000000, 0.9659258262890683122, 1.000000000000000000, 0.9659258262890683122, 1.000000000000000000, 0.9659258262890683122, 1.000000000000000000, 0.9659258262890683122, 1.000000000000000000, 0.9659258262890683122, 1.000000000000000000, 0.9659258262890683122, 1.000000000000000000, 0.9659258262890683122, 1.000000000000000000, 0.9659258262890683122, 1.000000000000000000, 0.9659258262890683122, 1.000000000000000000, 0.9659258262890683122, 1.000000000000000000, 0.9659258262890683122, 1.000000000000000000, 0.9659258262890683122, 1.000000000000000000, 0.9659258262890683122, 1.000000000000000000, 0.9659258262890683122, 1.000000000000000000, 0.9659258262890683122, 1.000000000000000000, 0.9659258262890683122, 1.000000000000000000, 0.9659258262890683122, 1.000000000000000000, 0.9659258262890683122, 1.000000000000000000, 0.9659258262890683122, 1.000000000000000000, 0.9659258262890683122, 1.000000000000000000, 0.9659258262890683122, 1.000000000000000000, 0.9659258262890683122, 1.000000000000000000, 0.9659258262890683122, 1.000000000000000000, 0.9659258262890683122, 1.000000000000000000, 0.9659258262890683122, 1.000000000000000000, 0.9659258262890683122, 1.000000000000000000, 0.9659258262890683122, 1.000000000000000000, 0.9659258262890683122, 1.000000000000000000, 0.9659258262890683122, 1.000000000000000000, 0.9659258262890683122, 1.000000000000000000, 0.9659258262890683122, 1.000000000000000000, 0.9659258262890683122, 1.000000000000000000, 0.9659258262890683122, 1.000000000000000000, 0.9659258262890683122, 1.000000000000000000, 0.9659258262890683122, 1.000000000000000000, 0.9659258262890683122, 1.000000000000000000, 0.9659258262890683122, 1.000000000000000000, 0.9659258262890683122, 1.000000000000000000, 0.9659258262890683122, 1.000000000000000000, 0.9659258262890683122, 1.000000000000000000, 0.9659258262890683122, 1.000000000000000000, 0.9659258262890683122, 1.000000000000000000, 0.9659258262890683122, 1.000000000000000000, 0.9659258262890683122, 1.000000000000000000, 0.9659258262890683122, 1.000000000000000000, 0.9659258262890683122, 1.000000000000000000, 0.9659258262890683122, 1.000000000000000000, 0.9659258262890683122, 1.000000000000000000, 0.9659258262890683122, 1.000000000000000000, 0.9659258262890683122, 1.000000000000000000, 0.9659258262890683122, 1.000000000000000000, 0.9659258262890683122, 1.000000000000000000, 0.9659258262890683122, 1.000000000000000000, 0.9659258262890683122, 1.000000000000000000, 0.9659258262890683122, 1.000000000000000000, 0.9659258262890683122, 1.000000000000000000, 0.9659258262890683122, 1.000000000000000000, 0.9659258262890683122, 1.000000000000000000, 0.9659258262890683122, 1.000000000000000000, 0.9659258262890683122, 1.000000000000000000, 0.9659258262890683122, 1.000000000000000000, 0.9659258262890683122, 1.000000000000000000, 0.9659258262890683122, 1.000000000000000000, 0.9659258262890683122, 1.000000000000000000, 0.9659258262890683122, 1.000000000000000000, 0.9659258262890683122, 1.000000000000000000, 0.9659258262890683122, 1.000000000000000000, 0.9659258262890683122, 1.000000000000000000, 0.9659258262890683122, 1.000000000000000000, 0.9659258262890683122, 1.000000000000000000, 0.9659258262890683122, 1.000000000000000000, 0.9659258262890683122, 1.000000000000000000, 0.9659258262890683122, 1.000000000000000000, 0.9659258262890683122, 1.000000000000000000, 0.9659258262890683122, 1.000000000000000000, 0.9659258262890683122, 1.000000000000000000, 0.9659258262890683122, 1.000000000000000000, 0.9659258262890683122, 1.000000000000000000, 0.9659258262890683122, 1.000000000000000000, 0.9659258262890683122, 1.000000000000000000, 0.9659258262890683122, 1.000000000000000000, 0.9659258262890683122, 1.000000000000000000, 0.9659258262890683122, 1.000000000000000000, 0.9659258262890683122, 1.000000000000000000, 0.9659258262890683122, 1.000000000000000000, 0.9659258262890683122, 1.000000000000000000, 0.9659258262890683122, 1.000000000000000000, 0.9659258262890683122, 1.000000000000000000, 0.9659258262890683122, 1.000000000000000000, 0.9659258262890683122, 1.000000000000000000, 0.9659258262890683122, 1.000000000000000000, 0.9659258262890683122, 1.000000000000000000, 0.9659258262890683122, 1.000000000000000000, 0.9659258262890683122, 1.000000000000000000, 0.9659258262890683122, 1.000000000000000000, 0.9659258262890683122, 1.000000000000000000, 0.9659258262890683122, 1.000000000000000000, 0.9659258262890683122, 1.000000000000000000, 0.9659258262890683122, 1.000000000000000000, 0.9659258262890683122, 1.000000000000000000, 0.9659258262890683122, 1.000000000000000000, 0.9659258262890683122, 1.000000000000000000, 0.9659258262890683122, 1.000000000000000000, 0.9659258262890683122, 1.000000000000000000, 0.9659258262890683122, 1.000000000000000000, 0.9659258262890683122, 1.000000000000000000, 0.9659258262890683122, 1.000000000000000000, 0.9659258262890683122, 1.000000000000000000, 0.9659258262890683122, 1.000000000000000000, 0.9659258262890683122, 1.000000000000000000, 0.9659258262890683122, 1.000000000000000000, 0.9659258262890683122, 1.000000000000000000, 0.9659258262890683122, 1.000000000000000000, 0.9659258262890683122, 1.000000000000000000, 0.9659258262890683122, 1.000000000000000000, 0.9659258262890683122, 1.000000000000000000, 0.9659258262890683122, 1.000000000000000000, 0.9659258262890683122, 1.000000000000000000, 0.9659258262890683122, 1.000000000000000000, 0.9659258262890683122, 1.000000000000000000, 0.9659258262890683122, 1.000000000000000000, 0.9659258262890683122, 1.000000000000000000, 0.9659258262890683122, 1.000000000000000000, 0.9659258262890683122, 1.000000000000000000, 0.9659258262890683122, 1.000000000000000000, 0.9659258262890683122, 1.000000000000000000, 0.9659258262890683122, 1.000000000000000000, 0.9659258262890683122, 1.000000000000000000, 0.9659258262890683122, 1.000000000000000000, 0.9659258262890683122, 1.000000000000000000, 0.9659258262890683122, 1.000000000000000000, 0.9659258262890683122, 1.000000000000000000, 0.9659258262890683122, 1.000000000000000000, 0.9659258262890683122, 1.000000000000000000, 0.9659258262890683122, 1.000000000000000000, 0.9659258262890683122, 1.000000000000000000, 0.9659258262890683122, 1.000000000000000000, 0.9659258262890683122, 1.000000000000000000, 0.9659258262890683122, 1.000000000000000000, 0.9659258262890683122, 1.000000000000000000, 0.9659258262890683122, 1.000000000000000000, 0.9659258262890683122, 1.000000000000000000, 0.9659258262890683122, 1.000000000000000000, 0.9659258262890683122, 1.000000000000000000, 0.9659258262890683122, 1.000000000000000000, 0.9659258262890683122, 1.000000000000000000, 0.9659258262890683122, 1.000000000000000000, 0.9659258262890683122, 1.000000000000000000, 0.9659258262890683122, 1.000000000000000000, 0.9659258262890683122, 1.000000000000000000, 0.9659258262890683122, 1.000000000000000000, 0.9659258262890683122, 1.000000000000000000, 0.9659258262890683122, 1.000000000000000000, 0.9659258262890683122, 1.000000000000000000, 0.9659258262890683122, 1.000000000000000000, 0.9659258262890683122, 1.000000000000000000, 0.9659258262890683122, 1.000000000000000000, 0.9659258262890683122, 1.000000000000000000, 0.9659258262890683122, 1.000000000000000000, 0.9659258262890683122, 1.000000000000000000, 0.9659258262890683122, 1.000000000000000000, 0.9659258262890683122, 1.000000000000000000, 0.9659258262890683122, 1.000000000000000000, 0.9659258262890683122, 1.000000000000000000, 0.9659258262890683122, 1.000000000000000000, 0.9659258262890683122, 1.000000000000000000, 0.9659258262890683122, 1.000000000000000000, 0.9659258262890683122, 1.000000000000000000, 0.9659258262890683122, 1.000000000000000000, 0.9659258262890683122, 1.000000000000000000, 0.9659258262890683122, 1.000000000000000000, 0.9659258262890683122, 1.000000000000000000, 0.9659258262890683122, 1.000000000000000000, 0.9659258262890683122, 1.000000000000000000, 0.9659258262890683122, 1.000000000000000000, 0.9659258262890683122, 1.000000000000000000, 0.9659258262890683122, 1.000000000000000000, 0.9659258262890683122, 1.000000000000000000, 0.9659258262890683122, 1.000000000000000000, 0.9659258262890683122, 1.000000000000000000, 0.9659258262890683122, 1.000000000000000000, 0.9659258262890683122, 1.000000000000000000, 0.9659258262890683122, 1.000000000000000000, 0.9659258262890683122, 1.000000000000000000, 0.9659258262890683122, 1.000000000000000000, 0.9659258262890683122, 1.000000000000000000, 0.9659258262890683122, 1.000000000000000000, 0.9659258262890683122, 1.000000000000000000, 0.9659258262890683122, 1.000000000000000000, 0.9659258262890683122, 1.000000000000000000, 0.9659258262890683122, 1.000000000000000000, 0.9659258262890683122, 1.000000000000000000, 0.9659258262890683122, 1.000000000000000000, 0.9659258262890683122, 1.000000000000000000, 0.9659258262890683122, 1.000000000000000000, 0.9659258262890683122, 1.000000000000000000, 0.9659258262890683122, 1.000000000000000000, 0.9659258262890683122, 1.000000000000000000, 0.9659258262890683122, 1.000000000000000000, 0.9659258262890683122, 1.000000000000000000, 0.9659258262890683122, 1.000000000000000000, 0.9659258262890683122, 1.000000000000000000),
 ( 1.000000000000000000, 0.9659258262890683122, 1.000000000000000000, 0.9659258262890683122, 1.000000000000000000, 0.9659258262890683122, 1.000000000000000000, 0.9659258262890683122, 1.000000000000000000, 0.9659258262890683122, 1.000000000000000000, 0.9659258262890683122, 1.000000000000000000, 0.9659258262890683122, 1.000000000000000000, 0.9659258262890683122, 1.000000000000000000, 0.9659258262890683122, 1.000000000000000000, 0.9659258262890683122, 1.000000000000000000, 0.9659258262890683122, 1.000000000000000000, 0.9659258262890683122, 1.000000000000000000, 0.9659258262890683122, 1.000000000000000000, 0.9659258262890683122, 1.000000000000000000, 0.9659258262890683122, 1.000000000000000000, 0.9659258262890683122, 1.000000000000000000, 0.9659258262890683122, 1.000000000000000000, 0.9659258262890683122, 1.000000000000000000, 0.9659258262890683122, 1.000000000000000000, 0.9659258262890683122, 1.000000000000000000, 0.9659258262890683122, 1.000000000000000000, 0.9659258262890683122, 1.000000000000000000, 0.9659258262890683122, 1.000000000000000000, 0.9659258262890683122, 1.000000000000000000, 0.9659258262890683122, 1.000000000000000000, 0.9659258262890683122, 1.000000000000000000, 0.9659258262890683122, 1.000000000000000000, 0.9659258262890683122, 1.000000000000000000, 0.9659258262890683122, 1.000000000000000000, 0.9659258262890683122, 1.000000000000000000, 0.9659258262890683122, 1.000000000000000000, 0.9659258262890683122, 1.000000000000000000, 0.9659258262890683122, 1.000000000000000000, 0.9659258262890683122, 1.000000000000000000, 0.9659258262890683122, 1.000000000000000000, 0.9659258262890683122, 1.000000000000000000, 0.9659258262890683122, 1.000000000000000000, 0.9659258262890683122, 1.000000000000000000, 0.9659258262890683122, 1.000000000000000000, 0.9659258262890683122, 1.000000000000000000, 0.9659258262890683122, 1.000000000000000000, 0.9659258262890683122, 1.000000000000000000, 0.9659258262890683122, 1.000000000000000000, 0.9659258262890683122, 1.000000000000000000, 0.9659258262890683122, 1.000000000000000000, 0.9659258262890683122, 1.000000000000000000, 0.9659258262890683122, 1.000000000000000000, 0.9659258262890683122, 1.000000000000000000, 0.9659258262890683122, 1.000000000000000000, 0.9659258262890683122, 1.000000000000000000, 0.9659258262890683122, 1.000000000000000000, 0.9659258262890683122, 1.000000000000000000, 0.9659258262890683122, 1.000000000000000000, 0.9659258262890683122, 1.000000000000000000, 0.9659258262890683122, 1.000000000000000000, 0.9659258262890683122, 1.000000000000000000, 0.9659258262890683122, 1.000000000000000000, 0.9659258262890683122, 1.000000000000000000, 0.9659258262890683122, 1.000000000000000000, 0.9659258262890683122, 1.000000000000000000, 0.9659258262890683122, 1.000000000000000000, 0.9659258262890683122, 1.000000000000000000, 0.9659258262890683122, 1.000000000000000000, 0.9659258262890683122, 1.000000000000000000, 0.9659258262890683122, 1.000000000000000000, 0.9659258262890683122, 1.000000000000000000, 0.9659258262890683122, 1.000000000000000000, 0.9659258262890683122, 1.000000000000000000, 0.9659258262890683122, 1.000000000000000000, 0.9659258262890683122, 1.000000000000000000, 0.9659258262890683122, 1.000000000000000000, 0.9659258262890683122, 1.000000000000000000, 0.9659258262890683122, 1.000000000000000000, 0.9659258262890683122, 1.000000000000000000, 0.9659258262890683122, 1.000000000000000000, 0.9659258262890683122, 1.000000000000000000, 0.9659258262890683122, 1.000000000000000000, 0.9659258262890683122, 1.000000000000000000, 0.9659258262890683122, 1.000000000000000000, 0.9659258262890683122, 1.000000000000000000, 0.9659258262890683122, 1.000000000000000000, 0.9659258262890683122, 1.000000000000000000, 0.9659258262890683122, 1.000000000000000000, 0.9659258262890683122, 1.000000000000000000, 0.9659258262890683122, 1.000000000000000000, 0.9659258262890683122, 1.000000000000000000, 0.9659258262890683122, 1.000000000000000000, 0.9659258262890683122, 1.000000000000000000, 0.9659258262890683122, 1.000000000000000000, 0.9659258262890683122, 1.000000000000000000, 0.9659258262890683122, 1.000000000000000000, 0.9659258262890683122, 1.000000000000000000, 0.9659258262890683122, 1.000000000000000000, 0.9659258262890683122, 1.000000000000000000, 0.9659258262890683122, 1.000000000000000000, 0.9659258262890683122, 1.000000000000000000, 0.9659258262890683122, 1.000000000000000000, 0.9659258262890683122, 1.000000000000000000, 0.9659258262890683122, 1.000000000000000000, 0.9659258262890683122, 1.000000000000000000, 0.9659258262890683122, 1.000000000000000000, 0.9659258262890683122, 1.000000000000000000, 0.9659258262890683122, 1.000000000000000000, 0.9659258262890683122, 1.000000000000000000, 0.9659258262890683122, 1.000000000000000000, 0.9659258262890683122, 1.000000000000000000, 0.9659258262890683122, 1.000000000000000000, 0.9659258262890683122, 1.000000000000000000, 0.9659258262890683122, 1.000000000000000000, 0.9659258262890683122, 1.000000000000000000, 0.9659258262890683122, 1.000000000000000000, 0.9659258262890683122, 1.000000000000000000, 0.9659258262890683122, 1.000000000000000000, 0.9659258262890683122, 1.000000000000000000, 0.9659258262890683122, 1.000000000000000000, 0.9659258262890683122, 1.000000000000000000, 0.9659258262890683122, 1.000000000000000000, 0.9659258262890683122, 1.000000000000000000, 0.9659258262890683122, 1.000000000000000000, 0.9659258262890683122, 1.000000000000000000, 0.9659258262890683122, 1.000000000000000000, 0.9659258262890683122, 1.000000000000000000, 0.9659258262890683122, 1.000000000000000000, 0.9659258262890683122, 1.000000000000000000, 0.9659258262890683122, 1.000000000000000000, 0.9659258262890683122, 1.000000000000000000, 0.9659258262890683122, 1.000000000000000000, 0.9659258262890683122, 1.000000000000000000, 0.9659258262890683122, 1.000000000000000000, 0.9659258262890683122, 1.000000000000000000, 0.9659258262890683122, 1.000000000000000000, 0.9659258262890683122, 1.000000000000000000, 0.9659258262890683122, 1.000000000000000000, 0.9659258262890683122, 1.000000000000000000, 0.9659258262890683122, 1.000000000000000000, 0.9659258262890683122, 1.000000000000000000, 0.9659258262890683122, 1.000000000000000000, 0.9659258262890683122, 1.000000000000000000, 0.9659258262890683122, 1.000000000000000000, 0.9659258262890683122, 1.000000000000000000, 0.9659258262890683122, 1.000000000000000000, 0.9659258262890683122, 1.000000000000000000, 0.9659258262890683122, 1.000000000000000000, 0.9659258262890683122, 1.000000000000000000, 0.9659258262890683122, 1.000000000000000000, 0.9659258262890683122, 1.000000000000000000, 0.9659258262890683122, 1.000000000000000000, 0.9659258262890683122, 1.000000000000000000, 0.9659258262890683122, 1.000000000000000000, 0.9659258262890683122, 1.000000000000000000, 0.9659258262890683122, 1.000000000000000000, 0.9659258262890683122, 1.000000000000000000, 0.9659258262890683122, 1.000000000000000000, 0.9659258262890683122, 1.000000000000000000, 0.9659258262890683122, 1.000000000000000000, 0.9659258262890683122, 1.000000000000000000, 0.9659258262890683122, 1.000000000000000000, 0.9659258262890683122, 1.000000000000000000, 0.9659258262890683122, 1.000000000000000000, 0.9659258262890683122, 1.000000000000000000, 0.9659258262890683122, 1.000000000000000000, 0.9659258262890683122, 1.000000000000000000, 0.9659258262890683122, 1.000000000000000000, 0.9659258262890683122, 1.000000000000000000, 0.9659258262890683122, 1.000000000000000000, 0.9659258262890683122, 1.000000000000000000, 0.9659258262890683122, 1.000000000000000000, 0.9659258262890683122, 1.000000000000000000, 0.9659258262890683122, 1.000000000000000000, 0.9659258262890683122, 1.000000000000000000, 0.9659258262890683122, 1.000000000000000000, 0.9659258262890683122, 1.000000000000000000, 0.9659258262890683122, 1.000000000000000000, 0.9659258262890683122, 1.000000000000000000, 0.9659258262890683122, 1.000000000000000000, 0.9659258262890683122, 1.000000000000000000, 0.9659258262890683122, 1.000000000000000000, 0.9659258262890683122, 1.000000000000000000, 0.9659258262890683122, 1.000000000000000000, 0.9659258262890683122, 1.000000000000000000, 0.9659258262890683122, 1.000000000000000000, 0.9659258262890683122, 1.000000000000000000, 0.9659258262890683122, 1.000000000000000000, 0.9659258262890683122, 1.000000000000000000, 0.9659258262890683122, 1.000000000000000000, 0.9659258262890683122, 1.000000000000000000, 0.9659258262890683122, 1.000000000000000000, 0.9659258262890683122, 1.000000000000000000, 0.9659258262890683122, 1.000000000000000000, 0.9659258262890683122, 1.000000000000000000, 0.9659258262890683122, 1.000000000000000000, 0.9659258262890683122, 1.000000000000000000, 0.9659258262890683122, 1.000000000000000000, 0.9659258262890683122, 1.000000000000000000, 0.9659258262890683122, 1.000000000000000000, 0.9659258262890683122, 1.000000000000000000, 0.9659258262890683122, 1.000000000000000000, 0.9659258262890683122, 1.000000000000000000, 0.9659258262890683122, 1.000000000000000000, 0.9659258262890683122, 1.000000000000000000, 0.9659258262890683122, 1.000000000000000000, 0.9659258262890683122, 1.000000000000000000, 0.9659258262890683122, 1.000000000000000000, 0.9659258262890683122, 1.000000000000000000, 0.9659258262890683122, 1.000000000000000000, 0.9659258262890683122, 1.000000000000000000, 0.9659258262890683122, 1.000000000000000000, 0.9659258262890683122, 1.000000000000000000, 0.9659258262890683122, 1.000000000000000000, 0.9659258262890683122, 1.000000000000000000, 0.9659258262890683122, 1.000000000000000000, 0.9659258262890683122, 1.000000000000000000, 0.9659258262890683122, 1.000000000000000000, 0.9659258262890683122, 1.000000000000000000, 0.9659258262890683122, 1.000000000000000000, 0.9659258262890683122, 1.000000000000000000, 0.9659258262890683122, 1.000000000000000000, 0.9659258262890683122, 1.000000000000000000, 0.9659258262890683122, 1.000000000000000000, 0.9659258262890683122, 1.000000000000000000, 0.9659258262890683122, 1.000000000000000000, 0.9659258262890683122, 1.000000000000000000, 0.9659258262890683122, 1.000000000000000000, 0.9659258262890683122, 1.000000000000000000, 0.9659258262890683122, 1.000000000000000000, 0.9659258262890683122, 1.000000000000000000, 0.9659258262890683122, 1.000000000000000000, 0.9659258262890683122, 1.000000000000000000, 0.9659258262890683122, 1.000000000000000000, 0.9659258262890683122, 1.000000000000000000, 0.9659258262890683122, 1.000000000000000000, 0.9659258262890683122, 1.000000000000000000, 0.9659258262890683122, 1.000000000000000000, 0.9659258262890683122, 1.000000000000000000, 0.9659258262890683122, 1.000000000000000000, 0.9659258262890683122, 1.000000000000000000, 0.9659258262890683122, 1.000000000000000000, 0.9659258262890683122, 1.000000000000000000, 0.9659258262890683122, 1.000000000000000000, 0.9659258262890683122, 1.000000000000000000, 0.9659258262890683122, 1.000000000000000000, 0.9659258262890683122, 1.000000000000000000, 0.9659258262890683122, 1.000000000000000000, 0.9659258262890683122, 1.000000000000000000, 0.9659258262890683122, 1.000000000000000000, 0.9659258262890683122, 1.000000000000000000, 0.9659258262890683122, 1.000000000000000000, 0.9659258262890683122, 1.000000000000000000, 0.9659258262890683122, 1.000000000000000000, 0.9659258262890683122, 1.000000000000000000, 0.9659258262890683122, 1.000000000000000000, 0.9659258262890683122, 1.000000000000000000, 0.9659258262890683122, 1.000000000000000000, 0.9659258262890683122, 1.000000000000000000, 0.9659258262890683122, 1.000000000000000000) ) ) 
 REPRESENTATION_ITEM ( '' )  SURFACE ( )  );
#53094 = CARTESIAN_POINT ( 'NONE',  ( -0.2887139107611542133, -0.6046776061558809534, -0.2411417322834644161 ) ) ;
#53096 = CARTESIAN_POINT ( 'NONE',  ( 0.6975637601868572846, -4.135162568743707313E-16, -0.3954985857520056380 ) ) ;
#53095 = CARTESIAN_POINT ( 'NONE',  ( 1.056430446194226658, 0.1771653543307087630, 0.09757992244046791164 ) ) ;
#53097 = CARTESIAN_POINT ( 'NONE',  ( -0.2362204724409447953, -0.4091458600556404646, -0.6148293963254594097 ) ) ;
#53098 = CARTESIAN_POINT ( 'NONE',  ( 1.213910761154856299, 0.1771653543307087630, 0.09757992244046791164 ) ) ;
#53099 = CARTESIAN_POINT ( 'NONE',  ( 1.102362204724410155, -0.1870078740157479769, 0.4822834645669291653 ) ) ;
#53100 = CIRCLE ( 'NONE', #15466, 0.5118110236220471121 ) ;
#53101 = CARTESIAN_POINT ( 'NONE',  ( -0.2891555358219909388, -0.2891555358219912164, -0.1358267716535433156 ) ) ;
#53102 = CARTESIAN_POINT ( 'NONE',  ( -0.01968503937007793844, -0.5400638737290844871, 0.3530559997133364547 ) ) ;
#53103 = DIRECTION ( 'NONE',  ( 0.000000000000000000, 0.000000000000000000, -1.000000000000000000 ) ) ;
#53104 = CARTESIAN_POINT ( 'NONE',  ( -1.463254593175852492, -0.6692913385826773087, -0.1292274648535924053 ) ) ;
#53105 = CARTESIAN_POINT ( 'NONE',  ( -0.2493438320209966919, 0.05413385826771626580, -0.4176697321401330321 ) ) ;
#53106 = CARTESIAN_POINT ( 'NONE',  ( 0.3949938075777409408, -0.1058382717557499186, -0.5032808398950131545 ) ) ;
#53107 = CARTESIAN_POINT ( 'NONE',  ( 1.174540682414699111, -0.3162353388693405765, 0.4822834645669290543 ) ) ;
#53108 = CARTESIAN_POINT ( 'NONE',  ( 0.5183727034120741983, 0.2952755905511810774, -0.1292274648535930714 ) ) ;
#53109 = CARTESIAN_POINT ( 'NONE',  ( 0.8595800524934390507, -0.2845877964562159024, 0.3641732283464567677 ) ) ;
#53110 = CARTESIAN_POINT ( 'NONE',  ( 1.192633591291867967, 1.535433070866141447, -0.5030666621580099918 ) ) ;
#53111 = CARTESIAN_POINT ( 'NONE',  ( 0.2559055118110243332, 0.07958543189024085140, 0.2665933059059887866 ) ) ;
#53112 = FACE_OUTER_BOUND ( 'NONE', #45286, .T. ) ;
#53113 = CARTESIAN_POINT ( 'NONE',  ( 0.1998031496062992463, 0.3460692066303959202, -1.166010498687663821 ) ) ;
#53114 = CARTESIAN_POINT ( 'NONE',  ( 0.9251968503937015864, 0.1660481256975883668, -0.3530559997133364547 ) ) ;
#53115 = CARTESIAN_POINT ( 'NONE',  ( -0.2867679344610364334, -0.2867679344610367109, -0.8385826771653541734 ) ) ;
#53117 = CARTESIAN_POINT ( 'NONE',  ( 0.8989501312335965721, 0.2952755905511811885, 0.1292274648535926551 ) ) ;
#53116 = CARTESIAN_POINT ( 'NONE',  ( 0.2362204724409456558, -0.1870078740157479769, 0.4822834645669291653 ) ) ;
#53118 = DIRECTION ( 'NONE',  ( 1.000000000000000000, 0.000000000000000000, 0.000000000000000000 ) ) ;
#53119 = CARTESIAN_POINT ( 'NONE',  ( 0.5446194225721792126, -0.08942795157528024563, -0.3641732283464568787 ) ) ;
#53120 = CARTESIAN_POINT ( 'NONE',  ( 0.3740157480314966754, -0.5400638737290844871, 0.3530559997133364547 ) ) ;
#53121 = CARTESIAN_POINT ( 'NONE',  ( -0.4670403427556097387, 1.622209144264169289, 2.152711368484138355 ) ) ;
#53122 = CARTESIAN_POINT ( 'NONE',  ( -1.030183727034119867, -0.08942795157528024563, -0.3641732283464568787 ) ) ;
#53123 = CARTESIAN_POINT ( 'NONE',  ( -0.8333333333333323711, -0.6692913385826773087, -0.1292274648535924053 ) ) ;
#53124 = CARTESIAN_POINT ( 'NONE',  ( -1.666666666666665853, 0.05413385826771626580, -0.4176697321401330321 ) ) ;
#53125 = CARTESIAN_POINT ( 'NONE',  ( 0.3674540682414705883, -0.6046776061558807314, 0.2411417322834647770 ) ) ;
#53126 = CARTESIAN_POINT ( 'NONE',  ( 1.482939632545932307, -0.4281496062992124485, 0.4176697321401328655 ) ) ;
#53127 = CARTESIAN_POINT ( 'NONE',  ( 0.4408028249046178626, -0.2072245076110159345, -0.1100941634872966285 ) ) ;
#53128 = CARTESIAN_POINT ( 'NONE',  ( 0.5183727034120741983, 0.2952755905511810774, -0.1292274648535930714 ) ) ;
#53129 = CARTESIAN_POINT ( 'NONE',  ( 0.4091458600556403535, 0.2362204724409449896, -2.727690288713910949 ) ) ;
#53130 = CARTESIAN_POINT ( 'NONE',  ( 0.4622690493055590655, 1.429647347090970522, 3.909775897616574181 ) ) ;
#53131 = CARTESIAN_POINT ( 'NONE',  ( 1.541994750656168645, 0.2952755905511810774, -0.1292274648535930714 ) ) ;
#53132 = CARTESIAN_POINT ( 'NONE',  ( -1.482939632545930975, -0.3690944881889765550, -0.3153832671262227771 ) ) ;
#53133 = CARTESIAN_POINT ( 'NONE',  ( 1.174540682414699111, -0.2845877964562159024, 0.3641732283464567677 ) ) ;
#53134 = CARTESIAN_POINT ( 'NONE',  ( -1.246719160104985846, -0.3690944881889765550, -0.3153832671262227771 ) ) ;
#53135 = CARTESIAN_POINT ( 'NONE',  ( -0.6758530183727028406, 0.1771653543307087630, 0.09757992244046791164 ) ) ;
#53136 = CARTESIAN_POINT ( 'NONE',  ( 1.561679790026247350, -0.4281496062992124485, 0.4176697321401328655 ) ) ;
#53137 = CARTESIAN_POINT ( 'NONE',  ( 0.7152230971128614723, -0.2845877964562161244, -0.3641732283464567121 ) ) ;
#53138 = CARTESIAN_POINT ( 'NONE',  ( 0.5052493438320218022, -0.6692913385826773087, -0.1292274648535924053 ) ) ;
#53139 = CARTESIAN_POINT ( 'NONE',  ( 1.259842519685040019, -0.1870078740157479769, 0.4822834645669291653 ) ) ;
#53140 = CARTESIAN_POINT ( 'NONE',  ( -0.006561679790025524116, -0.05778040916215560624, -0.4822834645669293319 ) ) ;
#53141 = CARTESIAN_POINT ( 'NONE',  ( 0.3280839895013130669, -0.004921259842519576551, 0.3153832671262227771 ) ) ;
#53142 = CARTESIAN_POINT ( 'NONE',  ( 1.358267716535433323, -0.5400638737290845981, -0.3530559997133363437 ) ) ;
#53143 = CARTESIAN_POINT ( 'NONE',  ( -0.1771653543307080136, 0.1012011053420775880, -0.2882089793578256898 ) ) ;
#53144 = CARTESIAN_POINT ( 'NONE',  ( -0.7611548556430438595, 0.2306618581243848609, 0.2411417322834645549 ) ) ;
#53145 = CARTESIAN_POINT ( 'NONE',  ( -0.2925321140481932369, 0.2925321140481931814, -0.9645669291338581086 ) ) ;
#53146 = CARTESIAN_POINT ( 'NONE',  ( 0.06632061457837788720, 2.409604939980833412E-17, -0.3464511005275205946 ) ) ;
#53148 = VECTOR ( 'NONE', #30116, 39.37007874015748854 ) ;
#53147 = CARTESIAN_POINT ( 'NONE',  ( -0.9973753280839886548, 0.2306618581243848609, 0.2411417322834645549 ) ) ;
#53149 = CARTESIAN_POINT ( 'NONE',  ( -0.1640419947506555343, -0.3162353388693405765, 0.4822834645669290543 ) ) ;
#53150 = CARTESIAN_POINT ( 'NONE',  ( -0.2925321140481932924, 0.2925321140481931814, -2.696850393700787052 ) ) ;
#53151 = CARTESIAN_POINT ( 'NONE',  ( 0.3949938075777409963, 2.418639510665530435E-17, -1.850393700787401396 ) ) ;
#53152 = CARTESIAN_POINT ( 'NONE',  ( -0.3917322834645670104, -7.196005306013484475E-17, -0.5039370078740157410 ) ) ;
#53153 = CARTESIAN_POINT ( 'NONE',  ( 3.831929248781927200, 2.755905511811024056, -0.5314960629921259283 ) ) ;
#53154 = CARTESIAN_POINT ( 'NONE',  ( -1.246719160104986512, -0.004921259842519576551, 0.3153832671262227771 ) ) ;
#53155 = CARTESIAN_POINT ( 'NONE',  ( -0.2867679344610364334, -0.2867679344610367109, -1.153543307086613900 ) ) ;
#53156 = CARTESIAN_POINT ( 'NONE',  ( -1.496062992125983815, -0.1870078740157480879, -0.4822834645669291653 ) ) ;
#53157 = B_SPLINE_CURVE_WITH_KNOTS ( 'NONE', 3,
 ( #36152, #69385, #11739, #5403 ),
 .UNSPECIFIED., .F., .F.,
 ( 4, 4 ),
 ( 2.453269466693398698E-18, 0.001494448006632143403 ),
 .UNSPECIFIED. ) ;
#53158 = CARTESIAN_POINT ( 'NONE',  ( 0.1958661417322836162, -0.3392501089628018329, -0.01441637975621864153 ) ) ;
#53159 = B_SPLINE_CURVE_WITH_KNOTS ( 'NONE', 3,
 ( #43379, #29939, #63583, #75000, #30353, #69495, #5105, #56022, #75814, #69079, #11430, #5917, #11844, #57246, #63172, #81730, #56433, #24449, #25268, #50934, #24855, #44611, #17346, #42974, #68670, #18157 ),
 .UNSPECIFIED., .F., .F.,
 ( 4, 2, 2, 2, 2, 2, 2, 2, 2, 2, 2, 2, 4 ),
 ( 0.000000000000000000, 0.002383650122917511851, 0.003575475184376268861, 0.004767300245835024569, 0.007150950368752538588, 0.008342775430211293863, 0.009534600491670042199, 0.01072642555312879054, 0.01191825061458753714, 0.01430190073750502340, 0.01549372579896377000, 0.01668555086042251834, 0.01906920098334001501 ),
 .UNSPECIFIED. ) ;
#53160 = CARTESIAN_POINT ( 'NONE',  ( 0.4921259842519691285, -0.5400638737290845981, -0.3530559997133363437 ) ) ;
#53161 = CARTESIAN_POINT ( 'NONE',  ( -0.3280839895013117347, -0.3690944881889763329, 0.3153832671262228327 ) ) ;
#53162 = CARTESIAN_POINT ( 'NONE',  ( 0.9973753280839902091, 0.2306618581243847221, -0.2411417322834647770 ) ) ;
#53163 = CARTESIAN_POINT ( 'NONE',  ( 0.5249343832021003964, 0.2306618581243847221, -0.2411417322834647770 ) ) ;
#53164 = CARTESIAN_POINT ( 'NONE',  ( 0.3466100433291510186, 1.213118387047130264, 1.067229880606827885 ) ) ;
#53165 = CARTESIAN_POINT ( 'NONE',  ( 0.3996062992125986035, 0.1070741851644054776, -2.486876640419947382 ) ) ;
#53166 = CARTESIAN_POINT ( 'NONE',  ( -0.2867679344610365444, -0.2867679344610367664, -1.000675483760841811 ) ) ;
#53167 = CARTESIAN_POINT ( 'NONE',  ( 1.187664041994751285, -0.05778040916215522460, 0.4822834645669289988 ) ) ;
#53168 = CARTESIAN_POINT ( 'NONE',  ( -0.1312335958005241554, 0.2306618581243848609, 0.2411417322834645549 ) ) ;
#53169 = CARTESIAN_POINT ( 'NONE',  ( 1.391076115485564868, -0.6046776061558807314, 0.2411417322834647770 ) ) ;
#53170 = CARTESIAN_POINT ( 'NONE',  ( 1.043307086614173818, 0.1660481256975885056, 0.3530559997133364547 ) ) ;
#53171 = CARTESIAN_POINT ( 'NONE',  ( -0.3392501089628019995, 0.1958661417322832277, -0.4258530183727035068 ) ) ;
#53172 = CARTESIAN_POINT ( 'NONE',  ( 0.1246719160104994284, -0.6692913385826771977, 0.1292274648535927661 ) ) ;
#53173 = CARTESIAN_POINT ( 'NONE',  ( 0.7874015748031503170, -0.1870078740157480879, -0.4822834645669291653 ) ) ;
#53174 = CARTESIAN_POINT ( 'NONE',  ( 0.05905511811023709395, -0.5400638737290844871, 0.3530559997133364547 ) ) ;
#53175 = CARTESIAN_POINT ( 'NONE',  ( 0.8333333333333340365, -0.5511811023622046335, 0.09757992244046803654 ) ) ;
#53176 = CARTESIAN_POINT ( 'NONE',  ( -1.332020997375327642, -0.3162353388693409650, -0.4822834645669289433 ) ) ;
#53177 = CARTESIAN_POINT ( 'NONE',  ( -1.568241469816272105, -0.05778040916215522460, 0.4822834645669289988 ) ) ;
#53178 = CARTESIAN_POINT ( 'NONE',  ( 0.8661417322834652488, -0.1870078740157480879, -0.4822834645669291653 ) ) ;
#53179 = CARTESIAN_POINT ( 'NONE',  ( -0.3401783215940975547, -0.1988659768061105948, -1.929133858267717105 ) ) ;
#53180 = CARTESIAN_POINT ( 'NONE',  ( 0.1049643490035304938, -0.3917322834645669549, -1.809711286089239035 ) ) ;
#53181 = ORIENTED_EDGE ( 'NONE', *, *, #23955, .T. ) ;
#53182 = CARTESIAN_POINT ( 'NONE',  ( -0.1998031496062991907, -0.3460692066303959757, -0.3805774278215223183 ) ) ;
#53183 = EDGE_LOOP ( 'NONE', ( #12595, #63521, #15551, #50473 ) ) ;
#53184 = CARTESIAN_POINT ( 'NONE',  ( 1.023622047244095334, -0.1870078740157479769, 0.4822834645669291653 ) ) ;
#53185 = CARTESIAN_POINT ( 'NONE',  ( 1.154855643044620184, 0.1283753931104746893, -0.1820866141732285504 ) ) ;
#53186 = VECTOR ( 'NONE', #79340, 39.37007874015748854 ) ;
#53187 = DIRECTION ( 'NONE',  ( 0.000000000000000000, 1.000000000000000000, -0.000000000000000000 ) ) ;
#53188 = EDGE_CURVE ( 'NONE', #64046, #41865, #69830, .T. ) ;
#53189 = CARTESIAN_POINT ( 'NONE',  ( 0.4091458600556404646, -0.2362204724409448231, -0.02427821522309711946 ) ) ;
#53190 = DIRECTION ( 'NONE',  ( 0.000000000000000000, 1.000000000000000000, -0.000000000000000000 ) ) ;
#53191 = CARTESIAN_POINT ( 'NONE',  ( 0.1049643490035304938, -0.3917322834645669549, -1.272309711286089273 ) ) ;
#53192 = CARTESIAN_POINT ( 'NONE',  ( 1.528871391076116026, -0.6692913385826773087, -0.1292274648535924053 ) ) ;
#53193 = CARTESIAN_POINT ( 'NONE',  ( -1.587926509186350810, 0.05413385826771626580, -0.4176697321401330321 ) ) ;
#53194 = CARTESIAN_POINT ( 'NONE',  ( -0.5249343832020990641, -0.6046776061558809534, -0.2411417322834644161 ) ) ;
#53195 = CARTESIAN_POINT ( 'NONE',  ( 1.266404199475066328, -0.05778040916215522460, 0.4822834645669289988 ) ) ;
#53196 = ORIENTED_EDGE ( 'NONE', *, *, #65648, .F. ) ;
#53197 = CARTESIAN_POINT ( 'NONE',  ( -1.397637795275589623, 0.1660481256975885056, 0.3530559997133364547 ) ) ;
#53198 = CARTESIAN_POINT ( 'NONE',  ( -1.084166635437626258, 1.161135222542148071, -0.2893535460047377272 ) ) ;
#53199 = CARTESIAN_POINT ( 'NONE',  ( 3.523619145740915393, 3.916330350904249524, 8.335517803990978081 ) ) ;
#53200 = CARTESIAN_POINT ( 'NONE',  ( 1.496062992125985147, -0.1870078740157479769, 0.3641732283464567677 ) ) ;
#53201 = CARTESIAN_POINT ( 'NONE',  ( -0.3034644639079859818, -2.551093532135090261E-15, 0.3791475997938242304 ) ) ;
#53202 = CARTESIAN_POINT ( 'NONE',  ( -0.8398950131233585692, 0.1283753931104748280, 0.1820866141732283561 ) ) ;
#53203 = CARTESIAN_POINT ( 'NONE',  ( -1.384514435695537005, -0.6692913385826773087, -0.1292274648535924053 ) ) ;
#53204 = CARTESIAN_POINT ( 'NONE',  ( 0.4330708661417329575, 0.2952755905511811885, 0.000000000000000000 ) ) ;
#53205 = AXIS2_PLACEMENT_3D ( 'NONE', #29603, #16583, #80153 ) ;
#53206 = ORIENTED_EDGE ( 'NONE', *, *, #29099, .F. ) ;
#53208 = CARTESIAN_POINT ( 'NONE',  ( 0.1181102362204724532, 0.09842519685039373412, 4.268512490100411895E-17 ) ) ;
#53207 = CARTESIAN_POINT ( 'NONE',  ( 1.456692913385827515, -0.6692913385826771977, 8.415575281601705876E-17 ) ) ;
#53209 = EDGE_CURVE ( 'NONE', #30609, #51397, #63731, .T. ) ;
#53210 = CARTESIAN_POINT ( 'NONE',  ( -0.6233595800524928121, -0.08942795157527998196, 0.3641732283464567121 ) ) ;
#53211 = CARTESIAN_POINT ( 'NONE',  ( 0.8661417322834653598, -0.1870078740157479769, 0.4822834645669291653 ) ) ;
#53212 = CARTESIAN_POINT ( 'NONE',  ( -1.732283464566928277, -0.1870078740157479769, 0.4822834645669291653 ) ) ;
#53213 = CARTESIAN_POINT ( 'NONE',  ( -0.3392501089628019439, 0.1958661417322832554, -1.208642101540995606 ) ) ;
#53214 = CARTESIAN_POINT ( 'NONE',  ( -0.7939632545931754048, -0.2845877964562159024, 0.3641732283464567677 ) ) ;
#53215 = CARTESIAN_POINT ( 'NONE',  ( 1.692913385826772421, 0.2952755905511811885, 0.000000000000000000 ) ) ;
#53216 = LINE ( 'NONE', #71765, #31683 ) ;
#53218 = EDGE_CURVE ( 'NONE', #53039, #17115, #36594, .T. ) ;
#53217 = CARTESIAN_POINT ( 'NONE',  ( 0.5577427821522314977, -0.3162353388693409650, -0.4822834645669289433 ) ) ;
#53219 = CARTESIAN_POINT ( 'NONE',  ( -0.7217847769028863381, -0.3690944881889763329, 0.3153832671262228327 ) ) ;
#53220 = CARTESIAN_POINT ( 'NONE',  ( -0.5052493438320203589, -0.5511811023622046335, 0.09757992244046803654 ) ) ;
#53221 = CARTESIAN_POINT ( 'NONE',  ( -0.2559055118110230564, 0.1660481256975883668, -0.3530559997133364547 ) ) ;
#53222 = CARTESIAN_POINT ( 'NONE',  ( 1.633858267716535639, -0.5400638737290844871, 0.3530559997133364547 ) ) ;
#53223 = CARTESIAN_POINT ( 'NONE',  ( -0.1958661417322833942, -0.3392501089628018884, -0.2198355887477184134 ) ) ;
#53224 = CARTESIAN_POINT ( 'NONE',  ( 0.5774278215223103139, -0.6046776061558809534, -0.2411417322834644161 ) ) ;
#53225 = CARTESIAN_POINT ( 'NONE',  ( -0.4724409448818898682, -8.678599364036362592E-17, -0.5885826771653542844 ) ) ;
#53226 = CARTESIAN_POINT ( 'NONE',  ( -0.3458507752293909498, 0.3458507752293907833, -1.828740157480315265 ) ) ;
#53227 = CARTESIAN_POINT ( 'NONE',  ( -0.9711286089238838626, -0.6046776061558807314, 0.2411417322834647770 ) ) ;
#53228 = CARTESIAN_POINT ( 'NONE',  ( -0.1968503937007867743, -0.5511811023622047445, 6.969142054262312111E-17 ) ) ;
#53229 = CARTESIAN_POINT ( 'NONE',  ( -1.371391076115484609, -0.6692913385826771977, 0.1292274648535927661 ) ) ;
#53230 = CARTESIAN_POINT ( 'NONE',  ( 0.4396325459317593221, 0.1771653543307087075, -0.09757992244046823083 ) ) ;
#53231 = CARTESIAN_POINT ( 'NONE',  ( -0.5643044619422565855, -0.004921259842519870586, -0.3153832671262229437 ) ) ;
#53232 = CARTESIAN_POINT ( 'NONE',  ( -1.148293963254592542, -0.6692913385826773087, -0.1292274648535924053 ) ) ;
#53233 = CARTESIAN_POINT ( 'NONE',  ( -1.581364829396324945, -0.3162353388693405765, 0.4822834645669290543 ) ) ;
#53234 = CARTESIAN_POINT ( 'NONE',  ( 1.607611548556431069, -0.6692913385826773087, -0.1292274648535924053 ) ) ;
#53235 = DIRECTION ( 'NONE',  ( 0.000000000000000000, -1.000000000000000000, 0.000000000000000000 ) ) ;
#53236 = CARTESIAN_POINT ( 'NONE',  ( 1.017060367454068803, -0.2845877964562159024, 0.3641732283464567677 ) ) ;
#53237 = CARTESIAN_POINT ( 'NONE',  ( 0.3215223097112867578, -0.3162353388693409650, -0.4822834645669289433 ) ) ;
#53238 = CARTESIAN_POINT ( 'NONE',  ( -1.358267716535432434, -0.5400638737290844871, 0.3530559997133364547 ) ) ;
#53239 = CARTESIAN_POINT ( 'NONE',  ( 1.233595800524935227, -0.5023911411419708095, 0.1820866141732285504 ) ) ;
#53240 = ORIENTED_EDGE ( 'NONE', *, *, #26035, .T. ) ;
#53241 = EDGE_CURVE ( 'NONE', #13252, #59983, #24790, .T. ) ;
#53242 = CARTESIAN_POINT ( 'NONE',  ( 0.1998031496062992463, 0.3460692066303959202, -2.740813648293963567 ) ) ;
#53243 = CARTESIAN_POINT ( 'NONE',  ( -1.272965879265091305, -0.004921259842519870586, -0.3153832671262229437 ) ) ;
#53244 = CARTESIAN_POINT ( 'NONE',  ( -0.6824146981627288167, 0.2306618581243848609, 0.2411417322834645549 ) ) ;
#53245 = CARTESIAN_POINT ( 'NONE',  ( 0.2034120734908142214, 0.2952755905511810774, -0.1292274648535930714 ) ) ;
#53246 = AXIS2_PLACEMENT_3D ( 'NONE', #8723, #60887, #60062 ) ;
#53247 = CARTESIAN_POINT ( 'NONE',  ( -1.660104986876639543, -0.08942795157528024563, -0.3641732283464568787 ) ) ;
#53248 = CARTESIAN_POINT ( 'NONE',  ( -0.3996062992125986590, 0.1070741851644051723, -1.684383202099737575 ) ) ;
#53249 = CARTESIAN_POINT ( 'NONE',  ( -1.213910761154854745, 0.2952755905511810774, -0.1292274648535930714 ) ) ;
#53250 = AXIS2_PLACEMENT_3D ( 'NONE', #53342, #45353, #64732 ) ;
#53251 = AXIS2_PLACEMENT_3D ( 'NONE', #57851, #13682, #65022 ) ;
#53252 = CARTESIAN_POINT ( 'NONE',  ( 0.3937007874015754361, -0.1870078740157479769, 0.4822834645669291653 ) ) ;
#53253 = CARTESIAN_POINT ( 'NONE',  ( 0.06561679790026316017, -0.4281496062992124485, 0.4176697321401328655 ) ) ;
#53254 = CARTESIAN_POINT ( 'NONE',  ( 1.108923884514436242, -0.05778040916215522460, 0.4822834645669289988 ) ) ;
#53255 = CARTESIAN_POINT ( 'NONE',  ( -0.1998031496062991630, -0.3460692066303959202, -0.9297900262467192478 ) ) ;
#53257 = ADVANCED_FACE ( 'NONE', ( #43720 ), #8663, .F. ) ;
#53256 = CARTESIAN_POINT ( 'NONE',  ( 0.3460692066303959202, 0.1998031496062993295, -1.548556430446194287 ) ) ;
#53258 = CARTESIAN_POINT ( 'NONE',  ( -0.2891555358219911054, 0.2891555358219909388, -0.8070866141732284671 ) ) ;
#53259 = CARTESIAN_POINT ( 'NONE',  ( 0.4732185887570711236, 1.572090529166663364, 2.557182324916609240 ) ) ;
#53260 = CARTESIAN_POINT ( 'NONE',  ( 0.3608923884514443348, 0.1771653543307087075, -0.09757992244046823083 ) ) ;
#53261 = CARTESIAN_POINT ( 'NONE',  ( -0.5118110236220466680, -0.6692913385826771977, 8.415575281601705876E-17 ) ) ;
#53262 = CARTESIAN_POINT ( 'NONE',  ( 1.332020997375328974, -0.05778040916215560624, -0.4822834645669293319 ) ) ;
#53263 = CARTESIAN_POINT ( 'NONE',  ( 0.1058382717557499880, 0.3949938075777409408, -1.645013123359580831 ) ) ;
#53264 = CARTESIAN_POINT ( 'NONE',  ( -0.1377952755905504645, -0.4536011799217368745, -0.2665933059059886201 ) ) ;
#53265 = ADVANCED_FACE ( 'NONE', ( #74929, #68597 ), #31521, .F. ) ;
#53266 = CARTESIAN_POINT ( 'NONE',  ( -1.141732283464566011, 0.2952755905511811885, 0.000000000000000000 ) ) ;
#53267 = CARTESIAN_POINT ( 'NONE',  ( 1.587926509186352142, 0.05413385826771666132, 0.4176697321401328100 ) ) ;
#53268 = CARTESIAN_POINT ( 'NONE',  ( 0.2362204724409449064, 0.4091458600556404646, -2.034120734908136718 ) ) ;
#53269 = CARTESIAN_POINT ( 'NONE',  ( 0.3859888145977959928, 0.06766049032611561043, -2.755905511811024056 ) ) ;
#53270 = AXIS2_PLACEMENT_3D ( 'NONE', #70922, #7785, #44796 ) ;
#53271 = VERTEX_POINT ( 'NONE', #82877 ) ;
#53272 = VERTEX_POINT ( 'NONE', #30702 ) ;
#53273 = CARTESIAN_POINT ( 'NONE',  ( 1.423884514435696191, -0.05778040916215522460, 0.4822834645669289988 ) ) ;
#53274 = CARTESIAN_POINT ( 'NONE',  ( -1.653543307086613234, -0.1870078740157480879, -0.4822834645669291653 ) ) ;
#53276 = CARTESIAN_POINT ( 'NONE',  ( -1.338582677165353729, -0.1870078740157479769, 0.4822834645669291653 ) ) ;
#53275 = CARTESIAN_POINT ( 'NONE',  ( -1.312335958005248715, 0.1283753931104748280, 0.1820866141732283561 ) ) ;
#53277 = CARTESIAN_POINT ( 'NONE',  ( -0.3392501089628018329, -0.1958661417322836440, -2.337251025425510331 ) ) ;
#53278 = CARTESIAN_POINT ( 'NONE',  ( -3.900966923095589678, 2.559055118110236560, 0.5314960629921260393 ) ) ;
#53279 = CARTESIAN_POINT ( 'NONE',  ( 1.062992125984252745, 0.2952755905511811885, 0.000000000000000000 ) ) ;
#53280 = CARTESIAN_POINT ( 'NONE',  ( -1.122047244094487306, -0.5400638737290844871, 0.3530559997133364547 ) ) ;
#53281 = CARTESIAN_POINT ( 'NONE',  ( -0.1377952755905504645, 0.1660481256975885056, 0.3530559997133364547 ) ) ;
#53282 = CARTESIAN_POINT ( 'NONE',  ( -1.246719160104985846, -0.4281496062992127816, -0.4176697321401328100 ) ) ;
#53283 = CARTESIAN_POINT ( 'NONE',  ( 0.3917322834645670104, 2.398668435337828261E-17, 0.1122047244094487306 ) ) ;
#53284 = CARTESIAN_POINT ( 'NONE',  ( 0.4265091863517067039, -0.6692913385826773087, -0.1292274648535924053 ) ) ;
#53285 = CARTESIAN_POINT ( 'NONE',  ( 0.3917322834645670104, -0.1049643490035303411, -1.678477690288713964 ) ) ;
#53286 = CARTESIAN_POINT ( 'NONE',  ( -1.259842519685038686, -0.1870078740157480601, -0.3641732283464567677 ) ) ;
#53287 = ORIENTED_EDGE ( 'NONE', *, *, #3380, .F. ) ;
#53288 = CARTESIAN_POINT ( 'NONE',  ( -0.2891555358219908833, -0.2891555358219912164, -2.263779527559055094 ) ) ;
#53289 = ORIENTED_EDGE ( 'NONE', *, *, #83098, .T. ) ;
#53290 = LINE ( 'NONE', #48641, #59697 ) ;
#53291 = CARTESIAN_POINT ( 'NONE',  ( -1.017060367454067249, -0.3162353388693409650, -0.4822834645669289433 ) ) ;
#53292 = CARTESIAN_POINT ( 'NONE',  ( -1.095800524934382292, -0.3162353388693409650, -0.4822834645669289433 ) ) ;
#53293 = CARTESIAN_POINT ( 'NONE',  ( -0.3996062992125987146, 0.1070741851644051862, -0.5052493438320209140 ) ) ;
#53294 = CARTESIAN_POINT ( 'NONE',  ( -1.371391076115484831, 0.2952755905511810774, -0.1292274648535930714 ) ) ;
#53295 = CARTESIAN_POINT ( 'NONE',  ( -1.568241469816272105, -0.05778040916215522460, 0.4822834645669289988 ) ) ;
#53296 = CARTESIAN_POINT ( 'NONE',  ( -1.496062992125983815, -0.1870078740157479769, 0.4822834645669291653 ) ) ;
#53297 = SURFACE_STYLE_USAGE ( .BOTH. , #45311 ) ;
#53298 = CARTESIAN_POINT ( 'NONE',  ( -0.3917322834645671215, 0.1049643490035301469, 0.1975065616797899160 ) ) ;
#53299 = CARTESIAN_POINT ( 'NONE',  ( -0.05905511811023545637, 0.07958543189024085140, 0.2665933059059887866 ) ) ;
#53300 = CARTESIAN_POINT ( 'NONE',  ( 0.3917322834645669549, 0.1049643490035304660, -0.6817585301837268963 ) ) ;
#53301 = CARTESIAN_POINT ( 'NONE',  ( -0.9055118110236215490, 0.1771653543307087630, 0.000000000000000000 ) ) ;
#53302 = CARTESIAN_POINT ( 'NONE',  ( -1.253280839895012377, -0.3162353388693409650, -0.4822834645669289433 ) ) ;
#53303 = CARTESIAN_POINT ( 'NONE',  ( 0.8858267716535438430, -0.5400638737290845981, -0.3530559997133363437 ) ) ;
#53304 = CARTESIAN_POINT ( 'NONE',  ( -0.8595800524934373854, -0.05778040916215522460, 0.4822834645669289988 ) ) ;
#53305 = CARTESIAN_POINT ( 'NONE',  ( 0.4606732211678798428, 1.541615089183433485, -0.5309055118110237448 ) ) ;
#53306 = ORIENTED_EDGE ( 'NONE', *, *, #81602, .T. ) ;
#53307 = CARTESIAN_POINT ( 'NONE',  ( -1.391076115485563314, -0.6046776061558809534, -0.2411417322834644161 ) ) ;
#53308 = CARTESIAN_POINT ( 'NONE',  ( 0.8267716535433077274, 0.2952755905511811885, 0.000000000000000000 ) ) ;
#53309 = CARTESIAN_POINT ( 'NONE',  ( -1.660104986876639543, -0.08942795157528024563, -0.3641732283464568787 ) ) ;
#53310 = CARTESIAN_POINT ( 'NONE',  ( -1.653543307086613234, -0.1870078740157480879, -0.4822834645669291653 ) ) ;
#53311 = CARTESIAN_POINT ( 'NONE',  ( -0.4724409448818895907, -0.1265901696524993070, -1.148293963254592986 ) ) ;
#53312 = FACE_OUTER_BOUND ( 'NONE', #7461, .T. ) ;
#53313 = CARTESIAN_POINT ( 'NONE',  ( -0.3392501089628017219, -0.1958661417322836718, -0.5170603674540682482 ) ) ;
#53314 = AXIS2_PLACEMENT_3D ( 'NONE', #35431, #40917, #34610 ) ;
#53315 = CARTESIAN_POINT ( 'NONE',  ( 0.2867679344610366554, 0.2867679344610366554, -2.584645669291338876 ) ) ;
#53316 = CARTESIAN_POINT ( 'NONE',  ( -0.1312335958005241554, -0.6046776061558809534, -0.2411417322834644161 ) ) ;
#53317 = CARTESIAN_POINT ( 'NONE',  ( 1.653543307086614789, -0.1870078740157479769, 0.4822834645669291653 ) ) ;
#53318 = AXIS2_PLACEMENT_3D ( 'NONE', #32222, #57880, #19592 ) ;
#53319 = VECTOR ( 'NONE', #29807, 39.37007874015748143 ) ;
#53320 = CARTESIAN_POINT ( 'NONE',  ( 0.3996062992125986035, -0.1070741851644052972, -0.1883202099737532609 ) ) ;
#53322 = CARTESIAN_POINT ( 'NONE',  ( -0.6561679790026240244, 0.1539470093639521697, -0.1968503937007875793 ) ) ;
#53321 = CARTESIAN_POINT ( 'NONE',  ( -1.601049868766403650, -0.6046776061558807314, 0.2411417322834647770 ) ) ;
#53323 = EDGE_CURVE ( 'NONE', #58782, #12593, #37430, .T. ) ;
#53324 = CARTESIAN_POINT ( 'NONE',  ( -1.620734908136482577, -0.6692913385826773087, -0.1292274648535924053 ) ) ;
#53325 = CARTESIAN_POINT ( 'NONE',  ( -0.5971128608923877978, 0.2952755905511811885, 0.1292274648535926551 ) ) ;
#53326 = CARTESIAN_POINT ( 'NONE',  ( 0.1958661417322834497, 0.3392501089628018329, 0.09057049688420130973 ) ) ;
#53327 = CARTESIAN_POINT ( 'NONE',  ( 0.4199475065616803948, -0.5023911411419708095, -0.1820866141732282451 ) ) ;
#53328 = CARTESIAN_POINT ( 'NONE',  ( -0.3917322834645669549, -0.1049643490035306603, -0.1305774278215224016 ) ) ;
#53329 = CARTESIAN_POINT ( 'NONE',  ( 0.4265091863517067594, 0.1771653543307087630, 0.09757992244046791164 ) ) ;
#53330 = CARTESIAN_POINT ( 'NONE',  ( 1.108923884514436242, -0.08942795157527998196, 0.3641732283464567121 ) ) ;
#53331 = CARTESIAN_POINT ( 'NONE',  ( 1.076115485564305141, -0.6046776061558807314, 0.2411417322834647770 ) ) ;
#53332 = CARTESIAN_POINT ( 'NONE',  ( 0.2165354330708668673, -0.4536011799217367080, 0.2665933059059888421 ) ) ;
#53333 = CARTESIAN_POINT ( 'NONE',  ( 0.1049643490035303689, 0.3917322834645670104, -1.717847769028871596 ) ) ;
#53334 = CARTESIAN_POINT ( 'NONE',  ( -1.312335958005248715, 0.2306618581243848609, 0.2411417322834645549 ) ) ;
#53335 = CARTESIAN_POINT ( 'NONE',  ( -0.2296587926509179312, -0.2845877964562161244, -0.3641732283464567121 ) ) ;
#53336 =( BOUNDED_SURFACE ( )  B_SPLINE_SURFACE ( 1, 2, ( 
 ( #24901, #70783, #13134, #24085, #44251, #49755, #12296, #75860, #38785, #30401, #11475, #37542, #69125, #37131, #5149, #37952, #63629, #5966, #31636, #57296, #44658, #1752, #6799, #53070, #34149, #71618, #14806, #20693, #65317, #72039, #58132, #15216, #13970, #501, #52656, #7222, #59810, #45504, #78362, #27409, #46765, #46344, #39627, #14395, #78781, #40465, #71201, #19855, #13544, #40052, #51815, #65738, #7655, #45920, #8071, #39200, #66143, #77520, #26584, #72457, #927, #64883, #59394, #2165, #21106, #33734, #8480, #53492, #27831, #26993, #79201, #21517, #47176, #32894, #72868, #64462, #32470, #26154, #58561, #52237, #33325, #77941, #58987, #20270, #1343, #9721, #28660, #9310, #35392, #34980, #35806, #67387, #60644, #15635, #61472, #60235, #23163, #16879, #55140, #79616, #2994, #67804, #10141, #41292, #2583, #42517, #66558, #80851, #21933, #8891, #66977, #34568, #48832, #42107, #16048, #3820, #74533, #28242, #61057, #53902, #3408, #54321, #29481, #68220, #47593, #80030, #40876, #73287, #29070, #22349, #80446, #48009, #54741, #73708, #41694, #22756, #74116, #48418, #16462, #39904, #66412, #72315, #33586, #40319, #58841, #773, #52086, #46620, #20128, #65592, #32747, #59250, #1608, #7925, #72723, #20961, #15489, #26435, #14662, #1199, #40728, #41146, #39481, #27264, #66835, #2442, #13822, #73140, #26849, #52924, #65168, #8749, #21783, #53349, #58414, #21376, #28100, #78638, #34420, #65998, #8337, #34003, #52507, #77796, #45775, #59664, #71474, #2020, #7504, #27684, #79059, #47031, #15070, #60088, #33173, #78216, #20548, #46200, #53756, #71895, #79466, #14246, #47445, #73564, #23023, #29747, #74803, #80709, #16318, #42371, #55411, #68478, #15908, #47859, #41557, #16730, #79885, #68070, #41963, #73973, #10414, #67245, #10816, #22203, #54591, #17150, #28923, #9576, #4080, #4493, #49099, #36071, #74387, #81530, #81118, #55001, #62151, #36476, #42783, #35246, #30160, #61743, #48690, #23434, #60910, #49517, #61322, #28513, #3677, #43186, #55822, #23850, #67657, #80301, #75210, #22615, #17554, #9168, #48275, #3262, #34840, #54171, #60500, #2849, #9993, #35659, #29340, #51149, #76843, #37308, #56245, #51562, #36893, #64219, #17963, #62569, #5321, #4908, #32225, #83163, #5720, #44826, #38539, #30579, #57056, #81941, #6134, #70523, #49926, #43599, #11650, #62982, #69301, #31391, #30979, #11233, #77265, #70108, #57469, #75625, #56646, #19177, #82748, #31809, #12460, #82347, #24666, #50334, #25482, #25070, #50744, #76031, #12879, #18376, #37711, #69710, #38122, #44016, #63796, #24253, #12054, #6553, #63384, #57882, #249, #76442, #18771, #25901, #19594, #44414, #68883, #21095, #59800, #33722, #14384, #21921, #7645, #34971, #28650, #66968, #78351, #59384, #53891, #79605, #40042, #58977, #54310, #39617, #9301, #20683, #65306, #8061, #33315, #60634, #2573, #8469, #47583, #41282, #1333, #2154, #26982, #27821, #65728, #73277, #80021, #46335, #78771, #22340, #2985, #52647, #71607, #1742, #34139, #72028, #15625, #13960, #8881, #27399, #60223, #53059, #46754, #72447, #53481, #14796, #79191, #40453, #66132, #21507, #47165, #72857, #15205, #40866, #66548, #34557, #28232, #4620, #36204, #30713, #16039, #41685, #82075, #80841, #67378, #61873, #74107, #43317, #29061, #4214, #68607, #30291, #29878, #55131, #81250, #23154, #56376, #17687, #54732, #5044, #16453, #68209, #80437, #55957, #37024, #10947, #73699, #36604, #69015, #48823, #81670, #55540, #74524, #23565, #42098, #9712, #35383, #49236, #61048, #16870, #48000, #42507, #10546, #74939, #23981, #17284, #3398, #22747, #48407, #67795, #42912, #10132, #62282, #35796, #11367, #61463, #49648, #75340, #62706, #3811, #29473, #57607, #44968, #385, #5451, #57187, #83298, #44553, #24388, #25620, #82889, #5854, #51283, #56780, #26041, #37439, #69839, #6689, #44147, #31112, #19315, #19738, #64352, #76986, #6270, #13432, #13020, #70243, #77403, #51701, #32359, #24795, #58021, #70664, #63934, #31946, #82479, #64769, #76575, #43729, #18903, #58447, #45392, #38257, #31531, #12189, #71089, #38674, #25209, #12598, #37846, #50463, #39088 ),
 ( #76167, #11786, #7108, #18504, #32778, #50059, #50875, #63524, #75754, #18096, #69433, #63113, #45809, #20159, #72346, #47060, #60120, #15101, #8367, #21812, #58874, #59282, #73168, #65201, #1232, #26881, #52541, #33210, #46653, #78250, #26470, #66867, #2050, #72752, #7537, #20581, #66441, #14694, #40757, #27714, #46232, #71929, #14278, #8778, #40350, #66029, #39940, #2471, #65626, #52955, #1639, #53381, #7957, #79088, #39512, #33619, #21406, #27297, #34451, #28130, #78670, #20991, #53785, #47476, #34033, #59694, #79497, #15519, #41177, #9197, #34870, #807, #52121, #77829, #71507, #13854, #25005, #50677, #18710, #75145, #69644, #68818, #31324, #37240, #11581, #43948, #41585, #47888, #11988, #4426, #30914, #5250, #36823, #17490, #17896, #76376, #37642, #12396, #22233, #79916, #49857, #43121, #56581, #70042, #36411, #23780, #81462, #62917, #11164, #62498, #56988, #28544, #82282, #49451, #73596, #4836, #24600, #24188, #30511, #15938, #63319, #62085, #56173, #30092, #43533, #55756, #67275, #9608, #44351, #75966, #50268, #81876, #75557, #82685, #60531, #54200, #69232, #18306, #5657, #2881, #19957, #6488, #52756, #33420, #70456, #6069, #57814, #31742, #1437, #52336, #58235, #14073, #7755, #57405, #26258, #83096, #51919, #32158, #46024, #20789, #44760, #45184, #46445, #59082, #19111, #78464, #64154, #602, #12814, #71718, #27093, #58663, #63729, #26681, #72138, #70887, #39726, #77624, #38886, #45607, #181, #25417, #51082, #71301, #76779, #13236, #38053, #64565, #6902, #32573, #78042, #13649, #38471, #25834, #51493, #77196, #39302, #19527, #64989, #7324, #32993, #1028, #20372, #65421, #80131, #2682, #21614, #47692, #35076, #73809, #78883, #47274, #73386, #34671, #14494, #15738, #72964, #79296, #41392, #46859, #16146, #27511, #59911, #22451, #34249, #21204, #9406, #9819, #54420, #67074, #79715, #3506, #3094, #60334, #67484, #41793, #48111, #14900, #35490, #60742, #54003, #22031, #72553, #54841, #66660, #33830, #8999, #48519, #61154, #28342, #15315, #2266, #29175, #28758, #40978, #80546, #27929, #40560, #22858, #59496, #40147, #65832, #8165, #66241, #53587, #1850, #53168, #8578, #61578, #56895, #42209, #10657, #3921, #36312, #24090, #36719, #49351, #29582, #75866, #48936, #61988, #16980, #56074, #68320, #35912, #55245, #63223, #5155, #37136, #75048, #80952, #43844, #74219, #67904, #62395, #23267, #69130, #74637, #81780, #42623, #5563, #62821, #50170, #30819, #49760, #11895, #4325, #17394, #31227, #29991, #55654, #81364, #23677, #43025, #4733, #68719, #16564, #82588, #75460, #56484, #11061, #30406, #82187, #17798, #24504, #43433, #11481, #18209, #69547, #37548, #24908, #10241, #76683, #26591, #32061, #19434, #51398, #77526, #57721, #45510, #5973, #19016, #19862, #50985, #58568, #71207, #84, #25737, #52243, #71624, #83000, #44664, #933, #77102, #45085, #38375, #39206, #70789, #31643, #13550, #45926, #64889, #13976, #39633, #7661, #64050, #77947, #13140, #20276, #26160, #507, #32900, #57302, #37958, #65324, #70360, #7228, #33332, #38791, #6390, #6805, #58993, #1349, #50576, #12302, #69947, #64468, #32476, #76283, #18614, #25321, #12715, #58138, #51822, #44257, #63635, #22357, #78368, #53909, #53076, #3001, #8487, #79208, #27838, #79623, #34156, #21940, #65744, #78788, #47600, #27415, #34987, #73294, #59817, #2172, #28667, #48016, #59400, #21113, #60651, #53500, #21524, #14813, #15643, #47183, #8077, #41299, #73716, #66985, #16055, #41701, #67394, #40472, #54328, #72875, #80037, #2590, #60243, #9317, #33740, #14401, #9728, #46773, #35399, #61064, #15223, #66150, #66565, #26999, #52662, #20700, #72046, #46350, #40883, #8899, #40057, #1758, #72464, #34575, #28249, #36621, #36220, #4230, #82089, #54748, #30307, #23171, #74124, #48840, #62299, #49253, #61889, #42115, #5058, #61480, #74541, #29489, #68623, #80859, #48425, #16470, #75768, #17703, #49665, #29894, #67812, #56390, #3415, #80454, #74955, #10149, #81686, #35815, #10963, #55148, #18110, #75355, #62721, #43331, #4636, #24403, #3829, #55557, #43743, #16887, #42526, #68228, #10562, #81266, #17301, #23581 ) ),
 .UNSPECIFIED., .F., .F., .F. ) 
 B_SPLINE_SURFACE_WITH_KNOTS ( ( 2, 2 ),
 ( 3, 2, 2, 2, 2, 2, 2, 2, 2, 2, 2, 2, 2, 2, 2, 2, 2, 2, 2, 2, 2, 2, 2, 2, 2, 2, 2, 2, 2, 2, 2, 2, 2, 2, 2, 2, 2, 2, 2, 2, 2, 2, 2, 2, 2, 2, 2, 2, 2, 2, 2, 2, 2, 2, 2, 2, 2, 2, 2, 2, 2, 2, 2, 2, 2, 2, 2, 2, 2, 2, 2, 2, 2, 2, 2, 2, 2, 2, 2, 2, 2, 2, 2, 2, 2, 2, 2, 2, 2, 2, 2, 2, 2, 2, 2, 2, 2, 2, 2, 2, 2, 2, 2, 2, 2, 2, 2, 2, 2, 2, 2, 2, 2, 2, 2, 2, 2, 2, 2, 2, 2, 2, 2, 2, 2, 2, 2, 2, 2, 2, 2, 2, 2, 2, 2, 2, 2, 2, 2, 2, 2, 2, 2, 2, 2, 2, 2, 2, 2, 2, 2, 2, 2, 2, 2, 2, 2, 2, 2, 2, 2, 2, 2, 2, 2, 2, 2, 2, 2, 2, 2, 2, 2, 2, 2, 2, 2, 2, 2, 2, 2, 2, 2, 2, 2, 2, 2, 2, 2, 2, 2, 2, 2, 2, 2, 2, 2, 2, 2, 2, 2, 2, 2, 2, 2, 2, 2, 2, 2, 2, 2, 2, 2, 2, 2, 2, 2, 2, 2, 2, 2, 2, 2, 2, 2, 2, 2, 2, 2, 2, 2, 2, 2, 2, 2, 2, 2, 2, 2, 2, 2, 2, 2, 2, 2, 2, 2, 2, 2, 2, 2, 2, 2, 2, 2, 3 ),
 ( 0.000000000000000000, 1.000000000000000000 ),
 ( 0.000000000000000000, 0.003787878787878787984, 0.007575757575757575968, 0.01136363636363636395, 0.01515151515151515194, 0.01893939393939393992, 0.02272727272727272790, 0.02651515151515151589, 0.03030303030303030387, 0.03409090909090908839, 0.03787878787878787984, 0.04166666666666666435, 0.04545454545454545581, 0.04924242424242424032, 0.05303030303030303177, 0.05681818181818181629, 0.06060606060606060774, 0.06439393939393939226, 0.06818181818181817677, 0.07196969696969697516, 0.07575757575757575968, 0.07954545454545454419, 0.08333333333333332871, 0.08712121212121212710, 0.09090909090909091161, 0.09469696969696969613, 0.09848484848484848064, 0.1022727272727272790, 0.1060606060606060635, 0.1098484848484848481, 0.1136363636363636326, 0.1174242424242424310, 0.1212121212121212155, 0.1250000000000000000, 0.1287878787878787845, 0.1325757575757575690, 0.1363636363636363535, 0.1401515151515151381, 0.1439393939393939503, 0.1477272727272727348, 0.1515151515151515194, 0.1553030303030303039, 0.1590909090909090884, 0.1628787878787878729, 0.1666666666666666574, 0.1704545454545454419, 0.1742424242424242542, 0.1780303030303030387, 0.1818181818181818232, 0.1856060606060606077, 0.1893939393939393923, 0.1931818181818181768, 0.1969696969696969613, 0.2007575757575757458, 0.2045454545454545581, 0.2083333333333333426, 0.2121212121212121271, 0.2159090909090909116, 0.2196969696969696961, 0.2234848484848484806, 0.2272727272727272652, 0.2310606060606060497, 0.2348484848484848619, 0.2386363636363636465, 0.2424242424242424310, 0.2462121212121212155, 0.2500000000000000000, 0.2537878787878787845, 0.2575757575757575690, 0.2613636363636363535, 0.2651515151515151381, 0.2689393939393939226, 0.2727272727272727071, 0.2765151515151514916, 0.2803030303030302761, 0.2840909090909091161, 0.2878787878787879007, 0.2916666666666666852, 0.2954545454545454697, 0.2992424242424242542, 0.3030303030303030387, 0.3068181818181818232, 0.3106060606060606077, 0.3143939393939393923, 0.3181818181818181768, 0.3219696969696969613, 0.3257575757575757458, 0.3295454545454545303, 0.3333333333333333148, 0.3371212121212120993, 0.3409090909090908839, 0.3446969696969697239, 0.3484848484848485084, 0.3522727272727272929, 0.3560606060606060774, 0.3598484848484848619, 0.3636363636363636465, 0.3674242424242424310, 0.3712121212121212155, 0.3750000000000000000, 0.3787878787878787845, 0.3825757575757575690, 0.3863636363636363535, 0.3901515151515151381, 0.3939393939393939226, 0.3977272727272727071, 0.4015151515151514916, 0.4053030303030302761, 0.4090909090909091161, 0.4128787878787879007, 0.4166666666666666852, 0.4204545454545454697, 0.4242424242424242542, 0.4280303030303030387, 0.4318181818181818232, 0.4356060606060606077, 0.4393939393939393923, 0.4431818181818181768, 0.4469696969696969613, 0.4507575757575757458, 0.4545454545454545303, 0.4583333333333333148, 0.4621212121212120993, 0.4659090909090908839, 0.4696969696969697239, 0.4734848484848485084, 0.4772727272727272929, 0.4810606060606060774, 0.4848484848484848619, 0.4886363636363636465, 0.4924242424242424310, 0.4962121212121212155, 0.5000000000000000000, 0.5037878787878787845, 0.5075757575757575690, 0.5113636363636363535, 0.5151515151515151381, 0.5189393939393939226, 0.5227272727272727071, 0.5265151515151514916, 0.5303030303030302761, 0.5340909090909090606, 0.5378787878787878451, 0.5416666666666666297, 0.5454545454545454142, 0.5492424242424241987, 0.5530303030303029832, 0.5568181818181817677, 0.5606060606060605522, 0.5643939393939394478, 0.5681818181818182323, 0.5719696969696970168, 0.5757575757575758013, 0.5795454545454545858, 0.5833333333333333703, 0.5871212121212121549, 0.5909090909090909394, 0.5946969696969697239, 0.5984848484848485084, 0.6022727272727272929, 0.6060606060606060774, 0.6098484848484848619, 0.6136363636363636465, 0.6174242424242424310, 0.6212121212121212155, 0.6250000000000000000, 0.6287878787878787845, 0.6325757575757575690, 0.6363636363636363535, 0.6401515151515151381, 0.6439393939393939226, 0.6477272727272727071, 0.6515151515151514916, 0.6553030303030302761, 0.6590909090909090606, 0.6628787878787878451, 0.6666666666666666297, 0.6704545454545454142, 0.6742424242424241987, 0.6780303030303029832, 0.6818181818181817677, 0.6856060606060605522, 0.6893939393939394478, 0.6931818181818182323, 0.6969696969696970168, 0.7007575757575758013, 0.7045454545454545858, 0.7083333333333333703, 0.7121212121212121549, 0.7159090909090909394, 0.7196969696969697239, 0.7234848484848485084, 0.7272727272727272929, 0.7310606060606060774, 0.7348484848484848619, 0.7386363636363636465, 0.7424242424242424310, 0.7462121212121212155, 0.7500000000000000000, 0.7537878787878787845, 0.7575757575757575690, 0.7613636363636363535, 0.7651515151515151381, 0.7689393939393939226, 0.7727272727272727071, 0.7765151515151514916, 0.7803030303030302761, 0.7840909090909090606, 0.7878787878787878451, 0.7916666666666666297, 0.7954545454545454142, 0.7992424242424241987, 0.8030303030303029832, 0.8068181818181817677, 0.8106060606060605522, 0.8143939393939394478, 0.8181818181818182323, 0.8219696969696970168, 0.8257575757575758013, 0.8295454545454545858, 0.8333333333333333703, 0.8371212121212121549, 0.8409090909090909394, 0.8446969696969697239, 0.8484848484848485084, 0.8522727272727272929, 0.8560606060606060774, 0.8598484848484848619, 0.8636363636363636465, 0.8674242424242424310, 0.8712121212121212155, 0.8750000000000000000, 0.8787878787878787845, 0.8825757575757575690, 0.8863636363636363535, 0.8901515151515151381, 0.8939393939393939226, 0.8977272727272727071, 0.9015151515151514916, 0.9053030303030302761, 0.9090909090909090606, 0.9128787878787878451, 0.9166666666666666297, 0.9204545454545454142, 0.9242424242424241987, 0.9280303030303029832, 0.9318181818181817677, 0.9356060606060605522, 0.9393939393939394478, 0.9431818181818182323, 0.9469696969696970168, 0.9507575757575758013, 0.9545454545454545858, 0.9583333333333333703, 0.9621212121212121549, 0.9659090909090909394 ),
 .UNSPECIFIED. ) 
 GEOMETRIC_REPRESENTATION_ITEM ( )  RATIONAL_B_SPLINE_SURFACE ( (
 ( 1.000000000000000000, 0.9659258262890683122, 1.000000000000000000, 0.9659258262890683122, 1.000000000000000000, 0.9659258262890683122, 1.000000000000000000, 0.9659258262890683122, 1.000000000000000000, 0.9659258262890683122, 1.000000000000000000, 0.9659258262890683122, 1.000000000000000000, 0.9659258262890683122, 1.000000000000000000, 0.9659258262890683122, 1.000000000000000000, 0.9659258262890683122, 1.000000000000000000, 0.9659258262890683122, 1.000000000000000000, 0.9659258262890683122, 1.000000000000000000, 0.9659258262890683122, 1.000000000000000000, 0.9659258262890683122, 1.000000000000000000, 0.9659258262890683122, 1.000000000000000000, 0.9659258262890683122, 1.000000000000000000, 0.9659258262890683122, 1.000000000000000000, 0.9659258262890683122, 1.000000000000000000, 0.9659258262890683122, 1.000000000000000000, 0.9659258262890683122, 1.000000000000000000, 0.9659258262890683122, 1.000000000000000000, 0.9659258262890683122, 1.000000000000000000, 0.9659258262890683122, 1.000000000000000000, 0.9659258262890683122, 1.000000000000000000, 0.9659258262890683122, 1.000000000000000000, 0.9659258262890683122, 1.000000000000000000, 0.9659258262890683122, 1.000000000000000000, 0.9659258262890683122, 1.000000000000000000, 0.9659258262890683122, 1.000000000000000000, 0.9659258262890683122, 1.000000000000000000, 0.9659258262890683122, 1.000000000000000000, 0.9659258262890683122, 1.000000000000000000, 0.9659258262890683122, 1.000000000000000000, 0.9659258262890683122, 1.000000000000000000, 0.9659258262890683122, 1.000000000000000000, 0.9659258262890683122, 1.000000000000000000, 0.9659258262890683122, 1.000000000000000000, 0.9659258262890683122, 1.000000000000000000, 0.9659258262890683122, 1.000000000000000000, 0.9659258262890683122, 1.000000000000000000, 0.9659258262890683122, 1.000000000000000000, 0.9659258262890683122, 1.000000000000000000, 0.9659258262890683122, 1.000000000000000000, 0.9659258262890683122, 1.000000000000000000, 0.9659258262890683122, 1.000000000000000000, 0.9659258262890683122, 1.000000000000000000, 0.9659258262890683122, 1.000000000000000000, 0.9659258262890683122, 1.000000000000000000, 0.9659258262890683122, 1.000000000000000000, 0.9659258262890683122, 1.000000000000000000, 0.9659258262890683122, 1.000000000000000000, 0.9659258262890683122, 1.000000000000000000, 0.9659258262890683122, 1.000000000000000000, 0.9659258262890683122, 1.000000000000000000, 0.9659258262890683122, 1.000000000000000000, 0.9659258262890683122, 1.000000000000000000, 0.9659258262890683122, 1.000000000000000000, 0.9659258262890683122, 1.000000000000000000, 0.9659258262890683122, 1.000000000000000000, 0.9659258262890683122, 1.000000000000000000, 0.9659258262890683122, 1.000000000000000000, 0.9659258262890683122, 1.000000000000000000, 0.9659258262890683122, 1.000000000000000000, 0.9659258262890683122, 1.000000000000000000, 0.9659258262890683122, 1.000000000000000000, 0.9659258262890683122, 1.000000000000000000, 0.9659258262890683122, 1.000000000000000000, 0.9659258262890683122, 1.000000000000000000, 0.9659258262890683122, 1.000000000000000000, 0.9659258262890683122, 1.000000000000000000, 0.9659258262890683122, 1.000000000000000000, 0.9659258262890683122, 1.000000000000000000, 0.9659258262890683122, 1.000000000000000000, 0.9659258262890683122, 1.000000000000000000, 0.9659258262890683122, 1.000000000000000000, 0.9659258262890683122, 1.000000000000000000, 0.9659258262890683122, 1.000000000000000000, 0.9659258262890683122, 1.000000000000000000, 0.9659258262890683122, 1.000000000000000000, 0.9659258262890683122, 1.000000000000000000, 0.9659258262890683122, 1.000000000000000000, 0.9659258262890683122, 1.000000000000000000, 0.9659258262890683122, 1.000000000000000000, 0.9659258262890683122, 1.000000000000000000, 0.9659258262890683122, 1.000000000000000000, 0.9659258262890683122, 1.000000000000000000, 0.9659258262890683122, 1.000000000000000000, 0.9659258262890683122, 1.000000000000000000, 0.9659258262890683122, 1.000000000000000000, 0.9659258262890683122, 1.000000000000000000, 0.9659258262890683122, 1.000000000000000000, 0.9659258262890683122, 1.000000000000000000, 0.9659258262890683122, 1.000000000000000000, 0.9659258262890683122, 1.000000000000000000, 0.9659258262890683122, 1.000000000000000000, 0.9659258262890683122, 1.000000000000000000, 0.9659258262890683122, 1.000000000000000000, 0.9659258262890683122, 1.000000000000000000, 0.9659258262890683122, 1.000000000000000000, 0.9659258262890683122, 1.000000000000000000, 0.9659258262890683122, 1.000000000000000000, 0.9659258262890683122, 1.000000000000000000, 0.9659258262890683122, 1.000000000000000000, 0.9659258262890683122, 1.000000000000000000, 0.9659258262890683122, 1.000000000000000000, 0.9659258262890683122, 1.000000000000000000, 0.9659258262890683122, 1.000000000000000000, 0.9659258262890683122, 1.000000000000000000, 0.9659258262890683122, 1.000000000000000000, 0.9659258262890683122, 1.000000000000000000, 0.9659258262890683122, 1.000000000000000000, 0.9659258262890683122, 1.000000000000000000, 0.9659258262890683122, 1.000000000000000000, 0.9659258262890683122, 1.000000000000000000, 0.9659258262890683122, 1.000000000000000000, 0.9659258262890683122, 1.000000000000000000, 0.9659258262890683122, 1.000000000000000000, 0.9659258262890683122, 1.000000000000000000, 0.9659258262890683122, 1.000000000000000000, 0.9659258262890683122, 1.000000000000000000, 0.9659258262890683122, 1.000000000000000000, 0.9659258262890683122, 1.000000000000000000, 0.9659258262890683122, 1.000000000000000000, 0.9659258262890683122, 1.000000000000000000, 0.9659258262890683122, 1.000000000000000000, 0.9659258262890683122, 1.000000000000000000, 0.9659258262890683122, 1.000000000000000000, 0.9659258262890683122, 1.000000000000000000, 0.9659258262890683122, 1.000000000000000000, 0.9659258262890683122, 1.000000000000000000, 0.9659258262890683122, 1.000000000000000000, 0.9659258262890683122, 1.000000000000000000, 0.9659258262890683122, 1.000000000000000000, 0.9659258262890683122, 1.000000000000000000, 0.9659258262890683122, 1.000000000000000000, 0.9659258262890683122, 1.000000000000000000, 0.9659258262890683122, 1.000000000000000000, 0.9659258262890683122, 1.000000000000000000, 0.9659258262890683122, 1.000000000000000000, 0.9659258262890683122, 1.000000000000000000, 0.9659258262890683122, 1.000000000000000000, 0.9659258262890683122, 1.000000000000000000, 0.9659258262890683122, 1.000000000000000000, 0.9659258262890683122, 1.000000000000000000, 0.9659258262890683122, 1.000000000000000000, 0.9659258262890683122, 1.000000000000000000, 0.9659258262890683122, 1.000000000000000000, 0.9659258262890683122, 1.000000000000000000, 0.9659258262890683122, 1.000000000000000000, 0.9659258262890683122, 1.000000000000000000, 0.9659258262890683122, 1.000000000000000000, 0.9659258262890683122, 1.000000000000000000, 0.9659258262890683122, 1.000000000000000000, 0.9659258262890683122, 1.000000000000000000, 0.9659258262890683122, 1.000000000000000000, 0.9659258262890683122, 1.000000000000000000, 0.9659258262890683122, 1.000000000000000000, 0.9659258262890683122, 1.000000000000000000, 0.9659258262890683122, 1.000000000000000000, 0.9659258262890683122, 1.000000000000000000, 0.9659258262890683122, 1.000000000000000000, 0.9659258262890683122, 1.000000000000000000, 0.9659258262890683122, 1.000000000000000000, 0.9659258262890683122, 1.000000000000000000, 0.9659258262890683122, 1.000000000000000000, 0.9659258262890683122, 1.000000000000000000, 0.9659258262890683122, 1.000000000000000000, 0.9659258262890683122, 1.000000000000000000, 0.9659258262890683122, 1.000000000000000000, 0.9659258262890683122, 1.000000000000000000, 0.9659258262890683122, 1.000000000000000000, 0.9659258262890683122, 1.000000000000000000, 0.9659258262890683122, 1.000000000000000000, 0.9659258262890683122, 1.000000000000000000, 0.9659258262890683122, 1.000000000000000000, 0.9659258262890683122, 1.000000000000000000, 0.9659258262890683122, 1.000000000000000000, 0.9659258262890683122, 1.000000000000000000, 0.9659258262890683122, 1.000000000000000000, 0.9659258262890683122, 1.000000000000000000, 0.9659258262890683122, 1.000000000000000000, 0.9659258262890683122, 1.000000000000000000, 0.9659258262890683122, 1.000000000000000000, 0.9659258262890683122, 1.000000000000000000, 0.9659258262890683122, 1.000000000000000000, 0.9659258262890683122, 1.000000000000000000, 0.9659258262890683122, 1.000000000000000000, 0.9659258262890683122, 1.000000000000000000, 0.9659258262890683122, 1.000000000000000000, 0.9659258262890683122, 1.000000000000000000, 0.9659258262890683122, 1.000000000000000000, 0.9659258262890683122, 1.000000000000000000, 0.9659258262890683122, 1.000000000000000000, 0.9659258262890683122, 1.000000000000000000, 0.9659258262890683122, 1.000000000000000000, 0.9659258262890683122, 1.000000000000000000, 0.9659258262890683122, 1.000000000000000000, 0.9659258262890683122, 1.000000000000000000, 0.9659258262890683122, 1.000000000000000000, 0.9659258262890683122, 1.000000000000000000, 0.9659258262890683122, 1.000000000000000000, 0.9659258262890683122, 1.000000000000000000, 0.9659258262890683122, 1.000000000000000000, 0.9659258262890683122, 1.000000000000000000, 0.9659258262890683122, 1.000000000000000000, 0.9659258262890683122, 1.000000000000000000, 0.9659258262890683122, 1.000000000000000000, 0.9659258262890683122, 1.000000000000000000, 0.9659258262890683122, 1.000000000000000000, 0.9659258262890683122, 1.000000000000000000, 0.9659258262890683122, 1.000000000000000000, 0.9659258262890683122, 1.000000000000000000, 0.9659258262890683122, 1.000000000000000000, 0.9659258262890683122, 1.000000000000000000, 0.9659258262890683122, 1.000000000000000000, 0.9659258262890683122, 1.000000000000000000, 0.9659258262890683122, 1.000000000000000000, 0.9659258262890683122, 1.000000000000000000, 0.9659258262890683122, 1.000000000000000000, 0.9659258262890683122, 1.000000000000000000, 0.9659258262890683122, 1.000000000000000000, 0.9659258262890683122, 1.000000000000000000, 0.9659258262890683122, 1.000000000000000000, 0.9659258262890683122, 1.000000000000000000, 0.9659258262890683122, 1.000000000000000000, 0.9659258262890683122, 1.000000000000000000, 0.9659258262890683122, 1.000000000000000000, 0.9659258262890683122, 1.000000000000000000, 0.9659258262890683122, 1.000000000000000000, 0.9659258262890683122, 1.000000000000000000, 0.9659258262890683122, 1.000000000000000000, 0.9659258262890683122, 1.000000000000000000, 0.9659258262890683122, 1.000000000000000000, 0.9659258262890683122, 1.000000000000000000, 0.9659258262890683122, 1.000000000000000000, 0.9659258262890683122, 1.000000000000000000, 0.9659258262890683122, 1.000000000000000000, 0.9659258262890683122, 1.000000000000000000, 0.9659258262890683122, 1.000000000000000000, 0.9659258262890683122, 1.000000000000000000, 0.9659258262890683122, 1.000000000000000000, 0.9659258262890683122, 1.000000000000000000, 0.9659258262890683122, 1.000000000000000000, 0.9659258262890683122, 1.000000000000000000, 0.9659258262890683122, 1.000000000000000000, 0.9659258262890683122, 1.000000000000000000, 0.9659258262890683122, 1.000000000000000000, 0.9659258262890683122, 1.000000000000000000, 0.9659258262890683122, 1.000000000000000000, 0.9659258262890683122, 1.000000000000000000, 0.9659258262890683122, 1.000000000000000000, 0.9659258262890683122, 1.000000000000000000, 0.9659258262890683122, 1.000000000000000000, 0.9659258262890683122, 1.000000000000000000, 0.9659258262890683122, 1.000000000000000000, 0.9659258262890683122, 1.000000000000000000),
 ( 1.000000000000000000, 0.9659258262890683122, 1.000000000000000000, 0.9659258262890683122, 1.000000000000000000, 0.9659258262890683122, 1.000000000000000000, 0.9659258262890683122, 1.000000000000000000, 0.9659258262890683122, 1.000000000000000000, 0.9659258262890683122, 1.000000000000000000, 0.9659258262890683122, 1.000000000000000000, 0.9659258262890683122, 1.000000000000000000, 0.9659258262890683122, 1.000000000000000000, 0.9659258262890683122, 1.000000000000000000, 0.9659258262890683122, 1.000000000000000000, 0.9659258262890683122, 1.000000000000000000, 0.9659258262890683122, 1.000000000000000000, 0.9659258262890683122, 1.000000000000000000, 0.9659258262890683122, 1.000000000000000000, 0.9659258262890683122, 1.000000000000000000, 0.9659258262890683122, 1.000000000000000000, 0.9659258262890683122, 1.000000000000000000, 0.9659258262890683122, 1.000000000000000000, 0.9659258262890683122, 1.000000000000000000, 0.9659258262890683122, 1.000000000000000000, 0.9659258262890683122, 1.000000000000000000, 0.9659258262890683122, 1.000000000000000000, 0.9659258262890683122, 1.000000000000000000, 0.9659258262890683122, 1.000000000000000000, 0.9659258262890683122, 1.000000000000000000, 0.9659258262890683122, 1.000000000000000000, 0.9659258262890683122, 1.000000000000000000, 0.9659258262890683122, 1.000000000000000000, 0.9659258262890683122, 1.000000000000000000, 0.9659258262890683122, 1.000000000000000000, 0.9659258262890683122, 1.000000000000000000, 0.9659258262890683122, 1.000000000000000000, 0.9659258262890683122, 1.000000000000000000, 0.9659258262890683122, 1.000000000000000000, 0.9659258262890683122, 1.000000000000000000, 0.9659258262890683122, 1.000000000000000000, 0.9659258262890683122, 1.000000000000000000, 0.9659258262890683122, 1.000000000000000000, 0.9659258262890683122, 1.000000000000000000, 0.9659258262890683122, 1.000000000000000000, 0.9659258262890683122, 1.000000000000000000, 0.9659258262890683122, 1.000000000000000000, 0.9659258262890683122, 1.000000000000000000, 0.9659258262890683122, 1.000000000000000000, 0.9659258262890683122, 1.000000000000000000, 0.9659258262890683122, 1.000000000000000000, 0.9659258262890683122, 1.000000000000000000, 0.9659258262890683122, 1.000000000000000000, 0.9659258262890683122, 1.000000000000000000, 0.9659258262890683122, 1.000000000000000000, 0.9659258262890683122, 1.000000000000000000, 0.9659258262890683122, 1.000000000000000000, 0.9659258262890683122, 1.000000000000000000, 0.9659258262890683122, 1.000000000000000000, 0.9659258262890683122, 1.000000000000000000, 0.9659258262890683122, 1.000000000000000000, 0.9659258262890683122, 1.000000000000000000, 0.9659258262890683122, 1.000000000000000000, 0.9659258262890683122, 1.000000000000000000, 0.9659258262890683122, 1.000000000000000000, 0.9659258262890683122, 1.000000000000000000, 0.9659258262890683122, 1.000000000000000000, 0.9659258262890683122, 1.000000000000000000, 0.9659258262890683122, 1.000000000000000000, 0.9659258262890683122, 1.000000000000000000, 0.9659258262890683122, 1.000000000000000000, 0.9659258262890683122, 1.000000000000000000, 0.9659258262890683122, 1.000000000000000000, 0.9659258262890683122, 1.000000000000000000, 0.9659258262890683122, 1.000000000000000000, 0.9659258262890683122, 1.000000000000000000, 0.9659258262890683122, 1.000000000000000000, 0.9659258262890683122, 1.000000000000000000, 0.9659258262890683122, 1.000000000000000000, 0.9659258262890683122, 1.000000000000000000, 0.9659258262890683122, 1.000000000000000000, 0.9659258262890683122, 1.000000000000000000, 0.9659258262890683122, 1.000000000000000000, 0.9659258262890683122, 1.000000000000000000, 0.9659258262890683122, 1.000000000000000000, 0.9659258262890683122, 1.000000000000000000, 0.9659258262890683122, 1.000000000000000000, 0.9659258262890683122, 1.000000000000000000, 0.9659258262890683122, 1.000000000000000000, 0.9659258262890683122, 1.000000000000000000, 0.9659258262890683122, 1.000000000000000000, 0.9659258262890683122, 1.000000000000000000, 0.9659258262890683122, 1.000000000000000000, 0.9659258262890683122, 1.000000000000000000, 0.9659258262890683122, 1.000000000000000000, 0.9659258262890683122, 1.000000000000000000, 0.9659258262890683122, 1.000000000000000000, 0.9659258262890683122, 1.000000000000000000, 0.9659258262890683122, 1.000000000000000000, 0.9659258262890683122, 1.000000000000000000, 0.9659258262890683122, 1.000000000000000000, 0.9659258262890683122, 1.000000000000000000, 0.9659258262890683122, 1.000000000000000000, 0.9659258262890683122, 1.000000000000000000, 0.9659258262890683122, 1.000000000000000000, 0.9659258262890683122, 1.000000000000000000, 0.9659258262890683122, 1.000000000000000000, 0.9659258262890683122, 1.000000000000000000, 0.9659258262890683122, 1.000000000000000000, 0.9659258262890683122, 1.000000000000000000, 0.9659258262890683122, 1.000000000000000000, 0.9659258262890683122, 1.000000000000000000, 0.9659258262890683122, 1.000000000000000000, 0.9659258262890683122, 1.000000000000000000, 0.9659258262890683122, 1.000000000000000000, 0.9659258262890683122, 1.000000000000000000, 0.9659258262890683122, 1.000000000000000000, 0.9659258262890683122, 1.000000000000000000, 0.9659258262890683122, 1.000000000000000000, 0.9659258262890683122, 1.000000000000000000, 0.9659258262890683122, 1.000000000000000000, 0.9659258262890683122, 1.000000000000000000, 0.9659258262890683122, 1.000000000000000000, 0.9659258262890683122, 1.000000000000000000, 0.9659258262890683122, 1.000000000000000000, 0.9659258262890683122, 1.000000000000000000, 0.9659258262890683122, 1.000000000000000000, 0.9659258262890683122, 1.000000000000000000, 0.9659258262890683122, 1.000000000000000000, 0.9659258262890683122, 1.000000000000000000, 0.9659258262890683122, 1.000000000000000000, 0.9659258262890683122, 1.000000000000000000, 0.9659258262890683122, 1.000000000000000000, 0.9659258262890683122, 1.000000000000000000, 0.9659258262890683122, 1.000000000000000000, 0.9659258262890683122, 1.000000000000000000, 0.9659258262890683122, 1.000000000000000000, 0.9659258262890683122, 1.000000000000000000, 0.9659258262890683122, 1.000000000000000000, 0.9659258262890683122, 1.000000000000000000, 0.9659258262890683122, 1.000000000000000000, 0.9659258262890683122, 1.000000000000000000, 0.9659258262890683122, 1.000000000000000000, 0.9659258262890683122, 1.000000000000000000, 0.9659258262890683122, 1.000000000000000000, 0.9659258262890683122, 1.000000000000000000, 0.9659258262890683122, 1.000000000000000000, 0.9659258262890683122, 1.000000000000000000, 0.9659258262890683122, 1.000000000000000000, 0.9659258262890683122, 1.000000000000000000, 0.9659258262890683122, 1.000000000000000000, 0.9659258262890683122, 1.000000000000000000, 0.9659258262890683122, 1.000000000000000000, 0.9659258262890683122, 1.000000000000000000, 0.9659258262890683122, 1.000000000000000000, 0.9659258262890683122, 1.000000000000000000, 0.9659258262890683122, 1.000000000000000000, 0.9659258262890683122, 1.000000000000000000, 0.9659258262890683122, 1.000000000000000000, 0.9659258262890683122, 1.000000000000000000, 0.9659258262890683122, 1.000000000000000000, 0.9659258262890683122, 1.000000000000000000, 0.9659258262890683122, 1.000000000000000000, 0.9659258262890683122, 1.000000000000000000, 0.9659258262890683122, 1.000000000000000000, 0.9659258262890683122, 1.000000000000000000, 0.9659258262890683122, 1.000000000000000000, 0.9659258262890683122, 1.000000000000000000, 0.9659258262890683122, 1.000000000000000000, 0.9659258262890683122, 1.000000000000000000, 0.9659258262890683122, 1.000000000000000000, 0.9659258262890683122, 1.000000000000000000, 0.9659258262890683122, 1.000000000000000000, 0.9659258262890683122, 1.000000000000000000, 0.9659258262890683122, 1.000000000000000000, 0.9659258262890683122, 1.000000000000000000, 0.9659258262890683122, 1.000000000000000000, 0.9659258262890683122, 1.000000000000000000, 0.9659258262890683122, 1.000000000000000000, 0.9659258262890683122, 1.000000000000000000, 0.9659258262890683122, 1.000000000000000000, 0.9659258262890683122, 1.000000000000000000, 0.9659258262890683122, 1.000000000000000000, 0.9659258262890683122, 1.000000000000000000, 0.9659258262890683122, 1.000000000000000000, 0.9659258262890683122, 1.000000000000000000, 0.9659258262890683122, 1.000000000000000000, 0.9659258262890683122, 1.000000000000000000, 0.9659258262890683122, 1.000000000000000000, 0.9659258262890683122, 1.000000000000000000, 0.9659258262890683122, 1.000000000000000000, 0.9659258262890683122, 1.000000000000000000, 0.9659258262890683122, 1.000000000000000000, 0.9659258262890683122, 1.000000000000000000, 0.9659258262890683122, 1.000000000000000000, 0.9659258262890683122, 1.000000000000000000, 0.9659258262890683122, 1.000000000000000000, 0.9659258262890683122, 1.000000000000000000, 0.9659258262890683122, 1.000000000000000000, 0.9659258262890683122, 1.000000000000000000, 0.9659258262890683122, 1.000000000000000000, 0.9659258262890683122, 1.000000000000000000, 0.9659258262890683122, 1.000000000000000000, 0.9659258262890683122, 1.000000000000000000, 0.9659258262890683122, 1.000000000000000000, 0.9659258262890683122, 1.000000000000000000, 0.9659258262890683122, 1.000000000000000000, 0.9659258262890683122, 1.000000000000000000, 0.9659258262890683122, 1.000000000000000000, 0.9659258262890683122, 1.000000000000000000, 0.9659258262890683122, 1.000000000000000000, 0.9659258262890683122, 1.000000000000000000, 0.9659258262890683122, 1.000000000000000000, 0.9659258262890683122, 1.000000000000000000, 0.9659258262890683122, 1.000000000000000000, 0.9659258262890683122, 1.000000000000000000, 0.9659258262890683122, 1.000000000000000000, 0.9659258262890683122, 1.000000000000000000, 0.9659258262890683122, 1.000000000000000000, 0.9659258262890683122, 1.000000000000000000, 0.9659258262890683122, 1.000000000000000000, 0.9659258262890683122, 1.000000000000000000, 0.9659258262890683122, 1.000000000000000000, 0.9659258262890683122, 1.000000000000000000, 0.9659258262890683122, 1.000000000000000000, 0.9659258262890683122, 1.000000000000000000, 0.9659258262890683122, 1.000000000000000000, 0.9659258262890683122, 1.000000000000000000, 0.9659258262890683122, 1.000000000000000000, 0.9659258262890683122, 1.000000000000000000, 0.9659258262890683122, 1.000000000000000000, 0.9659258262890683122, 1.000000000000000000, 0.9659258262890683122, 1.000000000000000000, 0.9659258262890683122, 1.000000000000000000, 0.9659258262890683122, 1.000000000000000000, 0.9659258262890683122, 1.000000000000000000, 0.9659258262890683122, 1.000000000000000000, 0.9659258262890683122, 1.000000000000000000, 0.9659258262890683122, 1.000000000000000000, 0.9659258262890683122, 1.000000000000000000, 0.9659258262890683122, 1.000000000000000000, 0.9659258262890683122, 1.000000000000000000, 0.9659258262890683122, 1.000000000000000000, 0.9659258262890683122, 1.000000000000000000, 0.9659258262890683122, 1.000000000000000000, 0.9659258262890683122, 1.000000000000000000, 0.9659258262890683122, 1.000000000000000000, 0.9659258262890683122, 1.000000000000000000, 0.9659258262890683122, 1.000000000000000000, 0.9659258262890683122, 1.000000000000000000, 0.9659258262890683122, 1.000000000000000000, 0.9659258262890683122, 1.000000000000000000, 0.9659258262890683122, 1.000000000000000000, 0.9659258262890683122, 1.000000000000000000, 0.9659258262890683122, 1.000000000000000000, 0.9659258262890683122, 1.000000000000000000, 0.9659258262890683122, 1.000000000000000000, 0.9659258262890683122, 1.000000000000000000, 0.9659258262890683122, 1.000000000000000000) ) ) 
 REPRESENTATION_ITEM ( '' )  SURFACE ( )  );
#53337 = CARTESIAN_POINT ( 'NONE',  ( -1.220472440944881054, -0.5511811023622047445, 6.969142054262312111E-17 ) ) ;
#53338 = CARTESIAN_POINT ( 'NONE',  ( 0.4724409448818898682, 2.892866454678787531E-17, -0.3523622047244094335 ) ) ;
#53339 = CARTESIAN_POINT ( 'NONE',  ( -1.115485564304461219, -0.004921259842519870586, -0.3153832671262229437 ) ) ;
#53340 = CARTESIAN_POINT ( 'NONE',  ( 0.4323985109340933719, 1.341647856265051564, -1.452992989815209190 ) ) ;
#53341 = CARTESIAN_POINT ( 'NONE',  ( 0.01312335958005323398, -0.4281496062992127816, -0.4176697321401328100 ) ) ;
#53342 = CARTESIAN_POINT ( 'NONE',  ( 2.795275590551181466, 2.793565526369266916, 0.000000000000000000 ) ) ;
#53343 = CARTESIAN_POINT ( 'NONE',  ( 0.4658792650918640033, -0.2845877964562159024, 0.3641732283464567677 ) ) ;
#53344 = CARTESIAN_POINT ( 'NONE',  ( -0.3740157480314953431, -0.4536011799217368745, -0.2665933059059886201 ) ) ;
#53345 = CARTESIAN_POINT ( 'NONE',  ( -0.1574803149606292529, -0.1870078740157480879, -0.4822834645669291653 ) ) ;
#53346 = CARTESIAN_POINT ( 'NONE',  ( -1.725721784776902190, -0.05778040916215522460, 0.4822834645669289988 ) ) ;
#53347 = CARTESIAN_POINT ( 'NONE',  ( -1.095800524934382292, -0.2845877964562161244, -0.3641732283464567121 ) ) ;
#53348 = DIRECTION ( 'NONE',  ( 0.000000000000000000, 0.000000000000000000, 1.000000000000000000 ) ) ;
#53349 = CARTESIAN_POINT ( 'NONE',  ( 0.5577427821522316087, -0.05778040916215522460, 0.4822834645669289988 ) ) ;
#53350 = ORIENTED_EDGE ( 'NONE', *, *, #58379, .T. ) ;
#53351 = CARTESIAN_POINT ( 'NONE',  ( 4.893765752498283308E-17, -0.3996062992125985480, -1.415354330708661346 ) ) ;
#53352 = CARTESIAN_POINT ( 'NONE',  ( -0.3917322834645670104, -7.196005306013484475E-17, -2.486220472440944906 ) ) ;
#53353 = CARTESIAN_POINT ( 'NONE',  ( -0.3346456692913377662, -0.4536011799217367080, 0.2665933059059888421 ) ) ;
#53354 = CARTESIAN_POINT ( 'NONE',  ( -1.437007874015747477, 0.1660481256975883668, -0.3530559997133364547 ) ) ;
#53355 = CARTESIAN_POINT ( 'NONE',  ( 1.666666666666667185, 0.05413385826771666132, 0.4176697321401328100 ) ) ;
#53356 = CARTESIAN_POINT ( 'NONE',  ( -3.909054398717938028, 1.460102366761165449, -0.4683312780462470237 ) ) ;
#53357 = B_SPLINE_CURVE_WITH_KNOTS ( 'NONE', 3,
 ( #45637, #1057, #27123, #26711, #33023, #52787, #71333 ),
 .UNSPECIFIED., .F., .F.,
 ( 4, 3, 4 ),
 ( 6.162975822039154730E-33, 0.001246232571205225159, 0.002492492258783241162 ),
 .UNSPECIFIED. ) ;
#53358 = CARTESIAN_POINT ( 'NONE',  ( -0.5183727034120726440, -0.5511811023622048555, -0.09757992244046775898 ) ) ;
#53359 = CARTESIAN_POINT ( 'NONE',  ( 0.03178304480586199854, -0.3983403474834772418, -9.560572922657961637E-16 ) ) ;
#53360 = CARTESIAN_POINT ( 'NONE',  ( 1.076115485564305141, -0.6046776061558807314, 0.2411417322834647770 ) ) ;
#53361 = CARTESIAN_POINT ( 'NONE',  ( -0.3460692066303960868, 0.1998031496062990242, -0.02624671916010499692 ) ) ;
#53362 = CARTESIAN_POINT ( 'NONE',  ( -0.3392501089628019995, 0.1958661417322831999, -2.700150549377639653 ) ) ;
#53363 = CARTESIAN_POINT ( 'NONE',  ( 0.4602855208775837870, 1.653389129435537175, -2.586148212265404922 ) ) ;
#53364 = CARTESIAN_POINT ( 'NONE',  ( -1.719160104986876103, 0.05413385826771666132, 0.4176697321401328100 ) ) ;
#53365 = CARTESIAN_POINT ( 'NONE',  ( -1.161417322834644716, -0.5400638737290845981, -0.3530559997133363437 ) ) ;
#53366 = CARTESIAN_POINT ( 'NONE',  ( 1.391076115485564868, -0.6046776061558807314, 0.2411417322834647770 ) ) ;
#53367 = CARTESIAN_POINT ( 'NONE',  ( 0.2867679344610365999, -0.2867679344610365444, -2.545275590551181022 ) ) ;
#53368 = CARTESIAN_POINT ( 'NONE',  ( 0.6167979002624679463, 0.05413385826771626580, -0.4176697321401330321 ) ) ;
#53369 = CARTESIAN_POINT ( 'NONE',  ( -0.2034120734908128059, 0.2952755905511811885, 0.1292274648535926551 ) ) ;
#53370 = CARTESIAN_POINT ( 'NONE',  ( 3.937007874015748143, 2.165354330708661568, 0.3149606299212600047 ) ) ;
#53371 = CIRCLE ( 'NONE', #6325, 0.3129921259842520787 ) ;
#53372 = AXIS2_PLACEMENT_3D ( 'NONE', #58580, #14414, #53512 ) ;
#53374 = CARTESIAN_POINT ( 'NONE',  ( 0.06680712611108469146, -6.211426067506147994E-17, -0.3627989612356148363 ) ) ;
#53373 = CIRCLE ( 'NONE', #28610, 0.3937007874015748254 ) ;
#53375 = CARTESIAN_POINT ( 'NONE',  ( 0.9186351706036751663, -0.5023911411419708095, 0.1820866141732285504 ) ) ;
#53376 = VERTEX_POINT ( 'NONE', #81659 ) ;
#53377 = CARTESIAN_POINT ( 'NONE',  ( 0.3392501089628018329, 0.1958661417322835607, -0.2854523866479808936 ) ) ;
#53378 = ORIENTED_EDGE ( 'NONE', *, *, #81012, .T. ) ;
#53379 = CARTESIAN_POINT ( 'NONE',  ( -0.3346456692913377662, -0.5400638737290844871, 0.3530559997133364547 ) ) ;
#53380 = PRODUCT_DEFINITION_SHAPE ( 'NONE', 'NONE',  #83317 ) ;
#53381 = CARTESIAN_POINT ( 'NONE',  ( 1.279527559055118724, 0.1660481256975885056, 0.3530559997133364547 ) ) ;
#53382 = CARTESIAN_POINT ( 'NONE',  ( 0.1377952755905518800, 0.1660481256975883668, -0.3530559997133364547 ) ) ;
#53383 = CARTESIAN_POINT ( 'NONE',  ( -0.4658792650918627265, -0.2845877964562161244, -0.3641732283464567121 ) ) ;
#53384 = CARTESIAN_POINT ( 'NONE',  ( 1.292650918635171564, -0.6692913385826773087, -0.1292274648535924053 ) ) ;
#53385 = CARTESIAN_POINT ( 'NONE',  ( -1.030183727034119867, -0.3162353388693405765, 0.4822834645669290543 ) ) ;
#53386 = CARTESIAN_POINT ( 'NONE',  ( 0.1181102362204730916, -0.6692913385826771977, 8.415575281601705876E-17 ) ) ;
#53387 = CARTESIAN_POINT ( 'NONE',  ( -0.9120734908136475250, 0.2952755905511811885, 0.1292274648535926551 ) ) ;
#53388 = CARTESIAN_POINT ( 'NONE',  ( 1.351706036745407458, -0.4281496062992127816, -0.4176697321401328100 ) ) ;
#53389 = CARTESIAN_POINT ( 'NONE',  ( 0.8005249343832027131, 0.05413385826771666132, 0.4176697321401328100 ) ) ;
#53390 = CARTESIAN_POINT ( 'NONE',  ( 1.076115485564305141, 0.2306618581243847221, -0.2411417322834647770 ) ) ;
#53391 = CARTESIAN_POINT ( 'NONE',  ( -0.1958661417322836718, 0.3392501089628017219, -0.7926509186351704539 ) ) ;
#53392 = CARTESIAN_POINT ( 'NONE',  ( 0.09186351706036827158, -0.004921259842519576551, 0.3153832671262227771 ) ) ;
#53393 = VERTEX_POINT ( 'NONE', #42494 ) ;
#53394 = CARTESIAN_POINT ( 'NONE',  ( 0.1058382717557500713, -0.3949938075777409408, -1.030183727034120755 ) ) ;
#53395 = VERTEX_POINT ( 'NONE', #23970 ) ;
#53396 = CARTESIAN_POINT ( 'NONE',  ( -0.6627296587926503335, -0.5511811023622046335, 0.09757992244046803654 ) ) ;
#53397 = CARTESIAN_POINT ( 'NONE',  ( -0.05905511811023545637, 0.1660481256975885056, 0.3530559997133364547 ) ) ;
#53398 = LINE ( 'NONE', #79516, #9919 ) ;
#53399 = CARTESIAN_POINT ( 'NONE',  ( -0.08530183727034056085, -0.05778040916215560624, -0.4822834645669293319 ) ) ;
#53400 = CARTESIAN_POINT ( 'NONE',  ( -0.3280839895013117347, -0.4281496062992124485, 0.4176697321401328655 ) ) ;
#53401 = CARTESIAN_POINT ( 'NONE',  ( -1.003937007874014853, 0.1660481256975885056, 0.3530559997133364547 ) ) ;
#53402 = CARTESIAN_POINT ( 'NONE',  ( -1.128608923884513837, -0.6046776061558807314, 0.2411417322834647770 ) ) ;
#53403 = CARTESIAN_POINT ( 'NONE',  ( 1.332020997375329197, -0.2845877964562159024, 0.3641732283464567677 ) ) ;
#53404 = CARTESIAN_POINT ( 'NONE',  ( -1.496062992125983815, -0.1870078740157479769, 0.4822834645669291653 ) ) ;
#53405 = DIRECTION ( 'NONE',  ( 1.000000000000000000, -1.734723475976808080E-16, 1.047444401652940007E-14 ) ) ;
#53406 = CARTESIAN_POINT ( 'NONE',  ( 0.5380577427821529035, -0.004921259842519870586, -0.3153832671262229437 ) ) ;
#53407 = CARTESIAN_POINT ( 'NONE',  ( 0.03280839895013198948, -0.6692913385826773087, -0.1292274648535924053 ) ) ;
#53408 = CARTESIAN_POINT ( 'NONE',  ( 0.2690288713910767848, 0.2952755905511811885, 0.1292274648535926551 ) ) ;
#53409 = ORIENTED_EDGE ( 'NONE', *, *, #61921, .F. ) ;
#53410 = CARTESIAN_POINT ( 'NONE',  ( 0.3996062992125986035, 0.1070741851644054776, -1.541994750656167978 ) ) ;
#53411 = CARTESIAN_POINT ( 'NONE',  ( 0.3460692066303958092, 0.1998031496062993018, -1.152887139107611425 ) ) ;
#53412 = CARTESIAN_POINT ( 'NONE',  ( 0.2925321140481932369, 0.2925321140481932369, -0.3720472440944882497 ) ) ;
#53413 = CARTESIAN_POINT ( 'NONE',  ( -0.4461942257217840213, 0.2306618581243848609, 0.2411417322834645549 ) ) ;
#53414 = CARTESIAN_POINT ( 'NONE',  ( 0.3458507752293908943, 0.3458507752293908943, 0.01968503937007874335 ) ) ;
#53415 = CARTESIAN_POINT ( 'NONE',  ( -0.3392501089628017219, -0.1958661417322836718, -2.184383202099737797 ) ) ;
#53416 = CARTESIAN_POINT ( 'NONE',  ( -1.463254593175852492, 0.1771653543307087630, 0.09757992244046791164 ) ) ;
#53417 = CARTESIAN_POINT ( 'NONE',  ( 0.7349081364829402885, -0.6046776061558809534, -0.2411417322834644161 ) ) ;
#53418 = CARTESIAN_POINT ( 'NONE',  ( 0.8005249343832028242, -0.4281496062992127816, -0.4176697321401328100 ) ) ;
#53419 = CARTESIAN_POINT ( 'NONE',  ( -0.2887139107611542133, -0.5023911411419708095, -0.1820866141732282451 ) ) ;
#53420 = CARTESIAN_POINT ( 'NONE',  ( 0.2034120734908142214, 0.2952755905511810774, -0.1292274648535930714 ) ) ;
#53421 = CARTESIAN_POINT ( 'NONE',  ( 0.2362204724409451007, -0.4091458600556402980, -1.900918635170603554 ) ) ;
#53422 = CARTESIAN_POINT ( 'NONE',  ( -0.1049868766404193215, -0.5023911411419708095, 0.1820866141732285504 ) ) ;
#53423 = CARTESIAN_POINT ( 'NONE',  ( -0.2296587926509179312, -0.3162353388693409650, -0.4822834645669289433 ) ) ;
#53424 = ADVANCED_FACE ( 'NONE', ( #69005 ), #37014, .T. ) ;
#53425 = CARTESIAN_POINT ( 'NONE',  ( -0.3949938075777409963, -7.255918531996591613E-17, -1.218503937007874072 ) ) ;
#53426 = CARTESIAN_POINT ( 'NONE',  ( 1.594488188976378673, 0.07958543189024085140, 0.2665933059059887866 ) ) ;
#53427 = CARTESIAN_POINT ( 'NONE',  ( -0.07217847769028813698, -0.2845877964562161244, -0.3641732283464567121 ) ) ;
#53428 = CARTESIAN_POINT ( 'NONE',  ( 1.522309711286089939, 0.1283753931104748280, 0.1820866141732283561 ) ) ;
#53429 = CARTESIAN_POINT ( 'NONE',  ( -0.6955380577427815458, -0.4281496062992127816, -0.4176697321401328100 ) ) ;
#53430 = CARTESIAN_POINT ( 'NONE',  ( -0.6758530183727028406, 0.1771653543307087630, 0.09757992244046791164 ) ) ;
#53431 = CARTESIAN_POINT ( 'NONE',  ( -0.4091458600556405756, 0.2362204724409446288, -2.307742782152230721 ) ) ;
#53432 = CARTESIAN_POINT ( 'NONE',  ( -0.5511811023622041894, -0.1870078740157480879, -0.4822834645669291653 ) ) ;
#53433 = CARTESIAN_POINT ( 'NONE',  ( -0.6364829396325453192, -0.05778040916215560624, -0.4822834645669293319 ) ) ;
#53434 = CARTESIAN_POINT ( 'NONE',  ( -0.1968503937007867743, 0.2952755905511811885, 0.000000000000000000 ) ) ;
#53435 = CARTESIAN_POINT ( 'NONE',  ( -0.3460692066303960313, 0.1998031496062989965, -2.622703412073490892 ) ) ;
#53436 = CARTESIAN_POINT ( 'NONE',  ( -9.594673741351310580E-17, 0.3917322834645669549, -1.969796957184039909 ) ) ;
#53437 = CARTESIAN_POINT ( 'NONE',  ( 0.5314960629920854052, 2.746034003362845866, 3.861376881555345086 ) ) ;
#53438 = CARTESIAN_POINT ( 'NONE',  ( 0.6233595800524942554, -0.08942795157528024563, -0.3641732283464568787 ) ) ;
#53439 = CARTESIAN_POINT ( 'NONE',  ( 1.528871391076116026, -0.6692913385826773087, -0.1292274648535924053 ) ) ;
#53440 = CARTESIAN_POINT ( 'NONE',  ( -1.423884514435694859, -0.2845877964562159024, 0.3641732283464567677 ) ) ;
#53441 = CARTESIAN_POINT ( 'NONE',  ( 1.299212598425197429, -0.6692913385826771977, 8.415575281601705876E-17 ) ) ;
#53442 = CARTESIAN_POINT ( 'NONE',  ( -0.9908136482939626788, -0.5511811023622048555, -0.09757992244046775898 ) ) ;
#53443 = CARTESIAN_POINT ( 'NONE',  ( -0.5971128608923877978, 0.2952755905511811885, 0.1292274648535926551 ) ) ;
#53444 = CARTESIAN_POINT ( 'NONE',  ( 0.1837270341207357105, -0.5023911411419708095, -0.1820866141732282451 ) ) ;
#53445 = CARTESIAN_POINT ( 'NONE',  ( 1.611560603071419129, 0.2819760470925486984, 0.1148666718267763592 ) ) ;
#53446 = CARTESIAN_POINT ( 'NONE',  ( 1.135170603674541256, 0.1771653543307087630, 0.09757992244046791164 ) ) ;
#53447 = CARTESIAN_POINT ( 'NONE',  ( 0.2690288713910767848, 0.2952755905511811885, 0.1292274648535926551 ) ) ;
#53448 = CARTESIAN_POINT ( 'NONE',  ( -0.2925321140481932369, 0.2925321140481931259, -0.4114173228346455491 ) ) ;
#53449 = CARTESIAN_POINT ( 'NONE',  ( -0.7677165354330699465, 0.1660481256975885056, 0.3530559997133364547 ) ) ;
#53450 = CARTESIAN_POINT ( 'NONE',  ( -0.3392501089628017219, -0.1958661417322836718, -1.239501312335958172 ) ) ;
#53451 = CARTESIAN_POINT ( 'NONE',  ( 1.043307086614173818, -0.4536011799217368745, -0.2665933059059886201 ) ) ;
#53452 = CARTESIAN_POINT ( 'NONE',  ( 0.2887139107611556010, 0.2306618581243847221, -0.2411417322834647770 ) ) ;
#53453 = CARTESIAN_POINT ( 'NONE',  ( -0.2559055118110227234, -0.5400638737290844871, 0.3530559997133364547 ) ) ;
#53454 = CARTESIAN_POINT ( 'NONE',  ( 0.1771653543307093182, -0.4536011799217368745, -0.2665933059059886201 ) ) ;
#53455 = CARTESIAN_POINT ( 'NONE',  ( -1.313877454013331780, 1.062992125984252079, 0.7983292792091805090 ) ) ;
#53456 = CARTESIAN_POINT ( 'NONE',  ( 0.03280839895013198948, -0.5511811023622048555, -0.09757992244046775898 ) ) ;
#53457 = CARTESIAN_POINT ( 'NONE',  ( 0.1640419947506569498, -0.3162353388693409650, -0.4822834645669289433 ) ) ;
#53458 = CARTESIAN_POINT ( 'NONE',  ( -0.9317585301837263412, -0.004921259842519576551, 0.3153832671262227771 ) ) ;
#53459 = CARTESIAN_POINT ( 'NONE',  ( 0.1070741851644053388, 0.3996062992125986035, -0.8576115485564304031 ) ) ;
#53460 = CARTESIAN_POINT ( 'NONE',  ( -1.017060367454067249, -0.05778040916215522460, 0.4822834645669289988 ) ) ;
#53461 = CARTESIAN_POINT ( 'NONE',  ( 2.795275590551181466, 0.7874015748031495399, -2.695814348275282069E-16 ) ) ;
#53462 = EDGE_LOOP ( 'NONE', ( #43138, #73181, #7660, #48817 ) ) ;
#53463 = CARTESIAN_POINT ( 'NONE',  ( -1.108923884514435132, -0.2845877964562159024, 0.3641732283464567677 ) ) ;
#53464 = CARTESIAN_POINT ( 'NONE',  ( -0.04593175853018302557, -0.6692913385826773087, -0.1292274648535924053 ) ) ;
#53465 = CARTESIAN_POINT ( 'NONE',  ( -1.548556430446193399, 0.2306618581243848609, 0.2411417322834645549 ) ) ;
#53466 = CARTESIAN_POINT ( 'NONE',  ( -0.7742782152230962556, -0.4281496062992127816, -0.4176697321401328100 ) ) ;
#53467 = CARTESIAN_POINT ( 'NONE',  ( -1.614173228346457378, 2.157411728916712068, -0.1372047244094477536 ) ) ;
#53469 = CARTESIAN_POINT ( 'NONE',  ( 1.089238845144357537, -0.4281496062992124485, 0.4176697321401328655 ) ) ;
#53468 = CARTESIAN_POINT ( 'NONE',  ( 1.049868766404200349, 0.2306618581243848609, 0.2411417322834645549 ) ) ;
#53470 = CARTESIAN_POINT ( 'NONE',  ( 0.7611548556430454138, 0.2306618581243847221, -0.2411417322834647770 ) ) ;
#53471 = CARTESIAN_POINT ( 'NONE',  ( -0.3392501089628017219, -0.1958661417322836718, -2.721784776902886893 ) ) ;
#53472 = CARTESIAN_POINT ( 'NONE',  ( 1.469816272965879911, 0.2306618581243847221, -0.2411417322834647770 ) ) ;
#53473 = CARTESIAN_POINT ( 'NONE',  ( -1.338582677165353729, -0.1870078740157480879, -0.4822834645669291653 ) ) ;
#53474 = CARTESIAN_POINT ( 'NONE',  ( 0.3996062992125986035, 0.1070741851644054776, -0.4396325459317584339 ) ) ;
#53475 = VERTEX_POINT ( 'NONE', #82065 ) ;
#53476 = CARTESIAN_POINT ( 'NONE',  ( -0.3740157480314953431, 0.07958543189024085140, 0.2665933059059887866 ) ) ;
#53477 = CARTESIAN_POINT ( 'NONE',  ( 0.2867679344610365999, 0.2867679344610365999, -2.334645669291338432 ) ) ;
#53478 = EDGE_LOOP ( 'NONE', ( #43627, #74920, #29341, #40843, #37338, #33548, #58134, #59780 ) ) ;
#53479 = CARTESIAN_POINT ( 'NONE',  ( 0.8792650918635177559, -0.4281496062992127816, -0.4176697321401328100 ) ) ;
#53480 = CARTESIAN_POINT ( 'NONE',  ( -0.1115485564304456306, 0.2952755905511810774, -0.1292274648535930714 ) ) ;
#53481 = CARTESIAN_POINT ( 'NONE',  ( -0.8136482939632537770, 0.2306618581243847221, -0.2411417322834647770 ) ) ;
#53482 = CARTESIAN_POINT ( 'NONE',  ( 1.673228346456693494, 0.1660481256975885056, 0.3530559997133364547 ) ) ;
#53483 = CARTESIAN_POINT ( 'NONE',  ( -1.069553805774277722, -0.5511811023622048555, -0.09757992244046775898 ) ) ;
#53484 = CARTESIAN_POINT ( 'NONE',  ( 5.785732909357575061E-17, -0.4724409448818898682, -2.045275590551181022 ) ) ;
#53485 = CARTESIAN_POINT ( 'NONE',  ( 0.5249343832021005074, -0.6046776061558807314, 0.2411417322834647770 ) ) ;
#53486 = CARTESIAN_POINT ( 'NONE',  ( 0.6299212598425204535, -0.1870078740157479769, 0.3641732283464567677 ) ) ;
#53487 = CARTESIAN_POINT ( 'NONE',  ( -0.5577427821522301654, -0.3162353388693405765, 0.4822834645669290543 ) ) ;
#53488 = CARTESIAN_POINT ( 'NONE',  ( 0.2867679344610365999, 0.2867679344610365999, -1.635151287892701255 ) ) ;
#53489 = CARTESIAN_POINT ( 'NONE',  ( -1.325459317585300889, 0.05413385826771666132, 0.4176697321401328100 ) ) ;
#53490 = ADVANCED_BREP_SHAPE_REPRESENTATION ( '', ( #33421, #22098 ), #46360 ) ;
#53491 = DIRECTION ( 'NONE',  ( -1.000000000000000000, -3.469446951953613696E-16, 0.000000000000000000 ) ) ;
#53492 = CARTESIAN_POINT ( 'NONE',  ( 1.253280839895013710, -0.05778040916215560624, -0.4822834645669293319 ) ) ;
#53493 = CARTESIAN_POINT ( 'NONE',  ( 1.391076115485564868, 0.1283753931104746893, -0.1820866141732285504 ) ) ;
#53494 = ORIENTED_EDGE ( 'NONE', *, *, #54568, .F. ) ;
#53495 = CARTESIAN_POINT ( 'NONE',  ( -0.1958661417322833942, -0.3392501089628018884, -2.739520628117797063 ) ) ;
#53496 = CARTESIAN_POINT ( 'NONE',  ( -0.3018372703412066094, -0.4281496062992127816, -0.4176697321401328100 ) ) ;
#53497 = ORIENTED_EDGE ( 'NONE', *, *, #30564, .T. ) ;
#53498 = AXIS2_PLACEMENT_3D ( 'NONE', #42072, #74912, #23130 ) ;
#53499 = CARTESIAN_POINT ( 'NONE',  ( 0.6758530183727039509, 0.1771653543307087075, -0.09757992244046823083 ) ) ;
#53500 = CARTESIAN_POINT ( 'NONE',  ( -1.141732283464566011, -0.6692913385826771977, 8.415575281601705876E-17 ) ) ;
#53501 = CARTESIAN_POINT ( 'NONE',  ( 0.9776902887139113929, 0.2952755905511811885, 0.1292274648535926551 ) ) ;
#53502 = CARTESIAN_POINT ( 'NONE',  ( 0.9711286089238851948, 0.2306618581243848609, 0.2411417322834645549 ) ) ;
#53503 = CARTESIAN_POINT ( 'NONE',  ( 0.1377952755905518800, -0.5400638737290844871, 0.3530559997133364547 ) ) ;
#53504 = CARTESIAN_POINT ( 'NONE',  ( -0.5314960629921250401, 0.1660481256975885056, 0.3530559997133364547 ) ) ;
#53505 = CARTESIAN_POINT ( 'NONE',  ( -0.3392501089628017219, -0.1958661417322836718, -1.869422572178477848 ) ) ;
#53506 = CARTESIAN_POINT ( 'NONE',  ( 1.555118110236221041, -0.4536011799217367080, 0.2665933059059888421 ) ) ;
#53507 = CARTESIAN_POINT ( 'NONE',  ( -0.5905511811023613777, -0.6692913385826771977, 8.415575281601705876E-17 ) ) ;
#53508 = CARTESIAN_POINT ( 'NONE',  ( -0.5577427821522301654, -0.2845877964562159024, 0.3641732283464567677 ) ) ;
#53509 = CARTESIAN_POINT ( 'NONE',  ( 1.679790026246720025, 0.2306618581243848609, 0.2411417322834645549 ) ) ;
#53510 = LINE ( 'NONE', #29088, #55847 ) ;
#53511 = CARTESIAN_POINT ( 'NONE',  ( -0.5380577427821514602, -0.4281496062992127816, -0.4176697321401328100 ) ) ;
#53512 = DIRECTION ( 'NONE',  ( 0.000000000000000000, -0.000000000000000000, -1.000000000000000000 ) ) ;
#53513 = CARTESIAN_POINT ( 'NONE',  ( 0.8792650918635177559, -0.4281496062992127816, -0.4176697321401328100 ) ) ;
#53514 = CARTESIAN_POINT ( 'NONE',  ( -9.787531504996567848E-17, 0.3996062992125986035, -2.047244094488188892 ) ) ;
#53515 = CARTESIAN_POINT ( 'NONE',  ( 3.924581109467853324, 1.180375947577095408, 0.3127951191726855429 ) ) ;
#53516 = EDGE_CURVE ( 'NONE', #63931, #37370, #5442, .T. ) ;
#53517 = CARTESIAN_POINT ( 'NONE',  ( -0.2099737532808391705, 0.2306618581243848609, 0.2411417322834645549 ) ) ;
#53519 = CARTESIAN_POINT ( 'NONE',  ( -1.646051170424378096, 0.000000000000000000, -0.3464511005275205946 ) ) ;
#53518 = CARTESIAN_POINT ( 'NONE',  ( 1.233595800524935227, 0.1283753931104746893, -0.1820866141732285504 ) ) ;
#53520 = CARTESIAN_POINT ( 'NONE',  ( 0.4091458600556404646, -0.2362204724409448231, -0.8116797900262466836 ) ) ;
#53521 = CARTESIAN_POINT ( 'NONE',  ( 1.384514435695538559, 0.1771653543307087075, -0.09757992244046823083 ) ) ;
#53522 = CARTESIAN_POINT ( 'NONE',  ( 1.141732283464567566, 0.2952755905511811885, 0.000000000000000000 ) ) ;
#53523 = CARTESIAN_POINT ( 'NONE',  ( 0.1974969037888706092, -0.3420746716998660508, -0.1686351706036745279 ) ) ;
#53524 = CARTESIAN_POINT ( 'NONE',  ( -0.4199475065616791736, 0.2306618581243847221, -0.2411417322834647770 ) ) ;
#53525 = CARTESIAN_POINT ( 'NONE',  ( -1.541994750656167090, -0.6692913385826773087, -0.1292274648535924053 ) ) ;
#53526 = CARTESIAN_POINT ( 'NONE',  ( -1.391076115485563758, 0.2306618581243848609, 0.2411417322834645549 ) ) ;
#53527 = CARTESIAN_POINT ( 'NONE',  ( -0.01312335958005186876, -0.4281496062992124485, 0.4176697321401328655 ) ) ;
#53528 = CARTESIAN_POINT ( 'NONE',  ( 0.3420746716998660508, -0.1974969037888704149, -0.6541994750656167090 ) ) ;
#53529 = CARTESIAN_POINT ( 'NONE',  ( 1.095800524934383846, -0.05778040916215560624, -0.4822834645669293319 ) ) ;
#53530 = CARTESIAN_POINT ( 'NONE',  ( 0.4002624671916016896, -0.3162353388693409650, -0.4822834645669289433 ) ) ;
#53531 = CARTESIAN_POINT ( 'NONE',  ( 0.5380577427821529035, -0.3690944881889763329, 0.3153832671262228327 ) ) ;
#53532 = CARTESIAN_POINT ( 'NONE',  ( 5.785732909357575061E-17, -0.4724409448818898682, -0.1555118110236220763 ) ) ;
#53533 = CARTESIAN_POINT ( 'NONE',  ( 0.5577427821522316087, -0.08942795157527998196, 0.3641732283464567121 ) ) ;
#53534 = CARTESIAN_POINT ( 'NONE',  ( -1.561679790026246017, -0.4281496062992127816, -0.4176697321401328100 ) ) ;
#53535 = CARTESIAN_POINT ( 'NONE',  ( -0.1998031496062994405, 0.3460692066303957537, -1.507217847769029007 ) ) ;
#53536 = CARTESIAN_POINT ( 'NONE',  ( 0.9448818897637802916, -0.1870078740157480879, -0.4822834645669291653 ) ) ;
#53537 = CARTESIAN_POINT ( 'NONE',  ( 0.2867679344610365999, -0.2867679344610365444, -0.8779527559055116948 ) ) ;
#53538 = DIRECTION ( 'NONE',  ( -0.000000000000000000, 1.000000000000000000, -1.408710688920637755E-15 ) ) ;
#53539 = CARTESIAN_POINT ( 'NONE',  ( -0.4724409448818898682, -8.678599364036362592E-17, -2.320866141732283783 ) ) ;
#53540 = CARTESIAN_POINT ( 'NONE',  ( 0.01968503937007930540, 0.07958543189024085140, 0.2665933059059887866 ) ) ;
#53541 = CARTESIAN_POINT ( 'NONE',  ( 0.6036745406824154392, 0.2306618581243847221, -0.2411417322834647770 ) ) ;
#53542 = CARTESIAN_POINT ( 'NONE',  ( 1.286089238845145033, -0.5023911411419708095, -0.1820866141732282451 ) ) ;
#53543 = CARTESIAN_POINT ( 'NONE',  ( -1.299212598425196097, -0.5511811023622047445, 6.969142054262312111E-17 ) ) ;
#53544 = CARTESIAN_POINT ( 'NONE',  ( -0.9842519685039365918, -0.6692913385826771977, 8.415575281601705876E-17 ) ) ;
#53545 = CARTESIAN_POINT ( 'NONE',  ( -1.686351706036744558, 0.2952755905511810774, -0.1292274648535930714 ) ) ;
#53546 = CARTESIAN_POINT ( 'NONE',  ( 0.5052493438320218022, -0.6692913385826773087, -0.1292274648535924053 ) ) ;
#53547 = CARTESIAN_POINT ( 'NONE',  ( 1.463254593175853824, -0.6692913385826771977, 0.1292274648535927661 ) ) ;
#53548 = CARTESIAN_POINT ( 'NONE',  ( 0.5120078740157480990, 0.000000000000000000, -1.512162153811850596 ) ) ;
#53549 = CARTESIAN_POINT ( 'NONE',  ( 0.7414698162729663755, -0.6692913385826773087, -0.1292274648535924053 ) ) ;
#53550 = CARTESIAN_POINT ( 'NONE',  ( -0.2362204724409451284, 0.4091458600556402425, -2.767060367454068359 ) ) ;
#53551 = CARTESIAN_POINT ( 'NONE',  ( 1.568241469816273659, -0.05778040916215560624, -0.4822834645669293319 ) ) ;
#53552 = CARTESIAN_POINT ( 'NONE',  ( 1.246719160104987623, 0.05413385826771626580, -0.4176697321401330321 ) ) ;
#53553 = CARTESIAN_POINT ( 'NONE',  ( -1.253280839895012377, -0.08942795157527998196, 0.3641732283464567121 ) ) ;
#53554 = CARTESIAN_POINT ( 'NONE',  ( 1.299212598425197429, -0.5511811023622047445, 6.969142054262312111E-17 ) ) ;
#53555 = CARTESIAN_POINT ( 'NONE',  ( -1.279527559055116948, 0.07958543189024071263, -0.2665933059059888421 ) ) ;
#53556 = CARTESIAN_POINT ( 'NONE',  ( -0.8661417322834640276, -0.1870078740157479769, 0.3641732283464567677 ) ) ;
#53557 = CARTESIAN_POINT ( 'NONE',  ( -3.937007874015748143, 2.755905511811024056, -0.5314960629921260393 ) ) ;
#53558 = CARTESIAN_POINT ( 'NONE',  ( 0.6167979002624678353, -0.3690944881889763329, 0.3153832671262228327 ) ) ;
#53559 = CARTESIAN_POINT ( 'NONE',  ( 0.2230971128608932319, -0.4281496062992124485, 0.4176697321401328655 ) ) ;
#53560 = CARTESIAN_POINT ( 'NONE',  ( 1.076115485564305141, -0.6046776061558807314, 0.2411417322834647770 ) ) ;
#53561 = CARTESIAN_POINT ( 'NONE',  ( 0.05905511811023709395, -0.5400638737290844871, 0.3530559997133364547 ) ) ;
#53562 = CARTESIAN_POINT ( 'NONE',  ( 0.04593175853018440641, 0.1771653543307087075, -0.09757992244046823083 ) ) ;
#53563 = CARTESIAN_POINT ( 'NONE',  ( 1.089238845144357537, -0.4281496062992124485, 0.4176697321401328655 ) ) ;
#53564 = CARTESIAN_POINT ( 'NONE',  ( -0.2230971128608915666, 0.009842519685039467087, 0.3409548833797002021 ) ) ;
#53565 = CARTESIAN_POINT ( 'NONE',  ( -0.9908136482939626788, -0.6692913385826773087, -0.1292274648535924053 ) ) ;
#53566 = CARTESIAN_POINT ( 'NONE',  ( 0.1070741851644054915, -0.3996062992125985480, -0.7152230971128609172 ) ) ;
#53567 = CARTESIAN_POINT ( 'NONE',  ( 1.011689015874864372, 1.456472319277303872E-16, -0.3627989612356145588 ) ) ;
#53568 = CARTESIAN_POINT ( 'NONE',  ( -0.8202099737532799750, 0.2952755905511810774, -0.1292274648535930714 ) ) ;
#53569 = CARTESIAN_POINT ( 'NONE',  ( -0.2427821522309703550, -0.05778040916215560624, -0.4822834645669293319 ) ) ;
#53570 = CARTESIAN_POINT ( 'NONE',  ( 0.3460692066303959757, -0.1998031496062991907, -2.467191601049868677 ) ) ;
#53571 = CARTESIAN_POINT ( 'NONE',  ( -0.3949938075777411628, 0.1058382717557497937, -2.395013123359580387 ) ) ;
#53572 = ORIENTED_EDGE ( 'NONE', *, *, #16744, .F. ) ;
#53573 = CARTESIAN_POINT ( 'NONE',  ( -0.2867679344610364334, -0.2867679344610367109, -0.9960629921259842590 ) ) ;
#53574 = CARTESIAN_POINT ( 'NONE',  ( 3.881246834694716874, 2.729333734409945755, -0.5314960629921260393 ) ) ;
#53575 = CARTESIAN_POINT ( 'NONE',  ( -1.253280839895012377, -0.08942795157527998196, 0.3641732283464567121 ) ) ;
#53576 = CARTESIAN_POINT ( 'NONE',  ( -0.3392501089628017219, -0.1958661417322836718, -1.146981627296587813 ) ) ;
#53577 = CARTESIAN_POINT ( 'NONE',  ( -1.587926509186350810, -0.4281496062992124485, 0.4176697321401328655 ) ) ;
#53578 = CARTESIAN_POINT ( 'NONE',  ( 0.3392501089628018329, -0.1958661417322834497, 0.1299405756243587895 ) ) ;
#53579 = CARTESIAN_POINT ( 'NONE',  ( -0.1115485564304453947, -0.6692913385826771977, 0.1292274648535927661 ) ) ;
#53580 = CARTESIAN_POINT ( 'NONE',  ( -0.5249343832020990641, -0.5023911411419708095, -0.1820866141732282451 ) ) ;
#53581 = CARTESIAN_POINT ( 'NONE',  ( 0.7939632545931766261, -0.05778040916215522460, 0.4822834645669289988 ) ) ;
#53582 = CARTESIAN_POINT ( 'NONE',  ( 0.5052493438320215802, 0.2952755905511811885, 0.1292274648535926551 ) ) ;
#53583 = CARTESIAN_POINT ( 'NONE',  ( 0.3763565203970011264, 1.248168874848284426, 1.057096006133714017 ) ) ;
#53584 = CARTESIAN_POINT ( 'NONE',  ( -0.3460692066303960868, 0.1998031496062990242, -2.545931758530183497 ) ) ;
#53585 = CARTESIAN_POINT ( 'NONE',  ( 0.1958661417322834775, 0.3392501089628018884, -1.400937950952442668 ) ) ;
#53586 = CARTESIAN_POINT ( 'NONE',  ( 1.227034120734908917, 0.2952755905511810774, -0.1292274648535930714 ) ) ;
#53587 = CARTESIAN_POINT ( 'NONE',  ( -0.1181102362204717315, 0.2952755905511811885, 0.000000000000000000 ) ) ;
#53588 = CARTESIAN_POINT ( 'NONE',  ( -0.8333333333333323711, 0.2952755905511811885, 0.1292274648535926551 ) ) ;
#53589 = CARTESIAN_POINT ( 'NONE',  ( 1.568241469816273437, -0.3162353388693405765, 0.4822834645669290543 ) ) ;
#53590 = CARTESIAN_POINT ( 'NONE',  ( 0.7874015748031503170, -0.1870078740157480879, -0.4822834645669291653 ) ) ;
#53591 = CARTESIAN_POINT ( 'NONE',  ( 0.2867679344610365999, -0.2867679344610365444, -0.6555118110236222151 ) ) ;
#53592 = CARTESIAN_POINT ( 'NONE',  ( -0.006561679790025524116, -0.3162353388693405765, 0.4822834645669290543 ) ) ;
#53593 = CARTESIAN_POINT ( 'NONE',  ( 0.6233595800524942554, -0.05778040916215560624, -0.4822834645669293319 ) ) ;
#53594 = CARTESIAN_POINT ( 'NONE',  ( 0.1312335958005257930, 0.2306618581243847221, -0.2411417322834647770 ) ) ;
#53595 = CARTESIAN_POINT ( 'NONE',  ( 0.7020997375328090762, -0.2845877964562159024, 0.3641732283464567677 ) ) ;
#53596 = CARTESIAN_POINT ( 'NONE',  ( -1.456692913385826182, -0.6692913385826771977, 8.415575281601705876E-17 ) ) ;
#53597 = CARTESIAN_POINT ( 'NONE',  ( -1.207349081364828880, 0.2306618581243847221, -0.2411417322834647770 ) ) ;
#53598 = CARTESIAN_POINT ( 'NONE',  ( 0.9383202099737536495, -0.3162353388693405765, 0.4822834645669290543 ) ) ;
#53599 = CARTESIAN_POINT ( 'NONE',  ( -0.2881610400570164265, -0.2661962643049016197, -1.929133858267716883 ) ) ;
#53600 = CARTESIAN_POINT ( 'NONE',  ( -9.594673741351313045E-17, 0.3917322834645670104, -2.354330708661417138 ) ) ;
#53601 = EDGE_LOOP ( 'NONE', ( #43213, #9312, #42432, #50555 ) ) ;
#53602 = CARTESIAN_POINT ( 'NONE',  ( 0.1070741851644054915, -0.3996062992125986035, -0.4002624671916010235 ) ) ;
#53603 = ORIENTED_EDGE ( 'NONE', *, *, #37540, .F. ) ;
#53604 = B_SPLINE_CURVE_WITH_KNOTS ( 'NONE', 3,
 ( #57655, #13479, #17, #52591 ),
 .UNSPECIFIED., .F., .F.,
 ( 4, 4 ),
 ( 0.1795298335526531730, 0.1809577925700029677 ),
 .UNSPECIFIED. ) ;
#53605 = CARTESIAN_POINT ( 'NONE',  ( 0.9317585301837276734, 0.05413385826771626580, -0.4176697321401330321 ) ) ;
#53606 = CARTESIAN_POINT ( 'NONE',  ( 0.4986876640419954376, 0.1283753931104748280, 0.1820866141732283561 ) ) ;
#53607 = CARTESIAN_POINT ( 'NONE',  ( 0.000000000000000000, 2.559055118110236560, 0.000000000000000000 ) ) ;
#53608 = CARTESIAN_POINT ( 'NONE',  ( 0.03757601356357168076, -0.4709442531824368783, -4.620136098463503353E-16 ) ) ;
#53609 = DIRECTION ( 'NONE',  ( 0.000000000000000000, 0.000000000000000000, -1.000000000000000000 ) ) ;
#53610 = CARTESIAN_POINT ( 'NONE',  ( 4.797336870675656522E-17, -0.3917322834645670104, -1.423228346456693050 ) ) ;
#53611 = CARTESIAN_POINT ( 'NONE',  ( -0.3986795681650724954, -0.0008564280373882149269, -1.929133858267715551 ) ) ;
#53612 = CARTESIAN_POINT ( 'NONE',  ( -0.1574803149606292529, -0.1870078740157479769, 0.4822834645669291653 ) ) ;
#53613 = CARTESIAN_POINT ( 'NONE',  ( 0.9186351706036751663, -0.6046776061558807314, 0.2411417322834647770 ) ) ;
#53614 = VERTEX_POINT ( 'NONE', #69422 ) ;
#53615 = CARTESIAN_POINT ( 'NONE',  ( -1.692913385826770645, 0.2952755905511811885, 0.000000000000000000 ) ) ;
#53616 = CARTESIAN_POINT ( 'NONE',  ( -1.116870163894023937, 1.075361400900961550, 0.1087570619416485251 ) ) ;
#53617 = DIRECTION ( 'NONE',  ( 9.948661822760824279E-18, 1.000000000000000000, 6.123233995736770966E-17 ) ) ;
#53618 = CARTESIAN_POINT ( 'NONE',  ( 1.489501312335958172, -0.2845877964562159024, 0.3641732283464567677 ) ) ;
#53619 = CARTESIAN_POINT ( 'NONE',  ( 0.3460692066303959202, -0.1998031496062991630, -2.071522309711286258 ) ) ;
#53620 = CARTESIAN_POINT ( 'NONE',  ( -1.371391076115484609, -0.5511811023622046335, 0.09757992244046803654 ) ) ;
#53621 = CARTESIAN_POINT ( 'NONE',  ( -1.574803149606298192, -0.1870078740157480879, -0.4822834645669291653 ) ) ;
#53622 = CARTESIAN_POINT ( 'NONE',  ( 0.1377952755905518800, 0.1660481256975883668, -0.3530559997133364547 ) ) ;
#53623 = ORIENTED_EDGE ( 'NONE', *, *, #8579, .T. ) ;
#53625 = DIRECTION ( 'NONE',  ( -0.000000000000000000, -1.000000000000000000, -1.408710688920637755E-15 ) ) ;
#53624 = CARTESIAN_POINT ( 'NONE',  ( 1.568241469816273659, -0.05778040916215560624, -0.4822834645669293319 ) ) ;
#53626 = CARTESIAN_POINT ( 'NONE',  ( -0.5380577427821514602, -0.3690944881889765550, -0.3153832671262227771 ) ) ;
#53627 = CARTESIAN_POINT ( 'NONE',  ( 0.9973753280839902091, -0.6046776061558807314, 0.2411417322834647770 ) ) ;
#53628 = CARTESIAN_POINT ( 'NONE',  ( 1.082677165354331228, -0.4536011799217367080, 0.2665933059059888421 ) ) ;
#53629 = CARTESIAN_POINT ( 'NONE',  ( -0.1958661417322836440, 0.3392501089628016664, -1.352999056921573295 ) ) ;
#53630 = CARTESIAN_POINT ( 'NONE',  ( -0.6758530183727028406, -0.5511811023622048555, -0.09757992244046775898 ) ) ;
#53631 = CARTESIAN_POINT ( 'NONE',  ( -1.377952755905511140, -0.5511811023622047445, 6.969142054262312111E-17 ) ) ;
#53632 = CARTESIAN_POINT ( 'NONE',  ( -0.3917322834645669549, -0.1049643490035306603, -1.075459317585301777 ) ) ;
#53633 = CARTESIAN_POINT ( 'NONE',  ( 0.6496062992125991586, 0.1660481256975885056, 0.3530559997133364547 ) ) ;
#53634 = CARTESIAN_POINT ( 'NONE',  ( -0.9120734908136475250, -0.5511811023622048555, -0.09757992244046775898 ) ) ;
#53635 = CARTESIAN_POINT ( 'NONE',  ( -0.3740157480314953431, -0.4536011799217368745, -0.2665933059059886201 ) ) ;
#53636 = EDGE_CURVE ( 'NONE', #1879, #57099, #31103, .T. ) ;
#53637 = CARTESIAN_POINT ( 'NONE',  ( -0.2165354330708654795, -0.5400638737290845981, -0.3530559997133363437 ) ) ;
#53638 = CARTESIAN_POINT ( 'NONE',  ( -1.351706036745406347, -0.3690944881889763329, 0.3153832671262228327 ) ) ;
#53639 = CARTESIAN_POINT ( 'NONE',  ( -0.1958661417322833942, -0.3392501089628018884, -0.06235527378708850127 ) ) ;
#53640 = CARTESIAN_POINT ( 'NONE',  ( 0.5446194225721792126, -0.05778040916215560624, -0.4822834645669293319 ) ) ;
#53641 = EDGE_CURVE ( 'NONE', #50964, #78564, #34197, .T. ) ;
#53642 = CARTESIAN_POINT ( 'NONE',  ( -0.2362204724409447953, -0.4091458600556404646, -0.2230971128608923715 ) ) ;
#53643 = CARTESIAN_POINT ( 'NONE',  ( -0.4724409448818895907, -0.1265901696524993070, -1.540026246719159886 ) ) ;
#53644 = CARTESIAN_POINT ( 'NONE',  ( -0.8267716535433065062, -0.6692913385826771977, 8.415575281601705876E-17 ) ) ;
#53645 = CARTESIAN_POINT ( 'NONE',  ( -0.3543307086614165824, -0.5511811023622047445, 6.969142054262312111E-17 ) ) ;
#53646 = CARTESIAN_POINT ( 'NONE',  ( -1.154855643044618851, 0.2306618581243848609, 0.2411417322834645549 ) ) ;
#53647 = CARTESIAN_POINT ( 'NONE',  ( 0.3674540682414705883, -0.5023911411419708095, 0.1820866141732285504 ) ) ;
#53648 = CARTESIAN_POINT ( 'NONE',  ( -0.5971128608923877978, 0.1771653543307087630, 0.09757992244046791164 ) ) ;
#53649 = CARTESIAN_POINT ( 'NONE',  ( -1.259842519685038686, -0.1870078740157479769, 0.4822834645669291653 ) ) ;
#53650 = CARTESIAN_POINT ( 'NONE',  ( -1.725721784776902190, -0.05778040916215522460, 0.4822834645669289988 ) ) ;
#53651 = CARTESIAN_POINT ( 'NONE',  ( 1.246719160104987623, 0.05413385826771626580, -0.4176697321401330321 ) ) ;
#53652 = CARTESIAN_POINT ( 'NONE',  ( 1.043307086614173818, 0.1012011053420777407, 0.2882089793578256898 ) ) ;
#53653 = CARTESIAN_POINT ( 'NONE',  ( 1.010498687664042716, -0.3690944881889763329, 0.3153832671262228327 ) ) ;
#53654 = CARTESIAN_POINT ( 'NONE',  ( 0.2690288713910767848, 0.2952755905511811885, 0.1292274648535926551 ) ) ;
#53655 = CARTESIAN_POINT ( 'NONE',  ( -1.384514435695537005, -0.6692913385826773087, -0.1292274648535924053 ) ) ;
#53656 = CARTESIAN_POINT ( 'NONE',  ( 1.286089238845145033, 0.1283753931104748280, 0.1820866141732283561 ) ) ;
#53657 = ORIENTED_EDGE ( 'NONE', *, *, #78852, .F. ) ;
#53658 = CARTESIAN_POINT ( 'NONE',  ( -0.1974969037888704149, -0.3420746716998661063, 0.1725721784776902690 ) ) ;
#53659 = EDGE_CURVE ( 'NONE', #15414, #1453, #76976, .T. ) ;
#53660 = CARTESIAN_POINT ( 'NONE',  ( -1.174540682414697335, -0.08942795157527998196, 0.3641732283464567121 ) ) ;
#53661 = CARTESIAN_POINT ( 'NONE',  ( -0.3280839895013117347, 0.05413385826771626580, -0.4176697321401330321 ) ) ;
#53662 = CARTESIAN_POINT ( 'NONE',  ( 0.4921259842519691285, 0.1660481256975885056, 0.3530559997133364547 ) ) ;
#53663 = CARTESIAN_POINT ( 'NONE',  ( -1.384514435695537005, 0.1771653543307087630, 0.09757992244046791164 ) ) ;
#53664 = CARTESIAN_POINT ( 'NONE',  ( -0.3460692066303960313, 0.1998031496062989965, -1.677821522309711488 ) ) ;
#53665 = CARTESIAN_POINT ( 'NONE',  ( -1.279527559055116948, -0.5400638737290844871, 0.3530559997133364547 ) ) ;
#53666 = CARTESIAN_POINT ( 'NONE',  ( 0.3608923884514443348, -0.6692913385826771977, 0.1292274648535927661 ) ) ;
#53667 = CARTESIAN_POINT ( 'NONE',  ( -0.03937007874015669567, 0.2952755905511811885, 0.000000000000000000 ) ) ;
#53668 = CARTESIAN_POINT ( 'NONE',  ( 1.299212598425197429, 0.2952755905511811885, 0.000000000000000000 ) ) ;
#53669 = CARTESIAN_POINT ( 'NONE',  ( -0.3996062992125985480, -7.340648628747423112E-17, -0.9035433070866141225 ) ) ;
#53670 = CARTESIAN_POINT ( 'NONE',  ( 0.1998031496062992740, 0.3460692066303959757, -1.246719160104986734 ) ) ;
#53671 = CARTESIAN_POINT ( 'NONE',  ( 4.837279021331060870E-17, -0.3949938075777409963, -1.023622047244094446 ) ) ;
#53672 = CARTESIAN_POINT ( 'NONE',  ( 0.3392501089628018884, -0.1958661417322834220, -0.2545931758530183275 ) ) ;
#53673 = CARTESIAN_POINT ( 'NONE',  ( -0.04593175853018302557, -0.5511811023622048555, -0.09757992244046775898 ) ) ;
#53674 = CARTESIAN_POINT ( 'NONE',  ( -0.3149606299212590610, -0.1870078740157479769, 0.4822834645669291653 ) ) ;
#53675 = CARTESIAN_POINT ( 'NONE',  ( 1.062992125984252745, -0.6692913385826771977, 8.415575281601705876E-17 ) ) ;
#53676 = CARTESIAN_POINT ( 'NONE',  ( -0.1974969037888704149, -0.3420746716998661063, -1.874671916010499428 ) ) ;
#53677 = CARTESIAN_POINT ( 'NONE',  ( 0.07874015748031558404, -0.1870078740157479769, 0.3641732283464567677 ) ) ;
#53678 = CARTESIAN_POINT ( 'NONE',  ( -1.233595800524933894, -0.6046776061558809534, -0.2411417322834644161 ) ) ;
#53679 = CARTESIAN_POINT ( 'NONE',  ( 1.561679790026247350, -0.4281496062992124485, 0.4176697321401328655 ) ) ;
#53680 = CARTESIAN_POINT ( 'NONE',  ( 0.4724409448818897572, -0.1265901696524988906, -2.001312335958005395 ) ) ;
#53681 = CARTESIAN_POINT ( 'NONE',  ( 0.3496712940256230251, 0.1778467755331661626, -2.755905511811022279 ) ) ;
#53682 = ORIENTED_EDGE ( 'NONE', *, *, #40727, .F. ) ;
#53683 = VERTEX_POINT ( 'NONE', #25611 ) ;
#53684 = CARTESIAN_POINT ( 'NONE',  ( 1.207349081364829990, -0.6046776061558809534, -0.2411417322834644161 ) ) ;
#53685 = CARTESIAN_POINT ( 'NONE',  ( 1.476377952755906220, 0.07958543189024071263, -0.2665933059059888421 ) ) ;
#53687 = CARTESIAN_POINT ( 'NONE',  ( -1.102362204724408601, -0.1870078740157480879, -0.4822834645669291653 ) ) ;
#53686 = CARTESIAN_POINT ( 'NONE',  ( -1.030183727034119867, -0.2845877964562159024, 0.3641732283464567677 ) ) ;
#53688 = CARTESIAN_POINT ( 'NONE',  ( -0.3917322834645669549, -7.196005306013483243E-17, -2.481607980806087799 ) ) ;
#53689 = DIRECTION ( 'NONE',  ( 0.000000000000000000, 0.000000000000000000, -1.000000000000000000 ) ) ;
#53690 = CARTESIAN_POINT ( 'NONE',  ( 1.023622047244095334, -0.1870078740157479769, 0.4822834645669291653 ) ) ;
#53691 = CARTESIAN_POINT ( 'NONE',  ( -1.607611548556429737, -0.6692913385826771977, 0.1292274648535927661 ) ) ;
#53692 = CARTESIAN_POINT ( 'NONE',  ( -0.1640419947506555343, -0.3162353388693405765, 0.4822834645669290543 ) ) ;
#53693 = CARTESIAN_POINT ( 'NONE',  ( -0.3477690288713905509, -0.6692913385826771977, 0.1292274648535927661 ) ) ;
#53694 = CARTESIAN_POINT ( 'NONE',  ( -1.305774278215222184, 0.2952755905511811885, 0.1292274648535926551 ) ) ;
#53695 = CARTESIAN_POINT ( 'NONE',  ( -0.1049643490035302024, -0.3917322834645671215, 0.1581364829396324501 ) ) ;
#53696 = CARTESIAN_POINT ( 'NONE',  ( 0.6036745406824153282, -0.6046776061558807314, 0.2411417322834647770 ) ) ;
#53697 = CARTESIAN_POINT ( 'NONE',  ( -0.1958661417322834220, -0.3392501089628018884, -1.790026246719160330 ) ) ;
#53698 = CARTESIAN_POINT ( 'NONE',  ( -1.391076115485563314, -0.5023911411419708095, -0.1820866141732282451 ) ) ;
#53699 = ORIENTED_EDGE ( 'NONE', *, *, #25885, .F. ) ;
#53700 = CARTESIAN_POINT ( 'NONE',  ( 0.1058382717557500713, -0.3949938075777409408, -2.447506561679789971 ) ) ;
#53701 = ORIENTED_EDGE ( 'NONE', *, *, #83060, .T. ) ;
#53702 = CARTESIAN_POINT ( 'NONE',  ( -1.481587895432891600, 1.357470117436001766, 0.4390532657067846012 ) ) ;
#53703 = CARTESIAN_POINT ( 'NONE',  ( -1.371391076115484831, 0.2952755905511810774, -0.1292274648535930714 ) ) ;
#53704 = CARTESIAN_POINT ( 'NONE',  ( -1.240157480314959759, -0.5400638737290845981, -0.3530559997133363437 ) ) ;
#53705 = CARTESIAN_POINT ( 'NONE',  ( -0.3996062992125986035, -0.1070741851644056997, -0.6758530183727035068 ) ) ;
#53706 = CARTESIAN_POINT ( 'NONE',  ( -1.633858267716534529, -0.5400638737290845981, -0.3530559997133363437 ) ) ;
#53707 = CARTESIAN_POINT ( 'NONE',  ( -1.627296587926508442, -0.6046776061558809534, -0.2411417322834644161 ) ) ;
#53708 = EDGE_CURVE ( 'NONE', #40053, #1230, #44392, .T. ) ;
#53709 = CARTESIAN_POINT ( 'NONE',  ( 0.4608550785314886045, 0.02791078216816508459, -0.4328096321851889194 ) ) ;
#53710 = CARTESIAN_POINT ( 'NONE',  ( -0.4744094488188894121, 1.537401574803149984, -2.170146923806595574 ) ) ;
#53711 = CARTESIAN_POINT ( 'NONE',  ( -0.3917322834645670104, -7.196005306013484475E-17, 0.1909448818897636901 ) ) ;
#53712 = CARTESIAN_POINT ( 'NONE',  ( 0.05249343832021075018, -0.5023911411419708095, 0.1820866141732285504 ) ) ;
#53713 = CARTESIAN_POINT ( 'NONE',  ( -0.7086614173228339419, -0.1870078740157480601, -0.3641732283464567677 ) ) ;
#53714 = CARTESIAN_POINT ( 'NONE',  ( -1.227034120734907141, -0.6692913385826773087, -0.1292274648535924053 ) ) ;
#53715 = CARTESIAN_POINT ( 'NONE',  ( 1.062992125984252745, -0.6692913385826771977, 8.415575281601705876E-17 ) ) ;
#53716 = CARTESIAN_POINT ( 'NONE',  ( -0.8333333333333323711, 0.2952755905511811885, 0.1292274648535926551 ) ) ;
#53717 = CARTESIAN_POINT ( 'NONE',  ( -0.3917322834645671215, 0.1049643490035301469, 0.1325459317585302166 ) ) ;
#53718 = ORIENTED_EDGE ( 'NONE', *, *, #71221, .F. ) ;
#53719 = CARTESIAN_POINT ( 'NONE',  ( -1.561679790026246017, -0.4281496062992127816, -0.4176697321401328100 ) ) ;
#53720 = CARTESIAN_POINT ( 'NONE',  ( -1.725721784776902190, -0.08942795157527998196, 0.3641732283464567121 ) ) ;
#53721 = CARTESIAN_POINT ( 'NONE',  ( -0.1341536278048670039, 1.050682278017461835, 0.2827841492639485144 ) ) ;
#53722 = CARTESIAN_POINT ( 'NONE',  ( -0.1265901696524993347, 0.4724409448818895907, -1.108923884514435798 ) ) ;
#53723 = EDGE_CURVE ( 'NONE', #19150, #79281, #6259, .T. ) ;
#53724 = CARTESIAN_POINT ( 'NONE',  ( 1.850419646634101412, 1.063020117359137373, 0.01785754392580130370 ) ) ;
#53725 = CARTESIAN_POINT ( 'NONE',  ( 0.3917322834645669549, 0.1049643490035304660, -0.5892388451443569819 ) ) ;
#53726 = CARTESIAN_POINT ( 'NONE',  ( 4.797336870675656522E-17, -0.3917322834645670104, -2.368110236220472675 ) ) ;
#53727 = CARTESIAN_POINT ( 'NONE',  ( -0.1640419947506553400, -0.05778040916215560624, -0.4822834645669293319 ) ) ;
#53728 = CARTESIAN_POINT ( 'NONE',  ( -1.502624671916009680, -0.2845877964562159024, 0.3641732283464567677 ) ) ;
#53729 = CARTESIAN_POINT ( 'NONE',  ( -9.787531504996566615E-17, 0.3996062992125985480, -0.07677165354330711677 ) ) ;
#53731 = CARTESIAN_POINT ( 'NONE',  ( -0.6958886929845781166, 0.004960608223778821026, 0.3437734562760189072 ) ) ;
#53730 = LINE ( 'NONE', #47420, #74568 ) ;
#53732 = CARTESIAN_POINT ( 'NONE',  ( -1.410761154855642463, -0.05778040916215522460, 0.4822834645669289988 ) ) ;
#53733 = CARTESIAN_POINT ( 'NONE',  ( -0.3149606299212590610, -0.1870078740157479769, 0.4822834645669291653 ) ) ;
#53734 = CARTESIAN_POINT ( 'NONE',  ( 0.2867679344610365999, 0.2867679344610365999, -0.06034813828640239741 ) ) ;
#53735 = CARTESIAN_POINT ( 'NONE',  ( 0.3937007874015754361, -0.1870078740157480601, -0.3641732283464567677 ) ) ;
#53736 = CARTESIAN_POINT ( 'NONE',  ( -2.795275590551185907, 0.4724409448818907564, -3.981376139758521912E-16 ) ) ;
#53737 = CARTESIAN_POINT ( 'NONE',  ( 0.3149606299212606708, -0.1870078740157480601, -0.3641732283464567677 ) ) ;
#53738 = CARTESIAN_POINT ( 'NONE',  ( 0.8464566929133865436, 0.07958543189024071263, -0.2665933059059888421 ) ) ;
#53739 = CARTESIAN_POINT ( 'NONE',  ( 1.036745406824147508, -0.4281496062992127816, -0.4176697321401328100 ) ) ;
#53740 = CARTESIAN_POINT ( 'NONE',  ( -0.4527559055118102749, -0.4536011799217368745, -0.2665933059059886201 ) ) ;
#53741 = CARTESIAN_POINT ( 'NONE',  ( 0.1958661417322834775, 0.3392501089628018884, -2.026246719160105236 ) ) ;
#53742 = CARTESIAN_POINT ( 'NONE',  ( -1.358267716535432434, -0.5400638737290844871, 0.3530559997133364547 ) ) ;
#53743 = CARTESIAN_POINT ( 'NONE',  ( 0.04593175853018440641, 0.1771653543307087075, -0.09757992244046823083 ) ) ;
#53744 = CARTESIAN_POINT ( 'NONE',  ( -1.450131233595799651, 0.1771653543307087075, -0.09757992244046823083 ) ) ;
#53745 = CARTESIAN_POINT ( 'NONE',  ( 0.4724409448818898682, 2.892866454678787531E-17, -0.5098425196850393526 ) ) ;
#53746 = CARTESIAN_POINT ( 'NONE',  ( -0.8858267716535425107, -0.4536011799217367080, 0.2665933059059888421 ) ) ;
#53747 = CARTESIAN_POINT ( 'NONE',  ( 0.000000000000000000, 2.559055118110236560, 0.000000000000000000 ) ) ;
#53748 = CARTESIAN_POINT ( 'NONE',  ( -0.2230971128608915943, 0.05413385826771666132, 0.4176697321401328100 ) ) ;
#53749 = CARTESIAN_POINT ( 'NONE',  ( 1.463254593175853824, -0.5511811023622046335, 0.09757992244046803654 ) ) ;
#53750 = CARTESIAN_POINT ( 'NONE',  ( 0.6036745406824153282, -0.5023911411419708095, 0.1820866141732285504 ) ) ;
#53751 = CARTESIAN_POINT ( 'NONE',  ( -0.4265091863517051496, 0.1771653543307087075, -0.09757992244046823083 ) ) ;
#53752 = CARTESIAN_POINT ( 'NONE',  ( -0.3740157480314953431, 0.1660481256975885056, 0.3530559997133364547 ) ) ;
#53753 = CARTESIAN_POINT ( 'NONE',  ( 0.5314960629921396951, 2.559055118110236560, -3.937007874015760578 ) ) ;
#53754 = CARTESIAN_POINT ( 'NONE',  ( -1.253280839895012377, -0.2845877964562161244, -0.3641732283464567121 ) ) ;
#53755 = CARTESIAN_POINT ( 'NONE',  ( -1.013613127888308485, -2.191421614605370878E-15, 0.4445507791589071167 ) ) ;
#53756 = CARTESIAN_POINT ( 'NONE',  ( 0.3937007874015754361, -0.1870078740157479769, 0.4822834645669291653 ) ) ;
#53757 = CARTESIAN_POINT ( 'NONE',  ( -9.787531504996566615E-17, 0.3996062992125985480, -1.494094488188976388 ) ) ;
#53758 = CARTESIAN_POINT ( 'NONE',  ( 1.535433070866142335, -0.6692913385826771977, 8.415575281601705876E-17 ) ) ;
#53759 = CARTESIAN_POINT ( 'NONE',  ( -0.2821522309711278487, 0.1771653543307087630, 0.09757992244046791164 ) ) ;
#53760 = CARTESIAN_POINT ( 'NONE',  ( -0.1312335958005241554, 0.2306618581243848609, 0.2411417322834645549 ) ) ;
#53761 = CARTESIAN_POINT ( 'NONE',  ( -1.496062992125983815, -0.1870078740157479769, 0.4822834645669291653 ) ) ;
#53762 = CARTESIAN_POINT ( 'NONE',  ( 1.535433070866142558, 0.2952755905511811885, 0.000000000000000000 ) ) ;
#53763 = CARTESIAN_POINT ( 'NONE',  ( 1.384514435695538559, 0.2952755905511810774, -0.1292274648535930714 ) ) ;
#53764 = CARTESIAN_POINT ( 'NONE',  ( -0.8333333333333323711, -0.5511811023622048555, -0.09757992244046775898 ) ) ;
#53765 = CARTESIAN_POINT ( 'NONE',  ( -0.1133856558944469489, 0.2726377952755905665, 0.1574803149606299191 ) ) ;
#53766 = CARTESIAN_POINT ( 'NONE',  ( -0.3996062992125986035, -7.340648628747425578E-17, -0.03937007874015749365 ) ) ;
#53767 = CARTESIAN_POINT ( 'NONE',  ( -0.3392501089628017219, -0.1958661417322836995, -2.568916953577114359 ) ) ;
#53768 = DIRECTION ( 'NONE',  ( -0.000000000000000000, -0.000000000000000000, -1.000000000000000000 ) ) ;
#53769 = CARTESIAN_POINT ( 'NONE',  ( 0.9645669291338588858, 0.07958543189024085140, 0.2665933059059887866 ) ) ;
#53770 = CARTESIAN_POINT ( 'NONE',  ( -1.633858267716534529, -0.5400638737290845981, -0.3530559997133363437 ) ) ;
#53771 = B_SPLINE_CURVE_WITH_KNOTS ( 'NONE', 3,
 ( #67777, #16437, #12069, #76862, #36906, #11248, #62582, #12476, #31825, #37726, #76046, #6151, #18390, #83179, #51165, #49940, #17977, #37324, #56661, #5735, #41671, #35366, #54714, #4924, #30592, #69724, #50760, #31407, #57071, #18787 ),
 .UNSPECIFIED., .F., .F.,
 ( 4, 2, 2, 2, 2, 2, 2, 2, 2, 2, 2, 2, 2, 2, 4 ),
 ( 0.01323639539072356958, 0.01388240907739069462, 0.01452842276405781965, 0.01582045013739205239, 0.01711247751072628165, 0.01840450488406051438, 0.02098855963072899372, 0.02357261437739747306, 0.02486464175073171967, 0.02615666912406597669, 0.02744869649740022677, 0.02874072387073448032, 0.03132477861740298741, 0.03261680599073724096, 0.03390883336407149451 ),
 .UNSPECIFIED. ) ;
#53772 = CARTESIAN_POINT ( 'NONE',  ( 0.8792650918635177559, -0.4281496062992127816, -0.4176697321401328100 ) ) ;
#53773 = CARTESIAN_POINT ( 'NONE',  ( 0.3392501089628018884, -0.1958661417322834220, -2.551837270341207109 ) ) ;
#53774 = CARTESIAN_POINT ( 'NONE',  ( 1.095800524934383846, -0.08942795157528024563, -0.3641732283464568787 ) ) ;
#53775 = CARTESIAN_POINT ( 'NONE',  ( 8.195543980992789655E-16, -0.1870078740157480879, -0.4822834645669291653 ) ) ;
#53776 = CARTESIAN_POINT ( 'NONE',  ( -0.5971128608923877978, -0.6692913385826773087, -0.1292274648535924053 ) ) ;
#53777 = CARTESIAN_POINT ( 'NONE',  ( 1.640419947506562393, -0.4281496062992124485, 0.4176697321401328655 ) ) ;
#53778 = CARTESIAN_POINT ( 'NONE',  ( -9.787531504996567848E-17, 0.3996062992125986035, -2.047244094488188892 ) ) ;
#53779 = CARTESIAN_POINT ( 'NONE',  ( 0.2230971128608929543, -0.004921259842519870586, -0.3153832671262229437 ) ) ;
#53780 = ADVANCED_FACE ( 'NONE', ( #77395 ), #13010, .T. ) ;
#53781 = ORIENTED_EDGE ( 'NONE', *, *, #2120, .T. ) ;
#53782 = CARTESIAN_POINT ( 'NONE',  ( -0.2867679344610365444, -0.2867679344610367664, -0.2132739089576921876 ) ) ;
#53783 = ORIENTED_EDGE ( 'NONE', *, *, #1707, .F. ) ;
#53784 = CARTESIAN_POINT ( 'NONE',  ( -0.5774278215223089816, 0.2306618581243847221, -0.2411417322834647770 ) ) ;
#53785 = CARTESIAN_POINT ( 'NONE',  ( 1.207349081364829990, -0.6046776061558809534, -0.2411417322834644161 ) ) ;
#53786 = CARTESIAN_POINT ( 'NONE',  ( 0.2887139107611556010, 0.2306618581243847221, -0.2411417322834647770 ) ) ;
#53787 = CARTESIAN_POINT ( 'NONE',  ( -0.3608923884514428360, 0.1771653543307087630, 0.09757992244046791164 ) ) ;
#53788 = CARTESIAN_POINT ( 'NONE',  ( 0.9317585301837276734, 0.05413385826771626580, -0.4176697321401330321 ) ) ;
#53789 = EDGE_CURVE ( 'NONE', #26484, #6163, #56486, .T. ) ;
#53790 = CARTESIAN_POINT ( 'NONE',  ( -0.7152230971128602510, -0.3162353388693405765, 0.4822834645669290543 ) ) ;
#53791 = CARTESIAN_POINT ( 'NONE',  ( -0.3346456692913377662, -0.5400638737290844871, 0.3530559997133364547 ) ) ;
#53792 = CARTESIAN_POINT ( 'NONE',  ( -0.8923884514435688198, 0.2306618581243847221, -0.2411417322834647770 ) ) ;
#53793 = CARTESIAN_POINT ( 'NONE',  ( 1.312335958005249825, 0.2306618581243847221, -0.2411417322834647770 ) ) ;
#53794 = CARTESIAN_POINT ( 'NONE',  ( 0.7414698162729663755, -0.6692913385826773087, -0.1292274648535924053 ) ) ;
#53795 = CARTESIAN_POINT ( 'NONE',  ( 0.9448818897637802916, -0.1870078740157480879, -0.4822834645669291653 ) ) ;
#53796 = CARTESIAN_POINT ( 'NONE',  ( -0.2867679344610364334, -0.2867679344610367109, -0.6811023622047243098 ) ) ;
#53797 = CARTESIAN_POINT ( 'NONE',  ( 0.1771653543307093182, -0.4536011799217368745, -0.2665933059059886201 ) ) ;
#53798 = ORIENTED_EDGE ( 'NONE', *, *, #56208, .F. ) ;
#53799 = CARTESIAN_POINT ( 'NONE',  ( -0.3949938075777409408, -0.1058382717557502933, -1.148293963254593431 ) ) ;
#53800 = ORIENTED_EDGE ( 'NONE', *, *, #35952, .F. ) ;
#53801 = CARTESIAN_POINT ( 'NONE',  ( -0.8202099737532801971, -0.5511811023622046335, 0.09757992244046803654 ) ) ;
#53802 = CARTESIAN_POINT ( 'NONE',  ( 0.01968503937007957949, -0.5400638737290845981, -0.3530559997133363437 ) ) ;
#53803 = CARTESIAN_POINT ( 'NONE',  ( 2.666390022512479696, 1.301092492065843320, 0.4123476441529870806 ) ) ;
#53804 = CARTESIAN_POINT ( 'NONE',  ( -0.2559055118110230564, 0.1660481256975883668, -0.3530559997133364547 ) ) ;
#53805 = CARTESIAN_POINT ( 'NONE',  ( -0.2559055118110230564, 0.1660481256975883668, -0.3530559997133364547 ) ) ;
#53806 = CARTESIAN_POINT ( 'NONE',  ( -1.122047244094487306, 0.1660481256975883668, -0.3530559997133364547 ) ) ;
#53807 = CARTESIAN_POINT ( 'NONE',  ( -1.292650918635170010, -0.6692913385826771977, 0.1292274648535927661 ) ) ;
#53808 = CARTESIAN_POINT ( 'NONE',  ( 1.246719160104987623, -0.004921259842519870586, -0.3153832671262229437 ) ) ;
#53809 = CARTESIAN_POINT ( 'NONE',  ( 1.348312163386739426, 0.2755905511811023723, 0.7386866130305692613 ) ) ;
#53810 = CARTESIAN_POINT ( 'NONE',  ( 0.2635424796782920853, 0.1334565945130699871, 5.584901928512098657 ) ) ;
#53811 = CARTESIAN_POINT ( 'NONE',  ( 0.5183727034120741983, 0.1771653543307087075, -0.09757992244046823083 ) ) ;
#53812 = CARTESIAN_POINT ( 'NONE',  ( 0.1968503937007881344, -0.6692913385826771977, 8.415575281601705876E-17 ) ) ;
#53813 = CARTESIAN_POINT ( 'NONE',  ( 0.5511811023622055217, -0.1870078740157479769, 0.4822834645669291653 ) ) ;
#53814 = ORIENTED_EDGE ( 'NONE', *, *, #39057, .T. ) ;
#53815 = CARTESIAN_POINT ( 'NONE',  ( 0.3460692066303959757, -0.1998031496062991907, -1.522309711286089273 ) ) ;
#53816 = DIRECTION ( 'NONE',  ( 0.000000000000000000, -0.000000000000000000, 1.000000000000000000 ) ) ;
#53817 = ORIENTED_EDGE ( 'NONE', *, *, #1563, .F. ) ;
#53818 = CARTESIAN_POINT ( 'NONE',  ( 0.3460692066303958092, 0.1998031496062993018, -0.9954068241469815614 ) ) ;
#53819 = CARTESIAN_POINT ( 'NONE',  ( -0.3996062992125984925, -0.1070741851644056858, -0.4376640419947506744 ) ) ;
#53820 = CARTESIAN_POINT ( 'NONE',  ( -0.6824146981627291497, -0.6046776061558809534, -0.2411417322834644161 ) ) ;
#53821 = CARTESIAN_POINT ( 'NONE',  ( 0.1070741851644054915, -0.3996062992125986035, -2.919947506561679784 ) ) ;
#53822 =( BOUNDED_CURVE ( )  B_SPLINE_CURVE ( 2, ( #80641, #75144, #17489, #54934, #67584, #47787, #9916, #43120, #68817 ),
 .UNSPECIFIED., .F., .F. ) 
 B_SPLINE_CURVE_WITH_KNOTS ( ( 3, 2, 2, 2, 3 ),
 ( 0.9375000000000000000, 0.9416666666666666519, 0.9458333333333333037, 0.9499999999999999556, 0.9506378855240343873 ),
 .UNSPECIFIED. ) 
 CURVE ( )  GEOMETRIC_REPRESENTATION_ITEM ( )  RATIONAL_B_SPLINE_CURVE ( ( 1.000000000000000000, 0.9659258262890683122, 1.000000000000000000, 0.9659258262890683122, 1.000000000000000000, 0.9659258262890683122, 1.000000000000000000, 0.9947834986831269877, 0.9911642120908010778 ) ) 
 REPRESENTATION_ITEM ( '' )  );
#53823 = CARTESIAN_POINT ( 'NONE',  ( 0.3392501089628018884, -0.1958661417322834220, -2.394356955380577467 ) ) ;
#53824 = CARTESIAN_POINT ( 'NONE',  ( -1.515748031496062076, -0.4536011799217367080, 0.2665933059059888421 ) ) ;
#53825 = CARTESIAN_POINT ( 'NONE',  ( 0.8005249343832027131, 0.05413385826771666132, 0.4176697321401328100 ) ) ;
#53826 = CARTESIAN_POINT ( 'NONE',  ( 0.7480314960629927956, 0.2952755905511811885, 0.000000000000000000 ) ) ;
#53827 = CARTESIAN_POINT ( 'NONE',  ( -0.03280839895013062252, 0.1771653543307087075, -0.09757992244046823083 ) ) ;
#53828 = CARTESIAN_POINT ( 'NONE',  ( 0.2493438320209980519, -0.4281496062992127816, -0.4176697321401328100 ) ) ;
#53829 = CARTESIAN_POINT ( 'NONE',  ( 0.1265901696524989462, 0.4724409448818897572, -1.959973753280839892 ) ) ;
#53830 = CARTESIAN_POINT ( 'NONE',  ( 0.08530183727034192087, -0.08942795157527998196, 0.3641732283464567121 ) ) ;
#53831 = CARTESIAN_POINT ( 'NONE',  ( -0.4986876640419942164, -0.6046776061558807314, 0.2411417322834647770 ) ) ;
#53832 = CARTESIAN_POINT ( 'NONE',  ( 0.1058382717557500852, -0.3949938075777408852, -1.736876640419947826 ) ) ;
#53833 = CARTESIAN_POINT ( 'NONE',  ( -1.443569553805773564, -0.6046776061558807314, 0.2411417322834647770 ) ) ;
#53834 = CARTESIAN_POINT ( 'NONE',  ( 0.2493438320209980519, -0.3690944881889765550, -0.3153832671262227771 ) ) ;
#53835 = CARTESIAN_POINT ( 'NONE',  ( -0.7137454485294953965, 2.001539355558159983, -0.4917280318828584074 ) ) ;
#53836 = CARTESIAN_POINT ( 'NONE',  ( -1.135170603674539924, -0.6692913385826771977, 0.1292274648535927661 ) ) ;
#53837 = CONICAL_SURFACE ( 'NONE', #12216, 1.181102362204724310, 0.7853981633974621568 ) ;
#53838 = CARTESIAN_POINT ( 'NONE',  ( -0.6036745406824141069, -0.5023911411419708095, -0.1820866141732282451 ) ) ;
#53839 = CARTESIAN_POINT ( 'NONE',  ( 0.3458507752293908943, 0.3458507752293908943, -2.261811023622047223 ) ) ;
#53840 = CARTESIAN_POINT ( 'NONE',  ( -1.279527559055116948, -0.5400638737290844871, 0.3530559997133364547 ) ) ;
#53841 = CARTESIAN_POINT ( 'NONE',  ( -0.5183727034120726440, 0.2952755905511811885, 0.1292274648535926551 ) ) ;
#53842 = CARTESIAN_POINT ( 'NONE',  ( 0.08530183727034192087, -0.05778040916215522460, 0.4822834645669289988 ) ) ;
#53843 = CARTESIAN_POINT ( 'NONE',  ( -0.1070741851644051862, -0.3996062992125986590, -2.511154855643044748 ) ) ;
#53844 = CARTESIAN_POINT ( 'NONE',  ( -0.3917322834645668994, -0.1049643490035306742, -2.330689345635483356 ) ) ;
#53845 = CARTESIAN_POINT ( 'NONE',  ( 3.184294706754630777, 2.755905511811024056, 0.5314960629921260393 ) ) ;
#53846 = CARTESIAN_POINT ( 'NONE',  ( 0.4265091863517067594, 0.1771653543307087630, 0.09757992244046791164 ) ) ;
#53847 = CARTESIAN_POINT ( 'NONE',  ( 1.128608923884514947, 0.2306618581243848609, 0.2411417322834645549 ) ) ;
#53848 = CARTESIAN_POINT ( 'NONE',  ( -1.305774278215222184, -0.5511811023622048555, -0.09757992244046775898 ) ) ;
#53849 = CARTESIAN_POINT ( 'NONE',  ( 1.259842519685040019, -0.1870078740157480879, -0.4822834645669291653 ) ) ;
#53850 = CARTESIAN_POINT ( 'NONE',  ( -1.489501312335957062, -0.2845877964562161244, -0.3641732283464567121 ) ) ;
#53851 = CARTESIAN_POINT ( 'NONE',  ( -0.3871391076115479057, -0.3162353388693409650, -0.4822834645669289433 ) ) ;
#53852 = CARTESIAN_POINT ( 'NONE',  ( 0.1312335958005257930, 0.1283753931104746893, -0.1820866141732285504 ) ) ;
#53853 = CARTESIAN_POINT ( 'NONE',  ( 1.473278426072734293, 0.2335363939278407575, -0.2780995266831703394 ) ) ;
#53854 = CARTESIAN_POINT ( 'NONE',  ( 0.5774278215223103139, -0.5023911411419708095, -0.1820866141732282451 ) ) ;
#53855 = AXIS2_PLACEMENT_3D ( 'NONE', #12586, #36591, #30278 ) ;
#53856 = CARTESIAN_POINT ( 'NONE',  ( 0.2755905511811031494, 0.2952755905511811885, 0.000000000000000000 ) ) ;
#53857 = CARTESIAN_POINT ( 'NONE',  ( 0.2925321140481932369, 0.2925321140481932369, -0.2145669291338583029 ) ) ;
#53858 = CARTESIAN_POINT ( 'NONE',  ( -0.7217847769028863381, 0.05413385826771626580, -0.4176697321401330321 ) ) ;
#53859 = CARTESIAN_POINT ( 'NONE',  ( -0.3917322834645670104, -7.196005306013484475E-17, -2.013779527559055094 ) ) ;
#53860 = CARTESIAN_POINT ( 'NONE',  ( 1.194225721784777594, -0.3690944881889765550, -0.3153832671262227771 ) ) ;
#53861 = CARTESIAN_POINT ( 'NONE',  ( 0.04593175853018440641, -0.6692913385826771977, 0.1292274648535927661 ) ) ;
#53862 = CARTESIAN_POINT ( 'NONE',  ( -0.4790026246719152336, -0.05778040916215560624, -0.4822834645669293319 ) ) ;
#53863 = CARTESIAN_POINT ( 'NONE',  ( -0.4921259842519677963, 0.07958543189024071263, -0.2665933059059888421 ) ) ;
#53864 = DIRECTION ( 'NONE',  ( -1.000000000000000000, -0.000000000000000000, -0.000000000000000000 ) ) ;
#53865 = CARTESIAN_POINT ( 'NONE',  ( -0.4265091863517051496, -0.5511811023622046335, 0.09757992244046803654 ) ) ;
#53866 = CARTESIAN_POINT ( 'NONE',  ( 0.3608923884514443348, -0.6692913385826771977, 0.1292274648535927661 ) ) ;
#53867 = CARTESIAN_POINT ( 'NONE',  ( -0.8464566929133852113, -0.4536011799217368745, -0.2665933059059886201 ) ) ;
#53868 = CARTESIAN_POINT ( 'NONE',  ( -0.3996062992125985480, -7.340648628747423112E-17, -0.9035433070866141225 ) ) ;
#53869 = CARTESIAN_POINT ( 'NONE',  ( -1.062992125984250968, -0.6692913385826771977, 8.415575281601705876E-17 ) ) ;
#53870 = CARTESIAN_POINT ( 'NONE',  ( -2.362204724409448620, 0.03937007874015751446, -2.474278114140802984E-14 ) ) ;
#53871 = EDGE_LOOP ( 'NONE', ( #42909, #28577, #22318, #39403 ) ) ;
#53872 = CARTESIAN_POINT ( 'NONE',  ( -0.9645669291338575535, -0.4536011799217367080, 0.2665933059059888421 ) ) ;
#53873 = CARTESIAN_POINT ( 'NONE',  ( 0.1049868766404206816, -0.6046776061558809534, -0.2411417322834644161 ) ) ;
#53874 = CARTESIAN_POINT ( 'NONE',  ( 0.3941128856533801517, 0.02500110683994734295, -1.220472440943932924 ) ) ;
#53875 = CARTESIAN_POINT ( 'NONE',  ( -0.6889763779527552368, 0.1660481256975885056, 0.3530559997133364547 ) ) ;
#53876 = CARTESIAN_POINT ( 'NONE',  ( 0.4724409448818881474, -0.1265901696525019160, -2.158792650918635037 ) ) ;
#53877 = CARTESIAN_POINT ( 'NONE',  ( 1.187664041994751285, -0.05778040916215522460, 0.4822834645669289988 ) ) ;
#53878 = CARTESIAN_POINT ( 'NONE',  ( 0.7545931758530189937, 0.2952755905511810774, -0.1292274648535930714 ) ) ;
#53879 = DIRECTION ( 'NONE',  ( 0.000000000000000000, -1.000000000000000000, 0.000000000000000000 ) ) ;
#53880 = PLANE ( 'NONE',  #36810 ) ;
#53881 = CARTESIAN_POINT ( 'NONE',  ( 0.2938400550950684975, -0.02965148040547824562, 5.527203440556594849 ) ) ;
#53882 = CARTESIAN_POINT ( 'NONE',  ( -1.640419947506561060, -0.4281496062992127816, -0.4176697321401328100 ) ) ;
#53883 = EDGE_CURVE ( 'NONE', #76967, #21745, #13895, .T. ) ;
#53884 = CARTESIAN_POINT ( 'NONE',  ( -0.3460692066303960868, 0.1998031496062990242, -0.3412073490813647969 ) ) ;
#53885 = VERTEX_POINT ( 'NONE', #32351 ) ;
#53886 = CARTESIAN_POINT ( 'NONE',  ( -0.5183727034120726440, 0.1771653543307087630, 0.09757992244046791164 ) ) ;
#53887 = CARTESIAN_POINT ( 'NONE',  ( -0.3392501089628017219, -0.1958661417322836718, -2.249343832020997525 ) ) ;
#53888 = VERTEX_POINT ( 'NONE', #12589 ) ;
#53889 = CARTESIAN_POINT ( 'NONE',  ( 0.8661417322834652488, -0.1870078740157480879, -0.4822834645669291653 ) ) ;
#53890 = CARTESIAN_POINT ( 'NONE',  ( 0.1640419947506569498, -0.05778040916215522460, 0.4822834645669289988 ) ) ;
#53891 = CARTESIAN_POINT ( 'NONE',  ( -0.5511811023622038563, -0.1870078740157479769, 0.4822834645669291653 ) ) ;
#53892 = CARTESIAN_POINT ( 'NONE',  ( 1.660104986876641320, -0.05778040916215522460, 0.4822834645669289988 ) ) ;
#53893 = CARTESIAN_POINT ( 'NONE',  ( -0.9120734908136475250, -0.5511811023622048555, -0.09757992244046775898 ) ) ;
#53894 = CARTESIAN_POINT ( 'NONE',  ( -0.4091458600556402980, -0.2362204724409451284, -2.019028871391076230 ) ) ;
#53895 = CARTESIAN_POINT ( 'NONE',  ( 0.3871391076115493490, -0.3162353388693405765, 0.4822834645669290543 ) ) ;
#53896 = CARTESIAN_POINT ( 'NONE',  ( 0.4658792650918640033, -0.2845877964562159024, 0.3641732283464567677 ) ) ;
#53897 = CIRCLE ( 'NONE', #4163, 0.01968503937007875723 ) ;
#53898 = CARTESIAN_POINT ( 'NONE',  ( -0.6561679790026240244, 0.2306618581243847221, -0.2411417322834647770 ) ) ;
#53899 = CARTESIAN_POINT ( 'NONE',  ( 0.3917322834645668994, -0.1049643490035303134, -1.766384883693226771 ) ) ;
#53900 = CARTESIAN_POINT ( 'NONE',  ( -1.076115485564303809, -0.6046776061558809534, -0.2411417322834644161 ) ) ;
#53901 = DIRECTION ( 'NONE',  ( -0.000000000000000000, 1.000000000000000000, -0.000000000000000000 ) ) ;
#53902 = CARTESIAN_POINT ( 'NONE',  ( 0.9120734908136490793, 0.2952755905511810774, -0.1292274648535930714 ) ) ;
#53903 = CARTESIAN_POINT ( 'NONE',  ( 1.108923884514436686, -0.2845877964562161244, -0.3641732283464567121 ) ) ;
#53904 = ORIENTED_EDGE ( 'NONE', *, *, #76928, .T. ) ;
#53905 = CARTESIAN_POINT ( 'NONE',  ( 0.1958661417322834775, 0.3392501089628018884, -2.818260785598111884 ) ) ;
#53906 = CARTESIAN_POINT ( 'NONE',  ( -0.5249343832020990641, 0.2306618581243848609, 0.2411417322834645549 ) ) ;
#53907 = ORIENTED_EDGE ( 'NONE', *, *, #17436, .F. ) ;
#53908 = CARTESIAN_POINT ( 'NONE',  ( 0.4986876640419954376, 0.1283753931104748280, 0.1820866141732283561 ) ) ;
#53909 = CARTESIAN_POINT ( 'NONE',  ( -0.9973753280839886548, -0.6046776061558809534, -0.2411417322834644161 ) ) ;
#53910 = CARTESIAN_POINT ( 'NONE',  ( 0.8136482939632553313, 0.2306618581243848609, 0.2411417322834645549 ) ) ;
#53911 = CARTESIAN_POINT ( 'NONE',  ( 0.8136482939632553313, 0.2306618581243848609, 0.2411417322834645549 ) ) ;
#53912 = CARTESIAN_POINT ( 'NONE',  ( 5.463695987328526437E-16, -0.1870078740157479769, 0.4822834645669291653 ) ) ;
#53913 = B_SPLINE_CURVE_WITH_KNOTS ( 'NONE', 3,
 ( #4268, #5094, #81305, #23619 ),
 .UNSPECIFIED., .F., .F.,
 ( 4, 4 ),
 ( 3.593986969189856268E-07, 0.001287825409103295115 ),
 .UNSPECIFIED. ) ;
#53914 = CARTESIAN_POINT ( 'NONE',  ( -0.2165354330708654795, 0.1660481256975885056, 0.3530559997133364547 ) ) ;
#53915 = CARTESIAN_POINT ( 'NONE',  ( -0.1958661417322834220, -0.3392501089628018884, -2.197506561679789971 ) ) ;
#53916 = CARTESIAN_POINT ( 'NONE',  ( -1.489501312335957062, -0.3162353388693409650, -0.4822834645669289433 ) ) ;
#53917 = CARTESIAN_POINT ( 'NONE',  ( -0.4724409448818890911, -0.1870078740157480879, -0.4822834645669291653 ) ) ;
#53918 = CARTESIAN_POINT ( 'NONE',  ( -0.4527559055118102749, -0.4536011799217368745, -0.2665933059059886201 ) ) ;
#53919 = CARTESIAN_POINT ( 'NONE',  ( 1.325459317585302665, -0.4281496062992124485, 0.4176697321401328655 ) ) ;
#53920 = VECTOR ( 'NONE', #21141, 39.37007874015748143 ) ;
#53921 = CARTESIAN_POINT ( 'NONE',  ( 1.496062992125985147, -0.1870078740157479769, 0.4822834645669291653 ) ) ;
#53922 = CARTESIAN_POINT ( 'NONE',  ( -0.7349081364829390672, 0.2306618581243847221, -0.2411417322834647770 ) ) ;
#53923 = CARTESIAN_POINT ( 'NONE',  ( -0.3460692066303960313, 0.1998031496062989965, 0.2119422572178477626 ) ) ;
#53924 = CARTESIAN_POINT ( 'NONE',  ( 0.6102362204724416372, -0.5400638737290844871, 0.3530559997133364547 ) ) ;
#53925 = CARTESIAN_POINT ( 'NONE',  ( 0.3996062992125986035, 2.446882876249141962E-17, -2.007874015748031482 ) ) ;
#53926 = CARTESIAN_POINT ( 'NONE',  ( 0.9285414500055713116, 0.000000000000000000, -0.6299212598425196763 ) ) ;
#53927 = CARTESIAN_POINT ( 'NONE',  ( -0.1771653543307080136, 0.1660481256975883668, -0.3530559997133364547 ) ) ;
#53928 = CARTESIAN_POINT ( 'NONE',  ( -1.148293963254592542, 0.1771653543307087630, 0.09757992244046791164 ) ) ;
#53930 = CARTESIAN_POINT ( 'NONE',  ( -0.4677827689124922084, 0.03937007874015747977, 2.154527559055118946 ) ) ;
#53929 = CARTESIAN_POINT ( 'NONE',  ( 1.089238845144357759, -0.004921259842519870586, -0.3153832671262229437 ) ) ;
#53931 = CARTESIAN_POINT ( 'NONE',  ( 0.2362204724409449064, 0.4091458600556404646, -0.8510498687664042050 ) ) ;
#53932 = CARTESIAN_POINT ( 'NONE',  ( 1.377952755905512472, 0.1771653543307087630, 0.000000000000000000 ) ) ;
#53933 = CARTESIAN_POINT ( 'NONE',  ( 0.6889763779527563470, 0.1660481256975883668, -0.3530559997133364547 ) ) ;
#53934 = CARTESIAN_POINT ( 'NONE',  ( 0.2891555358219910499, -0.2891555358219909944, -0.6476377952755905110 ) ) ;
#53935 = CARTESIAN_POINT ( 'NONE',  ( -0.2165354330708654795, -0.5400638737290845981, -0.3530559997133363437 ) ) ;
#53936 = CARTESIAN_POINT ( 'NONE',  ( 0.01000891935578606708, -2.191421614605370878E-15, 0.4445507791589071167 ) ) ;
#53937 = CARTESIAN_POINT ( 'NONE',  ( 1.194225721784777594, -0.3690944881889765550, -0.3153832671262227771 ) ) ;
#53938 = CARTESIAN_POINT ( 'NONE',  ( -0.006561679790025524116, -0.3162353388693405765, 0.4822834645669290543 ) ) ;
#53939 = CARTESIAN_POINT ( 'NONE',  ( 0.1058382717557499880, 0.3949938075777409408, -0.3851706036745406458 ) ) ;
#53940 = CARTESIAN_POINT ( 'NONE',  ( 1.312335958005250269, -0.6046776061558807314, 0.2411417322834647770 ) ) ;
#53941 = CARTESIAN_POINT ( 'NONE',  ( -0.07217847769028813698, -0.3162353388693409650, -0.4822834645669289433 ) ) ;
#53942 = CARTESIAN_POINT ( 'NONE',  ( 0.7020997375328090762, -0.2845877964562159024, 0.3641732283464567677 ) ) ;
#53943 = CARTESIAN_POINT ( 'NONE',  ( 0.1265901696524990572, -0.4724409448818897017, -0.1620734908136483021 ) ) ;
#53944 = CARTESIAN_POINT ( 'NONE',  ( 0.5839895013123367340, 0.1771653543307087630, 0.09757992244046791164 ) ) ;
#53945 = DIRECTION ( 'NONE',  ( 1.000000000000000000, 0.000000000000000000, -0.000000000000000000 ) ) ;
#53946 = CARTESIAN_POINT ( 'NONE',  ( 0.2925321140481932369, 0.2925321140481932369, -1.316929133858267820 ) ) ;
#53947 = CARTESIAN_POINT ( 'NONE',  ( 0.9055118110236227702, 0.2952755905511811885, 0.000000000000000000 ) ) ;
#53948 = CARTESIAN_POINT ( 'NONE',  ( -0.1958661417322834220, -0.3392501089628018884, -1.002624671916010568 ) ) ;
#53949 = CARTESIAN_POINT ( 'NONE',  ( 1.692913385826772421, 0.1771653543307087630, 0.000000000000000000 ) ) ;
#53950 = CARTESIAN_POINT ( 'NONE',  ( -0.3859888145977992124, -0.06766049032609708358, -3.091116300196750268E-17 ) ) ;
#53951 = CARTESIAN_POINT ( 'NONE',  ( -0.03280839895013062252, -0.5511811023622046335, 0.09757992244046803654 ) ) ;
#53952 = CARTESIAN_POINT ( 'NONE',  ( 0.2624671916010504757, 0.2306618581243848609, 0.2411417322834645549 ) ) ;
#53953 = CARTESIAN_POINT ( 'NONE',  ( 1.594488188976378673, -0.4536011799217368745, -0.2665933059059886201 ) ) ;
#53954 = CARTESIAN_POINT ( 'NONE',  ( -1.522309711286088607, 0.1283753931104746893, -0.1820866141732285504 ) ) ;
#53955 = CARTESIAN_POINT ( 'NONE',  ( -1.476377952755905110, -0.5400638737290845981, -0.3530559997133363437 ) ) ;
#53956 =( GEOMETRIC_REPRESENTATION_CONTEXT ( 3 ) GLOBAL_UNCERTAINTY_ASSIGNED_CONTEXT ( ( #39464 ) ) GLOBAL_UNIT_ASSIGNED_CONTEXT ( ( #73830, #72985, #10266 ) ) REPRESENTATION_CONTEXT ( 'NONE', 'WORKASPACE' ) );
#53957 = CARTESIAN_POINT ( 'NONE',  ( 0.4855643044619430415, -0.4281496062992127816, -0.4176697321401328100 ) ) ;
#53958 = CARTESIAN_POINT ( 'NONE',  ( 1.502624671916010790, -0.05778040916215522460, 0.4822834645669289988 ) ) ;
#53959 = CARTESIAN_POINT ( 'NONE',  ( 1.614173228346457378, 0.7794589730111999293, 0.1372047244094478369 ) ) ;
#53960 = CARTESIAN_POINT ( 'NONE',  ( 0.3740157480314966754, 0.1660481256975883668, -0.3530559997133364547 ) ) ;
#53961 = CARTESIAN_POINT ( 'NONE',  ( 0.2362204724409451007, -0.4091458600556402980, -2.688320209973753538 ) ) ;
#53962 = CARTESIAN_POINT ( 'NONE',  ( 0.2372001242736402615, 1.126255254315259968, 3.929879783441174279 ) ) ;
#53963 = CARTESIAN_POINT ( 'NONE',  ( 0.8989501312335964611, 0.2952755905511811885, 0.1292274648535926551 ) ) ;
#53964 = CARTESIAN_POINT ( 'NONE',  ( -1.614173228346456268, -0.5511811023622047445, 6.969142054262312111E-17 ) ) ;
#53965 = CARTESIAN_POINT ( 'NONE',  ( 1.305774278215223960, -0.5511811023622046335, 0.09757992244046803654 ) ) ;
#53966 = CARTESIAN_POINT ( 'NONE',  ( 1.660104986876641320, -0.05778040916215522460, 0.4822834645669289988 ) ) ;
#53967 = CARTESIAN_POINT ( 'NONE',  ( -0.6561679790026240244, 0.1283753931104746893, -0.1820866141732285504 ) ) ;
#53968 = CARTESIAN_POINT ( 'NONE',  ( -0.4091458600556405756, 0.2362204724409446288, -2.073490813648294129 ) ) ;
#53969 = CARTESIAN_POINT ( 'NONE',  ( 0.4986876640419954376, 0.1283753931104748280, 0.1820866141732283561 ) ) ;
#53970 = CARTESIAN_POINT ( 'NONE',  ( 0.02624671916010564918, -0.6046776061558809534, -0.2411417322834644161 ) ) ;
#53971 = CARTESIAN_POINT ( 'NONE',  ( 0.8858267716535438430, -0.5400638737290845981, -0.3530559997133363437 ) ) ;
#53972 = CARTESIAN_POINT ( 'NONE',  ( -0.3805774278215216522, 0.05413385826771666132, 0.4176697321401328100 ) ) ;
#53973 = CARTESIAN_POINT ( 'NONE',  ( 0.2099737532808405305, 0.1283753931104746893, -0.1820866141732285504 ) ) ;
#53974 = CARTESIAN_POINT ( 'NONE',  ( 1.391076115485564868, -0.6046776061558807314, 0.2411417322834647770 ) ) ;
#53975 = EDGE_CURVE ( 'NONE', #23435, #64696, #30408, .T. ) ;
#53976 = DIRECTION ( 'NONE',  ( 0.000000000000000000, 0.000000000000000000, -1.000000000000000000 ) ) ;
#53977 = CARTESIAN_POINT ( 'NONE',  ( -0.8267716535433065062, -0.6692913385826771977, 8.415575281601705876E-17 ) ) ;
#53979 = CARTESIAN_POINT ( 'NONE',  ( -0.3996062992125986035, -7.340648628747425578E-17, -0.6692913385826770867 ) ) ;
#53978 = DIRECTION ( 'NONE',  ( -0.000000000000000000, -1.000000000000000000, -0.000000000000000000 ) ) ;
#53980 = CARTESIAN_POINT ( 'NONE',  ( 2.094141031014985721, 1.724409448818900570, -0.4359958488159719758 ) ) ;
#53981 = CARTESIAN_POINT ( 'NONE',  ( -0.9711286089238838626, 0.2306618581243847221, -0.2411417322834647770 ) ) ;
#53982 = CARTESIAN_POINT ( 'NONE',  ( 0.07874015748031558404, -0.1870078740157480879, -0.4822834645669291653 ) ) ;
#53983 = CARTESIAN_POINT ( 'NONE',  ( -0.2362204724409447953, -0.4091458600556404646, 0.09186351706036745279 ) ) ;
#53984 = CARTESIAN_POINT ( 'NONE',  ( -0.1058382717557503211, 0.3949938075777409408, -2.368766404199475595 ) ) ;
#53985 = ORIENTED_EDGE ( 'NONE', *, *, #61343, .F. ) ;
#53986 = CARTESIAN_POINT ( 'NONE',  ( 0.7349081364829403995, 0.1283753931104748280, 0.1820866141732283561 ) ) ;
#53987 = CARTESIAN_POINT ( 'NONE',  ( -0.2867679344610365999, 0.2867679344610364889, -0.9566929133858265155 ) ) ;
#53988 = EDGE_CURVE ( 'NONE', #30815, #51378, #52456, .T. ) ;
#53989 = CARTESIAN_POINT ( 'NONE',  ( 1.056430446194226436, -0.6692913385826773087, -0.1292274648535924053 ) ) ;
#53990 = CARTESIAN_POINT ( 'NONE',  ( 3.884611959489589594, 2.725289161120230563, -0.5314960629921258173 ) ) ;
#53991 = CARTESIAN_POINT ( 'NONE',  ( -1.397637795275589623, 0.07958543189024085140, 0.2665933059059887866 ) ) ;
#53992 = CARTESIAN_POINT ( 'NONE',  ( 1.482939632545932307, -0.4281496062992124485, 0.4176697321401328655 ) ) ;
#53993 = CARTESIAN_POINT ( 'NONE',  ( -1.476377952755905110, -0.5400638737290845981, -0.3530559997133363437 ) ) ;
#53994 = CARTESIAN_POINT ( 'NONE',  ( 0.3917322834645668994, 0.1049643490035304522, -0.3621854086276097839 ) ) ;
#53995 = CARTESIAN_POINT ( 'NONE',  ( 0.1181102362204730916, 0.2952755905511811885, 0.000000000000000000 ) ) ;
#53996 = CARTESIAN_POINT ( 'NONE',  ( -0.5118110236220466680, -0.5511811023622047445, 6.969142054262312111E-17 ) ) ;
#53997 = CARTESIAN_POINT ( 'NONE',  ( 0.9580052493438326877, 0.05413385826771666132, 0.4176697321401328100 ) ) ;
#53998 = CARTESIAN_POINT ( 'NONE',  ( 0.1246719160104994284, -0.6692913385826771977, 0.1292274648535927661 ) ) ;
#53999 = CARTESIAN_POINT ( 'NONE',  ( -1.586052503253847501, 1.299212598425198095, 0.1653254495020568260 ) ) ;
#54000 = DIRECTION ( 'NONE',  ( 0.000000000000000000, 1.000000000000000000, 0.000000000000000000 ) ) ;
#54001 = CARTESIAN_POINT ( 'NONE',  ( 0.2867679344610366554, 0.2867679344610366554, -1.709336901083676086 ) ) ;
#54002 = CARTESIAN_POINT ( 'NONE',  ( 0.8136482939632553313, -0.6046776061558809534, -0.2411417322834644161 ) ) ;
#54003 = CARTESIAN_POINT ( 'NONE',  ( 0.03937007874015806264, 0.2952755905511811885, 0.000000000000000000 ) ) ;
#54004 = CARTESIAN_POINT ( 'NONE',  ( -0.9645669291338575535, 0.1660481256975883668, -0.3530559997133364547 ) ) ;
#54005 = CARTESIAN_POINT ( 'NONE',  ( 0.8989501312335963501, -0.6692913385826773087, -0.1292274648535924053 ) ) ;
#54006 = CARTESIAN_POINT ( 'NONE',  ( 0.8464566929133866546, -0.5400638737290844871, 0.3530559997133364547 ) ) ;
#54007 = CARTESIAN_POINT ( 'NONE',  ( -0.3392501089628017219, -0.1958661417322836718, -1.082020997375328086 ) ) ;
#54008 = CARTESIAN_POINT ( 'NONE',  ( -0.2952755905511804668, 0.1660481256975885056, 0.3530559997133364547 ) ) ;
#54009 = CARTESIAN_POINT ( 'NONE',  ( 0.6824146981627303710, -0.6046776061558807314, 0.2411417322834647770 ) ) ;
#54010 = CARTESIAN_POINT ( 'NONE',  ( -0.1574803149606292529, -0.1870078740157480879, -0.4822834645669291653 ) ) ;
#54011 = CARTESIAN_POINT ( 'NONE',  ( 0.5249343832021005074, -0.5023911411419708095, 0.1820866141732285504 ) ) ;
#54012 = CARTESIAN_POINT ( 'NONE',  ( -1.154855643044618851, -0.6046776061558809534, -0.2411417322834644161 ) ) ;
#54013 = CARTESIAN_POINT ( 'NONE',  ( -0.4061203303035118561, -2.613618158232546091E-15, -0.3464511005275220379 ) ) ;
#54014 = CARTESIAN_POINT ( 'NONE',  ( 0.9317585301837276734, -0.4281496062992124485, 0.4176697321401328655 ) ) ;
#54015 = VECTOR ( 'NONE', #30376, 39.37007874015748143 ) ;
#54016 = DIRECTION ( 'NONE',  ( -0.000000000000000000, -0.000000000000000000, -1.000000000000000000 ) ) ;
#54017 = CARTESIAN_POINT ( 'NONE',  ( 0.3392501089628018329, 0.1958661417322835607, -2.170603674540682260 ) ) ;
#54018 = ORIENTED_EDGE ( 'NONE', *, *, #66351, .F. ) ;
#54019 = VERTEX_POINT ( 'NONE', #60933 ) ;
#54020 = CARTESIAN_POINT ( 'NONE',  ( 1.305774278215223960, -0.6692913385826771977, 0.1292274648535927661 ) ) ;
#54021 = CARTESIAN_POINT ( 'NONE',  ( 0.7152230971128614723, -0.2845877964562161244, -0.3641732283464567121 ) ) ;
#54022 = CARTESIAN_POINT ( 'NONE',  ( -0.03443470937339728616, 1.062992125984252079, -1.537015892239756099 ) ) ;
#54023 = PLANE ( 'NONE',  #31586 ) ;
#54024 = LINE ( 'NONE', #8600, #70109 ) ;
#54025 = CARTESIAN_POINT ( 'NONE',  ( 0.1049643490035304938, -0.3917322834645669549, -1.114829396325459410 ) ) ;
#54026 = CARTESIAN_POINT ( 'NONE',  ( -0.3460692066303957537, -0.1998031496062994405, -2.176509186351706315 ) ) ;
#54027 = CARTESIAN_POINT ( 'NONE',  ( -0.6627296587926501115, 0.2952755905511810774, -0.1292274648535930714 ) ) ;
#54028 = CARTESIAN_POINT ( 'NONE',  ( -0.6167979002624665030, 0.05413385826771666132, 0.4176697321401328100 ) ) ;
#54029 = CARTESIAN_POINT ( 'NONE',  ( 1.200787401574803681, -0.5400638737290845981, -0.3530559997133363437 ) ) ;
#54030 = ORIENTED_EDGE ( 'NONE', *, *, #56216, .T. ) ;
#54031 = CARTESIAN_POINT ( 'NONE',  ( -1.620734908136482577, -0.6692913385826773087, -0.1292274648535924053 ) ) ;
#54032 = CARTESIAN_POINT ( 'NONE',  ( -1.053714247187549580, 1.260741004084709793, 0.3856939116699171222 ) ) ;
#54033 = CARTESIAN_POINT ( 'NONE',  ( 1.646981627296588035, -0.2845877964562159024, 0.3641732283464567677 ) ) ;
#54034 = DIRECTION ( 'NONE',  ( 0.000000000000000000, 0.000000000000000000, -1.000000000000000000 ) ) ;
#54035 = CARTESIAN_POINT ( 'NONE',  ( -1.167979002624671470, -0.004921259842519576551, 0.3153832671262227771 ) ) ;
#54036 = CARTESIAN_POINT ( 'NONE',  ( 0.2867679344610365999, 0.2867679344610365999, 0.02755905511811028441 ) ) ;
#54037 = CARTESIAN_POINT ( 'NONE',  ( 0.3477690288713918276, -0.6692913385826773087, -0.1292274648535924053 ) ) ;
#54039 = CARTESIAN_POINT ( 'NONE',  ( 0.6399301791983058596, -1.374501131054255944E-15, 0.4445507791589066726 ) ) ;
#54038 = CARTESIAN_POINT ( 'NONE',  ( 1.377952755905512472, 0.2952755905511811885, 0.000000000000000000 ) ) ;
#54040 = CARTESIAN_POINT ( 'NONE',  ( -0.8136482939632537770, -0.5023911411419708095, 0.1820866141732285504 ) ) ;
#54041 = CARTESIAN_POINT ( 'NONE',  ( 0.6102362204724416372, 0.1660481256975883668, -0.3530559997133364547 ) ) ;
#54042 = CARTESIAN_POINT ( 'NONE',  ( 1.391076115485564868, -0.5023911411419708095, 0.1820866141732285504 ) ) ;
#54043 = CARTESIAN_POINT ( 'NONE',  ( 0.1049643490035304522, -0.3917322834645668994, -1.110216904690602080 ) ) ;
#54044 = CARTESIAN_POINT ( 'NONE',  ( -0.8136482939632537770, -0.5023911411419708095, 0.1820866141732285504 ) ) ;
#54045 = CARTESIAN_POINT ( 'NONE',  ( 1.174540682414699111, -0.3162353388693405765, 0.4822834645669290543 ) ) ;
#54046 = CARTESIAN_POINT ( 'NONE',  ( 0.2768633925643534388, 1.846642183492231748, 0.1464305347622791575 ) ) ;
#54047 = CARTESIAN_POINT ( 'NONE',  ( -0.02624671916010428221, -0.6046776061558807314, 0.2411417322834647770 ) ) ;
#54048 = CARTESIAN_POINT ( 'NONE',  ( -0.7480314960629914633, -0.5511811023622047445, 6.969142054262312111E-17 ) ) ;
#54049 = CARTESIAN_POINT ( 'NONE',  ( -0.3412073490813641308, -0.5023911411419708095, 0.1820866141732285504 ) ) ;
#54050 = CARTESIAN_POINT ( 'NONE',  ( -0.2821522309711278487, 0.2952755905511811885, 0.1292274648535926551 ) ) ;
#54051 = CARTESIAN_POINT ( 'NONE',  ( -1.502624671916009680, -0.2845877964562159024, 0.3641732283464567677 ) ) ;
#54052 = CARTESIAN_POINT ( 'NONE',  ( 0.2867679344610366554, -0.2867679344610365999, -0.5676046176191095194 ) ) ;
#54053 = CARTESIAN_POINT ( 'NONE',  ( 0.4396325459317590445, -0.6692913385826771977, 0.1292274648535927661 ) ) ;
#54054 = CARTESIAN_POINT ( 'NONE',  ( 0.000000000000000000, 0.03937007874015751446, -2.874015748031495843 ) ) ;
#54055 = CARTESIAN_POINT ( 'NONE',  ( 0.1265901696524989462, 0.4724409448818897572, -1.487532808398950301 ) ) ;
#54056 = CARTESIAN_POINT ( 'NONE',  ( -0.7020997375328076329, -0.3162353388693409650, -0.4822834645669289433 ) ) ;
#54057 = CARTESIAN_POINT ( 'NONE',  ( -0.1312335958005241554, 0.1283753931104748280, 0.1820866141732283561 ) ) ;
#54058 = CARTESIAN_POINT ( 'NONE',  ( -1.522309711286088607, -0.6046776061558807314, 0.2411417322834647770 ) ) ;
#54059 = CARTESIAN_POINT ( 'NONE',  ( -0.09842519685039295696, -0.5400638737290844871, 0.3530559997133364547 ) ) ;
#54060 = CARTESIAN_POINT ( 'NONE',  ( 0.2821522309711292364, 0.1771653543307087075, -0.09757992244046823083 ) ) ;
#54061 = CARTESIAN_POINT ( 'NONE',  ( -0.7808398950131225646, -0.08942795157527998196, 0.3641732283464567121 ) ) ;
#54062 = CARTESIAN_POINT ( 'NONE',  ( -1.213910761154854745, 0.2952755905511810774, -0.1292274648535930714 ) ) ;
#54063 = CARTESIAN_POINT ( 'NONE',  ( 1.601049868766404982, 0.1283753931104748280, 0.1820866141732283561 ) ) ;
#54064 = CARTESIAN_POINT ( 'NONE',  ( 1.187664041994751285, -0.05778040916215522460, 0.4822834645669289988 ) ) ;
#54065 = CARTESIAN_POINT ( 'NONE',  ( 0.000000000000000000, 0.04488074079120461107, 0.000000000000000000 ) ) ;
#54066 = CARTESIAN_POINT ( 'NONE',  ( 0.7283464566929143125, 0.07958543189024085140, 0.2665933059059887866 ) ) ;
#54067 = PRODUCT_DEFINITION_SHAPE ( 'NONE', 'NONE',  #23368 ) ;
#54068 = CARTESIAN_POINT ( 'NONE',  ( 0.7152230971128616943, -0.05778040916215522460, 0.4822834645669289988 ) ) ;
#54069 = DIRECTION ( 'NONE',  ( 1.000000000000000000, 0.000000000000000000, 0.000000000000000000 ) ) ;
#54070 = CARTESIAN_POINT ( 'NONE',  ( 1.371391076115485719, -0.5511811023622048555, -0.09757992244046775898 ) ) ;
#54071 = AXIS2_PLACEMENT_3D ( 'NONE', #30101, #68826, #5664 ) ;
#54072 = ORIENTED_EDGE ( 'NONE', *, *, #6391, .T. ) ;
#54073 = CARTESIAN_POINT ( 'NONE',  ( 0.3460692066303959202, -0.1998031496062991630, -2.701443569553806157 ) ) ;
#54074 = CARTESIAN_POINT ( 'NONE',  ( -1.266404199475064773, -0.08942795157528024563, -0.3641732283464568787 ) ) ;
#54075 = CARTESIAN_POINT ( 'NONE',  ( -0.3740157480314953431, 0.1660481256975885056, 0.3530559997133364547 ) ) ;
#54076 = CARTESIAN_POINT ( 'NONE',  ( 0.5249343832021003964, 0.2306618581243847221, -0.2411417322834647770 ) ) ;
#54077 = CARTESIAN_POINT ( 'NONE',  ( -1.594488188976377563, -0.4536011799217367080, 0.2665933059059888421 ) ) ;
#54078 = CARTESIAN_POINT ( 'NONE',  ( 0.1070741851644053388, 0.3996062992125986035, -2.274934383202099397 ) ) ;
#54079 = CARTESIAN_POINT ( 'NONE',  ( -1.522309711286088607, 0.2306618581243847221, -0.2411417322834647770 ) ) ;
#54080 = CARTESIAN_POINT ( 'NONE',  ( 0.4396325459317593221, 0.2952755905511810774, -0.1292274648535930714 ) ) ;
#54081 = CARTESIAN_POINT ( 'NONE',  ( 0.1771653543307093182, -0.5400638737290845981, -0.3530559997133363437 ) ) ;
#54082 = CARTESIAN_POINT ( 'NONE',  ( 1.404199475065617264, -0.4281496062992124485, 0.4176697321401328655 ) ) ;
#54083 = CARTESIAN_POINT ( 'NONE',  ( 1.502624671916010790, -0.05778040916215522460, 0.4822834645669289988 ) ) ;
#54084 = CARTESIAN_POINT ( 'NONE',  ( 0.1998031496062994405, -0.3460692066303958092, -1.981627296587926690 ) ) ;
#54085 = CARTESIAN_POINT ( 'NONE',  ( 0.1058382717557500713, -0.3949938075777409408, -1.187664041994750619 ) ) ;
#54086 = CARTESIAN_POINT ( 'NONE',  ( 0.3996062992125986590, -0.1070741851644053111, -2.631233595800525293 ) ) ;
#54087 = PLANE ( 'NONE',  #19729 ) ;
#54088 = CARTESIAN_POINT ( 'NONE',  ( -0.2867679344610364334, -0.2867679344610367109, -0.2086614173228345526 ) ) ;
#54089 = CARTESIAN_POINT ( 'NONE',  ( -0.1640419947506555343, -0.2845877964562159024, 0.3641732283464567677 ) ) ;
#54090 = CARTESIAN_POINT ( 'NONE',  ( -0.2165354330708654795, -0.5400638737290845981, -0.3530559997133363437 ) ) ;
#54091 = CARTESIAN_POINT ( 'NONE',  ( 0.7152230971128614723, -0.3162353388693409650, -0.4822834645669289433 ) ) ;
#54092 = CARTESIAN_POINT ( 'NONE',  ( 0.2891555358219910499, -0.2891555358219909944, -2.222440944881889813 ) ) ;
#54093 = CARTESIAN_POINT ( 'NONE',  ( -0.01312335958005186876, -0.004921259842519870586, -0.3153832671262229437 ) ) ;
#54094 = CARTESIAN_POINT ( 'NONE',  ( -0.9776902887139098386, 0.2952755905511810774, -0.1292274648535930714 ) ) ;
#54095 = CARTESIAN_POINT ( 'NONE',  ( -1.607611548556429737, 0.2952755905511810774, -0.1292274648535930714 ) ) ;
#54096 = CARTESIAN_POINT ( 'NONE',  ( 0.2362204724409451007, -0.4091458600556402980, -2.139107611548556331 ) ) ;
#54097 = DIRECTION ( 'NONE',  ( 0.000000000000000000, 0.000000000000000000, 1.000000000000000000 ) ) ;
#54098 = VERTEX_POINT ( 'NONE', #67679 ) ;
#54099 = EDGE_LOOP ( 'NONE', ( #71502, #8191 ) ) ;
#54100 = CARTESIAN_POINT ( 'NONE',  ( 1.095800524934383846, -0.3162353388693405765, 0.4822834645669290543 ) ) ;
#54101 = CARTESIAN_POINT ( 'NONE',  ( -1.633858267716534529, -0.5400638737290845981, -0.3530559997133363437 ) ) ;
#54103 = CARTESIAN_POINT ( 'NONE',  ( -1.141732283464566011, 0.2952755905511811885, 0.000000000000000000 ) ) ;
#54102 = CARTESIAN_POINT ( 'NONE',  ( -1.404199475065615932, -0.3690944881889765550, -0.3153832671262227771 ) ) ;
#54104 = CARTESIAN_POINT ( 'NONE',  ( 4.797336870675655290E-17, -0.3917322834645669549, -2.206017429624985038 ) ) ;
#54105 = CARTESIAN_POINT ( 'NONE',  ( -1.646051170424378096, 0.000000000000000000, -0.3464511005275205946 ) ) ;
#54106 = CARTESIAN_POINT ( 'NONE',  ( 1.220472440944882608, 0.2952755905511811885, 0.000000000000000000 ) ) ;
#54107 = CARTESIAN_POINT ( 'NONE',  ( -1.555118110236219930, 0.1660481256975885056, 0.3530559997133364547 ) ) ;
#54108 = CARTESIAN_POINT ( 'NONE',  ( 0.09842519685039434474, -0.5400638737290845981, -0.3530559997133363437 ) ) ;
#54109 = CARTESIAN_POINT ( 'NONE',  ( -0.09842519685039295696, 0.1660481256975883668, -0.3530559997133364547 ) ) ;
#54110 = EDGE_CURVE ( 'NONE', #1055, #29055, #22379, .T. ) ;
#54111 = CARTESIAN_POINT ( 'NONE',  ( -1.404199475065615932, -0.4281496062992127816, -0.4176697321401328100 ) ) ;
#54112 = CARTESIAN_POINT ( 'NONE',  ( 0.3392501089628018329, 0.1958661417322835607, 0.09908136482939623735 ) ) ;
#54113 = CARTESIAN_POINT ( 'NONE',  ( 0.1312335958005255154, -0.6046776061558807314, 0.2411417322834647770 ) ) ;
#54114 = CARTESIAN_POINT ( 'NONE',  ( 0.1049643490035304938, -0.3917322834645669549, -1.967191601049868899 ) ) ;
#54115 = CARTESIAN_POINT ( 'NONE',  ( -1.167979002624671470, -0.004921259842519576551, 0.3153832671262227771 ) ) ;
#54116 = ORIENTED_EDGE ( 'NONE', *, *, #44186, .T. ) ;
#54117 = CARTESIAN_POINT ( 'NONE',  ( 0.2891555358219910499, 0.2891555358219910499, -2.500000000000000444 ) ) ;
#54118 = B_SPLINE_CURVE_WITH_KNOTS ( 'NONE', 3,
 ( #74592, #22409, #16936, #22816, #48473, #41747 ),
 .UNSPECIFIED., .F., .F.,
 ( 4, 2, 4 ),
 ( 0.001230262104865860332, 0.001674292070114364369, 0.002118322035362868189 ),
 .UNSPECIFIED. ) ;
#54119 = ORIENTED_EDGE ( 'NONE', *, *, #35777, .T. ) ;
#54120 = DIRECTION ( 'NONE',  ( 0.000000000000000000, 0.000000000000000000, -1.000000000000000000 ) ) ;
#54121 = CARTESIAN_POINT ( 'NONE',  ( -1.345144356955379816, -0.05778040916215560624, -0.4822834645669293319 ) ) ;
#54122 = CARTESIAN_POINT ( 'NONE',  ( -0.1070741851644056997, 0.3996062992125986035, -1.108923884514435798 ) ) ;
#54123 = CARTESIAN_POINT ( 'NONE',  ( -1.561679790026246017, 0.05413385826771666132, 0.4176697321401328100 ) ) ;
#54124 = CARTESIAN_POINT ( 'NONE',  ( -1.725721784776902190, -0.05778040916215522460, 0.4822834645669289988 ) ) ;
#54125 = CARTESIAN_POINT ( 'NONE',  ( -0.9776902887139098386, 0.2952755905511810219, -0.1292274648535930437 ) ) ;
#54126 = CARTESIAN_POINT ( 'NONE',  ( 1.220472440944882386, -0.1870078740157480046, 1.254653134982923898E-17 ) ) ;
#54127 = CARTESIAN_POINT ( 'NONE',  ( -0.1958661417322834220, -0.3392501089628018884, 0.1646981627296586759 ) ) ;
#54128 = CARTESIAN_POINT ( 'NONE',  ( -0.1902887139107604098, 0.1771653543307087075, -0.09757992244046823083 ) ) ;
#54129 = CARTESIAN_POINT ( 'NONE',  ( -0.8136482939632537770, -0.5023911411419708095, 0.1820866141732285504 ) ) ;
#54130 = CARTESIAN_POINT ( 'NONE',  ( -1.023622047244093558, -0.1870078740157479769, 0.4822834645669291653 ) ) ;
#54131 = CARTESIAN_POINT ( 'NONE',  ( 0.8661417322834652488, -0.1870078740157480879, -0.4822834645669291653 ) ) ;
#54132 = CARTESIAN_POINT ( 'NONE',  ( -0.7939632545931750718, -0.05778040916215560624, -0.4822834645669293319 ) ) ;
#54133 = CARTESIAN_POINT ( 'NONE',  ( 0.5314960629921393620, 2.751923335154144556, -3.846978723397334488 ) ) ;
#54134 = ORIENTED_EDGE ( 'NONE', *, *, #46355, .T. ) ;
#54135 = CARTESIAN_POINT ( 'NONE',  ( -1.548556430446193399, -0.6046776061558809534, -0.2411417322834644161 ) ) ;
#54136 = DIRECTION ( 'NONE',  ( 0.000000000000000000, -0.000000000000000000, 1.000000000000000000 ) ) ;
#54137 =( NAMED_UNIT ( * ) PLANE_ANGLE_UNIT ( ) SI_UNIT ( $, .RADIAN. ) );
#54138 = CARTESIAN_POINT ( 'NONE',  ( -0.4091458600556402980, -0.2362204724409451284, -1.469816272965879245 ) ) ;
#54139 = FACE_OUTER_BOUND ( 'NONE', #36329, .T. ) ;
#54140 = EDGE_CURVE ( 'NONE', #52448, #23493, #66464, .T. ) ;
#54141 = CARTESIAN_POINT ( 'NONE',  ( -0.3917322834645671215, 0.1049643490035301469, -0.6548556430446192955 ) ) ;
#54142 = CARTESIAN_POINT ( 'NONE',  ( -0.3917322834645670104, -7.196005306013484475E-17, -2.328740157480315265 ) ) ;
#54143 = CARTESIAN_POINT ( 'NONE',  ( -0.6496062992125976043, 0.1660481256975883668, -0.3530559997133364547 ) ) ;
#54144 = CARTESIAN_POINT ( 'NONE',  ( 1.233595800524935227, 0.2306618581243847221, -0.2411417322834647770 ) ) ;
#54145 = CARTESIAN_POINT ( 'NONE',  ( -0.1070741851644056997, 0.3996062992125984925, -0.08333333333333337034 ) ) ;
#54147 = CARTESIAN_POINT ( 'NONE',  ( 1.112371124080195450, -4.927456884911482678E-16, 0.4445507791589062840 ) ) ;
#54146 = DIRECTION ( 'NONE',  ( 1.000000000000000000, -0.000000000000000000, -0.000000000000000000 ) ) ;
#54148 = CARTESIAN_POINT ( 'NONE',  ( -1.397637795275589623, 0.1660481256975885056, 0.3530559997133364547 ) ) ;
#54149 = CARTESIAN_POINT ( 'NONE',  ( -0.6627296587926503335, -0.6692913385826771977, 0.1292274648535927661 ) ) ;
#54150 = CARTESIAN_POINT ( 'NONE',  ( -0.3917322834645668994, -0.1049643490035306742, -0.1259649361866648498 ) ) ;
#54151 = CARTESIAN_POINT ( 'NONE',  ( 0.3477690288713918276, 0.1771653543307087630, 0.09757992244046791164 ) ) ;
#54152 = CARTESIAN_POINT ( 'NONE',  ( -9.594673741351313045E-17, 0.3917322834645670104, -0.3996062992125985480 ) ) ;
#54153 = CARTESIAN_POINT ( 'NONE',  ( 0.3412073490813655186, -0.5023911411419708095, -0.1820866141732282451 ) ) ;
#54154 = CARTESIAN_POINT ( 'NONE',  ( 1.043307086614173818, -0.4536011799217368745, -0.2665933059059886201 ) ) ;
#54155 = CARTESIAN_POINT ( 'NONE',  ( 0.9383202099737536495, -0.3162353388693405765, 0.4822834645669290543 ) ) ;
#54156 = CARTESIAN_POINT ( 'NONE',  ( -0.4461942257217840213, -0.5023911411419708095, -0.1820866141732282451 ) ) ;
#54157 = CARTESIAN_POINT ( 'NONE',  ( -0.1958661417322834220, -0.3392501089628018884, -1.790026246719160330 ) ) ;
#54158 = CARTESIAN_POINT ( 'NONE',  ( -1.082677165354329896, -0.5400638737290845981, -0.3530559997133363437 ) ) ;
#54159 = ADVANCED_FACE ( 'NONE', ( #60523 ), #46642, .F. ) ;
#54160 = CARTESIAN_POINT ( 'NONE',  ( -1.148293963254592542, 0.1771653543307087630, 0.09757992244046791164 ) ) ;
#54161 = CARTESIAN_POINT ( 'NONE',  ( 5.785732909357575061E-17, -0.4724409448818898682, -0.1555118110236220763 ) ) ;
#54162 = CARTESIAN_POINT ( 'NONE',  ( -0.7414698162729651543, -0.5511811023622046335, 0.09757992244046803654 ) ) ;
#54163 = CARTESIAN_POINT ( 'NONE',  ( -0.2427821522309703550, -0.3162353388693405765, 0.4822834645669290543 ) ) ;
#54164 = LINE ( 'NONE', #41139, #64002 ) ;
#54165 = CARTESIAN_POINT ( 'NONE',  ( 0.4724409448818904789, -0.1870078740157479769, 0.3641732283464567677 ) ) ;
#54166 = CARTESIAN_POINT ( 'NONE',  ( -0.3871391076115479057, -0.2845877964562161244, -0.3641732283464567121 ) ) ;
#54167 = CARTESIAN_POINT ( 'NONE',  ( -0.8989501312335946848, -0.6692913385826771977, 0.1292274648535927661 ) ) ;
#54168 = CARTESIAN_POINT ( 'NONE',  ( -1.633858267716534529, -0.5400638737290845981, -0.3530559997133363437 ) ) ;
#54169 = DIRECTION ( 'NONE',  ( 1.000000000000000000, -0.000000000000000000, -0.000000000000000000 ) ) ;
#54170 = CIRCLE ( 'NONE', #12546, 0.2736220472440938911 ) ;
#54171 = CARTESIAN_POINT ( 'NONE',  ( -0.01968503937007793844, 0.1660481256975883668, -0.3530559997133364547 ) ) ;
#54172 = CARTESIAN_POINT ( 'NONE',  ( 0.2925321140481932369, -0.2925321140481931814, -1.435039370078740051 ) ) ;
#54173 = DIRECTION ( 'NONE',  ( 1.000000000000000000, 0.000000000000000000, 0.000000000000000000 ) ) ;
#54174 = CARTESIAN_POINT ( 'NONE',  ( -0.1049868766404193215, 0.1283753931104746893, -0.1820866141732285504 ) ) ;
#54175 = CARTESIAN_POINT ( 'NONE',  ( -0.01312335958005186876, -0.4281496062992124485, 0.4176697321401328655 ) ) ;
#54176 = CARTESIAN_POINT ( 'NONE',  ( -1.555118110236219930, -0.5400638737290845981, -0.3530559997133363437 ) ) ;
#54177 = CARTESIAN_POINT ( 'NONE',  ( 1.614173228346457378, -0.6692913385826771977, 8.415575281601705876E-17 ) ) ;
#54178 = CARTESIAN_POINT ( 'NONE',  ( 1.509186351706037543, 0.05413385826771666132, 0.4176697321401328100 ) ) ;
#54179 =( BOUNDED_SURFACE ( )  B_SPLINE_SURFACE ( 1, 2, ( 
 ( #67267, #79081, #47053, #9600, #72745, #80322, #22224, #28122, #53777, #73995, #16342, #66434, #8770, #41985, #79489, #34444, #10015, #60111, #2464, #21804, #35680, #78661, #20982, #72337, #14685, #40342, #47468, #73160, #15509, #66023, #34861, #54192, #8359, #2872, #42393, #5344, #81141, #24278, #81963, #30182, #10839, #11257, #44041, #31003, #5745, #16754, #74410, #43209, #68499, #49949, #63410, #37736, #12078, #56671, #10437, #4513, #55844, #50358, #23045, #75647, #74827, #68092, #17171, #81553, #55023, #42805, #80731, #23456, #4105, #17987, #48712, #36915, #49121, #36094, #61765, #69734, #43623, #4933, #18399, #29771, #24690, #55432, #36499, #17576, #62174, #23871, #68905, #49538, #63005, #75233, #62591, #30601, #56267, #69325, #11675, #76055, #37332, #82371, #63821, #39400, #20469, #52011, #57080, #20046, #1120, #76470, #46122, #694, #18797, #65083, #7421, #33091, #71817, #45283, #44441, #64244, #31416, #32250, #26771, #58758, #32665, #19621, #14167, #82775, #25097, #65512, #6579, #50769, #70978, #6998, #39824, #70134, #12485, #77716, #13743, #13323, #38564, #64659, #45698, #52426, #38149, #57911, #58332, #51589, #6160, #31835, #57496, #83187, #25510, #51175, #78136, #76871, #19203, #44852, #70550, #12905, #26350, #275, #71394, #25930, #38976, #77290, #80941, #54831, #61978, #36302, #16970, #8259, #74626, #67894, #48508, #74207, #65922, #49338, #61144, #27185, #3496, #43014, #42609, #22847, #16135, #28748, #4315, #10231, #41781, #61568, #29980, #68310, #52849, #78560, #55643, #75038, #81354, #14586, #54410, #10647, #23666, #35898, #20886, #17384, #33511, #7844, #40239, #59173, #80121, #1531, #46537, #23256, #29161, #72237, #33924, #60732, #80536, #3084, #22439, #48099, #73798, #67474, #9808, #35480, #16554, #42198, #3911, #29572, #55234, #48926, #11468, #37947, #12291, #43831, #24492, #24896, #57710, #19004, #19423, #30394, #4720, #56884, #82176, #63624, #77091, #51386, #25726, #44653, #24079, #18197, #69534, #64039, #36708, #5961, #5143, #56059, #30808, #11884, #68709, #56473, #11050, #37125, #17787, #31631, #62383, #50565, #62809, #81769, #49748, #73, #57291, #18603, #32050, #75449, #38363, #43422, #69119, #31216, #50159, #82989, #75855, #37536, #25310, #6378, #82577, #70349, #50974, #76269, #63212, #5552, #44246, #69935, #76672, #12704, #71196, #13539, #77515, #51810, #19850, #59390, #26989, #46340, #33729, #45499, #39195, #27405, #7651, #8067, #72034, #64878, #7217, #32888, #1748, #1338, #33321, #58557, #21101, #26580, #13966, #45916, #14390, #52233, #40048, #494, #923, #65734, #77936, #53066, #78777, #20266, #71614, #46760, #66138, #39622, #65312, #72453, #58983, #52652, #14802, #78357, #20689, #26149, #40460, #8476, #34145, #59806, #2161, #53487, #27827, #79197, #45075, #70778, #13129, #38780, #64457, #6794, #32465, #58127, #2579, #79611, #47589, #73283, #53898, #28238, #21928, #35801, #3403, #22752, #10137, #15631, #41288, #3816, #67383, #67800, #48412, #66973, #9306, #34976, #61468, #61053, #9717, #60640, #80847, #2990, #73704, #22345, #74112, #28656, #16458, #60229, #54315, #42103, #80026, #29477, #55136, #48005, #16044, #23159, #42512, #41690, #35388, #48828, #29066, #54737, #74529, #80442, #16875, #68214, #10551, #36209, #61878, #4219, #29883, #55546, #21513, #47172, #72863, #15212, #40872, #66554, #8887, #34564, #68612, #31536, #23986, #50468, #24800, #56381, #37029, #37444, #70248, #57192, #31952, #42917, #17289, #69438, #11372, #76172, #6276, #63939, #38261, #82894, #36609, #30718, #82080, #76580, #49241, #18509, #17693, #10952, #43321, #24394, #81255, #69021, #23570, #49653, #30296, #44152, #74944, #63118, #75345, #62288, #4625, #12604, #69844, #31118, #44559, #55962, #50880, #81675, #62711, #43734, #5049, #12194, #18101, #25214, #18908, #50064, #11791, #75759, #5456, #56785, #5860, #82485, #37852, #63529, #40356, #77409, #7114, #27303, #65206, #77834, #6695, #65632, #46659, #78255, #83304, #46238, #52962, #19322, #72353, #26886, #44974, #7963, #33625, #59288, #14700, #71512, #70670, #32785, #57613, #58454, #78676, #1645, #58879 ),
 ( #45814, #64775, #7543, #20586, #20997, #38680, #813, #33215, #20164, #25626, #32365, #13026, #76992, #8373, #58027, #66035, #64358, #19744, #39947, #45398, #391, #52546, #51289, #14283, #1237, #39518, #26049, #71934, #13859, #51707, #71095, #13438, #39094, #26476, #52126, #73603, #15945, #8785, #74423, #2889, #53388, #28551, #68105, #67694, #47895, #41184, #53793, #29376, #9614, #66874, #3297, #3713, #16355, #79095, #21414, #80744, #16770, #55037, #40764, #79504, #41999, #10029, #35284, #47067, #23058, #59702, #48726, #66449, #2057, #21820, #27721, #42407, #9204, #34039, #15108, #34458, #60127, #2478, #28137, #47483, #73176, #48311, #41591, #60946, #22652, #15526, #34877, #35694, #79924, #80337, #28961, #60538, #54208, #22240, #74008, #67281, #54626, #61359, #72759, #75247, #62607, #11271, #37347, #17592, #5357, #49138, #36514, #63020, #10853, #18412, #31017, #43223, #68921, #12093, #31431, #42819, #62190, #44055, #36930, #68513, #56685, #55859, #4948, #74842, #82386, #5761, #24703, #57093, #82789, #50783, #23887, #4527, #49552, #61778, #30197, #43636, #76070, #17186, #81155, #69747, #81569, #50372, #37750, #30618, #56281, #49964, #25110, #63424, #44458, #55446, #29784, #81978, #24293, #76484, #18811, #10451, #36107, #4119, #75661, #18002, #69339, #23471, #11689, #13756, #6592, #57511, #32263, #45296, #78572, #57924, #52862, #12920, #19217, #39413, #20898, #52024, #64258, #31848, #83202, #59186, #65096, #20059, #33523, #25524, #39837, #70148, #63836, #32679, #51189, #7434, #76887, #12500, #26783, #65526, #707, #46135, #1133, #77730, #7857, #44865, #70565, #288, #52439, #78150, #45712, #38577, #1544, #38162, #27198, #25944, #6173, #51602, #77305, #19635, #20481, #7011, #71829, #70992, #13336, #58346, #38989, #26364, #64672, #14179, #71409, #33104, #58770, #29281, #66347, #79400, #16255, #54108, #66773, #78991, #54526, #35598, #67184, #72249, #35187, #41902, #8271, #61261, #15850, #33936, #80241, #22557, #48219, #3615, #60438, #59601, #21719, #46551, #47383, #67596, #73915, #47798, #34779, #54945, #14598, #40251, #80651, #73074, #65934, #2789, #22140, #1956, #27618, #53281, #9514, #28864, #28449, #53692, #79824, #60848, #9927, #21311, #15423, #73502, #9106, #46964, #72656, #15006, #40663, #8686, #34356, #60022, #2377, #28034, #41084, #41499, #3200, #17907, #18314, #62925, #56182, #4845, #11996, #11590, #68827, #75974, #50276, #30923, #23375, #5259, #81885, #62507, #30520, #81059, #63327, #75154, #42311, #17499, #56997, #56589, #36834, #30102, #42725, #43956, #24196, #55764, #75566, #69652, #82290, #68009, #10354, #37650, #5665, #31332, #36014, #24609, #49043, #43543, #49866, #81471, #62094, #69242, #22964, #48630, #74325, #61685, #4026, #11174, #36421, #37250, #16672, #29690, #55353, #74740, #17088, #23788, #49459, #68421, #10761, #4436, #43129, #70050, #19120, #57823, #7764, #70466, #65431, #25426, #31752, #51928, #33430, #64574, #76788, #44359, #12405, #71728, #77633, #32583, #46033, #38063, #52345, #82694, #76384, #45193, #63739, #19965, #6078, #25013, #39310, #78052, #13246, #58671, #13657, #6911, #20381, #57414, #190, #14083, #83107, #51091, #44769, #12823, #38480, #64164, #6497, #64998, #58246, #611, #71310, #32167, #25843, #7333, #70896, #45616, #26267, #51503, #77207, #19536, #33001, #38895, #1036, #26690, #39735, #50686, #18717, #59920, #2691, #40568, #54012, #14503, #1858, #28351, #59505, #67083, #79724, #8588, #34259, #60751, #80140, #8173, #27520, #9415, #2275, #33838, #22041, #21212, #66249, #40156, #47701, #54430, #73397, #22462, #48120, #16155, #72561, #53176, #14908, #27103, #78891, #9008, #41401, #65840, #73818, #34680, #27938, #15747, #28768, #35085, #78474, #20798, #41802, #67493, #9829, #46867, #53596, #3103, #59091, #60343, #46454, #1446, #52765, #72147, #79305, #21623, #47283, #72973, #15325, #40990, #66669, #56084, #49769, #29184, #61997, #54852, #4334, #35921, #4743, #11491, #74228, #48946, #37145, #61587, #74647, #24100, #81373, #10667, #16573, #30416, #43442, #43034, #61164, #68730, #75469, #80555, #69140, #75057, #22867 ) ),
 .UNSPECIFIED., .F., .F., .F. ) 
 B_SPLINE_SURFACE_WITH_KNOTS ( ( 2, 2 ),
 ( 3, 2, 2, 2, 2, 2, 2, 2, 2, 2, 2, 2, 2, 2, 2, 2, 2, 2, 2, 2, 2, 2, 2, 2, 2, 2, 2, 2, 2, 2, 2, 2, 2, 2, 2, 2, 2, 2, 2, 2, 2, 2, 2, 2, 2, 2, 2, 2, 2, 2, 2, 2, 2, 2, 2, 2, 2, 2, 2, 2, 2, 2, 2, 2, 2, 2, 2, 2, 2, 2, 2, 2, 2, 2, 2, 2, 2, 2, 2, 2, 2, 2, 2, 2, 2, 2, 2, 2, 2, 2, 2, 2, 2, 2, 2, 2, 2, 2, 2, 2, 2, 2, 2, 2, 2, 2, 2, 2, 2, 2, 2, 2, 2, 2, 2, 2, 2, 2, 2, 2, 2, 2, 2, 2, 2, 2, 2, 2, 2, 2, 2, 2, 2, 2, 2, 2, 2, 2, 2, 2, 2, 2, 2, 2, 2, 2, 2, 2, 2, 2, 2, 2, 2, 2, 2, 2, 2, 2, 2, 2, 2, 2, 2, 2, 2, 2, 2, 2, 2, 2, 2, 2, 2, 2, 2, 2, 2, 2, 2, 2, 2, 2, 2, 2, 2, 2, 2, 2, 2, 2, 2, 2, 2, 2, 2, 2, 2, 2, 2, 2, 2, 2, 2, 2, 2, 2, 2, 2, 2, 2, 2, 2, 2, 2, 2, 2, 2, 2, 2, 2, 2, 2, 2, 2, 2, 2, 2, 2, 2, 2, 2, 2, 2, 2, 2, 2, 2, 2, 2, 2, 2, 2, 2, 2, 2, 2, 2, 2, 2, 2, 2, 2, 2, 2, 2, 3 ),
 ( 0.000000000000000000, 1.000000000000000000 ),
 ( 0.000000000000000000, 0.003787878787878787984, 0.007575757575757575968, 0.01136363636363636395, 0.01515151515151515194, 0.01893939393939393992, 0.02272727272727272790, 0.02651515151515151589, 0.03030303030303030387, 0.03409090909090908839, 0.03787878787878787984, 0.04166666666666666435, 0.04545454545454545581, 0.04924242424242424032, 0.05303030303030303177, 0.05681818181818181629, 0.06060606060606060774, 0.06439393939393939226, 0.06818181818181817677, 0.07196969696969697516, 0.07575757575757575968, 0.07954545454545454419, 0.08333333333333332871, 0.08712121212121212710, 0.09090909090909091161, 0.09469696969696969613, 0.09848484848484848064, 0.1022727272727272790, 0.1060606060606060635, 0.1098484848484848481, 0.1136363636363636326, 0.1174242424242424310, 0.1212121212121212155, 0.1250000000000000000, 0.1287878787878787845, 0.1325757575757575690, 0.1363636363636363535, 0.1401515151515151381, 0.1439393939393939503, 0.1477272727272727348, 0.1515151515151515194, 0.1553030303030303039, 0.1590909090909090884, 0.1628787878787878729, 0.1666666666666666574, 0.1704545454545454419, 0.1742424242424242542, 0.1780303030303030387, 0.1818181818181818232, 0.1856060606060606077, 0.1893939393939393923, 0.1931818181818181768, 0.1969696969696969613, 0.2007575757575757458, 0.2045454545454545581, 0.2083333333333333426, 0.2121212121212121271, 0.2159090909090909116, 0.2196969696969696961, 0.2234848484848484806, 0.2272727272727272652, 0.2310606060606060497, 0.2348484848484848619, 0.2386363636363636465, 0.2424242424242424310, 0.2462121212121212155, 0.2500000000000000000, 0.2537878787878787845, 0.2575757575757575690, 0.2613636363636363535, 0.2651515151515151381, 0.2689393939393939226, 0.2727272727272727071, 0.2765151515151514916, 0.2803030303030302761, 0.2840909090909091161, 0.2878787878787879007, 0.2916666666666666852, 0.2954545454545454697, 0.2992424242424242542, 0.3030303030303030387, 0.3068181818181818232, 0.3106060606060606077, 0.3143939393939393923, 0.3181818181818181768, 0.3219696969696969613, 0.3257575757575757458, 0.3295454545454545303, 0.3333333333333333148, 0.3371212121212120993, 0.3409090909090908839, 0.3446969696969697239, 0.3484848484848485084, 0.3522727272727272929, 0.3560606060606060774, 0.3598484848484848619, 0.3636363636363636465, 0.3674242424242424310, 0.3712121212121212155, 0.3750000000000000000, 0.3787878787878787845, 0.3825757575757575690, 0.3863636363636363535, 0.3901515151515151381, 0.3939393939393939226, 0.3977272727272727071, 0.4015151515151514916, 0.4053030303030302761, 0.4090909090909091161, 0.4128787878787879007, 0.4166666666666666852, 0.4204545454545454697, 0.4242424242424242542, 0.4280303030303030387, 0.4318181818181818232, 0.4356060606060606077, 0.4393939393939393923, 0.4431818181818181768, 0.4469696969696969613, 0.4507575757575757458, 0.4545454545454545303, 0.4583333333333333148, 0.4621212121212120993, 0.4659090909090908839, 0.4696969696969697239, 0.4734848484848485084, 0.4772727272727272929, 0.4810606060606060774, 0.4848484848484848619, 0.4886363636363636465, 0.4924242424242424310, 0.4962121212121212155, 0.5000000000000000000, 0.5037878787878787845, 0.5075757575757575690, 0.5113636363636363535, 0.5151515151515151381, 0.5189393939393939226, 0.5227272727272727071, 0.5265151515151514916, 0.5303030303030302761, 0.5340909090909090606, 0.5378787878787878451, 0.5416666666666666297, 0.5454545454545454142, 0.5492424242424241987, 0.5530303030303029832, 0.5568181818181817677, 0.5606060606060605522, 0.5643939393939394478, 0.5681818181818182323, 0.5719696969696970168, 0.5757575757575758013, 0.5795454545454545858, 0.5833333333333333703, 0.5871212121212121549, 0.5909090909090909394, 0.5946969696969697239, 0.5984848484848485084, 0.6022727272727272929, 0.6060606060606060774, 0.6098484848484848619, 0.6136363636363636465, 0.6174242424242424310, 0.6212121212121212155, 0.6250000000000000000, 0.6287878787878787845, 0.6325757575757575690, 0.6363636363636363535, 0.6401515151515151381, 0.6439393939393939226, 0.6477272727272727071, 0.6515151515151514916, 0.6553030303030302761, 0.6590909090909090606, 0.6628787878787878451, 0.6666666666666666297, 0.6704545454545454142, 0.6742424242424241987, 0.6780303030303029832, 0.6818181818181817677, 0.6856060606060605522, 0.6893939393939394478, 0.6931818181818182323, 0.6969696969696970168, 0.7007575757575758013, 0.7045454545454545858, 0.7083333333333333703, 0.7121212121212121549, 0.7159090909090909394, 0.7196969696969697239, 0.7234848484848485084, 0.7272727272727272929, 0.7310606060606060774, 0.7348484848484848619, 0.7386363636363636465, 0.7424242424242424310, 0.7462121212121212155, 0.7500000000000000000, 0.7537878787878787845, 0.7575757575757575690, 0.7613636363636363535, 0.7651515151515151381, 0.7689393939393939226, 0.7727272727272727071, 0.7765151515151514916, 0.7803030303030302761, 0.7840909090909090606, 0.7878787878787878451, 0.7916666666666666297, 0.7954545454545454142, 0.7992424242424241987, 0.8030303030303029832, 0.8068181818181817677, 0.8106060606060605522, 0.8143939393939394478, 0.8181818181818182323, 0.8219696969696970168, 0.8257575757575758013, 0.8295454545454545858, 0.8333333333333333703, 0.8371212121212121549, 0.8409090909090909394, 0.8446969696969697239, 0.8484848484848485084, 0.8522727272727272929, 0.8560606060606060774, 0.8598484848484848619, 0.8636363636363636465, 0.8674242424242424310, 0.8712121212121212155, 0.8750000000000000000, 0.8787878787878787845, 0.8825757575757575690, 0.8863636363636363535, 0.8901515151515151381, 0.8939393939393939226, 0.8977272727272727071, 0.9015151515151514916, 0.9053030303030302761, 0.9090909090909090606, 0.9128787878787878451, 0.9166666666666666297, 0.9204545454545454142, 0.9242424242424241987, 0.9280303030303029832, 0.9318181818181817677, 0.9356060606060605522, 0.9393939393939394478, 0.9431818181818182323, 0.9469696969696970168, 0.9507575757575758013, 0.9545454545454545858, 0.9583333333333333703, 0.9621212121212121549, 0.9659090909090909394 ),
 .UNSPECIFIED. ) 
 GEOMETRIC_REPRESENTATION_ITEM ( )  RATIONAL_B_SPLINE_SURFACE ( (
 ( 1.000000000000000000, 0.9659258262890683122, 1.000000000000000000, 0.9659258262890683122, 1.000000000000000000, 0.9659258262890683122, 1.000000000000000000, 0.9659258262890683122, 1.000000000000000000, 0.9659258262890683122, 1.000000000000000000, 0.9659258262890683122, 1.000000000000000000, 0.9659258262890683122, 1.000000000000000000, 0.9659258262890683122, 1.000000000000000000, 0.9659258262890683122, 1.000000000000000000, 0.9659258262890683122, 1.000000000000000000, 0.9659258262890683122, 1.000000000000000000, 0.9659258262890683122, 1.000000000000000000, 0.9659258262890683122, 1.000000000000000000, 0.9659258262890683122, 1.000000000000000000, 0.9659258262890683122, 1.000000000000000000, 0.9659258262890683122, 1.000000000000000000, 0.9659258262890683122, 1.000000000000000000, 0.9659258262890683122, 1.000000000000000000, 0.9659258262890683122, 1.000000000000000000, 0.9659258262890683122, 1.000000000000000000, 0.9659258262890683122, 1.000000000000000000, 0.9659258262890683122, 1.000000000000000000, 0.9659258262890683122, 1.000000000000000000, 0.9659258262890683122, 1.000000000000000000, 0.9659258262890683122, 1.000000000000000000, 0.9659258262890683122, 1.000000000000000000, 0.9659258262890683122, 1.000000000000000000, 0.9659258262890683122, 1.000000000000000000, 0.9659258262890683122, 1.000000000000000000, 0.9659258262890683122, 1.000000000000000000, 0.9659258262890683122, 1.000000000000000000, 0.9659258262890683122, 1.000000000000000000, 0.9659258262890683122, 1.000000000000000000, 0.9659258262890683122, 1.000000000000000000, 0.9659258262890683122, 1.000000000000000000, 0.9659258262890683122, 1.000000000000000000, 0.9659258262890683122, 1.000000000000000000, 0.9659258262890683122, 1.000000000000000000, 0.9659258262890683122, 1.000000000000000000, 0.9659258262890683122, 1.000000000000000000, 0.9659258262890683122, 1.000000000000000000, 0.9659258262890683122, 1.000000000000000000, 0.9659258262890683122, 1.000000000000000000, 0.9659258262890683122, 1.000000000000000000, 0.9659258262890683122, 1.000000000000000000, 0.9659258262890683122, 1.000000000000000000, 0.9659258262890683122, 1.000000000000000000, 0.9659258262890683122, 1.000000000000000000, 0.9659258262890683122, 1.000000000000000000, 0.9659258262890683122, 1.000000000000000000, 0.9659258262890683122, 1.000000000000000000, 0.9659258262890683122, 1.000000000000000000, 0.9659258262890683122, 1.000000000000000000, 0.9659258262890683122, 1.000000000000000000, 0.9659258262890683122, 1.000000000000000000, 0.9659258262890683122, 1.000000000000000000, 0.9659258262890683122, 1.000000000000000000, 0.9659258262890683122, 1.000000000000000000, 0.9659258262890683122, 1.000000000000000000, 0.9659258262890683122, 1.000000000000000000, 0.9659258262890683122, 1.000000000000000000, 0.9659258262890683122, 1.000000000000000000, 0.9659258262890683122, 1.000000000000000000, 0.9659258262890683122, 1.000000000000000000, 0.9659258262890683122, 1.000000000000000000, 0.9659258262890683122, 1.000000000000000000, 0.9659258262890683122, 1.000000000000000000, 0.9659258262890683122, 1.000000000000000000, 0.9659258262890683122, 1.000000000000000000, 0.9659258262890683122, 1.000000000000000000, 0.9659258262890683122, 1.000000000000000000, 0.9659258262890683122, 1.000000000000000000, 0.9659258262890683122, 1.000000000000000000, 0.9659258262890683122, 1.000000000000000000, 0.9659258262890683122, 1.000000000000000000, 0.9659258262890683122, 1.000000000000000000, 0.9659258262890683122, 1.000000000000000000, 0.9659258262890683122, 1.000000000000000000, 0.9659258262890683122, 1.000000000000000000, 0.9659258262890683122, 1.000000000000000000, 0.9659258262890683122, 1.000000000000000000, 0.9659258262890683122, 1.000000000000000000, 0.9659258262890683122, 1.000000000000000000, 0.9659258262890683122, 1.000000000000000000, 0.9659258262890683122, 1.000000000000000000, 0.9659258262890683122, 1.000000000000000000, 0.9659258262890683122, 1.000000000000000000, 0.9659258262890683122, 1.000000000000000000, 0.9659258262890683122, 1.000000000000000000, 0.9659258262890683122, 1.000000000000000000, 0.9659258262890683122, 1.000000000000000000, 0.9659258262890683122, 1.000000000000000000, 0.9659258262890683122, 1.000000000000000000, 0.9659258262890683122, 1.000000000000000000, 0.9659258262890683122, 1.000000000000000000, 0.9659258262890683122, 1.000000000000000000, 0.9659258262890683122, 1.000000000000000000, 0.9659258262890683122, 1.000000000000000000, 0.9659258262890683122, 1.000000000000000000, 0.9659258262890683122, 1.000000000000000000, 0.9659258262890683122, 1.000000000000000000, 0.9659258262890683122, 1.000000000000000000, 0.9659258262890683122, 1.000000000000000000, 0.9659258262890683122, 1.000000000000000000, 0.9659258262890683122, 1.000000000000000000, 0.9659258262890683122, 1.000000000000000000, 0.9659258262890683122, 1.000000000000000000, 0.9659258262890683122, 1.000000000000000000, 0.9659258262890683122, 1.000000000000000000, 0.9659258262890683122, 1.000000000000000000, 0.9659258262890683122, 1.000000000000000000, 0.9659258262890683122, 1.000000000000000000, 0.9659258262890683122, 1.000000000000000000, 0.9659258262890683122, 1.000000000000000000, 0.9659258262890683122, 1.000000000000000000, 0.9659258262890683122, 1.000000000000000000, 0.9659258262890683122, 1.000000000000000000, 0.9659258262890683122, 1.000000000000000000, 0.9659258262890683122, 1.000000000000000000, 0.9659258262890683122, 1.000000000000000000, 0.9659258262890683122, 1.000000000000000000, 0.9659258262890683122, 1.000000000000000000, 0.9659258262890683122, 1.000000000000000000, 0.9659258262890683122, 1.000000000000000000, 0.9659258262890683122, 1.000000000000000000, 0.9659258262890683122, 1.000000000000000000, 0.9659258262890683122, 1.000000000000000000, 0.9659258262890683122, 1.000000000000000000, 0.9659258262890683122, 1.000000000000000000, 0.9659258262890683122, 1.000000000000000000, 0.9659258262890683122, 1.000000000000000000, 0.9659258262890683122, 1.000000000000000000, 0.9659258262890683122, 1.000000000000000000, 0.9659258262890683122, 1.000000000000000000, 0.9659258262890683122, 1.000000000000000000, 0.9659258262890683122, 1.000000000000000000, 0.9659258262890683122, 1.000000000000000000, 0.9659258262890683122, 1.000000000000000000, 0.9659258262890683122, 1.000000000000000000, 0.9659258262890683122, 1.000000000000000000, 0.9659258262890683122, 1.000000000000000000, 0.9659258262890683122, 1.000000000000000000, 0.9659258262890683122, 1.000000000000000000, 0.9659258262890683122, 1.000000000000000000, 0.9659258262890683122, 1.000000000000000000, 0.9659258262890683122, 1.000000000000000000, 0.9659258262890683122, 1.000000000000000000, 0.9659258262890683122, 1.000000000000000000, 0.9659258262890683122, 1.000000000000000000, 0.9659258262890683122, 1.000000000000000000, 0.9659258262890683122, 1.000000000000000000, 0.9659258262890683122, 1.000000000000000000, 0.9659258262890683122, 1.000000000000000000, 0.9659258262890683122, 1.000000000000000000, 0.9659258262890683122, 1.000000000000000000, 0.9659258262890683122, 1.000000000000000000, 0.9659258262890683122, 1.000000000000000000, 0.9659258262890683122, 1.000000000000000000, 0.9659258262890683122, 1.000000000000000000, 0.9659258262890683122, 1.000000000000000000, 0.9659258262890683122, 1.000000000000000000, 0.9659258262890683122, 1.000000000000000000, 0.9659258262890683122, 1.000000000000000000, 0.9659258262890683122, 1.000000000000000000, 0.9659258262890683122, 1.000000000000000000, 0.9659258262890683122, 1.000000000000000000, 0.9659258262890683122, 1.000000000000000000, 0.9659258262890683122, 1.000000000000000000, 0.9659258262890683122, 1.000000000000000000, 0.9659258262890683122, 1.000000000000000000, 0.9659258262890683122, 1.000000000000000000, 0.9659258262890683122, 1.000000000000000000, 0.9659258262890683122, 1.000000000000000000, 0.9659258262890683122, 1.000000000000000000, 0.9659258262890683122, 1.000000000000000000, 0.9659258262890683122, 1.000000000000000000, 0.9659258262890683122, 1.000000000000000000, 0.9659258262890683122, 1.000000000000000000, 0.9659258262890683122, 1.000000000000000000, 0.9659258262890683122, 1.000000000000000000, 0.9659258262890683122, 1.000000000000000000, 0.9659258262890683122, 1.000000000000000000, 0.9659258262890683122, 1.000000000000000000, 0.9659258262890683122, 1.000000000000000000, 0.9659258262890683122, 1.000000000000000000, 0.9659258262890683122, 1.000000000000000000, 0.9659258262890683122, 1.000000000000000000, 0.9659258262890683122, 1.000000000000000000, 0.9659258262890683122, 1.000000000000000000, 0.9659258262890683122, 1.000000000000000000, 0.9659258262890683122, 1.000000000000000000, 0.9659258262890683122, 1.000000000000000000, 0.9659258262890683122, 1.000000000000000000, 0.9659258262890683122, 1.000000000000000000, 0.9659258262890683122, 1.000000000000000000, 0.9659258262890683122, 1.000000000000000000, 0.9659258262890683122, 1.000000000000000000, 0.9659258262890683122, 1.000000000000000000, 0.9659258262890683122, 1.000000000000000000, 0.9659258262890683122, 1.000000000000000000, 0.9659258262890683122, 1.000000000000000000, 0.9659258262890683122, 1.000000000000000000, 0.9659258262890683122, 1.000000000000000000, 0.9659258262890683122, 1.000000000000000000, 0.9659258262890683122, 1.000000000000000000, 0.9659258262890683122, 1.000000000000000000, 0.9659258262890683122, 1.000000000000000000, 0.9659258262890683122, 1.000000000000000000, 0.9659258262890683122, 1.000000000000000000, 0.9659258262890683122, 1.000000000000000000, 0.9659258262890683122, 1.000000000000000000, 0.9659258262890683122, 1.000000000000000000, 0.9659258262890683122, 1.000000000000000000, 0.9659258262890683122, 1.000000000000000000, 0.9659258262890683122, 1.000000000000000000, 0.9659258262890683122, 1.000000000000000000, 0.9659258262890683122, 1.000000000000000000, 0.9659258262890683122, 1.000000000000000000, 0.9659258262890683122, 1.000000000000000000, 0.9659258262890683122, 1.000000000000000000, 0.9659258262890683122, 1.000000000000000000, 0.9659258262890683122, 1.000000000000000000, 0.9659258262890683122, 1.000000000000000000, 0.9659258262890683122, 1.000000000000000000, 0.9659258262890683122, 1.000000000000000000, 0.9659258262890683122, 1.000000000000000000, 0.9659258262890683122, 1.000000000000000000, 0.9659258262890683122, 1.000000000000000000, 0.9659258262890683122, 1.000000000000000000, 0.9659258262890683122, 1.000000000000000000, 0.9659258262890683122, 1.000000000000000000, 0.9659258262890683122, 1.000000000000000000, 0.9659258262890683122, 1.000000000000000000, 0.9659258262890683122, 1.000000000000000000, 0.9659258262890683122, 1.000000000000000000, 0.9659258262890683122, 1.000000000000000000, 0.9659258262890683122, 1.000000000000000000, 0.9659258262890683122, 1.000000000000000000, 0.9659258262890683122, 1.000000000000000000, 0.9659258262890683122, 1.000000000000000000, 0.9659258262890683122, 1.000000000000000000, 0.9659258262890683122, 1.000000000000000000, 0.9659258262890683122, 1.000000000000000000, 0.9659258262890683122, 1.000000000000000000, 0.9659258262890683122, 1.000000000000000000, 0.9659258262890683122, 1.000000000000000000, 0.9659258262890683122, 1.000000000000000000, 0.9659258262890683122, 1.000000000000000000, 0.9659258262890683122, 1.000000000000000000, 0.9659258262890683122, 1.000000000000000000, 0.9659258262890683122, 1.000000000000000000, 0.9659258262890683122, 1.000000000000000000, 0.9659258262890683122, 1.000000000000000000, 0.9659258262890683122, 1.000000000000000000, 0.9659258262890683122, 1.000000000000000000),
 ( 1.000000000000000000, 0.9659258262890683122, 1.000000000000000000, 0.9659258262890683122, 1.000000000000000000, 0.9659258262890683122, 1.000000000000000000, 0.9659258262890683122, 1.000000000000000000, 0.9659258262890683122, 1.000000000000000000, 0.9659258262890683122, 1.000000000000000000, 0.9659258262890683122, 1.000000000000000000, 0.9659258262890683122, 1.000000000000000000, 0.9659258262890683122, 1.000000000000000000, 0.9659258262890683122, 1.000000000000000000, 0.9659258262890683122, 1.000000000000000000, 0.9659258262890683122, 1.000000000000000000, 0.9659258262890683122, 1.000000000000000000, 0.9659258262890683122, 1.000000000000000000, 0.9659258262890683122, 1.000000000000000000, 0.9659258262890683122, 1.000000000000000000, 0.9659258262890683122, 1.000000000000000000, 0.9659258262890683122, 1.000000000000000000, 0.9659258262890683122, 1.000000000000000000, 0.9659258262890683122, 1.000000000000000000, 0.9659258262890683122, 1.000000000000000000, 0.9659258262890683122, 1.000000000000000000, 0.9659258262890683122, 1.000000000000000000, 0.9659258262890683122, 1.000000000000000000, 0.9659258262890683122, 1.000000000000000000, 0.9659258262890683122, 1.000000000000000000, 0.9659258262890683122, 1.000000000000000000, 0.9659258262890683122, 1.000000000000000000, 0.9659258262890683122, 1.000000000000000000, 0.9659258262890683122, 1.000000000000000000, 0.9659258262890683122, 1.000000000000000000, 0.9659258262890683122, 1.000000000000000000, 0.9659258262890683122, 1.000000000000000000, 0.9659258262890683122, 1.000000000000000000, 0.9659258262890683122, 1.000000000000000000, 0.9659258262890683122, 1.000000000000000000, 0.9659258262890683122, 1.000000000000000000, 0.9659258262890683122, 1.000000000000000000, 0.9659258262890683122, 1.000000000000000000, 0.9659258262890683122, 1.000000000000000000, 0.9659258262890683122, 1.000000000000000000, 0.9659258262890683122, 1.000000000000000000, 0.9659258262890683122, 1.000000000000000000, 0.9659258262890683122, 1.000000000000000000, 0.9659258262890683122, 1.000000000000000000, 0.9659258262890683122, 1.000000000000000000, 0.9659258262890683122, 1.000000000000000000, 0.9659258262890683122, 1.000000000000000000, 0.9659258262890683122, 1.000000000000000000, 0.9659258262890683122, 1.000000000000000000, 0.9659258262890683122, 1.000000000000000000, 0.9659258262890683122, 1.000000000000000000, 0.9659258262890683122, 1.000000000000000000, 0.9659258262890683122, 1.000000000000000000, 0.9659258262890683122, 1.000000000000000000, 0.9659258262890683122, 1.000000000000000000, 0.9659258262890683122, 1.000000000000000000, 0.9659258262890683122, 1.000000000000000000, 0.9659258262890683122, 1.000000000000000000, 0.9659258262890683122, 1.000000000000000000, 0.9659258262890683122, 1.000000000000000000, 0.9659258262890683122, 1.000000000000000000, 0.9659258262890683122, 1.000000000000000000, 0.9659258262890683122, 1.000000000000000000, 0.9659258262890683122, 1.000000000000000000, 0.9659258262890683122, 1.000000000000000000, 0.9659258262890683122, 1.000000000000000000, 0.9659258262890683122, 1.000000000000000000, 0.9659258262890683122, 1.000000000000000000, 0.9659258262890683122, 1.000000000000000000, 0.9659258262890683122, 1.000000000000000000, 0.9659258262890683122, 1.000000000000000000, 0.9659258262890683122, 1.000000000000000000, 0.9659258262890683122, 1.000000000000000000, 0.9659258262890683122, 1.000000000000000000, 0.9659258262890683122, 1.000000000000000000, 0.9659258262890683122, 1.000000000000000000, 0.9659258262890683122, 1.000000000000000000, 0.9659258262890683122, 1.000000000000000000, 0.9659258262890683122, 1.000000000000000000, 0.9659258262890683122, 1.000000000000000000, 0.9659258262890683122, 1.000000000000000000, 0.9659258262890683122, 1.000000000000000000, 0.9659258262890683122, 1.000000000000000000, 0.9659258262890683122, 1.000000000000000000, 0.9659258262890683122, 1.000000000000000000, 0.9659258262890683122, 1.000000000000000000, 0.9659258262890683122, 1.000000000000000000, 0.9659258262890683122, 1.000000000000000000, 0.9659258262890683122, 1.000000000000000000, 0.9659258262890683122, 1.000000000000000000, 0.9659258262890683122, 1.000000000000000000, 0.9659258262890683122, 1.000000000000000000, 0.9659258262890683122, 1.000000000000000000, 0.9659258262890683122, 1.000000000000000000, 0.9659258262890683122, 1.000000000000000000, 0.9659258262890683122, 1.000000000000000000, 0.9659258262890683122, 1.000000000000000000, 0.9659258262890683122, 1.000000000000000000, 0.9659258262890683122, 1.000000000000000000, 0.9659258262890683122, 1.000000000000000000, 0.9659258262890683122, 1.000000000000000000, 0.9659258262890683122, 1.000000000000000000, 0.9659258262890683122, 1.000000000000000000, 0.9659258262890683122, 1.000000000000000000, 0.9659258262890683122, 1.000000000000000000, 0.9659258262890683122, 1.000000000000000000, 0.9659258262890683122, 1.000000000000000000, 0.9659258262890683122, 1.000000000000000000, 0.9659258262890683122, 1.000000000000000000, 0.9659258262890683122, 1.000000000000000000, 0.9659258262890683122, 1.000000000000000000, 0.9659258262890683122, 1.000000000000000000, 0.9659258262890683122, 1.000000000000000000, 0.9659258262890683122, 1.000000000000000000, 0.9659258262890683122, 1.000000000000000000, 0.9659258262890683122, 1.000000000000000000, 0.9659258262890683122, 1.000000000000000000, 0.9659258262890683122, 1.000000000000000000, 0.9659258262890683122, 1.000000000000000000, 0.9659258262890683122, 1.000000000000000000, 0.9659258262890683122, 1.000000000000000000, 0.9659258262890683122, 1.000000000000000000, 0.9659258262890683122, 1.000000000000000000, 0.9659258262890683122, 1.000000000000000000, 0.9659258262890683122, 1.000000000000000000, 0.9659258262890683122, 1.000000000000000000, 0.9659258262890683122, 1.000000000000000000, 0.9659258262890683122, 1.000000000000000000, 0.9659258262890683122, 1.000000000000000000, 0.9659258262890683122, 1.000000000000000000, 0.9659258262890683122, 1.000000000000000000, 0.9659258262890683122, 1.000000000000000000, 0.9659258262890683122, 1.000000000000000000, 0.9659258262890683122, 1.000000000000000000, 0.9659258262890683122, 1.000000000000000000, 0.9659258262890683122, 1.000000000000000000, 0.9659258262890683122, 1.000000000000000000, 0.9659258262890683122, 1.000000000000000000, 0.9659258262890683122, 1.000000000000000000, 0.9659258262890683122, 1.000000000000000000, 0.9659258262890683122, 1.000000000000000000, 0.9659258262890683122, 1.000000000000000000, 0.9659258262890683122, 1.000000000000000000, 0.9659258262890683122, 1.000000000000000000, 0.9659258262890683122, 1.000000000000000000, 0.9659258262890683122, 1.000000000000000000, 0.9659258262890683122, 1.000000000000000000, 0.9659258262890683122, 1.000000000000000000, 0.9659258262890683122, 1.000000000000000000, 0.9659258262890683122, 1.000000000000000000, 0.9659258262890683122, 1.000000000000000000, 0.9659258262890683122, 1.000000000000000000, 0.9659258262890683122, 1.000000000000000000, 0.9659258262890683122, 1.000000000000000000, 0.9659258262890683122, 1.000000000000000000, 0.9659258262890683122, 1.000000000000000000, 0.9659258262890683122, 1.000000000000000000, 0.9659258262890683122, 1.000000000000000000, 0.9659258262890683122, 1.000000000000000000, 0.9659258262890683122, 1.000000000000000000, 0.9659258262890683122, 1.000000000000000000, 0.9659258262890683122, 1.000000000000000000, 0.9659258262890683122, 1.000000000000000000, 0.9659258262890683122, 1.000000000000000000, 0.9659258262890683122, 1.000000000000000000, 0.9659258262890683122, 1.000000000000000000, 0.9659258262890683122, 1.000000000000000000, 0.9659258262890683122, 1.000000000000000000, 0.9659258262890683122, 1.000000000000000000, 0.9659258262890683122, 1.000000000000000000, 0.9659258262890683122, 1.000000000000000000, 0.9659258262890683122, 1.000000000000000000, 0.9659258262890683122, 1.000000000000000000, 0.9659258262890683122, 1.000000000000000000, 0.9659258262890683122, 1.000000000000000000, 0.9659258262890683122, 1.000000000000000000, 0.9659258262890683122, 1.000000000000000000, 0.9659258262890683122, 1.000000000000000000, 0.9659258262890683122, 1.000000000000000000, 0.9659258262890683122, 1.000000000000000000, 0.9659258262890683122, 1.000000000000000000, 0.9659258262890683122, 1.000000000000000000, 0.9659258262890683122, 1.000000000000000000, 0.9659258262890683122, 1.000000000000000000, 0.9659258262890683122, 1.000000000000000000, 0.9659258262890683122, 1.000000000000000000, 0.9659258262890683122, 1.000000000000000000, 0.9659258262890683122, 1.000000000000000000, 0.9659258262890683122, 1.000000000000000000, 0.9659258262890683122, 1.000000000000000000, 0.9659258262890683122, 1.000000000000000000, 0.9659258262890683122, 1.000000000000000000, 0.9659258262890683122, 1.000000000000000000, 0.9659258262890683122, 1.000000000000000000, 0.9659258262890683122, 1.000000000000000000, 0.9659258262890683122, 1.000000000000000000, 0.9659258262890683122, 1.000000000000000000, 0.9659258262890683122, 1.000000000000000000, 0.9659258262890683122, 1.000000000000000000, 0.9659258262890683122, 1.000000000000000000, 0.9659258262890683122, 1.000000000000000000, 0.9659258262890683122, 1.000000000000000000, 0.9659258262890683122, 1.000000000000000000, 0.9659258262890683122, 1.000000000000000000, 0.9659258262890683122, 1.000000000000000000, 0.9659258262890683122, 1.000000000000000000, 0.9659258262890683122, 1.000000000000000000, 0.9659258262890683122, 1.000000000000000000, 0.9659258262890683122, 1.000000000000000000, 0.9659258262890683122, 1.000000000000000000, 0.9659258262890683122, 1.000000000000000000, 0.9659258262890683122, 1.000000000000000000, 0.9659258262890683122, 1.000000000000000000, 0.9659258262890683122, 1.000000000000000000, 0.9659258262890683122, 1.000000000000000000, 0.9659258262890683122, 1.000000000000000000, 0.9659258262890683122, 1.000000000000000000, 0.9659258262890683122, 1.000000000000000000, 0.9659258262890683122, 1.000000000000000000, 0.9659258262890683122, 1.000000000000000000, 0.9659258262890683122, 1.000000000000000000, 0.9659258262890683122, 1.000000000000000000, 0.9659258262890683122, 1.000000000000000000, 0.9659258262890683122, 1.000000000000000000, 0.9659258262890683122, 1.000000000000000000, 0.9659258262890683122, 1.000000000000000000, 0.9659258262890683122, 1.000000000000000000, 0.9659258262890683122, 1.000000000000000000, 0.9659258262890683122, 1.000000000000000000, 0.9659258262890683122, 1.000000000000000000, 0.9659258262890683122, 1.000000000000000000, 0.9659258262890683122, 1.000000000000000000, 0.9659258262890683122, 1.000000000000000000, 0.9659258262890683122, 1.000000000000000000, 0.9659258262890683122, 1.000000000000000000, 0.9659258262890683122, 1.000000000000000000, 0.9659258262890683122, 1.000000000000000000, 0.9659258262890683122, 1.000000000000000000, 0.9659258262890683122, 1.000000000000000000, 0.9659258262890683122, 1.000000000000000000, 0.9659258262890683122, 1.000000000000000000, 0.9659258262890683122, 1.000000000000000000, 0.9659258262890683122, 1.000000000000000000, 0.9659258262890683122, 1.000000000000000000, 0.9659258262890683122, 1.000000000000000000, 0.9659258262890683122, 1.000000000000000000, 0.9659258262890683122, 1.000000000000000000, 0.9659258262890683122, 1.000000000000000000, 0.9659258262890683122, 1.000000000000000000, 0.9659258262890683122, 1.000000000000000000, 0.9659258262890683122, 1.000000000000000000, 0.9659258262890683122, 1.000000000000000000, 0.9659258262890683122, 1.000000000000000000, 0.9659258262890683122, 1.000000000000000000) ) ) 
 REPRESENTATION_ITEM ( '' )  SURFACE ( )  );
#54180 = CARTESIAN_POINT ( 'NONE',  ( -0.6036745406824141069, 0.1283753931104748280, 0.1820866141732283561 ) ) ;
#54181 = CARTESIAN_POINT ( 'NONE',  ( -0.1070741851644057135, 0.3996062992125984925, -0.2408136482939632061 ) ) ;
#54182 = CARTESIAN_POINT ( 'NONE',  ( 0.3996062992125986035, 2.446882876249141962E-17, 0.03937007874015747283 ) ) ;
#54183 = CARTESIAN_POINT ( 'NONE',  ( 0.1958661417322836718, -0.3392501089628017219, -2.923247662238532385 ) ) ;
#54184 = CARTESIAN_POINT ( 'NONE',  ( 0.03175677952934891773, -0.3980111619244106613, -1.112674926538824158E-15 ) ) ;
#54185 = CARTESIAN_POINT ( 'NONE',  ( 1.286089238845145033, 0.1283753931104748280, 0.1820866141732283561 ) ) ;
#54186 = CARTESIAN_POINT ( 'NONE',  ( 0.2017716535433070613, 0.2017716535433070613, 0.000000000000000000 ) ) ;
#54187 = CARTESIAN_POINT ( 'NONE',  ( 0.8267716535433077274, 0.2952755905511811885, 0.000000000000000000 ) ) ;
#54188 = CARTESIAN_POINT ( 'NONE',  ( 0.1958661417322836440, -0.3392501089628017219, -2.538713910761154491 ) ) ;
#54189 = CARTESIAN_POINT ( 'NONE',  ( 1.286089238845145033, -0.5023911411419708095, -0.1820866141732282451 ) ) ;
#54190 = CARTESIAN_POINT ( 'NONE',  ( 0.01968503937007957949, -0.5400638737290845981, -0.3530559997133363437 ) ) ;
#54191 = CARTESIAN_POINT ( 'NONE',  ( -0.4593175853018364174, -0.4281496062992127816, -0.4176697321401328100 ) ) ;
#54192 = CARTESIAN_POINT ( 'NONE',  ( 1.489501312335958172, -0.3162353388693405765, 0.4822834645669290543 ) ) ;
#54193 = CARTESIAN_POINT ( 'NONE',  ( 0.1265901696524990294, -0.4724409448818896462, -0.8727034120734907807 ) ) ;
#54194 = CARTESIAN_POINT ( 'NONE',  ( 0.2925321140481932369, -0.2925321140481931814, -1.988188976377952777 ) ) ;
#54195 = CARTESIAN_POINT ( 'NONE',  ( 0.1968503937007881344, 0.1771653543307087630, 0.000000000000000000 ) ) ;
#54196 = ORIENTED_EDGE ( 'NONE', *, *, #60977, .T. ) ;
#54197 = CARTESIAN_POINT ( 'NONE',  ( -0.3392501089628017219, -0.1958661417322836995, -0.2067122291676659340 ) ) ;
#54198 = EDGE_LOOP ( 'NONE', ( #33600, #12729, #69821, #78981 ) ) ;
#54199 = CARTESIAN_POINT ( 'NONE',  ( -0.5511811023622041894, -0.1870078740157480879, -0.4822834645669291653 ) ) ;
#54200 = CARTESIAN_POINT ( 'NONE',  ( 0.7283464566929140904, -0.5400638737290845981, -0.3530559997133363437 ) ) ;
#54201 = CARTESIAN_POINT ( 'NONE',  ( 0.02624671916010564918, -0.6046776061558809534, -0.2411417322834644161 ) ) ;
#54202 = CARTESIAN_POINT ( 'NONE',  ( -0.3083989501312330295, -0.2845877964562161244, -0.3641732283464567121 ) ) ;
#54203 = CARTESIAN_POINT ( 'NONE',  ( 0.8792650918635177559, 0.05413385826771666132, 0.4176697321401328100 ) ) ;
#54204 = CARTESIAN_POINT ( 'NONE',  ( -0.8267716535433065062, 0.2952755905511811885, 0.000000000000000000 ) ) ;
#54205 = ADVANCED_FACE ( 'NONE', ( #54613 ), #22638, .T. ) ;
#54206 = CARTESIAN_POINT ( 'NONE',  ( -0.2887139107611542133, 0.2306618581243848609, 0.2411417322834645549 ) ) ;
#54207 = CARTESIAN_POINT ( 'NONE',  ( -0.7020997375328076329, -0.3162353388693409650, -0.4822834645669289433 ) ) ;
#54208 = CARTESIAN_POINT ( 'NONE',  ( 1.010498687664042716, 0.05413385826771626580, -0.4176697321401330321 ) ) ;
#54209 = CARTESIAN_POINT ( 'NONE',  ( 0.8070866141732288002, 0.1660481256975885056, 0.3530559997133364547 ) ) ;
#54210 = B_SPLINE_CURVE_WITH_KNOTS ( 'NONE', 3,
 ( #81433, #16213, #43091, #61220 ),
 .UNSPECIFIED., .F., .F.,
 ( 4, 4 ),
 ( 3.593986969197074047E-07, 0.001287825409103121209 ),
 .UNSPECIFIED. ) ;
#54211 = CARTESIAN_POINT ( 'NONE',  ( 0.9186351706036752773, 0.2306618581243847221, -0.2411417322834647770 ) ) ;
#54212 = CARTESIAN_POINT ( 'NONE',  ( 0.2867679344610365999, -0.2867679344610365444, -0.7204724409448818312 ) ) ;
#54213 = CARTESIAN_POINT ( 'NONE',  ( 0.03280839895013198948, -0.5511811023622048555, -0.09757992244046775898 ) ) ;
#54214 = EDGE_LOOP ( 'NONE', ( #5671, #6197, #67699 ) ) ;
#54215 = CARTESIAN_POINT ( 'NONE',  ( -0.1058382717557497937, -0.3949938075777411628, -1.017060367454068359 ) ) ;
#54216 = ORIENTED_EDGE ( 'NONE', *, *, #45360, .T. ) ;
#54217 = CARTESIAN_POINT ( 'NONE',  ( -1.017060367454067249, -0.2845877964562161244, -0.3641732283464567121 ) ) ;
#54218 = CARTESIAN_POINT ( 'NONE',  ( -0.5052493438320203589, 0.2952755905511810774, -0.1292274648535930714 ) ) ;
#54219 = CARTESIAN_POINT ( 'NONE',  ( 2.704643427489220375, 1.253539720428394677, 0.3811758253793009477 ) ) ;
#54220 = CARTESIAN_POINT ( 'NONE',  ( -0.4658792650918627265, -0.05778040916215522460, 0.4822834645669289988 ) ) ;
#54221 = CARTESIAN_POINT ( 'NONE',  ( -0.5052493438320203589, -0.6692913385826771977, 0.1292274648535927661 ) ) ;
#54222 = CARTESIAN_POINT ( 'NONE',  ( -1.167979002624671470, 0.05413385826771666132, 0.4176697321401328100 ) ) ;
#54223 = CARTESIAN_POINT ( 'NONE',  ( -1.437007874015747477, -0.5400638737290844871, 0.3530559997133364547 ) ) ;
#54224 = CARTESIAN_POINT ( 'NONE',  ( 1.141732283464567788, -0.5511811023622047445, 6.969142054262312111E-17 ) ) ;
#54225 = CARTESIAN_POINT ( 'NONE',  ( 0.1265901696524989184, 0.4724409448818898127, -0.3851706036745407014 ) ) ;
#54226 = CARTESIAN_POINT ( 'NONE',  ( 0.2797625792873952855, 0.09458053269141719621, 5.851882566737993230 ) ) ;
#54227 = CARTESIAN_POINT ( 'NONE',  ( 0.5118110236220478892, 0.1771653543307087630, 0.000000000000000000 ) ) ;
#54228 = AXIS2_PLACEMENT_3D ( 'NONE', #39903, #76952, #51666 ) ;
#54229 = CARTESIAN_POINT ( 'NONE',  ( -0.1246719160104980823, -0.6692913385826773087, -0.1292274648535924053 ) ) ;
#54230 = CARTESIAN_POINT ( 'NONE',  ( 0.3215223097112867578, -0.3162353388693409650, -0.4822834645669289433 ) ) ;
#54231 = EDGE_LOOP ( 'NONE', ( #16634, #63536, #47900, #42600 ) ) ;
#54232 = CARTESIAN_POINT ( 'NONE',  ( -0.1998031496062991907, -0.3460692066303959757, -1.797900262467191590 ) ) ;
#54233 = DIRECTION ( 'NONE',  ( -1.000000000000000000, -0.000000000000000000, -0.000000000000000000 ) ) ;
#54234 = ORIENTED_EDGE ( 'NONE', *, *, #14670, .F. ) ;
#54235 = CARTESIAN_POINT ( 'NONE',  ( 0.3460692066303959202, -0.1998031496062991630, -1.126640419947506633 ) ) ;
#54236 = CARTESIAN_POINT ( 'NONE',  ( 0.3996062992125986035, -0.1070741851644052972, -0.5032808398950130435 ) ) ;
#54237 = CARTESIAN_POINT ( 'NONE',  ( -0.5183727034120726440, -0.5511811023622048555, -0.09757992244046775898 ) ) ;
#54238 = CARTESIAN_POINT ( 'NONE',  ( -0.6430446194225716283, -0.4281496062992124485, 0.4176697321401328655 ) ) ;
#54239 = CARTESIAN_POINT ( 'NONE',  ( -0.1265901696524993347, 0.4724409448818895907, -0.006561679790026246628 ) ) ;
#54240 = CARTESIAN_POINT ( 'NONE',  ( 0.1049643490035303689, 0.3917322834645670104, -2.440288713910760521 ) ) ;
#54241 = CARTESIAN_POINT ( 'NONE',  ( -1.535433070866141225, -0.5511811023622047445, 6.969142054262312111E-17 ) ) ;
#54242 = CARTESIAN_POINT ( 'NONE',  ( 0.8464566929133865436, 0.1660481256975883668, -0.3530559997133364547 ) ) ;
#54243 = CARTESIAN_POINT ( 'NONE',  ( 1.017060367454068803, -0.3162353388693405765, 0.4822834645669290543 ) ) ;
#54244 = CARTESIAN_POINT ( 'NONE',  ( -0.4724409448818890911, -0.1870078740157480601, -0.3641732283464567677 ) ) ;
#54245 = CARTESIAN_POINT ( 'NONE',  ( 0.2559055118110243332, -0.5400638737290845981, -0.3530559997133363437 ) ) ;
#54246 = CARTESIAN_POINT ( 'NONE',  ( 0.4724409448818898682, 2.892866454678787531E-17, -1.769685039370078927 ) ) ;
#54247 = CARTESIAN_POINT ( 'NONE',  ( 0.03937007874015833325, -0.5511811023622047445, 6.969142054262312111E-17 ) ) ;
#54248 = CARTESIAN_POINT ( 'NONE',  ( -0.6561679790026240244, -0.6046776061558807314, 0.2411417322834647770 ) ) ;
#54249 = AXIS2_PLACEMENT_3D ( 'NONE', #51718, #25636, #32796 ) ;
#54250 = CARTESIAN_POINT ( 'NONE',  ( -0.3420746716998660508, -0.1974969037888706924, -1.861548556430446588 ) ) ;
#54251 = CARTESIAN_POINT ( 'NONE',  ( -1.581364829396324945, -0.3162353388693405765, 0.4822834645669290543 ) ) ;
#54252 = CARTESIAN_POINT ( 'NONE',  ( -0.07874015748031421014, -0.1870078740157480601, -0.3641732283464567677 ) ) ;
#54253 = CARTESIAN_POINT ( 'NONE',  ( 1.587926509186352586, -0.3690944881889765550, -0.3153832671262227771 ) ) ;
#54254 = CARTESIAN_POINT ( 'NONE',  ( -0.9973753280839886548, -0.6046776061558809534, -0.2411417322834644161 ) ) ;
#54255 = CARTESIAN_POINT ( 'NONE',  ( -0.8464566929133852113, 0.07958543189024085140, 0.2665933059059887866 ) ) ;
#54256 = CARTESIAN_POINT ( 'NONE',  ( -3.937007874015748143, 1.537401574803149984, -0.4744094488188975722 ) ) ;
#54257 = CARTESIAN_POINT ( 'NONE',  ( -1.069553805774277722, 0.2952755905511811885, 0.1292274648535926551 ) ) ;
#54258 = CARTESIAN_POINT ( 'NONE',  ( -0.2165354330708654795, 0.1660481256975885056, 0.3530559997133364547 ) ) ;
#54259 = CARTESIAN_POINT ( 'NONE',  ( -0.3996062992125984925, -0.1070741851644056858, -2.484908136482939955 ) ) ;
#54260 = CARTESIAN_POINT ( 'NONE',  ( 0.3917322834645668994, 0.1049643490035304522, -2.566909818076428706 ) ) ;
#54261 = CARTESIAN_POINT ( 'NONE',  ( -1.947751274789666587, 1.170105060311635192, -0.3006284332565725692 ) ) ;
#54262 = CARTESIAN_POINT ( 'NONE',  ( 0.2362204724409456558, -0.1870078740157479769, 0.3641732283464567677 ) ) ;
#54263 = CARTESIAN_POINT ( 'NONE',  ( 0.9973753280839902091, 0.2306618581243847221, -0.2411417322834647770 ) ) ;
#54264 = CARTESIAN_POINT ( 'NONE',  ( -1.286089238845143479, -0.5023911411419708095, 0.1820866141732285504 ) ) ;
#54265 = EDGE_CURVE ( 'NONE', #29875, #6933, #10045, .T. ) ;
#54266 = CARTESIAN_POINT ( 'NONE',  ( 1.325459317585302665, -0.4281496062992124485, 0.4176697321401328655 ) ) ;
#54267 = CARTESIAN_POINT ( 'NONE',  ( -1.522309711286088607, 0.1283753931104746893, -0.1820866141732285504 ) ) ;
#54268 = CARTESIAN_POINT ( 'NONE',  ( -0.5380577427821514602, -0.4281496062992127816, -0.4176697321401328100 ) ) ;
#54269 = CARTESIAN_POINT ( 'NONE',  ( 0.2296587926509192634, -0.2845877964562159024, 0.3641732283464567677 ) ) ;
#54270 = CARTESIAN_POINT ( 'NONE',  ( 0.4091458600556404646, -0.2362204724409448231, -0.8923884514435694859 ) ) ;
#54271 = CARTESIAN_POINT ( 'NONE',  ( 0.4921259842519691285, 0.07958543189024085140, 0.2665933059059887866 ) ) ;
#54272 = ADVANCED_FACE ( 'NONE', ( #34026 ), #54179, .F. ) ;
#54273 = CARTESIAN_POINT ( 'NONE',  ( -0.006561679790025524116, -0.05778040916215560624, -0.4822834645669293319 ) ) ;
#54274 = CARTESIAN_POINT ( 'NONE',  ( 0.3996062992125985480, 2.446882876249141654E-17, -0.5098425196850393526 ) ) ;
#54275 = CARTESIAN_POINT ( 'NONE',  ( -1.227034120734907585, 0.2952755905511811885, 0.1292274648535926551 ) ) ;
#54276 = CARTESIAN_POINT ( 'NONE',  ( 0.3392501089628018884, -0.1958661417322834220, -1.921916010498687877 ) ) ;
#54277 = CARTESIAN_POINT ( 'NONE',  ( 1.036745406824147508, -0.3690944881889765550, -0.3153832671262227771 ) ) ;
#54278 = CARTESIAN_POINT ( 'NONE',  ( -0.05905511811023545637, 0.1660481256975885056, 0.3530559997133364547 ) ) ;
#54279 = CARTESIAN_POINT ( 'NONE',  ( -0.2427821522309703550, -0.3162353388693405765, 0.4822834645669290543 ) ) ;
#54280 = CARTESIAN_POINT ( 'NONE',  ( -0.5118110236220466680, 0.1771653543307087630, 0.000000000000000000 ) ) ;
#54281 = CARTESIAN_POINT ( 'NONE',  ( 0.9711286089238851948, 0.1539470093639523085, 0.1968503937007873850 ) ) ;
#54282 = CARTESIAN_POINT ( 'NONE',  ( -0.3740157480314953431, 0.07958543189024085140, 0.2665933059059887866 ) ) ;
#54283 = CARTESIAN_POINT ( 'NONE',  ( 0.3149606299212606708, -0.1870078740157480879, -0.4822834645669291653 ) ) ;
#54284 = CARTESIAN_POINT ( 'NONE',  ( -0.6364829396325453192, -0.2845877964562159024, 0.3641732283464567677 ) ) ;
#54285 = CARTESIAN_POINT ( 'NONE',  ( -0.1070741851644056997, 0.3996062992125984925, -1.028215223097112663 ) ) ;
#54286 = CARTESIAN_POINT ( 'NONE',  ( -1.174540682414697335, -0.05778040916215522460, 0.4822834645669289988 ) ) ;
#54287 = DIRECTION ( 'NONE',  ( -1.000000000000000000, -0.000000000000000000, -0.000000000000000000 ) ) ;
#54288 = EDGE_LOOP ( 'NONE', ( #30066, #44775 ) ) ;
#54289 = CIRCLE ( 'NONE', #3243, 0.2165354330708660069 ) ;
#54290 = CARTESIAN_POINT ( 'NONE',  ( -1.010498687664041384, -0.3690944881889765550, -0.3153832671262227771 ) ) ;
#54291 = CARTESIAN_POINT ( 'NONE',  ( -0.4068241469816267775, 0.05413385826771626580, -0.4176697321401330321 ) ) ;
#54292 = ADVANCED_FACE ( 'NONE', ( #80961 ), #62830, .F. ) ;
#54293 = CARTESIAN_POINT ( 'NONE',  ( -1.607611548556429737, -0.6692913385826771977, 0.1292274648535927661 ) ) ;
#54294 = CARTESIAN_POINT ( 'NONE',  ( -1.213910761154854745, -0.6692913385826771977, 0.1292274648535927661 ) ) ;
#54295 = CARTESIAN_POINT ( 'NONE',  ( -1.092353285368623750, -2.191421614605370878E-15, 0.4445507791589071167 ) ) ;
#54296 = CARTESIAN_POINT ( 'NONE',  ( 1.338582677165355062, -0.1870078740157479769, 0.4822834645669291653 ) ) ;
#54297 = CARTESIAN_POINT ( 'NONE',  ( 0.9251968503937015864, 0.1660481256975883668, -0.3530559997133364547 ) ) ;
#54298 = CARTESIAN_POINT ( 'NONE',  ( -0.3392501089628019995, 0.1958661417322832277, -2.695538057742782101 ) ) ;
#54299 = CARTESIAN_POINT ( 'NONE',  ( 0.2952755905511811885, -0.01202990275164721873, 5.879133660591332244 ) ) ;
#54300 = CARTESIAN_POINT ( 'NONE',  ( 1.423884514435696191, -0.08942795157527998196, 0.3641732283464567121 ) ) ;
#54301 = CARTESIAN_POINT ( 'NONE',  ( -0.1070741851644051862, -0.3996062992125987146, -0.3871391076115485719 ) ) ;
#54303 = ADVANCED_FACE ( 'NONE', ( #35500 ), #54683, .F. ) ;
#54302 = ORIENTED_EDGE ( 'NONE', *, *, #2422, .F. ) ;
#54304 = CARTESIAN_POINT ( 'NONE',  ( -0.3149606299212590610, -0.1870078740157480601, -0.3641732283464567677 ) ) ;
#54306 = CARTESIAN_POINT ( 'NONE',  ( -0.1049643490035302024, -0.3917322834645671215, -2.269028871391075786 ) ) ;
#54305 = AXIS2_PLACEMENT_3D ( 'NONE', #60212, #53879, #21909 ) ;
#54307 = ORIENTED_EDGE ( 'NONE', *, *, #27431, .T. ) ;
#54308 = CARTESIAN_POINT ( 'NONE',  ( 0.9186351706036751663, -0.6046776061558807314, 0.2411417322834647770 ) ) ;
#54309 = CARTESIAN_POINT ( 'NONE',  ( -0.5183727034120726440, -0.6692913385826773087, -0.1292274648535924053 ) ) ;
#54310 = CARTESIAN_POINT ( 'NONE',  ( -0.5774278215223089816, -0.6046776061558807314, 0.2411417322834647770 ) ) ;
#54311 = CARTESIAN_POINT ( 'NONE',  ( 1.574803149606299746, -0.1870078740157480879, -0.4822834645669291653 ) ) ;
#54312 = CARTESIAN_POINT ( 'NONE',  ( -1.332020997375327642, -0.08942795157527998196, 0.3641732283464567121 ) ) ;
#54313 = CARTESIAN_POINT ( 'NONE',  ( 0.3458507752293908943, -0.3458507752293908943, -2.064960629921259283 ) ) ;
#54314 = CARTESIAN_POINT ( 'NONE',  ( 0.4265091863517067594, 0.2952755905511811885, 0.1292274648535926551 ) ) ;
#54315 = CARTESIAN_POINT ( 'NONE',  ( -0.8398950131233585692, 0.2306618581243848609, 0.2411417322834645549 ) ) ;
#54316 = CARTESIAN_POINT ( 'NONE',  ( -0.2867679344610366554, 0.2867679344610365444, -1.517041051672229024 ) ) ;
#54317 = CARTESIAN_POINT ( 'NONE',  ( -1.437007874015747477, 0.1660481256975883668, -0.3530559997133364547 ) ) ;
#54318 = FACE_OUTER_BOUND ( 'NONE', #40431, .T. ) ;
#54319 =( BOUNDED_CURVE ( )  B_SPLINE_CURVE ( 3, ( #60475, #2826, #28487, #59224 ),
 .UNSPECIFIED., .F., .F. ) 
 B_SPLINE_CURVE_WITH_KNOTS ( ( 4, 4 ),
 ( 5.657991264764151040, 6.283185307179586232 ),
 .UNSPECIFIED. ) 
 CURVE ( )  GEOMETRIC_REPRESENTATION_ITEM ( )  RATIONAL_B_SPLINE_CURVE ( ( 1.000000000000000000, 0.9676920770090842172, 0.9676920770090842172, 1.000000000000000000 ) ) 
 REPRESENTATION_ITEM ( '' )  );
#54320 = EDGE_CURVE ( 'NONE', #59512, #21899, #21649, .T. ) ;
#54321 = CARTESIAN_POINT ( 'NONE',  ( 0.8989501312335964611, 0.2952755905511811885, 0.1292274648535926551 ) ) ;
#54322 = CARTESIAN_POINT ( 'NONE',  ( 1.115485564304462551, -0.3690944881889765550, -0.3153832671262227771 ) ) ;
#54323 = ORIENTED_EDGE ( 'NONE', *, *, #20226, .F. ) ;
#54324 = CARTESIAN_POINT ( 'NONE',  ( 0.1058382717557500713, -0.3949938075777409408, 0.07217847769028866434 ) ) ;
#54325 = CARTESIAN_POINT ( 'NONE',  ( -0.4986876640419939388, 0.2306618581243847221, -0.2411417322834647770 ) ) ;
#54326 = ORIENTED_EDGE ( 'NONE', *, *, #5433, .T. ) ;
#54327 = CARTESIAN_POINT ( 'NONE',  ( 0.2099737532808405305, 0.1283753931104746893, -0.1820866141732285504 ) ) ;
#54328 = CARTESIAN_POINT ( 'NONE',  ( -1.227034120734907585, 0.2952755905511811885, 0.1292274648535926551 ) ) ;
#54329 = CARTESIAN_POINT ( 'NONE',  ( 0.9908136482939640111, 0.2952755905511810774, -0.1292274648535930714 ) ) ;
#54330 = CARTESIAN_POINT ( 'NONE',  ( 0.6955380577427828781, 0.05413385826771626580, -0.4176697321401330321 ) ) ;
#54331 = CARTESIAN_POINT ( 'NONE',  ( 0.03937007874015806264, 0.2952755905511811885, 0.000000000000000000 ) ) ;
#54332 = CARTESIAN_POINT ( 'NONE',  ( 4.797336870675656522E-17, -0.3917322834645670659, -1.335321153052180243 ) ) ;
#54333 = CARTESIAN_POINT ( 'NONE',  ( -0.7742782152230962556, -0.4281496062992127816, -0.4176697321401328100 ) ) ;
#54334 = CARTESIAN_POINT ( 'NONE',  ( 0.1958661417322836440, -0.3392501089628017219, -2.381233595800524849 ) ) ;
#54335 = CARTESIAN_POINT ( 'NONE',  ( -1.450131233595799651, -0.6692913385826771977, 0.1292274648535927661 ) ) ;
#54336 = CARTESIAN_POINT ( 'NONE',  ( -0.6102362204724400829, -0.5400638737290845981, -0.3530559997133363437 ) ) ;
#54337 = CARTESIAN_POINT ( 'NONE',  ( -0.4790026246719152336, -0.08942795157528024563, -0.3641732283464568787 ) ) ;
#54338 = CARTESIAN_POINT ( 'NONE',  ( 1.423884514435696413, -0.3162353388693409650, -0.4822834645669289433 ) ) ;
#54339 = CARTESIAN_POINT ( 'NONE',  ( 1.640419947506562393, -0.4281496062992124485, 0.4176697321401328655 ) ) ;
#54340 = CARTESIAN_POINT ( 'NONE',  ( -0.7414698162729651543, 0.2952755905511810774, -0.1292274648535930714 ) ) ;
#54341 = CARTESIAN_POINT ( 'NONE',  ( -9.787531504996566615E-17, 0.3996062992125985480, 0.2381889763779527491 ) ) ;
#54342 = CARTESIAN_POINT ( 'NONE',  ( 0.7414698162729663755, -0.6692913385826773087, -0.1292274648535924053 ) ) ;
#54343 = CARTESIAN_POINT ( 'NONE',  ( -0.1070741851644051862, -0.3996062992125987146, -1.804461942257217677 ) ) ;
#54344 = CARTESIAN_POINT ( 'NONE',  ( 1.607611548556431069, 0.2952755905511811885, 0.1292274648535926551 ) ) ;
#54345 = CARTESIAN_POINT ( 'NONE',  ( -0.2034120734908128059, 0.2952755905511811885, 0.1292274648535926551 ) ) ;
#54346 = CARTESIAN_POINT ( 'NONE',  ( -1.108923884514435132, -0.08942795157528024563, -0.3641732283464568787 ) ) ;
#54347 = CARTESIAN_POINT ( 'NONE',  ( 0.9383202099737538715, -0.08942795157528024563, -0.3641732283464568787 ) ) ;
#54348 = CARTESIAN_POINT ( 'NONE',  ( -0.2362204724409447953, -0.4091458600556404646, -0.4573490813648293796 ) ) ;
#54349 = CARTESIAN_POINT ( 'NONE',  ( 1.200787401574803681, 0.07958543189024085140, 0.2665933059059887866 ) ) ;
#54350 = CARTESIAN_POINT ( 'NONE',  ( 0.9580052493438326877, 0.05413385826771666132, 0.4176697321401328100 ) ) ;
#54351 = CARTESIAN_POINT ( 'NONE',  ( 0.3949938075777408852, 0.1058382717557500435, -0.6738845144356955252 ) ) ;
#54352 = CARTESIAN_POINT ( 'NONE',  ( -0.2099737532808391705, -0.6046776061558809534, -0.2411417322834644161 ) ) ;
#54353 = LINE ( 'NONE', #29920, #32403 ) ;
#54354 = VECTOR ( 'NONE', #71757, 39.37007874015748143 ) ;
#54355 = CARTESIAN_POINT ( 'NONE',  ( 1.292650918635171564, 0.1771653543307087630, 0.09757992244046791164 ) ) ;
#54356 = CARTESIAN_POINT ( 'NONE',  ( -0.5577427821522301654, -0.05778040916215560624, -0.4822834645669293319 ) ) ;
#54357 = CARTESIAN_POINT ( 'NONE',  ( 0.3420746716998660508, -0.1974969037888704149, -0.3392388451443569819 ) ) ;
#54358 = CARTESIAN_POINT ( 'NONE',  ( 1.482939632545932307, -0.4281496062992124485, 0.4176697321401328655 ) ) ;
#54359 = CARTESIAN_POINT ( 'NONE',  ( 0.01312335958005323398, 0.05413385826771666132, 0.4176697321401328100 ) ) ;
#54360 = CARTESIAN_POINT ( 'NONE',  ( 0.4724409448818904789, -0.1870078740157480601, -0.3641732283464567677 ) ) ;
#54361 = CARTESIAN_POINT ( 'NONE',  ( -0.1687104285705298135, 1.093727987196848161, -1.109387722385912101 ) ) ;
#54362 = CARTESIAN_POINT ( 'NONE',  ( 0.2493438320209980519, -0.004921259842519576551, 0.3153832671262227771 ) ) ;
#54363 = CARTESIAN_POINT ( 'NONE',  ( -1.614173228346455824, 0.2952755905511811885, 0.000000000000000000 ) ) ;
#54364 = CARTESIAN_POINT ( 'NONE',  ( 0.3996062992125986035, -0.1070741851644052972, -1.448162729658792669 ) ) ;
#54365 = CARTESIAN_POINT ( 'NONE',  ( 0.7349081364829403995, 0.2306618581243848609, 0.2411417322834645549 ) ) ;
#54366 = CARTESIAN_POINT ( 'NONE',  ( -0.1958661417322834220, -0.3392501089628018884, -1.160104986876640210 ) ) ;
#54367 = LINE ( 'NONE', #68268, #62762 ) ;
#54368 = CARTESIAN_POINT ( 'NONE',  ( -0.3874523867751280548, 0.05870088567680999819, 1.458593243026437152E-17 ) ) ;
#54369 = CARTESIAN_POINT ( 'NONE',  ( 0.09842519685039434474, -0.4536011799217368745, -0.2665933059059886201 ) ) ;
#54370 = EDGE_CURVE ( 'NONE', #14171, #9936, #13271, .T. ) ;
#54371 = AXIS2_PLACEMENT_3D ( 'NONE', #35945, #81400, #4361 ) ;
#54372 = CARTESIAN_POINT ( 'NONE',  ( 0.2559055118110243332, 0.1660481256975885056, 0.3530559997133364547 ) ) ;
#54373 = CARTESIAN_POINT ( 'NONE',  ( 1.561679790026247350, -0.004921259842519870586, -0.3153832671262229437 ) ) ;
#54374 = CARTESIAN_POINT ( 'NONE',  ( -1.286089238845143479, -0.5023911411419708095, 0.1820866141732285504 ) ) ;
#54375 = CARTESIAN_POINT ( 'NONE',  ( -1.528871391076114250, 0.2952755905511810774, -0.1292274648535930714 ) ) ;
#54376 = CARTESIAN_POINT ( 'NONE',  ( 0.3608923884514443348, -0.6692913385826771977, 0.1292274648535927661 ) ) ;
#54377 = CARTESIAN_POINT ( 'NONE',  ( 1.305774278215223960, -0.6692913385826771977, 0.1292274648535927661 ) ) ;
#54378 = CARTESIAN_POINT ( 'NONE',  ( 1.603475055217291612, 0.7793870273546369409, -0.04573490813648244807 ) ) ;
#54379 = CARTESIAN_POINT ( 'NONE',  ( 0.6430446194225728496, 0.05413385826771666132, 0.4176697321401328100 ) ) ;
#54380 = CARTESIAN_POINT ( 'NONE',  ( 1.292650918635171564, -0.6692913385826773087, -0.1292274648535924053 ) ) ;
#54381 = CARTESIAN_POINT ( 'NONE',  ( 0.7677165354330716118, 0.1660481256975883668, -0.3530559997133364547 ) ) ;
#54382 = CARTESIAN_POINT ( 'NONE',  ( 0.1265901696524990572, -0.4724409448818897017, -0.3195538057742782212 ) ) ;
#54383 = CARTESIAN_POINT ( 'NONE',  ( 0.6233595800524942554, -0.08942795157528024563, -0.3641732283464568787 ) ) ;
#54384 = CARTESIAN_POINT ( 'NONE',  ( 1.653543307086614789, -0.1870078740157479769, 0.4822834645669291653 ) ) ;
#54385 = CARTESIAN_POINT ( 'NONE',  ( -0.9776902887139098386, 0.1771653543307087075, -0.09757992244046823083 ) ) ;
#54386 = CARTESIAN_POINT ( 'NONE',  ( 0.5380577427821529035, -0.004921259842519870586, -0.3153832671262229437 ) ) ;
#54387 = CARTESIAN_POINT ( 'NONE',  ( 0.1312335958005257930, 0.2306618581243847221, -0.2411417322834647770 ) ) ;
#54388 = CARTESIAN_POINT ( 'NONE',  ( 0.7349081364829402885, -0.6046776061558809534, -0.2411417322834644161 ) ) ;
#54389 = CARTESIAN_POINT ( 'NONE',  ( -0.3543307086614165824, 0.2952755905511811885, 0.000000000000000000 ) ) ;
#54390 = CARTESIAN_POINT ( 'NONE',  ( 0.1902887139107617975, 0.1771653543307087630, 0.09757992244046791164 ) ) ;
#54391 = CARTESIAN_POINT ( 'NONE',  ( 0.8530183727034126306, 0.05413385826771626580, -0.4176697321401330321 ) ) ;
#54392 = CARTESIAN_POINT ( 'NONE',  ( -1.614140194556460184, 1.133714490967797417, 0.2492166689920113365 ) ) ;
#54393 = CARTESIAN_POINT ( 'NONE',  ( -0.8858267716535425107, 0.1660481256975883668, -0.3530559997133364547 ) ) ;
#54395 = CARTESIAN_POINT ( 'NONE',  ( 0.3996062992125986035, -0.1070741851644053111, -0.5839895013123358458 ) ) ;
#54394 = FACE_OUTER_BOUND ( 'NONE', #72044, .T. ) ;
#54396 = CARTESIAN_POINT ( 'NONE',  ( -0.8267716535433065062, 0.2952755905511811885, 0.000000000000000000 ) ) ;
#54397 = CARTESIAN_POINT ( 'NONE',  ( -0.3477690288713905509, -0.6692913385826771977, 0.1292274648535927661 ) ) ;
#54398 = B_SPLINE_CURVE_WITH_KNOTS ( 'NONE', 3,
 ( #46056, #14103, #27541, #7783, #34280, #19559, #45218, #2297, #33451, #70919, #59111, #7354, #40588, #1468, #20819, #53198, #78911, #21232, #66270, #8609, #59941, #51528, #13268, #38918, #64599, #6934, #54872, #73838, #22060, #53616, #10689, #29206, #16593, #34700, #28371, #10273, #16178, #74250, #80578, #60363, #54032, #9852, #17012, #42238, #41825, #80985, #55275, #35941, #79744, #61610 ),
 .UNSPECIFIED., .F., .F.,
 ( 4, 2, 2, 2, 2, 2, 2, 2, 2, 2, 2, 2, 2, 2, 2, 2, 2, 2, 2, 2, 2, 2, 2, 2, 4 ),
 ( 0.004882041752397744960, 0.007267356590370914471, 0.008460014009357500961, 0.009652671428344087451, 0.01084532884733067221, 0.01203798626631725870, 0.01442330110429044902, 0.01561595852327704072, 0.01680861594226363415, 0.01919393078023681060, 0.02038658819922340576, 0.02157924561820999398, 0.02277190303719658568, 0.02396456045618317390, 0.02634987529415635729, 0.02754253271314294899, 0.02873519013212954415, 0.03112050497010273101, 0.03350581980807591786, 0.03469847722706250609, 0.03589113464604909431, 0.03827644948402229158, 0.03946910690300887981, 0.04066176432199546803, 0.04304707915996866530 ),
 .UNSPECIFIED. ) ;
#54399 = CARTESIAN_POINT ( 'NONE',  ( 0.1265901696524989462, 0.4724409448818897572, 0.006561679790026246628 ) ) ;
#54400 = CARTESIAN_POINT ( 'NONE',  ( 4.837279021331060870E-17, -0.3949938075777409963, -2.283464566929133799 ) ) ;
#54401 = EDGE_LOOP ( 'NONE', ( #35718, #80203, #69834, #5750 ) ) ;
#54402 = CARTESIAN_POINT ( 'NONE',  ( 0.9448818897637802916, -0.1870078740157480601, -0.3641732283464567677 ) ) ;
#54403 = CARTESIAN_POINT ( 'NONE',  ( -0.3392501089628017219, -0.1958661417322836718, -0.8320209973753279753 ) ) ;
#54404 = CARTESIAN_POINT ( 'NONE',  ( 1.010498687664042716, 0.05413385826771626580, -0.4176697321401330321 ) ) ;
#54405 = AXIS2_PLACEMENT_3D ( 'NONE', #82718, #51117, #12847 ) ;
#54406 = CARTESIAN_POINT ( 'NONE',  ( 3.937007874015748143, 2.755905511811024056, 0.5314960629921260393 ) ) ;
#54407 = CARTESIAN_POINT ( 'NONE',  ( -1.299212598425196097, -0.5511811023622047445, 6.969142054262312111E-17 ) ) ;
#54408 = CARTESIAN_POINT ( 'NONE',  ( 1.496062992125985147, -0.1870078740157479769, 0.4822834645669291653 ) ) ;
#54409 = CARTESIAN_POINT ( 'NONE',  ( -1.384514435695537005, 0.2952755905511811885, 0.1292274648535926551 ) ) ;
#54410 = CARTESIAN_POINT ( 'NONE',  ( 0.4199475065616805614, 0.2306618581243848609, 0.2411417322834645549 ) ) ;
#54411 = CARTESIAN_POINT ( 'NONE',  ( 0.3917322834645668994, -0.1049643490035303134, -0.1915817340869272467 ) ) ;
#54412 = CARTESIAN_POINT ( 'NONE',  ( 0.2034120734908144990, -0.6692913385826771977, 0.1292274648535927661 ) ) ;
#54413 = CARTESIAN_POINT ( 'NONE',  ( -0.8661417322834640276, -0.1870078740157480601, -0.3641732283464567677 ) ) ;
#54414 = CARTESIAN_POINT ( 'NONE',  ( 0.8989501312335963501, -0.6692913385826773087, -0.1292274648535924053 ) ) ;
#54415 = CARTESIAN_POINT ( 'NONE',  ( 0.1115485564304467270, -0.6692913385826773087, -0.1292274648535924053 ) ) ;
#54416 = CARTESIAN_POINT ( 'NONE',  ( 0.4359958488159310086, 1.724409448818897461, 3.912791665790203766 ) ) ;
#54417 = CARTESIAN_POINT ( 'NONE',  ( -0.01193304242178637453, 5.354677644401852583E-19, -0.3627985898453510716 ) ) ;
#54418 = CARTESIAN_POINT ( 'NONE',  ( -0.3392501089628019995, 0.1958661417322831999, -1.440308029692600522 ) ) ;
#54419 = CARTESIAN_POINT ( 'NONE',  ( 0.6758530183727039509, -0.6692913385826771977, 0.1292274648535927661 ) ) ;
#54420 = CARTESIAN_POINT ( 'NONE',  ( 0.1181102362204730916, -0.6692913385826771977, 8.415575281601705876E-17 ) ) ;
#54421 = CARTESIAN_POINT ( 'NONE',  ( -1.122047244094487306, 0.1660481256975883668, -0.3530559997133364547 ) ) ;
#54423 = CARTESIAN_POINT ( 'NONE',  ( 1.082677165354331228, -0.5400638737290844871, 0.3530559997133364547 ) ) ;
#54422 = VECTOR ( 'NONE', #62941, 39.37007874015748143 ) ;
#54424 = CARTESIAN_POINT ( 'NONE',  ( 0.3412073490813655186, -0.6046776061558809534, -0.2411417322834644161 ) ) ;
#54425 = CARTESIAN_POINT ( 'NONE',  ( 0.2867679344610365999, 0.2867679344610365999, -1.167322834645669438 ) ) ;
#54426 = CARTESIAN_POINT ( 'NONE',  ( -0.1837270341207343505, -0.6046776061558807314, 0.2411417322834647770 ) ) ;
#54427 = CARTESIAN_POINT ( 'NONE',  ( 0.7152230971128616943, -0.05778040916215522460, 0.4822834645669289988 ) ) ;
#54428 = CARTESIAN_POINT ( 'NONE',  ( 0.1246719160104994284, 0.2952755905511810774, -0.1292274648535930714 ) ) ;
#54429 = CARTESIAN_POINT ( 'NONE',  ( 0.8727034120734913358, -0.08942795157527998196, 0.3641732283464567121 ) ) ;
#54430 = CARTESIAN_POINT ( 'NONE',  ( -1.292650918635170010, -0.6692913385826771977, 0.1292274648535927661 ) ) ;
#54431 = LINE ( 'NONE', #9830, #7256 ) ;
#54432 = CARTESIAN_POINT ( 'NONE',  ( 0.2362204724409456558, -0.1870078740157480879, -0.4822834645669291653 ) ) ;
#54433 = LENGTH_MEASURE_WITH_UNIT ( LENGTH_MEASURE( 0.02539999999999999897 ), #3106 );
#54434 = CARTESIAN_POINT ( 'NONE',  ( 0.1049643490035304938, -0.3917322834645669549, -2.439632545931758045 ) ) ;
#54435 = ORIENTED_EDGE ( 'NONE', *, *, #33602, .T. ) ;
#54436 = VERTEX_POINT ( 'NONE', #52370 ) ;
#54437 = CARTESIAN_POINT ( 'NONE',  ( 0.9186351706036752773, 0.2306618581243847221, -0.2411417322834647770 ) ) ;
#54438 = CARTESIAN_POINT ( 'NONE',  ( 0.6299212598425204535, -0.1870078740157479769, 0.3641732283464567677 ) ) ;
#54439 = B_SPLINE_CURVE_WITH_KNOTS ( 'NONE', 3,
 ( #79595, #2144, #52637, #20673 ),
 .UNSPECIFIED., .F., .F.,
 ( 4, 4 ),
 ( 3.210432057756949332E-07, 0.001287787053612054989 ),
 .UNSPECIFIED. ) ;
#54441 = CARTESIAN_POINT ( 'NONE',  ( 0.6199123404867349363, 8.471767977567108961E-16, -0.4445507791589058955 ) ) ;
#54440 = CARTESIAN_POINT ( 'NONE',  ( -1.313877454013331780, 0.2755905511811023723, 0.7983292792091805090 ) ) ;
#54442 = DIRECTION ( 'NONE',  ( 0.000000000000000000, 0.000000000000000000, -1.000000000000000000 ) ) ;
#54443 = CARTESIAN_POINT ( 'NONE',  ( -0.4724409448818898682, 5.785732909357575061E-17, -2.755905511811024056 ) ) ;
#54444 = CARTESIAN_POINT ( 'NONE',  ( -0.1049643490035302024, -0.3917322834645671215, -1.259186351706037099 ) ) ;
#54445 = CARTESIAN_POINT ( 'NONE',  ( -0.1070741851644056997, 0.3996062992125984925, -2.288057742782152015 ) ) ;
#54446 = CARTESIAN_POINT ( 'NONE',  ( -0.8530183727034112984, 0.05413385826771666132, 0.4176697321401328100 ) ) ;
#54447 = CARTESIAN_POINT ( 'NONE',  ( -0.6627296587926503335, -0.6692913385826771977, 0.1292274648535927661 ) ) ;
#54448 = CARTESIAN_POINT ( 'NONE',  ( 0.8136482939632553313, 0.2306618581243848609, 0.2411417322834645549 ) ) ;
#54449 = ORIENTED_EDGE ( 'NONE', *, *, #31652, .T. ) ;
#54450 = CARTESIAN_POINT ( 'NONE',  ( 1.338582677165355062, -0.1870078740157480879, -0.4822834645669291653 ) ) ;
#54451 = CARTESIAN_POINT ( 'NONE',  ( 1.673228346456693494, 0.07958543189024085140, 0.2665933059059887866 ) ) ;
#54452 = APPLICATION_PROTOCOL_DEFINITION ( 'draft international standard', 'automotive_design', 1998, #9492 ) ;
#54453 = DIRECTION ( 'NONE',  ( 0.000000000000000000, 0.000000000000000000, -1.000000000000000000 ) ) ;
#54454 = CARTESIAN_POINT ( 'NONE',  ( 0.2925321140481931814, 0.2925321140481931814, -2.104330708661417582 ) ) ;
#54455 = CARTESIAN_POINT ( 'NONE',  ( -1.213910761154854745, -0.5511811023622046335, 0.09757992244046803654 ) ) ;
#54456 = CARTESIAN_POINT ( 'NONE',  ( -0.1049643490035302024, -0.3917322834645671215, 0.09317585301837272294 ) ) ;
#54457 = CARTESIAN_POINT ( 'NONE',  ( 0.07874015748031558404, -0.1870078740157479769, 0.4822834645669291653 ) ) ;
#54459 = DIRECTION ( 'NONE',  ( -0.000000000000000000, -1.000000000000000000, -0.000000000000000000 ) ) ;
#54458 = CARTESIAN_POINT ( 'NONE',  ( 1.384514435695538559, 0.2952755905511810774, -0.1292274648535930714 ) ) ;
#54460 = CARTESIAN_POINT ( 'NONE',  ( -1.043307086614172707, 0.07958543189024071263, -0.2665933059059888421 ) ) ;
#54461 = CARTESIAN_POINT ( 'NONE',  ( 0.9383202099737538715, -0.05778040916215560624, -0.4822834645669293319 ) ) ;
#54462 = CARTESIAN_POINT ( 'NONE',  ( 1.161417322834646271, 0.07958543189024071263, -0.2665933059059888421 ) ) ;
#54463 = EDGE_CURVE ( 'NONE', #2914, #1754, #63281, .T. ) ;
#54464 = CARTESIAN_POINT ( 'NONE',  ( -0.1049643490035301746, -0.3917322834645670659, -1.254573860071179103 ) ) ;
#54465 = CARTESIAN_POINT ( 'NONE',  ( -1.351706036745406347, -0.004921259842519870586, -0.3153832671262229437 ) ) ;
#54466 = CARTESIAN_POINT ( 'NONE',  ( 1.338582677165355062, -0.1870078740157479769, 0.4822834645669291653 ) ) ;
#54467 = CARTESIAN_POINT ( 'NONE',  ( 0.2492559019816136257, 1.884140522857724376, 0.1894193705508290526 ) ) ;
#54468 = CARTESIAN_POINT ( 'NONE',  ( -0.07874015748031421014, -0.1870078740157480879, -0.4822834645669291653 ) ) ;
#54469 = CARTESIAN_POINT ( 'NONE',  ( -1.450131233595799651, 0.1771653543307087075, -0.09757992244046823083 ) ) ;
#54470 = CARTESIAN_POINT ( 'NONE',  ( -0.1837270341207343505, -0.5023911411419708095, 0.1820866141732285504 ) ) ;
#54471 = CARTESIAN_POINT ( 'NONE',  ( -0.6889763779527552368, -0.5400638737290845981, -0.3530559997133363437 ) ) ;
#54472 = CARTESIAN_POINT ( 'NONE',  ( -1.607611548556429737, 0.1771653543307087075, -0.09757992244046823083 ) ) ;
#54473 = CARTESIAN_POINT ( 'NONE',  ( 4.797336870675656522E-17, -0.3917322834645670659, -0.5479195782490308142 ) ) ;
#54474 = CARTESIAN_POINT ( 'NONE',  ( 0.2493438320209980519, -0.4281496062992127816, -0.4176697321401328100 ) ) ;
#54475 = CARTESIAN_POINT ( 'NONE',  ( 0.6889763779527560139, 1.446433227339393149E-17, -0.1181102362204724116 ) ) ;
#54476 = CARTESIAN_POINT ( 'NONE',  ( 0.1265901696524989462, 0.4724409448818897572, -1.802493438320209584 ) ) ;
#54477 = CIRCLE ( 'NONE', #47746, 0.2165354330708660069 ) ;
#54478 = CARTESIAN_POINT ( 'NONE',  ( -1.108923884514435132, -0.3162353388693405765, 0.4822834645669290543 ) ) ;
#54479 = CARTESIAN_POINT ( 'NONE',  ( -0.6036745406824141069, 0.1283753931104748280, 0.1820866141732283561 ) ) ;
#54480 = CARTESIAN_POINT ( 'NONE',  ( 1.220472440944882386, 1.277248692536265747E-15, -0.4445507791589058955 ) ) ;
#54481 = CARTESIAN_POINT ( 'NONE',  ( 0.06561679790026316017, -0.4281496062992124485, 0.4176697321401328655 ) ) ;
#54482 = CARTESIAN_POINT ( 'NONE',  ( 0.3412073490813655186, -0.5023911411419708095, -0.1820866141732282451 ) ) ;
#54483 = CARTESIAN_POINT ( 'NONE',  ( -0.8989501312335946848, 0.1771653543307087075, -0.09757992244046823083 ) ) ;
#54484 = CARTESIAN_POINT ( 'NONE',  ( -1.010498687664041384, -0.4281496062992127816, -0.4176697321401328100 ) ) ;
#54485 = CARTESIAN_POINT ( 'NONE',  ( -1.535433070866141225, 0.2952755905511811885, 0.000000000000000000 ) ) ;
#54486 = CARTESIAN_POINT ( 'NONE',  ( 1.581364829396326277, -0.3162353388693409650, -0.4822834645669289433 ) ) ;
#54487 = CARTESIAN_POINT ( 'NONE',  ( 0.3813326747118215287, 1.253753238304358808, 2.019942904136674322 ) ) ;
#54488 = CARTESIAN_POINT ( 'NONE',  ( 0.8792650918635177559, -0.004921259842519576551, 0.3153832671262227771 ) ) ;
#54489 = CARTESIAN_POINT ( 'NONE',  ( 0.9186351706036752773, 0.2306618581243847221, -0.2411417322834647770 ) ) ;
#54490 = CARTESIAN_POINT ( 'NONE',  ( 0.03178304480586199854, -0.3983403474834772418, -9.560572922657961637E-16 ) ) ;
#54491 = CARTESIAN_POINT ( 'NONE',  ( 1.515748031496063186, -0.4536011799217368745, -0.2665933059059886201 ) ) ;
#54492 = ORIENTED_EDGE ( 'NONE', *, *, #15723, .T. ) ;
#54493 = CARTESIAN_POINT ( 'NONE',  ( -0.9317585301837263412, -0.4281496062992127816, -0.4176697321401328100 ) ) ;
#54494 = CARTESIAN_POINT ( 'NONE',  ( -1.023622047244093558, -0.1870078740157479769, 0.4822834645669291653 ) ) ;
#54495 = CARTESIAN_POINT ( 'NONE',  ( 0.5183727034120741983, 0.2952755905511810774, -0.1292274648535930714 ) ) ;
#54496 = CARTESIAN_POINT ( 'NONE',  ( -1.489501312335957062, -0.2845877964562161244, -0.3641732283464567121 ) ) ;
#54497 = CARTESIAN_POINT ( 'NONE',  ( 0.3996062992125984925, 0.1070741851644054637, -2.406167979002624246 ) ) ;
#54498 = CARTESIAN_POINT ( 'NONE',  ( 1.430446194225722500, -0.004921259842519576551, 0.3153832671262227771 ) ) ;
#54499 = CARTESIAN_POINT ( 'NONE',  ( 0.2493438320209980519, 0.05413385826771666132, 0.4176697321401328100 ) ) ;
#54500 = CARTESIAN_POINT ( 'NONE',  ( 0.8202099737532813073, 0.2952755905511811885, 0.1292274648535926551 ) ) ;
#54501 = CARTESIAN_POINT ( 'NONE',  ( -0.3996062992125986035, -0.1070741851644056997, -1.935695538057742526 ) ) ;
#54502 = CARTESIAN_POINT ( 'NONE',  ( -0.1058382717557497937, -0.3949938075777411628, -1.174540682414698223 ) ) ;
#54503 = CARTESIAN_POINT ( 'NONE',  ( 0.3460692066303959757, -0.1998031496062991907, -2.624671916010498762 ) ) ;
#54504 = CARTESIAN_POINT ( 'NONE',  ( -1.586052503253848167, 1.023622047244095556, -0.1653254495020564929 ) ) ;
#54505 = CARTESIAN_POINT ( 'NONE',  ( 0.3392501089628018329, 0.1958661417322835607, -0.2808398950131232863 ) ) ;
#54506 = CARTESIAN_POINT ( 'NONE',  ( -0.2690288713910754526, 0.1771653543307087075, -0.09757992244046823083 ) ) ;
#54507 = CARTESIAN_POINT ( 'NONE',  ( -0.1902887139107604098, -0.6692913385826771977, 0.1292274648535927661 ) ) ;
#54508 = CARTESIAN_POINT ( 'NONE',  ( 0.7414698162729663755, -0.6692913385826773087, -0.1292274648535924053 ) ) ;
#54509 = CARTESIAN_POINT ( 'NONE',  ( 0.1058382717557499880, 0.3949938075777409408, -1.959973753280839670 ) ) ;
#54510 = CARTESIAN_POINT ( 'NONE',  ( -0.01968503937007793844, 0.07958543189024071263, -0.2665933059059888421 ) ) ;
#54511 = CARTESIAN_POINT ( 'NONE',  ( -1.351706036745406347, -0.4281496062992124485, 0.4176697321401328655 ) ) ;
#54512 = CARTESIAN_POINT ( 'NONE',  ( 1.377952755905512472, -0.6692913385826771977, 8.415575281601705876E-17 ) ) ;
#54513 = CARTESIAN_POINT ( 'NONE',  ( 0.4724409448818897572, -0.1265901696524988906, -2.631233595800525293 ) ) ;
#54514 = CARTESIAN_POINT ( 'NONE',  ( -0.2925321140481932924, 0.2925321140481931814, -1.909448818897637512 ) ) ;
#54515 = DIRECTION ( 'NONE',  ( 0.000000000000000000, 1.000000000000000000, 0.000000000000000000 ) ) ;
#54516 = ORIENTED_EDGE ( 'NONE', *, *, #11815, .F. ) ;
#54517 = EDGE_LOOP ( 'NONE', ( #29749, #15330, #66529, #50444 ) ) ;
#54518 = CARTESIAN_POINT ( 'NONE',  ( 1.181102362204724976, -0.1870078740157480879, -0.4822834645669291653 ) ) ;
#54519 = CARTESIAN_POINT ( 'NONE',  ( -1.614173228346456268, -0.6692913385826771977, 8.415575281601705876E-17 ) ) ;
#54521 = CARTESIAN_POINT ( 'NONE',  ( 1.496062992125984703, -0.1870078740157480879, -0.4822834645669291653 ) ) ;
#54520 = CARTESIAN_POINT ( 'NONE',  ( -1.233595800524933894, -0.5023911411419708095, -0.1820866141732282451 ) ) ;
#54522 = CARTESIAN_POINT ( 'NONE',  ( 0.3917322834645668994, -0.1049643490035303134, -2.711266773457006174 ) ) ;
#54523 = CARTESIAN_POINT ( 'NONE',  ( 1.191801538614238209, 4.598214627222820490E-16, 0.4118484887281966822 ) ) ;
#54524 = CARTESIAN_POINT ( 'NONE',  ( 1.253280839895013710, -0.05778040916215560624, -0.4822834645669293319 ) ) ;
#54525 = CARTESIAN_POINT ( 'NONE',  ( -1.509186351706035767, 0.05413385826771626580, -0.4176697321401330321 ) ) ;
#54526 = CARTESIAN_POINT ( 'NONE',  ( 0.07874015748031558404, -0.1870078740157480879, -0.4822834645669291653 ) ) ;
#54527 = CARTESIAN_POINT ( 'NONE',  ( -0.6758530183727028406, -0.6692913385826773087, -0.1292274648535924053 ) ) ;
#54528 = CARTESIAN_POINT ( 'NONE',  ( -1.581364829396324945, -0.05778040916215560624, -0.4822834645669293319 ) ) ;
#54529 = CARTESIAN_POINT ( 'NONE',  ( -0.3917322834645669549, -0.1049643490035306603, 0.02690288713910752097 ) ) ;
#54530 = CARTESIAN_POINT ( 'NONE',  ( 0.3477690288713918276, 0.2952755905511811885, 0.1292274648535926551 ) ) ;
#54531 = CARTESIAN_POINT ( 'NONE',  ( -0.1958661417322834220, -0.3392501089628018884, -2.104986876640420057 ) ) ;
#54532 = CARTESIAN_POINT ( 'NONE',  ( -1.450131233595799651, 0.1771653543307087075, -0.09757992244046823083 ) ) ;
#54533 = ORIENTED_EDGE ( 'NONE', *, *, #80068, .T. ) ;
#54534 = CARTESIAN_POINT ( 'NONE',  ( 0.3949938075777409963, 2.418639510665530435E-17, -2.480314960629921295 ) ) ;
#54535 = VERTEX_POINT ( 'NONE', #30029 ) ;
#54536 = CARTESIAN_POINT ( 'NONE',  ( -1.680497585818729434, 1.332856214479095414, 0.4284113646842339640 ) ) ;
#54537 = AXIS2_PLACEMENT_3D ( 'NONE', #54022, #22050, #46044 ) ;
#54538 = CARTESIAN_POINT ( 'NONE',  ( -1.607611548556429737, -0.6692913385826771977, 0.1292274648535927661 ) ) ;
#54539 = CARTESIAN_POINT ( 'NONE',  ( 4.893765752498283924E-17, -0.3996062992125986035, -0.8661417322834645827 ) ) ;
#54540 = DIRECTION ( 'NONE',  ( 0.000000000000000000, 0.000000000000000000, 1.000000000000000000 ) ) ;
#54541 = CARTESIAN_POINT ( 'NONE',  ( -1.594488188976377563, -0.5400638737290844871, 0.3530559997133364547 ) ) ;
#54542 = LINE ( 'NONE', #29706, #71873 ) ;
#54543 = CARTESIAN_POINT ( 'NONE',  ( 0.9348729704079946634, -8.644661201599092366E-16, -0.4445507791589066171 ) ) ;
#54544 = CARTESIAN_POINT ( 'NONE',  ( 0.3392501089628018884, -0.1958661417322834220, 0.1253280839895012100 ) ) ;
#54545 = CARTESIAN_POINT ( 'NONE',  ( -0.4855643044619415427, -0.004921259842519870586, -0.3153832671262229437 ) ) ;
#54546 = CARTESIAN_POINT ( 'NONE',  ( -0.8398950131233589023, -0.5023911411419708095, -0.1820866141732282451 ) ) ;
#54547 = CARTESIAN_POINT ( 'NONE',  ( -1.174540682414697335, -0.05778040916215522460, 0.4822834645669289988 ) ) ;
#54548 = CARTESIAN_POINT ( 'NONE',  ( 0.4396325459317590445, -0.6692913385826771977, 0.1292274648535927661 ) ) ;
#54549 = CARTESIAN_POINT ( 'NONE',  ( -1.437007874015747477, 0.1660481256975883668, -0.3530559997133364547 ) ) ;
#54550 = CARTESIAN_POINT ( 'NONE',  ( -0.3917322834645669549, -0.1049643490035306603, 0.1194225721784776956 ) ) ;
#54551 = EDGE_LOOP ( 'NONE', ( #35505, #52625, #11693, #75882, #3395, #79203, #66898, #20487, #68621, #25634, #37116, #70555, #35178, #61460, #65103, #61388, #14088, #4109, #10019, #99, #13340, #55537, #4306, #81760, #26177, #42520, #14808, #4870, #279, #42223 ) ) ;
#54552 = CARTESIAN_POINT ( 'NONE',  ( -1.220472440944881054, -0.6692913385826771977, 8.415575281601705876E-17 ) ) ;
#54553 = CARTESIAN_POINT ( 'NONE',  ( -1.614173228346457378, 1.606230626554505658, 0.1372047244094476981 ) ) ;
#54554 =( LENGTH_UNIT ( ) NAMED_UNIT ( * ) SI_UNIT ( $, .METRE. ) );
#54555 = CARTESIAN_POINT ( 'NONE',  ( -1.157146581871515012E-16, 0.4724409448818898682, -1.889763779527559251 ) ) ;
#54556 = CARTESIAN_POINT ( 'NONE',  ( -1.614173228346457378, 0.2753471884572478157, -0.1372047244094478091 ) ) ;
#54557 = EDGE_CURVE ( 'NONE', #24503, #17964, #67109, .T. ) ;
#54558 = CARTESIAN_POINT ( 'NONE',  ( 0.2867679344610365999, -0.2867679344610365444, -0.7204724409448818312 ) ) ;
#54559 = DIRECTION ( 'NONE',  ( 1.692413147294446216E-16, -0.000000000000000000, 1.000000000000000000 ) ) ;
#54560 = CARTESIAN_POINT ( 'NONE',  ( -0.7152230971128602510, -0.3162353388693405765, 0.4822834645669290543 ) ) ;
#54561 = CARTESIAN_POINT ( 'NONE',  ( 1.601049868766404982, -0.6046776061558809534, -0.2411417322834644161 ) ) ;
#54563 = DIRECTION ( 'NONE',  ( 0.000000000000000000, 0.000000000000000000, 1.000000000000000000 ) ) ;
#54562 = CARTESIAN_POINT ( 'NONE',  ( -1.509186351706035767, 0.05413385826771626580, -0.4176697321401330321 ) ) ;
#54564 = B_SPLINE_CURVE_WITH_KNOTS ( 'NONE', 3,
 ( #32971, #7733, #13216, #33400, #1417, #78443, #27907, #14472, #38862, #58639, #1007, #40126, #8145, #72942, #41767, #29148, #36288, #47253, #66635, #74193, #35884, #61130, #74611, #28319 ),
 .UNSPECIFIED., .F., .F.,
 ( 4, 2, 2, 2, 2, 2, 2, 2, 2, 2, 2, 4 ),
 ( 0.03819530504429712037, 0.04014388769883309172, 0.04209247035336907000, 0.04404105300790504135, 0.04598963566244101964, 0.04696392698970900531, 0.04793821831697699098, 0.04891250964424497666, 0.04988680097151296233, 0.05183538362604894062, 0.05280967495331692629, 0.05378396628058491891 ),
 .UNSPECIFIED. ) ;
#54565 = CARTESIAN_POINT ( 'NONE',  ( -1.404199475065615932, 0.05413385826771666132, 0.4176697321401328100 ) ) ;
#54566 = CARTESIAN_POINT ( 'NONE',  ( -0.9908136482939626788, -0.6692913385826773087, -0.1292274648535924053 ) ) ;
#54567 = CARTESIAN_POINT ( 'NONE',  ( -0.2867679344610366554, 0.2867679344610365444, 0.05776209793407005577 ) ) ;
#54568 = EDGE_CURVE ( 'NONE', #82716, #80251, #47643, .T. ) ;
#54569 = CARTESIAN_POINT ( 'NONE',  ( 0.6430446194225728496, -0.004921259842519576551, 0.3153832671262227771 ) ) ;
#54570 = CARTESIAN_POINT ( 'NONE',  ( 0.3392501089628018884, -0.1958661417322834220, -0.5045931758530184386 ) ) ;
#54571 = CARTESIAN_POINT ( 'NONE',  ( 0.06561679790026316017, -0.3690944881889763329, 0.3153832671262228327 ) ) ;
#54572 = CARTESIAN_POINT ( 'NONE',  ( 0.9317585301837276734, -0.3690944881889763329, 0.3153832671262228327 ) ) ;
#54573 = CARTESIAN_POINT ( 'NONE',  ( 1.010498687664042716, 0.05413385826771626580, -0.4176697321401330321 ) ) ;
#54574 = UNCERTAINTY_MEASURE_WITH_UNIT (LENGTH_MEASURE( 1.000000000000000082E-05 ), #29310, 'distance_accuracy_value', 'NONE');
#54575 = CARTESIAN_POINT ( 'NONE',  ( -0.2952755905511803003, -0.4536011799217368745, -0.2665933059059886201 ) ) ;
#54576 = CARTESIAN_POINT ( 'NONE',  ( 0.1958661417322836440, -0.3392501089628017219, -2.446194225721784576 ) ) ;
#54577 = CARTESIAN_POINT ( 'NONE',  ( -1.489501312335957062, -0.05778040916215522460, 0.4822834645669289988 ) ) ;
#54578 = CIRCLE ( 'NONE', #15680, 1.220472440944881942 ) ;
#54579 = CARTESIAN_POINT ( 'NONE',  ( -1.122047244094487306, 0.07958543189024071263, -0.2665933059059888421 ) ) ;
#54580 = CONICAL_SURFACE ( 'NONE', #825, 1.250000000000000000, 0.1221730476396033355 ) ;
#54581 = CARTESIAN_POINT ( 'NONE',  ( 0.1265901696524990294, -0.4724409448818896462, -0.1620734908136483021 ) ) ;
#54582 = CONICAL_SURFACE ( 'NONE', #23635, 1.220472440944881942, 0.7853981633974621568 ) ;
#54583 = CARTESIAN_POINT ( 'NONE',  ( -0.03937007874015669567, -0.6692913385826771977, 8.415575281601705876E-17 ) ) ;
#54584 = CARTESIAN_POINT ( 'NONE',  ( -0.07217847769028787330, -0.05778040916215522460, 0.4822834645669289988 ) ) ;
#54585 = CARTESIAN_POINT ( 'NONE',  ( 1.482939632545932307, -0.3690944881889763329, 0.3153832671262228327 ) ) ;
#54586 = CARTESIAN_POINT ( 'NONE',  ( 0.4593175853018379162, -0.3690944881889763329, 0.3153832671262228327 ) ) ;
#54587 = CARTESIAN_POINT ( 'NONE',  ( -0.1377952755905504645, 0.07958543189024085140, 0.2665933059059887866 ) ) ;
#54588 = CARTESIAN_POINT ( 'NONE',  ( -0.6955380577427815458, 0.05413385826771666132, 0.4176697321401328100 ) ) ;
#54589 = CARTESIAN_POINT ( 'NONE',  ( -3.861376881555339757, 2.746034003362845866, 0.5314960629921258173 ) ) ;
#54590 = CARTESIAN_POINT ( 'NONE',  ( 0.3458507752293908943, 0.3458507752293908943, -1.946850393700787274 ) ) ;
#54591 = CARTESIAN_POINT ( 'NONE',  ( 0.2230971128608932319, -0.4281496062992124485, 0.4176697321401328655 ) ) ;
#54592 = CARTESIAN_POINT ( 'NONE',  ( 0.3996062992125986035, -0.1070741851644052972, -1.763123359580051952 ) ) ;
#54593 = DIRECTION ( 'NONE',  ( 0.000000000000000000, 0.000000000000000000, 1.000000000000000000 ) ) ;
#54594 = CARTESIAN_POINT ( 'NONE',  ( -0.3674540682414692561, -0.5023911411419708095, -0.1820866141732282451 ) ) ;
#54595 = AXIS2_PLACEMENT_3D ( 'NONE', #50403, #31463, #49584 ) ;
#54596 = CARTESIAN_POINT ( 'NONE',  ( -0.1049868766404193215, 0.2306618581243847221, -0.2411417322834647770 ) ) ;
#54597 = CARTESIAN_POINT ( 'NONE',  ( -1.653543307086613234, -0.1870078740157479769, 0.4822834645669291653 ) ) ;
#54598 = CARTESIAN_POINT ( 'NONE',  ( -1.463254593175852492, 0.1771653543307087630, 0.09757992244046791164 ) ) ;
#54599 = CARTESIAN_POINT ( 'NONE',  ( 1.167979002624672580, -0.4281496062992124485, 0.4176697321401328655 ) ) ;
#54600 = DIRECTION ( 'NONE',  ( -0.000000000000000000, -1.000000000000000000, -0.000000000000000000 ) ) ;
#54601 = CARTESIAN_POINT ( 'NONE',  ( -0.4724409448818890911, -0.1870078740157479769, 0.3641732283464567677 ) ) ;
#54602 = CARTESIAN_POINT ( 'NONE',  ( 0.3996062992125985480, 2.446882876249141654E-17, -0.03740157480314963701 ) ) ;
#54603 = CARTESIAN_POINT ( 'NONE',  ( 0.2925321140481932369, -0.2925321140481932369, -0.5708661417322833387 ) ) ;
#54604 = CARTESIAN_POINT ( 'NONE',  ( 0.2867679344610366554, -0.2867679344610365999, -2.929809342028559360 ) ) ;
#54605 = CARTESIAN_POINT ( 'NONE',  ( 1.692913385826772421, 0.1771653543307087630, 0.000000000000000000 ) ) ;
#54606 = CARTESIAN_POINT ( 'NONE',  ( 1.089238845144357537, -0.3690944881889763329, 0.3153832671262228327 ) ) ;
#54607 = DIRECTION ( 'NONE',  ( 0.000000000000000000, 0.000000000000000000, 1.000000000000000000 ) ) ;
#54608 = CARTESIAN_POINT ( 'NONE',  ( 0.7283464566929140904, -0.5400638737290845981, -0.3530559997133363437 ) ) ;
#54609 = CARTESIAN_POINT ( 'NONE',  ( -0.3949938075777408852, -0.1058382717557502933, -1.067585301837270739 ) ) ;
#54610 = CARTESIAN_POINT ( 'NONE',  ( 1.056430446194226658, 0.1771653543307087630, 0.09757992244046791164 ) ) ;
#54611 = CARTESIAN_POINT ( 'NONE',  ( 0.2690288713910767848, 0.2952755905511811885, 0.1292274648535926551 ) ) ;
#54612 = CARTESIAN_POINT ( 'NONE',  ( -0.9645669291338575535, 0.1660481256975883668, -0.3530559997133364547 ) ) ;
#54613 = FACE_OUTER_BOUND ( 'NONE', #33964, .T. ) ;
#54614 = CARTESIAN_POINT ( 'NONE',  ( -1.157146581871515012E-16, 0.4724409448818898682, -1.102362204724409489 ) ) ;
#54615 = CARTESIAN_POINT ( 'NONE',  ( -0.3996062992125986590, 0.1070741851644051862, -2.237532808398950301 ) ) ;
#54616 = CARTESIAN_POINT ( 'NONE',  ( 0.3543307086614179147, 0.1771653543307087630, 0.000000000000000000 ) ) ;
#54617 = EDGE_LOOP ( 'NONE', ( #41991, #57930, #53985 ) ) ;
#54618 = CARTESIAN_POINT ( 'NONE',  ( -0.1049643490035302301, -0.3917322834645671770, -0.5413578984590045051 ) ) ;
#54619 = ORIENTED_EDGE ( 'NONE', *, *, #9980, .F. ) ;
#54620 = CARTESIAN_POINT ( 'NONE',  ( -0.6364829396325453192, -0.3162353388693405765, 0.4822834645669290543 ) ) ;
#54621 = CARTESIAN_POINT ( 'NONE',  ( -0.3543307086614165824, 0.2952755905511811885, 0.000000000000000000 ) ) ;
#54622 = CARTESIAN_POINT ( 'NONE',  ( -0.2559055118110227234, -0.4536011799217367080, 0.2665933059059888421 ) ) ;
#54623 = CARTESIAN_POINT ( 'NONE',  ( 0.6496062992125991586, -0.5400638737290845981, -0.3530559997133363437 ) ) ;
#54624 = CARTESIAN_POINT ( 'NONE',  ( -0.7349081364829387342, -0.6046776061558807314, 0.2411417322834647770 ) ) ;
#54625 = CARTESIAN_POINT ( 'NONE',  ( -0.2559055118110230564, 0.1660481256975883668, -0.3530559997133364547 ) ) ;
#54626 = CARTESIAN_POINT ( 'NONE',  ( 0.9842519685039375910, 0.2952755905511811885, 0.000000000000000000 ) ) ;
#54627 = CARTESIAN_POINT ( 'NONE',  ( 1.010498687664042716, 0.05413385826771626580, -0.4176697321401330321 ) ) ;
#54628 = CARTESIAN_POINT ( 'NONE',  ( 0.7874015748031503170, -0.1870078740157480879, -0.4822834645669291653 ) ) ;
#54629 = CARTESIAN_POINT ( 'NONE',  ( -0.2867679344610364334, -0.2867679344610367109, -0.9960629921259842590 ) ) ;
#54630 = CARTESIAN_POINT ( 'NONE',  ( -0.1640419947506553400, -0.08942795157528024563, -0.3641732283464568787 ) ) ;
#54631 = ORIENTED_EDGE ( 'NONE', *, *, #27901, .F. ) ;
#54632 = CARTESIAN_POINT ( 'NONE',  ( 0.1974969037888704704, 0.3420746716998660508, -1.089238845144357093 ) ) ;
#54633 = AXIS2_PLACEMENT_3D ( 'NONE', #67940, #54459, #80586 ) ;
#54634 = ORIENTED_EDGE ( 'NONE', *, *, #16141, .T. ) ;
#54635 = CARTESIAN_POINT ( 'NONE',  ( -0.8267716535433065062, -0.5511811023622047445, 6.969142054262312111E-17 ) ) ;
#54636 = AXIS2_PLACEMENT_3D ( 'NONE', #4906, #42369, #62567 ) ;
#54637 = VECTOR ( 'NONE', #66695, 39.37007874015748143 ) ;
#54638 = CARTESIAN_POINT ( 'NONE',  ( -0.6430446194225712953, 0.05413385826771626580, -0.4176697321401330321 ) ) ;
#54639 = CARTESIAN_POINT ( 'NONE',  ( 0.7754685323813633735, -1.606403293320555582E-18, -0.3627985898453514046 ) ) ;
#54640 = CARTESIAN_POINT ( 'NONE',  ( -0.3280839895013117347, -0.4281496062992124485, 0.4176697321401328655 ) ) ;
#54641 = CARTESIAN_POINT ( 'NONE',  ( -0.5708661417322828946, 0.1660481256975883668, -0.3530559997133364547 ) ) ;
#54642 = CARTESIAN_POINT ( 'NONE',  ( -1.108923884514435132, -0.05778040916215560624, -0.4822834645669293319 ) ) ;
#54643 = CARTESIAN_POINT ( 'NONE',  ( -1.253280839895012377, -0.05778040916215522460, 0.4822834645669289988 ) ) ;
#54644 = CARTESIAN_POINT ( 'NONE',  ( 0.8595800524934390507, -0.2845877964562159024, 0.3641732283464567677 ) ) ;
#54645 = CARTESIAN_POINT ( 'NONE',  ( 0.4724409448818898682, 2.892866454678787531E-17, -0.3523622047244094335 ) ) ;
#54646 = CARTESIAN_POINT ( 'NONE',  ( 0.2858256400101374384, 0.07430968296373897941, 5.862902060615214239 ) ) ;
#54647 = CARTESIAN_POINT ( 'NONE',  ( 0.3346456692913390985, 0.07958543189024085140, 0.2665933059059887866 ) ) ;
#54648 = CARTESIAN_POINT ( 'NONE',  ( -0.07874015748031421014, -0.1870078740157479769, 0.4822834645669291653 ) ) ;
#54649 = CARTESIAN_POINT ( 'NONE',  ( 0.4986876640419954376, -0.6046776061558809534, -0.2411417322834644161 ) ) ;
#54650 = VERTEX_POINT ( 'NONE', #74256 ) ;
#54651 = CARTESIAN_POINT ( 'NONE',  ( -0.1070741851644056997, 0.3996062992125986035, -1.581364829396325389 ) ) ;
#54652 = CARTESIAN_POINT ( 'NONE',  ( 0.000000000000000000, 0.4177165354330708569, -1.178877988035069047 ) ) ;
#54653 = ORIENTED_EDGE ( 'NONE', *, *, #22073, .F. ) ;
#54654 = CARTESIAN_POINT ( 'NONE',  ( 0.3996062992125986035, -0.1070741851644052972, -0.9757217847769029673 ) ) ;
#54655 = CARTESIAN_POINT ( 'NONE',  ( -0.7152230971128602510, -0.08942795157528024563, -0.3641732283464568787 ) ) ;
#54656 = CARTESIAN_POINT ( 'NONE',  ( -1.135170603674539924, -0.6692913385826771977, 0.1292274648535927661 ) ) ;
#54657 = CARTESIAN_POINT ( 'NONE',  ( 0.3458507752293908943, -0.3458507752293908943, -0.2559055118110235560 ) ) ;
#54658 = CARTESIAN_POINT ( 'NONE',  ( -0.3392501089628017219, -0.1958661417322836718, -2.656824146981627166 ) ) ;
#54659 = CARTESIAN_POINT ( 'NONE',  ( 1.541994750656168645, 0.2952755905511810774, -0.1292274648535930714 ) ) ;
#54660 = CARTESIAN_POINT ( 'NONE',  ( 0.6692913385826777528, 0.2952755905511811885, 0.000000000000000000 ) ) ;
#54661 = CARTESIAN_POINT ( 'NONE',  ( 0.6758530183727039509, -0.6692913385826771977, 0.1292274648535927661 ) ) ;
#54662 = CARTESIAN_POINT ( 'NONE',  ( -0.4461942257217840213, -0.5023911411419708095, -0.1820866141732282451 ) ) ;
#54663 = CARTESIAN_POINT ( 'NONE',  ( 0.01312335958005323398, 0.05413385826771666132, 0.4176697321401328100 ) ) ;
#54664 = CARTESIAN_POINT ( 'NONE',  ( -0.1265901696524986964, -0.4724409448818899238, -2.353674540682414218 ) ) ;
#54665 = CARTESIAN_POINT ( 'NONE',  ( -0.6233595800524928121, -0.2845877964562161244, -0.3641732283464567121 ) ) ;
#54666 = CARTESIAN_POINT ( 'NONE',  ( -0.2755905511811018171, 0.2952755905511811885, 0.000000000000000000 ) ) ;
#54667 = CARTESIAN_POINT ( 'NONE',  ( 0.2891555358219910499, 0.2891555358219910499, -1.789370078740157632 ) ) ;
#54668 = CARTESIAN_POINT ( 'NONE',  ( -1.601049868766403650, -0.6046776061558807314, 0.2411417322834647770 ) ) ;
#54669 = CARTESIAN_POINT ( 'NONE',  ( -0.1115485564304456306, 0.1771653543307087075, -0.09757992244046823083 ) ) ;
#54670 = CARTESIAN_POINT ( 'NONE',  ( 1.660104986876641320, -0.08942795157527998196, 0.3641732283464567121 ) ) ;
#54671 = CARTESIAN_POINT ( 'NONE',  ( -1.122047244094487306, -0.5400638737290844871, 0.3530559997133364547 ) ) ;
#54672 = CARTESIAN_POINT ( 'NONE',  ( -0.8989501312335946848, -0.5511811023622046335, 0.09757992244046803654 ) ) ;
#54673 = DIRECTION ( 'NONE',  ( 1.000000000000000000, -1.445602896647338917E-16, 0.000000000000000000 ) ) ;
#54674 = CARTESIAN_POINT ( 'NONE',  ( -1.220472440944881054, 0.2952755905511811885, 0.000000000000000000 ) ) ;
#54675 = CARTESIAN_POINT ( 'NONE',  ( -0.5577427821522301654, -0.3162353388693405765, 0.4822834645669290543 ) ) ;
#54676 = B_SPLINE_CURVE_WITH_KNOTS ( 'NONE', 3,
 ( #30390, #49334, #74622, #43010 ),
 .UNSPECIFIED., .F., .F.,
 ( 4, 4 ),
 ( 2.888536477588258382E-07, 0.001436607511248039464 ),
 .UNSPECIFIED. ) ;
#54677 = CARTESIAN_POINT ( 'NONE',  ( 0.4133858267716541968, 0.1660481256975885056, 0.3530559997133364547 ) ) ;
#54678 = CARTESIAN_POINT ( 'NONE',  ( -0.2867679344610366554, 0.2867679344610365444, -2.304442626475378564 ) ) ;
#54679 = CARTESIAN_POINT ( 'NONE',  ( 0.5314960629920851831, 2.702643891907236195, 3.896872718254352108 ) ) ;
#54680 = CARTESIAN_POINT ( 'NONE',  ( 0.5052493438320218022, -0.5511811023622048555, -0.09757992244046775898 ) ) ;
#54681 = CARTESIAN_POINT ( 'NONE',  ( 1.043307086614173818, -0.5400638737290845981, -0.3530559997133363437 ) ) ;
#54682 = CARTESIAN_POINT ( 'NONE',  ( -1.404199475065615932, -0.004921259842519576551, 0.3153832671262227771 ) ) ;
#54683 =( BOUNDED_SURFACE ( )  B_SPLINE_SURFACE ( 1, 2, ( 
 ( #62404, #68329, #3933, #29591, #67914, #17809, #81789, #10250, #36323, #55254, #23276, #30000, #16989, #55664, #42632, #23686, #49360, #17404, #36728, #33232, #34054, #41201, #8389, #40371, #27738, #66465, #71527, #39962, #66052, #27318, #7128, #65222, #45828, #26491, #32802, #39534, #8800, #20178, #52561, #72774, #26902, #13874, #2073, #2493, #47084, #59718, #72368, #79521, #79111, #52978, #60142, #34476, #15125, #7560, #40779, #53403, #46675, #14717, #58894, #47499, #59304, #52143, #1661, #58469, #28153, #21014, #14302, #78270, #53808, #21429, #65649, #21836, #73192, #15542, #77849, #1254, #833, #20601, #46254, #71949, #7978, #33642, #78691, #42423, #54224, #55874, #9219, #62204, #15960, #34892, #3313, #60554, #30212, #81169, #3728, #42834, #36529, #2904, #55052, #28568, #80759, #35300, #74859, #49568, #73618, #74023, #75264, #28977, #16369, #4541, #74439, #29392, #41607, #10468, #48326, #61794, #22255, #9630, #36121, #67296, #17201, #4134, #42016, #67709, #68527, #81586, #60962, #54644, #10868, #10046, #80354, #29799, #22667, #35709, #47913, #55460, #23903, #23487, #17607, #66889, #79941, #61379, #23073, #48741, #16786, #68123, #49153, #25539, #24308, #30632, #76902, #69353, #12516, #70163, #18428, #82400, #82803, #32278, #19232, #77322, #4965, #62622, #31445, #56701, #38177, #51617, #25959, #304, #44882, #81994, #76084, #44070, #38594, #11285, #63852, #63034, #56297, #5372, #69762, #43239, #31033, #68936, #11707, #75676, #6189, #36945, #25127, #37362, #49978, #18016, #57938, #31867, #76498, #6607, #43651, #12936, #24718, #50387, #50797, #12107, #18826, #37765, #63440, #83218, #64272, #57109, #5776, #44472, #57527, #51205, #70582, #78168, #8705, #726, #77747, #45730, #71426, #52042, #26384, #20080, #33957, #1564, #20915, #8289, #13773, #39430, #1973, #65546, #65953, #46570, #65116, #7453, #33123, #59619, #59203, #7877, #58793, #79011, #1151, #71848, #20499, #21331, #40682, #39005, #78590, #2397, #13352, #32697, #26802, #72268, #53712, #14616, #52879, #40270, #46983, #52460, #46153, #27637, #39855, #19651, #14198, #58363, #64689, #45313, #33541, #72677, #27218, #53299, #15026, #66368, #34376, #60041, #28054, #71008, #7028, #61280, #68439, #68028, #41921, #49061, #23394, #4044, #79842, #61704, #54963, #35617, #3633, #54128, #36439, #48237, #15444, #73933, #30120, #29709, #9945, #3220, #15869, #74760, #80670, #28883, #48649, #17109, #55372, #41104, #66792, #42743, #62112, #10779, #2808, #41517, #81078, #4455, #22983, #9127, #79419, #21739, #47404, #28467, #73093, #67202, #34798, #60457, #10372, #16276, #22159, #47819, #73520, #67615, #9534, #29301, #35205, #60867, #54545, #80260, #22576, #74345, #16690, #42329, #36030, #63346, #75992, #4864, #63755, #44787, #76402, #81490, #44376, #25443, #17517, #70483, #25031, #43149, #6096, #31770, #57431, #12840, #69671, #68846, #5279, #55782, #56608, #51109, #83124, #57016, #43974, #38499, #23806, #49479, #82308, #76806, #19137, #56202, #38081, #31350, #12014, #37668, #30538, #64181, #24628, #75172, #50294, #6515, #11194, #5681, #62944, #75586, #36853, #82712, #30941, #50704, #62526, #81903, #24214, #49885, #17925, #43561, #69262, #11609, #37268, #18334, #18734, #70068, #12423, #22375, #57840, #28685, #64592, #208, #51943, #25861, #80057, #47617, #52360, #9334, #3018, #51521, #20397, #77224, #46049, #626, #41321, #16072, #38912, #39326, #41718, #77648, #65012, #54346, #40901, #78066, #6928, #67002, #48035, #53928, #19553, #21958, #73737, #45212, #67411, #2609, #70913, #35005, #60670, #32185, #13262, #71743, #32599, #7347, #58262, #33015, #26282, #19981, #34595, #15241, #45631, #71326, #13674, #58685, #1050, #26704, #66582, #8918, #60260, #28266, #79640, #73313, #15660, #43761, #10979, #42946, #30325, #69050, #74142, #42543, #68640, #29911, #9745, #67828, #48442, #29094, #35416, #42133, #11399, #22782, #55167, #75373, #29506, #16487, #4652, #5076, #49681, #36639, #74973, #82107, #81703, #55575, #62740, #17318, #62315, #24013, #10167, #35832, #17722, #81285, #55991, #43348, #61499, #3846, #80876, #37056, #49270 ),
 ( #30745, #68246, #10580, #56408, #24420, #23188, #48859, #50090, #36237, #74559, #75786, #16905, #61907, #4249, #18128, #61081, #3432, #54766, #80470, #23601, #82922, #18537, #25243, #37471, #44180, #19355, #51739, #50496, #56812, #19775, #12225, #38710, #13056, #44586, #50907, #25657, #58484, #45429, #20193, #31146, #5485, #57642, #76608, #64388, #77864, #52160, #26506, #71124, #24827, #18938, #70280, #64805, #63144, #6724, #5891, #82511, #31563, #12633, #69466, #57221, #11819, #37882, #69872, #32394, #76199, #51319, #63557, #38292, #63969, #849, #58057, #45004, #32817, #6305, #39124, #31982, #5, #77022, #70704, #423, #26079, #77442, #13467, #7144, #59735, #45844, #71964, #34071, #1269, #20617, #21030, #34909, #26917, #46269, #14319, #39977, #78286, #52577, #65667, #60158, #2089, #59320, #15140, #54243, #28587, #2923, #21853, #7993, #78706, #46690, #41219, #13890, #72790, #33657, #33248, #1676, #72383, #79960, #27333, #71543, #52993, #14733, #40796, #39549, #27754, #40385, #7576, #58910, #60572, #66481, #79127, #9237, #66068, #15559, #65238, #8404, #53418, #21444, #47101, #8816, #34493, #2510, #66906, #28169, #53826, #79540, #47517, #73209, #80372, #80777, #11306, #3331, #22685, #48344, #74041, #54661, #28995, #16388, #36548, #4153, #23506, #10888, #42035, #67729, #4562, #68142, #68547, #49173, #10064, #35727, #61397, #62224, #61813, #10487, #3746, #81607, #29410, #74459, #23093, #74878, #55069, #17222, #60981, #48760, #42854, #16806, #30233, #55895, #42442, #36141, #23923, #43259, #29818, #55479, #49589, #81189, #75284, #17627, #68956, #36965, #62642, #4986, #30653, #56317, #22273, #47933, #73636, #15978, #41625, #67314, #9649, #35318, #31885, #64290, #63054, #69374, #32296, #24739, #51224, #25557, #57129, #37786, #38195, #71026, #57956, #32716, #43671, #18037, #37383, #56723, #82824, #13370, #5392, #82420, #50407, #76105, #31054, #18448, #44090, #12954, #63870, #83236, #70600, #69784, #12129, #6624, #44492, #44902, #76922, #63463, #5797, #31467, #38612, #6208, #70183, #25148, #324, #50816, #76517, #18846, #19250, #12536, #25978, #57545, #51636, #77341, #19670, #45331, #39023, #64707, #7047, #82015, #24329, #49999, #75696, #11727, #59220, #33141, #53316, #20517, #65562, #39448, #79028, #53727, #47000, #21754, #47417, #15459, #71865, #7472, #14215, #26403, #58812, #8306, #40697, #65136, #45748, #8719, #1169, #27653, #1990, #33557, #39873, #14632, #73108, #34390, #9141, #20097, #77765, #46588, #7896, #21347, #66807, #41117, #58383, #60056, #13791, #1581, #27236, #79435, #52059, #72694, #78186, #71443, #46169, #52895, #744, #78608, #26820, #52478, #20931, #15041, #72286, #40288, #65969, #33973, #59634, #66382, #2411, #28069, #81502, #73537, #4467, #34812, #28483, #42344, #15882, #74360, #73946, #43161, #74774, #30132, #48662, #60471, #60883, #22997, #55795, #54143, #16703, #79857, #68042, #3234, #42757, #17530, #41530, #41935, #68857, #54560, #67631, #23823, #10388, #54976, #67216, #68452, #49492, #55384, #2822, #23407, #75184, #22174, #47832, #4055, #9549, #10791, #36451, #62125, #35219, #36045, #28898, #9962, #80275, #35633, #22589, #48250, #61717, #29722, #16291, #61294, #3650, #29315, #80683, #81090, #49074, #17123, #77236, #4878, #24227, #37281, #38093, #45225, #12433, #44387, #31780, #70494, #75597, #43987, #70080, #31363, #11206, #69273, #49899, #30552, #36865, #43572, #12852, #17936, #56620, #76816, #30953, #11619, #6107, #6527, #51121, #63767, #76414, #220, #83135, #57028, #64192, #38510, #19148, #62956, #44799, #57442, #50716, #18744, #5293, #51533, #63358, #56218, #5692, #62540, #32197, #25042, #18346, #82320, #57853, #25454, #69683, #25871, #19565, #81916, #24639, #50306, #76004, #12026, #37683, #82722, #33028, #53203, #78916, #46477, #58273, #59946, #27962, #20824, #21237, #51954, #638, #46893, #13684, #40181, #14530, #46061, #19991, #71337, #72587, #71754, #45642, #65865, #58697, #78078, #77660, #8200, #66275, #59529, #34285, #2302, #53621, #1062, #33865, #1886, #27546, #79329, #72173, #14934, #39337, #26294, #40593, #65024, #8615 ) ),
 .UNSPECIFIED., .F., .F., .F. ) 
 B_SPLINE_SURFACE_WITH_KNOTS ( ( 2, 2 ),
 ( 3, 2, 2, 2, 2, 2, 2, 2, 2, 2, 2, 2, 2, 2, 2, 2, 2, 2, 2, 2, 2, 2, 2, 2, 2, 2, 2, 2, 2, 2, 2, 2, 2, 2, 2, 2, 2, 2, 2, 2, 2, 2, 2, 2, 2, 2, 2, 2, 2, 2, 2, 2, 2, 2, 2, 2, 2, 2, 2, 2, 2, 2, 2, 2, 2, 2, 2, 2, 2, 2, 2, 2, 2, 2, 2, 2, 2, 2, 2, 2, 2, 2, 2, 2, 2, 2, 2, 2, 2, 2, 2, 2, 2, 2, 2, 2, 2, 2, 2, 2, 2, 2, 2, 2, 2, 2, 2, 2, 2, 2, 2, 2, 2, 2, 2, 2, 2, 2, 2, 2, 2, 2, 2, 2, 2, 2, 2, 2, 2, 2, 2, 2, 2, 2, 2, 2, 2, 2, 2, 2, 2, 2, 2, 2, 2, 2, 2, 2, 2, 2, 2, 2, 2, 2, 2, 2, 2, 2, 2, 2, 2, 2, 2, 2, 2, 2, 2, 2, 2, 2, 2, 2, 2, 2, 2, 2, 2, 2, 2, 2, 2, 2, 2, 2, 2, 2, 2, 2, 2, 2, 2, 2, 2, 2, 2, 2, 2, 2, 2, 2, 2, 2, 2, 2, 2, 2, 2, 2, 2, 2, 2, 2, 2, 2, 2, 2, 2, 2, 2, 2, 2, 2, 2, 2, 2, 2, 2, 2, 2, 2, 2, 2, 2, 2, 2, 2, 2, 2, 2, 2, 2, 2, 2, 2, 2, 2, 2, 2, 2, 2, 2, 2, 2, 2, 2, 3 ),
 ( 0.000000000000000000, 1.000000000000000000 ),
 ( 0.000000000000000000, 0.003787878787878787984, 0.007575757575757575968, 0.01136363636363636395, 0.01515151515151515194, 0.01893939393939393992, 0.02272727272727272790, 0.02651515151515151589, 0.03030303030303030387, 0.03409090909090908839, 0.03787878787878787984, 0.04166666666666666435, 0.04545454545454545581, 0.04924242424242424032, 0.05303030303030303177, 0.05681818181818181629, 0.06060606060606060774, 0.06439393939393939226, 0.06818181818181817677, 0.07196969696969697516, 0.07575757575757575968, 0.07954545454545454419, 0.08333333333333332871, 0.08712121212121212710, 0.09090909090909091161, 0.09469696969696969613, 0.09848484848484848064, 0.1022727272727272790, 0.1060606060606060635, 0.1098484848484848481, 0.1136363636363636326, 0.1174242424242424310, 0.1212121212121212155, 0.1250000000000000000, 0.1287878787878787845, 0.1325757575757575690, 0.1363636363636363535, 0.1401515151515151381, 0.1439393939393939503, 0.1477272727272727348, 0.1515151515151515194, 0.1553030303030303039, 0.1590909090909090884, 0.1628787878787878729, 0.1666666666666666574, 0.1704545454545454419, 0.1742424242424242542, 0.1780303030303030387, 0.1818181818181818232, 0.1856060606060606077, 0.1893939393939393923, 0.1931818181818181768, 0.1969696969696969613, 0.2007575757575757458, 0.2045454545454545581, 0.2083333333333333426, 0.2121212121212121271, 0.2159090909090909116, 0.2196969696969696961, 0.2234848484848484806, 0.2272727272727272652, 0.2310606060606060497, 0.2348484848484848619, 0.2386363636363636465, 0.2424242424242424310, 0.2462121212121212155, 0.2500000000000000000, 0.2537878787878787845, 0.2575757575757575690, 0.2613636363636363535, 0.2651515151515151381, 0.2689393939393939226, 0.2727272727272727071, 0.2765151515151514916, 0.2803030303030302761, 0.2840909090909091161, 0.2878787878787879007, 0.2916666666666666852, 0.2954545454545454697, 0.2992424242424242542, 0.3030303030303030387, 0.3068181818181818232, 0.3106060606060606077, 0.3143939393939393923, 0.3181818181818181768, 0.3219696969696969613, 0.3257575757575757458, 0.3295454545454545303, 0.3333333333333333148, 0.3371212121212120993, 0.3409090909090908839, 0.3446969696969697239, 0.3484848484848485084, 0.3522727272727272929, 0.3560606060606060774, 0.3598484848484848619, 0.3636363636363636465, 0.3674242424242424310, 0.3712121212121212155, 0.3750000000000000000, 0.3787878787878787845, 0.3825757575757575690, 0.3863636363636363535, 0.3901515151515151381, 0.3939393939393939226, 0.3977272727272727071, 0.4015151515151514916, 0.4053030303030302761, 0.4090909090909091161, 0.4128787878787879007, 0.4166666666666666852, 0.4204545454545454697, 0.4242424242424242542, 0.4280303030303030387, 0.4318181818181818232, 0.4356060606060606077, 0.4393939393939393923, 0.4431818181818181768, 0.4469696969696969613, 0.4507575757575757458, 0.4545454545454545303, 0.4583333333333333148, 0.4621212121212120993, 0.4659090909090908839, 0.4696969696969697239, 0.4734848484848485084, 0.4772727272727272929, 0.4810606060606060774, 0.4848484848484848619, 0.4886363636363636465, 0.4924242424242424310, 0.4962121212121212155, 0.5000000000000000000, 0.5037878787878787845, 0.5075757575757575690, 0.5113636363636363535, 0.5151515151515151381, 0.5189393939393939226, 0.5227272727272727071, 0.5265151515151514916, 0.5303030303030302761, 0.5340909090909090606, 0.5378787878787878451, 0.5416666666666666297, 0.5454545454545454142, 0.5492424242424241987, 0.5530303030303029832, 0.5568181818181817677, 0.5606060606060605522, 0.5643939393939394478, 0.5681818181818182323, 0.5719696969696970168, 0.5757575757575758013, 0.5795454545454545858, 0.5833333333333333703, 0.5871212121212121549, 0.5909090909090909394, 0.5946969696969697239, 0.5984848484848485084, 0.6022727272727272929, 0.6060606060606060774, 0.6098484848484848619, 0.6136363636363636465, 0.6174242424242424310, 0.6212121212121212155, 0.6250000000000000000, 0.6287878787878787845, 0.6325757575757575690, 0.6363636363636363535, 0.6401515151515151381, 0.6439393939393939226, 0.6477272727272727071, 0.6515151515151514916, 0.6553030303030302761, 0.6590909090909090606, 0.6628787878787878451, 0.6666666666666666297, 0.6704545454545454142, 0.6742424242424241987, 0.6780303030303029832, 0.6818181818181817677, 0.6856060606060605522, 0.6893939393939394478, 0.6931818181818182323, 0.6969696969696970168, 0.7007575757575758013, 0.7045454545454545858, 0.7083333333333333703, 0.7121212121212121549, 0.7159090909090909394, 0.7196969696969697239, 0.7234848484848485084, 0.7272727272727272929, 0.7310606060606060774, 0.7348484848484848619, 0.7386363636363636465, 0.7424242424242424310, 0.7462121212121212155, 0.7500000000000000000, 0.7537878787878787845, 0.7575757575757575690, 0.7613636363636363535, 0.7651515151515151381, 0.7689393939393939226, 0.7727272727272727071, 0.7765151515151514916, 0.7803030303030302761, 0.7840909090909090606, 0.7878787878787878451, 0.7916666666666666297, 0.7954545454545454142, 0.7992424242424241987, 0.8030303030303029832, 0.8068181818181817677, 0.8106060606060605522, 0.8143939393939394478, 0.8181818181818182323, 0.8219696969696970168, 0.8257575757575758013, 0.8295454545454545858, 0.8333333333333333703, 0.8371212121212121549, 0.8409090909090909394, 0.8446969696969697239, 0.8484848484848485084, 0.8522727272727272929, 0.8560606060606060774, 0.8598484848484848619, 0.8636363636363636465, 0.8674242424242424310, 0.8712121212121212155, 0.8750000000000000000, 0.8787878787878787845, 0.8825757575757575690, 0.8863636363636363535, 0.8901515151515151381, 0.8939393939393939226, 0.8977272727272727071, 0.9015151515151514916, 0.9053030303030302761, 0.9090909090909090606, 0.9128787878787878451, 0.9166666666666666297, 0.9204545454545454142, 0.9242424242424241987, 0.9280303030303029832, 0.9318181818181817677, 0.9356060606060605522, 0.9393939393939394478, 0.9431818181818182323, 0.9469696969696970168, 0.9507575757575758013, 0.9545454545454545858, 0.9583333333333333703, 0.9621212121212121549, 0.9659090909090909394 ),
 .UNSPECIFIED. ) 
 GEOMETRIC_REPRESENTATION_ITEM ( )  RATIONAL_B_SPLINE_SURFACE ( (
 ( 1.000000000000000000, 0.9659258262890683122, 1.000000000000000000, 0.9659258262890683122, 1.000000000000000000, 0.9659258262890683122, 1.000000000000000000, 0.9659258262890683122, 1.000000000000000000, 0.9659258262890683122, 1.000000000000000000, 0.9659258262890683122, 1.000000000000000000, 0.9659258262890683122, 1.000000000000000000, 0.9659258262890683122, 1.000000000000000000, 0.9659258262890683122, 1.000000000000000000, 0.9659258262890683122, 1.000000000000000000, 0.9659258262890683122, 1.000000000000000000, 0.9659258262890683122, 1.000000000000000000, 0.9659258262890683122, 1.000000000000000000, 0.9659258262890683122, 1.000000000000000000, 0.9659258262890683122, 1.000000000000000000, 0.9659258262890683122, 1.000000000000000000, 0.9659258262890683122, 1.000000000000000000, 0.9659258262890683122, 1.000000000000000000, 0.9659258262890683122, 1.000000000000000000, 0.9659258262890683122, 1.000000000000000000, 0.9659258262890683122, 1.000000000000000000, 0.9659258262890683122, 1.000000000000000000, 0.9659258262890683122, 1.000000000000000000, 0.9659258262890683122, 1.000000000000000000, 0.9659258262890683122, 1.000000000000000000, 0.9659258262890683122, 1.000000000000000000, 0.9659258262890683122, 1.000000000000000000, 0.9659258262890683122, 1.000000000000000000, 0.9659258262890683122, 1.000000000000000000, 0.9659258262890683122, 1.000000000000000000, 0.9659258262890683122, 1.000000000000000000, 0.9659258262890683122, 1.000000000000000000, 0.9659258262890683122, 1.000000000000000000, 0.9659258262890683122, 1.000000000000000000, 0.9659258262890683122, 1.000000000000000000, 0.9659258262890683122, 1.000000000000000000, 0.9659258262890683122, 1.000000000000000000, 0.9659258262890683122, 1.000000000000000000, 0.9659258262890683122, 1.000000000000000000, 0.9659258262890683122, 1.000000000000000000, 0.9659258262890683122, 1.000000000000000000, 0.9659258262890683122, 1.000000000000000000, 0.9659258262890683122, 1.000000000000000000, 0.9659258262890683122, 1.000000000000000000, 0.9659258262890683122, 1.000000000000000000, 0.9659258262890683122, 1.000000000000000000, 0.9659258262890683122, 1.000000000000000000, 0.9659258262890683122, 1.000000000000000000, 0.9659258262890683122, 1.000000000000000000, 0.9659258262890683122, 1.000000000000000000, 0.9659258262890683122, 1.000000000000000000, 0.9659258262890683122, 1.000000000000000000, 0.9659258262890683122, 1.000000000000000000, 0.9659258262890683122, 1.000000000000000000, 0.9659258262890683122, 1.000000000000000000, 0.9659258262890683122, 1.000000000000000000, 0.9659258262890683122, 1.000000000000000000, 0.9659258262890683122, 1.000000000000000000, 0.9659258262890683122, 1.000000000000000000, 0.9659258262890683122, 1.000000000000000000, 0.9659258262890683122, 1.000000000000000000, 0.9659258262890683122, 1.000000000000000000, 0.9659258262890683122, 1.000000000000000000, 0.9659258262890683122, 1.000000000000000000, 0.9659258262890683122, 1.000000000000000000, 0.9659258262890683122, 1.000000000000000000, 0.9659258262890683122, 1.000000000000000000, 0.9659258262890683122, 1.000000000000000000, 0.9659258262890683122, 1.000000000000000000, 0.9659258262890683122, 1.000000000000000000, 0.9659258262890683122, 1.000000000000000000, 0.9659258262890683122, 1.000000000000000000, 0.9659258262890683122, 1.000000000000000000, 0.9659258262890683122, 1.000000000000000000, 0.9659258262890683122, 1.000000000000000000, 0.9659258262890683122, 1.000000000000000000, 0.9659258262890683122, 1.000000000000000000, 0.9659258262890683122, 1.000000000000000000, 0.9659258262890683122, 1.000000000000000000, 0.9659258262890683122, 1.000000000000000000, 0.9659258262890683122, 1.000000000000000000, 0.9659258262890683122, 1.000000000000000000, 0.9659258262890683122, 1.000000000000000000, 0.9659258262890683122, 1.000000000000000000, 0.9659258262890683122, 1.000000000000000000, 0.9659258262890683122, 1.000000000000000000, 0.9659258262890683122, 1.000000000000000000, 0.9659258262890683122, 1.000000000000000000, 0.9659258262890683122, 1.000000000000000000, 0.9659258262890683122, 1.000000000000000000, 0.9659258262890683122, 1.000000000000000000, 0.9659258262890683122, 1.000000000000000000, 0.9659258262890683122, 1.000000000000000000, 0.9659258262890683122, 1.000000000000000000, 0.9659258262890683122, 1.000000000000000000, 0.9659258262890683122, 1.000000000000000000, 0.9659258262890683122, 1.000000000000000000, 0.9659258262890683122, 1.000000000000000000, 0.9659258262890683122, 1.000000000000000000, 0.9659258262890683122, 1.000000000000000000, 0.9659258262890683122, 1.000000000000000000, 0.9659258262890683122, 1.000000000000000000, 0.9659258262890683122, 1.000000000000000000, 0.9659258262890683122, 1.000000000000000000, 0.9659258262890683122, 1.000000000000000000, 0.9659258262890683122, 1.000000000000000000, 0.9659258262890683122, 1.000000000000000000, 0.9659258262890683122, 1.000000000000000000, 0.9659258262890683122, 1.000000000000000000, 0.9659258262890683122, 1.000000000000000000, 0.9659258262890683122, 1.000000000000000000, 0.9659258262890683122, 1.000000000000000000, 0.9659258262890683122, 1.000000000000000000, 0.9659258262890683122, 1.000000000000000000, 0.9659258262890683122, 1.000000000000000000, 0.9659258262890683122, 1.000000000000000000, 0.9659258262890683122, 1.000000000000000000, 0.9659258262890683122, 1.000000000000000000, 0.9659258262890683122, 1.000000000000000000, 0.9659258262890683122, 1.000000000000000000, 0.9659258262890683122, 1.000000000000000000, 0.9659258262890683122, 1.000000000000000000, 0.9659258262890683122, 1.000000000000000000, 0.9659258262890683122, 1.000000000000000000, 0.9659258262890683122, 1.000000000000000000, 0.9659258262890683122, 1.000000000000000000, 0.9659258262890683122, 1.000000000000000000, 0.9659258262890683122, 1.000000000000000000, 0.9659258262890683122, 1.000000000000000000, 0.9659258262890683122, 1.000000000000000000, 0.9659258262890683122, 1.000000000000000000, 0.9659258262890683122, 1.000000000000000000, 0.9659258262890683122, 1.000000000000000000, 0.9659258262890683122, 1.000000000000000000, 0.9659258262890683122, 1.000000000000000000, 0.9659258262890683122, 1.000000000000000000, 0.9659258262890683122, 1.000000000000000000, 0.9659258262890683122, 1.000000000000000000, 0.9659258262890683122, 1.000000000000000000, 0.9659258262890683122, 1.000000000000000000, 0.9659258262890683122, 1.000000000000000000, 0.9659258262890683122, 1.000000000000000000, 0.9659258262890683122, 1.000000000000000000, 0.9659258262890683122, 1.000000000000000000, 0.9659258262890683122, 1.000000000000000000, 0.9659258262890683122, 1.000000000000000000, 0.9659258262890683122, 1.000000000000000000, 0.9659258262890683122, 1.000000000000000000, 0.9659258262890683122, 1.000000000000000000, 0.9659258262890683122, 1.000000000000000000, 0.9659258262890683122, 1.000000000000000000, 0.9659258262890683122, 1.000000000000000000, 0.9659258262890683122, 1.000000000000000000, 0.9659258262890683122, 1.000000000000000000, 0.9659258262890683122, 1.000000000000000000, 0.9659258262890683122, 1.000000000000000000, 0.9659258262890683122, 1.000000000000000000, 0.9659258262890683122, 1.000000000000000000, 0.9659258262890683122, 1.000000000000000000, 0.9659258262890683122, 1.000000000000000000, 0.9659258262890683122, 1.000000000000000000, 0.9659258262890683122, 1.000000000000000000, 0.9659258262890683122, 1.000000000000000000, 0.9659258262890683122, 1.000000000000000000, 0.9659258262890683122, 1.000000000000000000, 0.9659258262890683122, 1.000000000000000000, 0.9659258262890683122, 1.000000000000000000, 0.9659258262890683122, 1.000000000000000000, 0.9659258262890683122, 1.000000000000000000, 0.9659258262890683122, 1.000000000000000000, 0.9659258262890683122, 1.000000000000000000, 0.9659258262890683122, 1.000000000000000000, 0.9659258262890683122, 1.000000000000000000, 0.9659258262890683122, 1.000000000000000000, 0.9659258262890683122, 1.000000000000000000, 0.9659258262890683122, 1.000000000000000000, 0.9659258262890683122, 1.000000000000000000, 0.9659258262890683122, 1.000000000000000000, 0.9659258262890683122, 1.000000000000000000, 0.9659258262890683122, 1.000000000000000000, 0.9659258262890683122, 1.000000000000000000, 0.9659258262890683122, 1.000000000000000000, 0.9659258262890683122, 1.000000000000000000, 0.9659258262890683122, 1.000000000000000000, 0.9659258262890683122, 1.000000000000000000, 0.9659258262890683122, 1.000000000000000000, 0.9659258262890683122, 1.000000000000000000, 0.9659258262890683122, 1.000000000000000000, 0.9659258262890683122, 1.000000000000000000, 0.9659258262890683122, 1.000000000000000000, 0.9659258262890683122, 1.000000000000000000, 0.9659258262890683122, 1.000000000000000000, 0.9659258262890683122, 1.000000000000000000, 0.9659258262890683122, 1.000000000000000000, 0.9659258262890683122, 1.000000000000000000, 0.9659258262890683122, 1.000000000000000000, 0.9659258262890683122, 1.000000000000000000, 0.9659258262890683122, 1.000000000000000000, 0.9659258262890683122, 1.000000000000000000, 0.9659258262890683122, 1.000000000000000000, 0.9659258262890683122, 1.000000000000000000, 0.9659258262890683122, 1.000000000000000000, 0.9659258262890683122, 1.000000000000000000, 0.9659258262890683122, 1.000000000000000000, 0.9659258262890683122, 1.000000000000000000, 0.9659258262890683122, 1.000000000000000000, 0.9659258262890683122, 1.000000000000000000, 0.9659258262890683122, 1.000000000000000000, 0.9659258262890683122, 1.000000000000000000, 0.9659258262890683122, 1.000000000000000000, 0.9659258262890683122, 1.000000000000000000, 0.9659258262890683122, 1.000000000000000000, 0.9659258262890683122, 1.000000000000000000, 0.9659258262890683122, 1.000000000000000000, 0.9659258262890683122, 1.000000000000000000, 0.9659258262890683122, 1.000000000000000000, 0.9659258262890683122, 1.000000000000000000, 0.9659258262890683122, 1.000000000000000000, 0.9659258262890683122, 1.000000000000000000, 0.9659258262890683122, 1.000000000000000000, 0.9659258262890683122, 1.000000000000000000, 0.9659258262890683122, 1.000000000000000000, 0.9659258262890683122, 1.000000000000000000, 0.9659258262890683122, 1.000000000000000000, 0.9659258262890683122, 1.000000000000000000, 0.9659258262890683122, 1.000000000000000000, 0.9659258262890683122, 1.000000000000000000, 0.9659258262890683122, 1.000000000000000000, 0.9659258262890683122, 1.000000000000000000, 0.9659258262890683122, 1.000000000000000000, 0.9659258262890683122, 1.000000000000000000, 0.9659258262890683122, 1.000000000000000000, 0.9659258262890683122, 1.000000000000000000, 0.9659258262890683122, 1.000000000000000000, 0.9659258262890683122, 1.000000000000000000, 0.9659258262890683122, 1.000000000000000000, 0.9659258262890683122, 1.000000000000000000, 0.9659258262890683122, 1.000000000000000000, 0.9659258262890683122, 1.000000000000000000, 0.9659258262890683122, 1.000000000000000000, 0.9659258262890683122, 1.000000000000000000, 0.9659258262890683122, 1.000000000000000000, 0.9659258262890683122, 1.000000000000000000, 0.9659258262890683122, 1.000000000000000000, 0.9659258262890683122, 1.000000000000000000, 0.9659258262890683122, 1.000000000000000000, 0.9659258262890683122, 1.000000000000000000, 0.9659258262890683122, 1.000000000000000000, 0.9659258262890683122, 1.000000000000000000, 0.9659258262890683122, 1.000000000000000000, 0.9659258262890683122, 1.000000000000000000, 0.9659258262890683122, 1.000000000000000000, 0.9659258262890683122, 1.000000000000000000, 0.9659258262890683122, 1.000000000000000000, 0.9659258262890683122, 1.000000000000000000),
 ( 1.000000000000000000, 0.9659258262890683122, 1.000000000000000000, 0.9659258262890683122, 1.000000000000000000, 0.9659258262890683122, 1.000000000000000000, 0.9659258262890683122, 1.000000000000000000, 0.9659258262890683122, 1.000000000000000000, 0.9659258262890683122, 1.000000000000000000, 0.9659258262890683122, 1.000000000000000000, 0.9659258262890683122, 1.000000000000000000, 0.9659258262890683122, 1.000000000000000000, 0.9659258262890683122, 1.000000000000000000, 0.9659258262890683122, 1.000000000000000000, 0.9659258262890683122, 1.000000000000000000, 0.9659258262890683122, 1.000000000000000000, 0.9659258262890683122, 1.000000000000000000, 0.9659258262890683122, 1.000000000000000000, 0.9659258262890683122, 1.000000000000000000, 0.9659258262890683122, 1.000000000000000000, 0.9659258262890683122, 1.000000000000000000, 0.9659258262890683122, 1.000000000000000000, 0.9659258262890683122, 1.000000000000000000, 0.9659258262890683122, 1.000000000000000000, 0.9659258262890683122, 1.000000000000000000, 0.9659258262890683122, 1.000000000000000000, 0.9659258262890683122, 1.000000000000000000, 0.9659258262890683122, 1.000000000000000000, 0.9659258262890683122, 1.000000000000000000, 0.9659258262890683122, 1.000000000000000000, 0.9659258262890683122, 1.000000000000000000, 0.9659258262890683122, 1.000000000000000000, 0.9659258262890683122, 1.000000000000000000, 0.9659258262890683122, 1.000000000000000000, 0.9659258262890683122, 1.000000000000000000, 0.9659258262890683122, 1.000000000000000000, 0.9659258262890683122, 1.000000000000000000, 0.9659258262890683122, 1.000000000000000000, 0.9659258262890683122, 1.000000000000000000, 0.9659258262890683122, 1.000000000000000000, 0.9659258262890683122, 1.000000000000000000, 0.9659258262890683122, 1.000000000000000000, 0.9659258262890683122, 1.000000000000000000, 0.9659258262890683122, 1.000000000000000000, 0.9659258262890683122, 1.000000000000000000, 0.9659258262890683122, 1.000000000000000000, 0.9659258262890683122, 1.000000000000000000, 0.9659258262890683122, 1.000000000000000000, 0.9659258262890683122, 1.000000000000000000, 0.9659258262890683122, 1.000000000000000000, 0.9659258262890683122, 1.000000000000000000, 0.9659258262890683122, 1.000000000000000000, 0.9659258262890683122, 1.000000000000000000, 0.9659258262890683122, 1.000000000000000000, 0.9659258262890683122, 1.000000000000000000, 0.9659258262890683122, 1.000000000000000000, 0.9659258262890683122, 1.000000000000000000, 0.9659258262890683122, 1.000000000000000000, 0.9659258262890683122, 1.000000000000000000, 0.9659258262890683122, 1.000000000000000000, 0.9659258262890683122, 1.000000000000000000, 0.9659258262890683122, 1.000000000000000000, 0.9659258262890683122, 1.000000000000000000, 0.9659258262890683122, 1.000000000000000000, 0.9659258262890683122, 1.000000000000000000, 0.9659258262890683122, 1.000000000000000000, 0.9659258262890683122, 1.000000000000000000, 0.9659258262890683122, 1.000000000000000000, 0.9659258262890683122, 1.000000000000000000, 0.9659258262890683122, 1.000000000000000000, 0.9659258262890683122, 1.000000000000000000, 0.9659258262890683122, 1.000000000000000000, 0.9659258262890683122, 1.000000000000000000, 0.9659258262890683122, 1.000000000000000000, 0.9659258262890683122, 1.000000000000000000, 0.9659258262890683122, 1.000000000000000000, 0.9659258262890683122, 1.000000000000000000, 0.9659258262890683122, 1.000000000000000000, 0.9659258262890683122, 1.000000000000000000, 0.9659258262890683122, 1.000000000000000000, 0.9659258262890683122, 1.000000000000000000, 0.9659258262890683122, 1.000000000000000000, 0.9659258262890683122, 1.000000000000000000, 0.9659258262890683122, 1.000000000000000000, 0.9659258262890683122, 1.000000000000000000, 0.9659258262890683122, 1.000000000000000000, 0.9659258262890683122, 1.000000000000000000, 0.9659258262890683122, 1.000000000000000000, 0.9659258262890683122, 1.000000000000000000, 0.9659258262890683122, 1.000000000000000000, 0.9659258262890683122, 1.000000000000000000, 0.9659258262890683122, 1.000000000000000000, 0.9659258262890683122, 1.000000000000000000, 0.9659258262890683122, 1.000000000000000000, 0.9659258262890683122, 1.000000000000000000, 0.9659258262890683122, 1.000000000000000000, 0.9659258262890683122, 1.000000000000000000, 0.9659258262890683122, 1.000000000000000000, 0.9659258262890683122, 1.000000000000000000, 0.9659258262890683122, 1.000000000000000000, 0.9659258262890683122, 1.000000000000000000, 0.9659258262890683122, 1.000000000000000000, 0.9659258262890683122, 1.000000000000000000, 0.9659258262890683122, 1.000000000000000000, 0.9659258262890683122, 1.000000000000000000, 0.9659258262890683122, 1.000000000000000000, 0.9659258262890683122, 1.000000000000000000, 0.9659258262890683122, 1.000000000000000000, 0.9659258262890683122, 1.000000000000000000, 0.9659258262890683122, 1.000000000000000000, 0.9659258262890683122, 1.000000000000000000, 0.9659258262890683122, 1.000000000000000000, 0.9659258262890683122, 1.000000000000000000, 0.9659258262890683122, 1.000000000000000000, 0.9659258262890683122, 1.000000000000000000, 0.9659258262890683122, 1.000000000000000000, 0.9659258262890683122, 1.000000000000000000, 0.9659258262890683122, 1.000000000000000000, 0.9659258262890683122, 1.000000000000000000, 0.9659258262890683122, 1.000000000000000000, 0.9659258262890683122, 1.000000000000000000, 0.9659258262890683122, 1.000000000000000000, 0.9659258262890683122, 1.000000000000000000, 0.9659258262890683122, 1.000000000000000000, 0.9659258262890683122, 1.000000000000000000, 0.9659258262890683122, 1.000000000000000000, 0.9659258262890683122, 1.000000000000000000, 0.9659258262890683122, 1.000000000000000000, 0.9659258262890683122, 1.000000000000000000, 0.9659258262890683122, 1.000000000000000000, 0.9659258262890683122, 1.000000000000000000, 0.9659258262890683122, 1.000000000000000000, 0.9659258262890683122, 1.000000000000000000, 0.9659258262890683122, 1.000000000000000000, 0.9659258262890683122, 1.000000000000000000, 0.9659258262890683122, 1.000000000000000000, 0.9659258262890683122, 1.000000000000000000, 0.9659258262890683122, 1.000000000000000000, 0.9659258262890683122, 1.000000000000000000, 0.9659258262890683122, 1.000000000000000000, 0.9659258262890683122, 1.000000000000000000, 0.9659258262890683122, 1.000000000000000000, 0.9659258262890683122, 1.000000000000000000, 0.9659258262890683122, 1.000000000000000000, 0.9659258262890683122, 1.000000000000000000, 0.9659258262890683122, 1.000000000000000000, 0.9659258262890683122, 1.000000000000000000, 0.9659258262890683122, 1.000000000000000000, 0.9659258262890683122, 1.000000000000000000, 0.9659258262890683122, 1.000000000000000000, 0.9659258262890683122, 1.000000000000000000, 0.9659258262890683122, 1.000000000000000000, 0.9659258262890683122, 1.000000000000000000, 0.9659258262890683122, 1.000000000000000000, 0.9659258262890683122, 1.000000000000000000, 0.9659258262890683122, 1.000000000000000000, 0.9659258262890683122, 1.000000000000000000, 0.9659258262890683122, 1.000000000000000000, 0.9659258262890683122, 1.000000000000000000, 0.9659258262890683122, 1.000000000000000000, 0.9659258262890683122, 1.000000000000000000, 0.9659258262890683122, 1.000000000000000000, 0.9659258262890683122, 1.000000000000000000, 0.9659258262890683122, 1.000000000000000000, 0.9659258262890683122, 1.000000000000000000, 0.9659258262890683122, 1.000000000000000000, 0.9659258262890683122, 1.000000000000000000, 0.9659258262890683122, 1.000000000000000000, 0.9659258262890683122, 1.000000000000000000, 0.9659258262890683122, 1.000000000000000000, 0.9659258262890683122, 1.000000000000000000, 0.9659258262890683122, 1.000000000000000000, 0.9659258262890683122, 1.000000000000000000, 0.9659258262890683122, 1.000000000000000000, 0.9659258262890683122, 1.000000000000000000, 0.9659258262890683122, 1.000000000000000000, 0.9659258262890683122, 1.000000000000000000, 0.9659258262890683122, 1.000000000000000000, 0.9659258262890683122, 1.000000000000000000, 0.9659258262890683122, 1.000000000000000000, 0.9659258262890683122, 1.000000000000000000, 0.9659258262890683122, 1.000000000000000000, 0.9659258262890683122, 1.000000000000000000, 0.9659258262890683122, 1.000000000000000000, 0.9659258262890683122, 1.000000000000000000, 0.9659258262890683122, 1.000000000000000000, 0.9659258262890683122, 1.000000000000000000, 0.9659258262890683122, 1.000000000000000000, 0.9659258262890683122, 1.000000000000000000, 0.9659258262890683122, 1.000000000000000000, 0.9659258262890683122, 1.000000000000000000, 0.9659258262890683122, 1.000000000000000000, 0.9659258262890683122, 1.000000000000000000, 0.9659258262890683122, 1.000000000000000000, 0.9659258262890683122, 1.000000000000000000, 0.9659258262890683122, 1.000000000000000000, 0.9659258262890683122, 1.000000000000000000, 0.9659258262890683122, 1.000000000000000000, 0.9659258262890683122, 1.000000000000000000, 0.9659258262890683122, 1.000000000000000000, 0.9659258262890683122, 1.000000000000000000, 0.9659258262890683122, 1.000000000000000000, 0.9659258262890683122, 1.000000000000000000, 0.9659258262890683122, 1.000000000000000000, 0.9659258262890683122, 1.000000000000000000, 0.9659258262890683122, 1.000000000000000000, 0.9659258262890683122, 1.000000000000000000, 0.9659258262890683122, 1.000000000000000000, 0.9659258262890683122, 1.000000000000000000, 0.9659258262890683122, 1.000000000000000000, 0.9659258262890683122, 1.000000000000000000, 0.9659258262890683122, 1.000000000000000000, 0.9659258262890683122, 1.000000000000000000, 0.9659258262890683122, 1.000000000000000000, 0.9659258262890683122, 1.000000000000000000, 0.9659258262890683122, 1.000000000000000000, 0.9659258262890683122, 1.000000000000000000, 0.9659258262890683122, 1.000000000000000000, 0.9659258262890683122, 1.000000000000000000, 0.9659258262890683122, 1.000000000000000000, 0.9659258262890683122, 1.000000000000000000, 0.9659258262890683122, 1.000000000000000000, 0.9659258262890683122, 1.000000000000000000, 0.9659258262890683122, 1.000000000000000000, 0.9659258262890683122, 1.000000000000000000, 0.9659258262890683122, 1.000000000000000000, 0.9659258262890683122, 1.000000000000000000, 0.9659258262890683122, 1.000000000000000000, 0.9659258262890683122, 1.000000000000000000, 0.9659258262890683122, 1.000000000000000000, 0.9659258262890683122, 1.000000000000000000, 0.9659258262890683122, 1.000000000000000000, 0.9659258262890683122, 1.000000000000000000, 0.9659258262890683122, 1.000000000000000000, 0.9659258262890683122, 1.000000000000000000, 0.9659258262890683122, 1.000000000000000000, 0.9659258262890683122, 1.000000000000000000, 0.9659258262890683122, 1.000000000000000000, 0.9659258262890683122, 1.000000000000000000, 0.9659258262890683122, 1.000000000000000000, 0.9659258262890683122, 1.000000000000000000, 0.9659258262890683122, 1.000000000000000000, 0.9659258262890683122, 1.000000000000000000, 0.9659258262890683122, 1.000000000000000000, 0.9659258262890683122, 1.000000000000000000, 0.9659258262890683122, 1.000000000000000000, 0.9659258262890683122, 1.000000000000000000, 0.9659258262890683122, 1.000000000000000000, 0.9659258262890683122, 1.000000000000000000, 0.9659258262890683122, 1.000000000000000000, 0.9659258262890683122, 1.000000000000000000, 0.9659258262890683122, 1.000000000000000000, 0.9659258262890683122, 1.000000000000000000, 0.9659258262890683122, 1.000000000000000000, 0.9659258262890683122, 1.000000000000000000, 0.9659258262890683122, 1.000000000000000000, 0.9659258262890683122, 1.000000000000000000, 0.9659258262890683122, 1.000000000000000000) ) ) 
 REPRESENTATION_ITEM ( '' )  SURFACE ( )  );
#54684 = CARTESIAN_POINT ( 'NONE',  ( 0.9908136482939640111, -0.6692913385826771977, 0.1292274648535927661 ) ) ;
#54685 = CARTESIAN_POINT ( 'NONE',  ( -1.640419947506561060, -0.3690944881889765550, -0.3153832671262227771 ) ) ;
#54686 = CARTESIAN_POINT ( 'NONE',  ( -0.4986876640419942164, -0.6046776061558807314, 0.2411417322834647770 ) ) ;
#54687 = CARTESIAN_POINT ( 'NONE',  ( 0.2099737532808405305, -0.5023911411419708095, 0.1820866141732285504 ) ) ;
#54688 = DIRECTION ( 'NONE',  ( 0.000000000000000000, 0.000000000000000000, 1.000000000000000000 ) ) ;
#54689 = CARTESIAN_POINT ( 'NONE',  ( 0.6824146981627303710, 0.1283753931104746893, -0.1820866141732285504 ) ) ;
#54690 = EDGE_CURVE ( 'NONE', #57945, #79833, #55280, .T. ) ;
#54691 = AXIS2_PLACEMENT_3D ( 'NONE', #59783, #73684, #59367 ) ;
#54692 = CARTESIAN_POINT ( 'NONE',  ( 0.01968503937007957949, -0.5400638737290845981, -0.3530559997133363437 ) ) ;
#54693 = CARTESIAN_POINT ( 'NONE',  ( 0.1998031496062994128, -0.3460692066303957537, -0.1686351706036745557 ) ) ;
#54694 = EDGE_CURVE ( 'NONE', #73064, #24616, #10694, .T. ) ;
#54695 = CARTESIAN_POINT ( 'NONE',  ( -0.9120734908136475250, 0.2952755905511811885, 0.1292274648535926551 ) ) ;
#54696 = AXIS2_PLACEMENT_3D ( 'NONE', #53557, #71686, #28306 ) ;
#54697 = CARTESIAN_POINT ( 'NONE',  ( -0.1049643490035307020, 0.3917322834645669549, -1.980971128608924214 ) ) ;
#54698 = CARTESIAN_POINT ( 'NONE',  ( 1.128608923884514947, 0.1283753931104748280, 0.1820866141732283561 ) ) ;
#54700 = AXIS2_PLACEMENT_3D ( 'NONE', #43953, #11993, #37647 ) ;
#54699 = CARTESIAN_POINT ( 'NONE',  ( -0.07874015748031421014, -0.1870078740157479769, 0.4822834645669291653 ) ) ;
#54701 = AXIS2_PLACEMENT_3D ( 'NONE', #25406, #44340, #70031 ) ;
#54702 = CARTESIAN_POINT ( 'NONE',  ( -0.3674540682414689785, 0.2306618581243848609, 0.2411417322834645549 ) ) ;
#54703 = CARTESIAN_POINT ( 'NONE',  ( -0.4396325459317577122, -0.5511811023622048555, -0.09757992244046775898 ) ) ;
#54704 = DIRECTION ( 'NONE',  ( -0.000000000000000000, -1.000000000000000000, -0.000000000000000000 ) ) ;
#54705 = CARTESIAN_POINT ( 'NONE',  ( -0.4133858267716528645, -0.4536011799217367080, 0.2665933059059888421 ) ) ;
#54706 = CARTESIAN_POINT ( 'NONE',  ( 0.1902887139107617975, -0.6692913385826773087, -0.1292274648535924053 ) ) ;
#54707 = CARTESIAN_POINT ( 'NONE',  ( -1.266404199475064773, -0.2845877964562159024, 0.3641732283464567677 ) ) ;
#54708 = CARTESIAN_POINT ( 'NONE',  ( -0.3460692066303957537, -0.1998031496062994405, -1.074146981627296604 ) ) ;
#54709 = CARTESIAN_POINT ( 'NONE',  ( -1.312335958005248715, 0.2306618581243848609, 0.2411417322834645549 ) ) ;
#54710 = DIRECTION ( 'NONE',  ( 0.000000000000000000, 1.000000000000000000, -1.734723475976808327E-16 ) ) ;
#54711 = ORIENTED_EDGE ( 'NONE', *, *, #18760, .T. ) ;
#54712 = CARTESIAN_POINT ( 'NONE',  ( -1.515748031496062076, 0.07958543189024071263, -0.2665933059059888421 ) ) ;
#54713 = CARTESIAN_POINT ( 'NONE',  ( -0.5905511811023615998, 0.2952755905511811885, 0.000000000000000000 ) ) ;
#54714 = CARTESIAN_POINT ( 'NONE',  ( 0.2096960158929673246, 1.111548270248051473, 2.829355687306212008 ) ) ;
#54715 = CARTESIAN_POINT ( 'NONE',  ( -1.377952755905511140, -0.6692913385826771977, 8.415575281601705876E-17 ) ) ;
#54716 = CARTESIAN_POINT ( 'NONE',  ( 0.1049643490035304938, -0.3917322834645669549, -1.744750656167979308 ) ) ;
#54717 = CARTESIAN_POINT ( 'NONE',  ( 0.2417350488526480157, 0.3089825338611894012, -1.220472440944881942 ) ) ;
#54718 = EDGE_CURVE ( 'NONE', #70474, #17581, #77529, .T. ) ;
#54719 = CARTESIAN_POINT ( 'NONE',  ( 1.279527559055118724, -0.5400638737290845981, -0.3530559997133363437 ) ) ;
#54720 = CARTESIAN_POINT ( 'NONE',  ( 0.6692913385826778638, -0.6692913385826771977, 8.415575281601705876E-17 ) ) ;
#54721 = CARTESIAN_POINT ( 'NONE',  ( 0.5314960629921350321, 2.755905511811024056, -2.583694225513478937 ) ) ;
#54722 = CARTESIAN_POINT ( 'NONE',  ( 0.1998031496062992463, 0.3460692066303959202, -2.268372703412073754 ) ) ;
#54723 = ADVANCED_FACE ( 'NONE', ( #29211, #41425 ), #68355, .T. ) ;
#54724 = CARTESIAN_POINT ( 'NONE',  ( -1.686351706036744558, 0.2952755905511810774, -0.1292274648535930714 ) ) ;
#54725 = CARTESIAN_POINT ( 'NONE',  ( 0.3460692066303959757, -0.1998031496062991907, -0.4199475065616797842 ) ) ;
#54726 = VERTEX_POINT ( 'NONE', #35111 ) ;
#54727 = CARTESIAN_POINT ( 'NONE',  ( -0.4133858267716528645, -0.4536011799217367080, 0.2665933059059888421 ) ) ;
#54728 = CARTESIAN_POINT ( 'NONE',  ( -0.2867679344610364334, -0.2867679344610367109, -2.255905511811023612 ) ) ;
#54729 = ORIENTED_EDGE ( 'NONE', *, *, #21343, .T. ) ;
#54730 = CARTESIAN_POINT ( 'NONE',  ( 0.9317585301837276734, -0.4281496062992124485, 0.4176697321401328655 ) ) ;
#54731 = CARTESIAN_POINT ( 'NONE',  ( -0.4527559055118102749, 0.1660481256975885056, 0.3530559997133364547 ) ) ;
#54732 = CARTESIAN_POINT ( 'NONE',  ( -1.036745406824146176, -0.4281496062992124485, 0.4176697321401328655 ) ) ;
#54733 = CARTESIAN_POINT ( 'NONE',  ( 1.404199475065617708, 0.05413385826771626580, -0.4176697321401330321 ) ) ;
#54734 = CARTESIAN_POINT ( 'NONE',  ( -1.476377952755905110, 0.07958543189024085140, 0.2665933059059887866 ) ) ;
#54735 = CARTESIAN_POINT ( 'NONE',  ( -0.4744094488188880798, 1.537401574803149984, -2.554262525012305218 ) ) ;
#54736 = CARTESIAN_POINT ( 'NONE',  ( 0.2887139107611556010, 0.2306618581243847221, -0.2411417322834647770 ) ) ;
#54737 = CARTESIAN_POINT ( 'NONE',  ( -0.9251968503937002541, -0.5400638737290845981, -0.3530559997133363437 ) ) ;
#54738 = CARTESIAN_POINT ( 'NONE',  ( 0.3392501089628018329, 0.1958661417322835052, -1.471109293142045304 ) ) ;
#54739 = CARTESIAN_POINT ( 'NONE',  ( -1.069553805774277722, -0.6692913385826773087, -0.1292274648535924053 ) ) ;
#54740 = DIRECTION ( 'NONE',  ( -0.1923134147744552658, 0.6939076129059796871, 0.6939076129060073317 ) ) ;
#54741 = CARTESIAN_POINT ( 'NONE',  ( 0.8267716535433078384, -0.6692913385826771977, 8.415575281601705876E-17 ) ) ;
#54742 = CARTESIAN_POINT ( 'NONE',  ( 1.266404199475066328, -0.2845877964562161244, -0.3641732283464567121 ) ) ;
#54743 = EDGE_LOOP ( 'NONE', ( #313, #33531, #37209, #42224 ) ) ;
#54744 = CARTESIAN_POINT ( 'NONE',  ( -0.3917322834645671770, 0.1049643490035302024, -2.864192544128295825 ) ) ;
#54745 = CARTESIAN_POINT ( 'NONE',  ( -0.4068241469816264999, -0.4281496062992124485, 0.4176697321401328655 ) ) ;
#54746 = ORIENTED_EDGE ( 'NONE', *, *, #22, .T. ) ;
#54747 = CARTESIAN_POINT ( 'NONE',  ( 0.5577427821522314977, -0.2845877964562161244, -0.3641732283464567121 ) ) ;
#54748 = CARTESIAN_POINT ( 'NONE',  ( -1.430446194225721390, -0.4281496062992124485, 0.4176697321401328655 ) ) ;
#54749 = CARTESIAN_POINT ( 'NONE',  ( 0.9711286089238851948, 0.2306618581243848609, 0.2411417322834645549 ) ) ;
#54750 = CARTESIAN_POINT ( 'NONE',  ( 0.7545931758530188826, -0.6692913385826771977, 0.1292274648535927661 ) ) ;
#54751 = CARTESIAN_POINT ( 'NONE',  ( -0.2887139107611542133, 0.2306618581243848609, 0.2411417322834645549 ) ) ;
#54752 = CARTESIAN_POINT ( 'NONE',  ( -0.1049643490035302301, -0.3917322834645671770, -1.171279158301524292 ) ) ;
#54753 = CARTESIAN_POINT ( 'NONE',  ( -0.7086614173228339419, -0.1870078740157479769, 0.4822834645669291653 ) ) ;
#54754 = CARTESIAN_POINT ( 'NONE',  ( -0.1049643490035307020, 0.3917322834645669549, -2.295931758530183497 ) ) ;
#54755 = CARTESIAN_POINT ( 'NONE',  ( -1.732283464566928277, -0.1870078740157479769, 0.4822834645669291653 ) ) ;
#54756 = CARTESIAN_POINT ( 'NONE',  ( -1.069553805774277722, -0.6692913385826773087, -0.1292274648535924053 ) ) ;
#54757 = CARTESIAN_POINT ( 'NONE',  ( 1.318897637795276356, -0.5400638737290844871, 0.3530559997133364547 ) ) ;
#54758 = CARTESIAN_POINT ( 'NONE',  ( 1.692913385826772421, 0.2952755905511811885, 0.000000000000000000 ) ) ;
#54759 = CARTESIAN_POINT ( 'NONE',  ( -1.049868766404198794, 0.2306618581243847221, -0.2411417322834647770 ) ) ;
#54760 = CARTESIAN_POINT ( 'NONE',  ( 0.3460692066303958092, 0.1998031496062993018, -0.05052493438320210251 ) ) ;
#54761 = CARTESIAN_POINT ( 'NONE',  ( 0.4002624671916016896, -0.3162353388693409650, -0.4822834645669289433 ) ) ;
#54762 = CARTESIAN_POINT ( 'NONE',  ( 0.1070741851644054915, -0.3996062992125986035, -1.817585301837270517 ) ) ;
#54763 = AXIS2_PLACEMENT_3D ( 'NONE', #79049, #36369, #55710 ) ;
#54764 = CARTESIAN_POINT ( 'NONE',  ( -0.7545931758530176614, -0.6692913385826773087, -0.1292274648535924053 ) ) ;
#54765 = VECTOR ( 'NONE', #29542, 39.37007874015748143 ) ;
#54766 = CARTESIAN_POINT ( 'NONE',  ( 1.581364829396326277, -0.3162353388693409650, -0.4822834645669289433 ) ) ;
#54767 = CARTESIAN_POINT ( 'NONE',  ( 0.7742782152230979209, -0.004921259842519870586, -0.3153832671262229437 ) ) ;
#54768 = CARTESIAN_POINT ( 'NONE',  ( 1.253280839895013710, -0.3162353388693405765, 0.4822834645669290543 ) ) ;
#54769 = CARTESIAN_POINT ( 'NONE',  ( 0.2362204724409449064, 0.4091458600556404646, -0.6935695538057742304 ) ) ;
#54770 = CARTESIAN_POINT ( 'NONE',  ( 1.010498687664042716, -0.3690944881889763329, 0.3153832671262228327 ) ) ;
#54771 = CARTESIAN_POINT ( 'NONE',  ( 0.8333333333333340365, 0.2952755905511810774, -0.1292274648535930714 ) ) ;
#54772 = CARTESIAN_POINT ( 'NONE',  ( -0.3420746716998662729, 0.1974969037888702206, -0.7329396325459319739 ) ) ;
#54773 = CARTESIAN_POINT ( 'NONE',  ( -0.4724409448818890911, -0.1870078740157479769, 0.4822834645669291653 ) ) ;
#54774 = CARTESIAN_POINT ( 'NONE',  ( -0.03443470937339728616, 0.2755905511811023723, -1.537015892239756099 ) ) ;
#54775 = CARTESIAN_POINT ( 'NONE',  ( 1.279527559055118724, 0.07958543189024085140, 0.2665933059059887866 ) ) ;
#54776 = CARTESIAN_POINT ( 'NONE',  ( -0.4396325459317579898, 0.2952755905511811885, 0.1292274648535926551 ) ) ;
#54777 = CARTESIAN_POINT ( 'NONE',  ( 0.3949938075777409408, -0.1058382717557499186, -0.3458005249343832910 ) ) ;
#54778 = CARTESIAN_POINT ( 'NONE',  ( 1.476377952755906442, -0.5400638737290844871, 0.3530559997133364547 ) ) ;
#54779 = CARTESIAN_POINT ( 'NONE',  ( 0.1246719160104994284, -0.6692913385826771977, 0.1292274648535927661 ) ) ;
#54780 = CARTESIAN_POINT ( 'NONE',  ( 0.5183727034120741983, -0.5511811023622046335, 0.09757992244046803654 ) ) ;
#54781 = CARTESIAN_POINT ( 'NONE',  ( -0.03443470937339728616, 0.2755905511811023723, -1.537015892239756099 ) ) ;
#54782 = CARTESIAN_POINT ( 'NONE',  ( 0.1574803149606306130, -0.1870078740157480601, -0.3641732283464567677 ) ) ;
#54783 = CARTESIAN_POINT ( 'NONE',  ( -1.601049868766403650, 0.2306618581243847221, -0.2411417322834647770 ) ) ;
#54784 = EDGE_CURVE ( 'NONE', #17596, #24792, #47400, .T. ) ;
#54785 = CARTESIAN_POINT ( 'NONE',  ( 0.1070741851644053388, 0.3996062992125986035, -1.487532808398950301 ) ) ;
#54786 = CARTESIAN_POINT ( 'NONE',  ( 0.7808398950131241190, -0.05778040916215560624, -0.4822834645669293319 ) ) ;
#54787 = CARTESIAN_POINT ( 'NONE',  ( 0.1049643490035304938, -0.3917322834645669549, -1.179790026246718915 ) ) ;
#54788 = CARTESIAN_POINT ( 'NONE',  ( 1.594488188976378673, -0.4536011799217368745, -0.2665933059059886201 ) ) ;
#54789 = DIRECTION ( 'NONE',  ( -0.000000000000000000, 1.000000000000000000, -0.000000000000000000 ) ) ;
#54790 = CARTESIAN_POINT ( 'NONE',  ( -0.08530183727034056085, -0.08942795157528024563, -0.3641732283464568787 ) ) ;
#54791 = CARTESIAN_POINT ( 'NONE',  ( 0.01312335958005323398, -0.4281496062992127816, -0.4176697321401328100 ) ) ;
#54792 = CARTESIAN_POINT ( 'NONE',  ( 1.555118110236221041, 0.07958543189024071263, -0.2665933059059888421 ) ) ;
#54793 = CARTESIAN_POINT ( 'NONE',  ( -1.358267716535432434, 0.07958543189024071263, -0.2665933059059888421 ) ) ;
#54794 = CARTESIAN_POINT ( 'NONE',  ( -1.601049868766403650, -0.6046776061558807314, 0.2411417322834647770 ) ) ;
#54795 = CARTESIAN_POINT ( 'NONE',  ( 0.6561679790026253567, -0.6046776061558809534, -0.2411417322834644161 ) ) ;
#54796 = CARTESIAN_POINT ( 'NONE',  ( 1.207349081364829990, 0.2306618581243848609, 0.2411417322834645549 ) ) ;
#54797 = CARTESIAN_POINT ( 'NONE',  ( -3.937007874015748143, 2.755905511811024056, 0.5314960629921260393 ) ) ;
#54798 = CARTESIAN_POINT ( 'NONE',  ( 0.07874015748031558404, -0.1870078740157480879, -0.4822834645669291653 ) ) ;
#54799 = CARTESIAN_POINT ( 'NONE',  ( 1.397637795275591177, 0.1660481256975883668, -0.3530559997133364547 ) ) ;
#54800 = CARTESIAN_POINT ( 'NONE',  ( 1.181102362204725198, -0.1870078740157479769, 0.4822834645669291653 ) ) ;
#54801 = LINE ( 'NONE', #10617, #19917 ) ;
#54802 = CARTESIAN_POINT ( 'NONE',  ( 0.6955380577427828781, -0.3690944881889763329, 0.3153832671262228327 ) ) ;
#54803 = CARTESIAN_POINT ( 'NONE',  ( 1.541994750656168645, 0.2952755905511810774, -0.1292274648535930714 ) ) ;
#54804 = CARTESIAN_POINT ( 'NONE',  ( -0.07217847769028813698, -0.2845877964562161244, -0.3641732283464567121 ) ) ;
#54805 = CARTESIAN_POINT ( 'NONE',  ( -0.03280839895013062252, 0.2952755905511810774, -0.1292274648535930714 ) ) ;
#54806 = CARTESIAN_POINT ( 'NONE',  ( 0.7808398950131240079, -0.3162353388693405765, 0.4822834645669290543 ) ) ;
#54807 = CARTESIAN_POINT ( 'NONE',  ( -0.3018372703412066094, -0.4281496062992127816, -0.4176697321401328100 ) ) ;
#54808 = CARTESIAN_POINT ( 'NONE',  ( -0.2559055118110230564, 0.07958543189024071263, -0.2665933059059888421 ) ) ;
#54809 = CARTESIAN_POINT ( 'NONE',  ( 0.7874015748031503170, -0.1870078740157479769, 0.4822834645669291653 ) ) ;
#54810 = CARTESIAN_POINT ( 'NONE',  ( 0.8464566929133866546, -0.4536011799217367080, 0.2665933059059888421 ) ) ;
#54811 =( BOUNDED_CURVE ( )  B_SPLINE_CURVE ( 2, ( #41608, #16787, #67297, #60963, #62205, #4542, #42424, #16370, #73619, #79522, #21837, #47500, #73193 ),
 .UNSPECIFIED., .F., .F. ) 
 B_SPLINE_CURVE_WITH_KNOTS ( ( 3, 2, 2, 2, 2, 2, 3 ),
 ( 0.3624999999999999889, 0.3666666666666666408, 0.3708333333333333481, 0.3750000000000000000, 0.3791666666666666519, 0.3833333333333333592, 0.3875000000000000111 ),
 .UNSPECIFIED. ) 
 CURVE ( )  GEOMETRIC_REPRESENTATION_ITEM ( )  RATIONAL_B_SPLINE_CURVE ( ( 1.000000000000000000, 0.9659258262890683122, 1.000000000000000000, 0.9659258262890683122, 1.000000000000000000, 0.9659258262890683122, 1.000000000000000000, 0.9659258262890683122, 1.000000000000000000, 0.9659258262890683122, 1.000000000000000000, 0.9659258262890683122, 1.000000000000000000 ) ) 
 REPRESENTATION_ITEM ( '' )  );
#54812 = EDGE_CURVE ( 'NONE', #19838, #74748, #4615, .T. ) ;
#54813 = FACE_OUTER_BOUND ( 'NONE', #72622, .T. ) ;
#54815 = CARTESIAN_POINT ( 'NONE',  ( 0.3996062992125986035, -0.1070741851644053111, -1.056430446194225770 ) ) ;
#54814 = CARTESIAN_POINT ( 'NONE',  ( 0.3307086614173228023, 0.000000000000000000, 0.000000000000000000 ) ) ;
#54816 = CARTESIAN_POINT ( 'NONE',  ( 2.152447471807405588, 1.622068519643040663, -0.4668652553835656027 ) ) ;
#54817 = CIRCLE ( 'NONE', #60241, 1.220472440944881942 ) ;
#54818 = CARTESIAN_POINT ( 'NONE',  ( -1.345144356955379816, -0.3162353388693405765, 0.4822834645669290543 ) ) ;
#54819 = CARTESIAN_POINT ( 'NONE',  ( -0.3543307086614165824, -0.6692913385826771977, 8.415575281601705876E-17 ) ) ;
#54820 = CARTESIAN_POINT ( 'NONE',  ( 0.3458507752293908943, -0.3458507752293908943, 0.05905511811023620578 ) ) ;
#54821 = CARTESIAN_POINT ( 'NONE',  ( 0.1058382717557499880, 0.3949938075777411073, -2.513123359580052174 ) ) ;
#54822 = EDGE_LOOP ( 'NONE', ( #68927, #63360, #5851, #3289 ) ) ;
#54823 = CARTESIAN_POINT ( 'NONE',  ( 0.7283464566929143125, 0.07958543189024085140, 0.2665933059059887866 ) ) ;
#54824 = CARTESIAN_POINT ( 'NONE',  ( 0.3392501089628018329, 0.1958661417322835607, -0.7532808398950130435 ) ) ;
#54825 = CARTESIAN_POINT ( 'NONE',  ( 0.9711286089238851948, 0.2306618581243848609, 0.2411417322834645549 ) ) ;
#54826 = CARTESIAN_POINT ( 'NONE',  ( -0.1265901696524986964, -0.4724409448818899238, -2.276902887139107268 ) ) ;
#54827 = CARTESIAN_POINT ( 'NONE',  ( 3.900447471620230200, 2.687524476698323284, -0.5314960629921260393 ) ) ;
#54828 = CARTESIAN_POINT ( 'NONE',  ( -1.568241469816272105, -0.08942795157527998196, 0.3641732283464567121 ) ) ;
#54829 = DIRECTION ( 'NONE',  ( -1.000000000000000000, -3.412570772413390973E-16, 0.000000000000000000 ) ) ;
#54830 = CARTESIAN_POINT ( 'NONE',  ( 1.496062992125984703, -0.1870078740157480601, -0.3641732283464567677 ) ) ;
#54831 = CARTESIAN_POINT ( 'NONE',  ( 0.6233595800524942554, -0.05778040916215560624, -0.4822834645669293319 ) ) ;
#54832 = CARTESIAN_POINT ( 'NONE',  ( -0.2867679344610366554, 0.2867679344610365444, -0.09971821702655986330 ) ) ;
#54833 = CARTESIAN_POINT ( 'NONE',  ( 0.2230971128608932319, -0.4281496062992124485, 0.4176697321401328655 ) ) ;
#54834 = CARTESIAN_POINT ( 'NONE',  ( -0.8727034120734901146, -0.08942795157528024563, -0.3641732283464568787 ) ) ;
#54835 = CARTESIAN_POINT ( 'NONE',  ( 0.8202099737532813073, 0.2952755905511811885, 0.1292274648535926551 ) ) ;
#54836 = CARTESIAN_POINT ( 'NONE',  ( -0.2230971128608915943, -0.4281496062992127816, -0.4176697321401328100 ) ) ;
#54837 = CARTESIAN_POINT ( 'NONE',  ( 0.4824498642376759960, 1.223219560026271499E-15, 0.4445507791589056734 ) ) ;
#54838 = CARTESIAN_POINT ( 'NONE',  ( -0.01069919276010446348, 1.490381362800744269E-15, -0.4118477457932981367 ) ) ;
#54839 = CARTESIAN_POINT ( 'NONE',  ( 0.3917322834645670659, 2.398668435337828261E-17, -1.532171546752967739 ) ) ;
#54840 = CARTESIAN_POINT ( 'NONE',  ( 0.7545931758530189937, 0.2952755905511810774, -0.1292274648535930714 ) ) ;
#54841 = CARTESIAN_POINT ( 'NONE',  ( 0.01968503937007930540, 0.1660481256975885056, 0.3530559997133364547 ) ) ;
#54842 = CARTESIAN_POINT ( 'NONE',  ( -1.003937007874014853, 0.1660481256975885056, 0.3530559997133364547 ) ) ;
#54843 = ADVANCED_FACE ( 'NONE', ( #48973 ), #17580, .T. ) ;
#54844 = CARTESIAN_POINT ( 'NONE',  ( 0.9645669291338588858, 0.1660481256975885056, 0.3530559997133364547 ) ) ;
#54845 = CARTESIAN_POINT ( 'NONE',  ( 0.2821522309711292364, 0.2952755905511810774, -0.1292274648535930714 ) ) ;
#54846 = CARTESIAN_POINT ( 'NONE',  ( -0.1049643490035302024, -0.3917322834645671215, -1.101706036745407014 ) ) ;
#54847 = CARTESIAN_POINT ( 'NONE',  ( -0.4199475065616791736, 0.2306618581243847221, -0.2411417322834647770 ) ) ;
#54848 = CARTESIAN_POINT ( 'NONE',  ( 0.5511811023622055217, -0.1870078740157479769, 0.4822834645669291653 ) ) ;
#54849 = CARTESIAN_POINT ( 'NONE',  ( -0.01968503937007793844, 0.1660481256975883668, -0.3530559997133364547 ) ) ;
#54850 = EDGE_CURVE ( 'NONE', #25851, #38370, #63498, .T. ) ;
#54851 = CARTESIAN_POINT ( 'NONE',  ( 0.5839895013123367340, 0.1771653543307087630, 0.09757992244046791164 ) ) ;
#54852 = CARTESIAN_POINT ( 'NONE',  ( -1.581364829396324945, -0.3162353388693405765, 0.4822834645669290543 ) ) ;
#54853 = CARTESIAN_POINT ( 'NONE',  ( -0.4258029703577156933, 1.326239216270301391, -2.646999490626495977 ) ) ;
#54854 = CARTESIAN_POINT ( 'NONE',  ( 0.3740157480314966754, 0.1660481256975883668, -0.3530559997133364547 ) ) ;
#54855 = CARTESIAN_POINT ( 'NONE',  ( 0.1049643490035303689, 0.3917322834645670104, -2.505249343832020248 ) ) ;
#54856 = EDGE_LOOP ( 'NONE', ( #7035, #70983, #67208, #9209 ) ) ;
#54857 = VERTEX_POINT ( 'NONE', #8995 ) ;
#54858 = CARTESIAN_POINT ( 'NONE',  ( 0.8398950131233602345, -0.6046776061558807314, 0.2411417322834647770 ) ) ;
#54859 = CARTESIAN_POINT ( 'NONE',  ( 0.6758530183727039509, 0.1771653543307087075, -0.09757992244046823083 ) ) ;
#54861 = CARTESIAN_POINT ( 'NONE',  ( -0.1938976377952756625, 0.1938976377952755792, 0.1574803149606299191 ) ) ;
#54860 = CARTESIAN_POINT ( 'NONE',  ( -1.016821367227983774, 1.553543944314659475, 0.4744094488188969616 ) ) ;
#54862 = CARTESIAN_POINT ( 'NONE',  ( -0.2867679344610364334, -0.2867679344610367109, -0.9311023622047245318 ) ) ;
#54863 = CARTESIAN_POINT ( 'NONE',  ( -0.4422825626179747727, 1.709752412933176258, 3.912091147757427390 ) ) ;
#54864 = CARTESIAN_POINT ( 'NONE',  ( -0.03443470937339728616, 1.062992125984252079, -1.635441089090149402 ) ) ;
#54865 = CARTESIAN_POINT ( 'NONE',  ( -0.1958661417322834220, -0.3392501089628018884, -1.252624671916010568 ) ) ;
#54866 = CARTESIAN_POINT ( 'NONE',  ( -9.787531504996566615E-17, 0.3996062992125985480, -2.596456692913385655 ) ) ;
#54867 = CARTESIAN_POINT ( 'NONE',  ( 0.9908136482939640111, 0.2952755905511810774, -0.1292274648535930714 ) ) ;
#54868 = CARTESIAN_POINT ( 'NONE',  ( -1.017060367454067249, -0.05778040916215522460, 0.4822834645669289988 ) ) ;
#54869 = CARTESIAN_POINT ( 'NONE',  ( -0.8398950131233589023, -0.6046776061558809534, -0.2411417322834644161 ) ) ;
#54870 = CARTESIAN_POINT ( 'NONE',  ( 0.7414698162729663755, -0.6692913385826773087, -0.1292274648535924053 ) ) ;
#54871 = CARTESIAN_POINT ( 'NONE',  ( 1.207349081364829990, -0.6046776061558809534, -0.2411417322834644161 ) ) ;
#54872 = CARTESIAN_POINT ( 'NONE',  ( -1.122048159108791632, 1.062989961842522035, -0.01571064279740208569 ) ) ;
#54873 = APPLICATION_PROTOCOL_DEFINITION ( 'draft international standard', 'automotive_design', 1998, #32577 ) ;
#54874 = CARTESIAN_POINT ( 'NONE',  ( 1.272965879265092637, -0.3690944881889765550, -0.3153832671262227771 ) ) ;
#54875 = CARTESIAN_POINT ( 'NONE',  ( -0.3460692066303957537, -0.1998031496062994405, -2.176509186351706315 ) ) ;
#54876 = CARTESIAN_POINT ( 'NONE',  ( -1.463254593175852492, 0.1771653543307087630, 0.09757992244046791164 ) ) ;
#54877 = CARTESIAN_POINT ( 'NONE',  ( -0.1958661417322836718, 0.3392501089628017219, 0.1522309711286089495 ) ) ;
#54878 = CARTESIAN_POINT ( 'NONE',  ( 0.1574803149606306130, -0.1870078740157480879, -0.4822834645669291653 ) ) ;
#54879 = VECTOR ( 'NONE', #47678, 39.37007874015748143 ) ;
#54881 = CARTESIAN_POINT ( 'NONE',  ( -3.909100906889131810, 1.617089521489746273, -0.4679440794864275222 ) ) ;
#54880 = CARTESIAN_POINT ( 'NONE',  ( 1.522309711286089939, 0.2306618581243848609, 0.2411417322834645549 ) ) ;
#54882 = CARTESIAN_POINT ( 'NONE',  ( -0.9711286089238838626, -0.5023911411419708095, 0.1820866141732285504 ) ) ;
#54883 = CARTESIAN_POINT ( 'NONE',  ( 0.1968503937007881344, -0.6692913385826771977, 8.415575281601705876E-17 ) ) ;
#54884 = CARTESIAN_POINT ( 'NONE',  ( 1.187664041994751285, -0.2845877964562161244, -0.3641732283464567121 ) ) ;
#54885 = CARTESIAN_POINT ( 'NONE',  ( -0.3917322834645668994, -0.1049643490035306742, -1.070846825950444448 ) ) ;
#54886 = CARTESIAN_POINT ( 'NONE',  ( -1.023622047244094002, -0.1870078740157480601, -0.3641732283464567677 ) ) ;
#54887 = CARTESIAN_POINT ( 'NONE',  ( 1.463254593175853824, -0.6692913385826771977, 0.1292274648535927661 ) ) ;
#54888 = DIRECTION ( 'NONE',  ( 0.000000000000000000, 1.000000000000000000, -0.000000000000000000 ) ) ;
#54889 = CARTESIAN_POINT ( 'NONE',  ( -0.1509186351706028884, -0.05778040916215522460, 0.4822834645669289988 ) ) ;
#54890 = CARTESIAN_POINT ( 'NONE',  ( -1.423884514435694859, -0.08942795157528024563, -0.3641732283464568787 ) ) ;
#54891 = CARTESIAN_POINT ( 'NONE',  ( -0.5905511811023615998, 0.2952755905511811885, 0.000000000000000000 ) ) ;
#54892 = CARTESIAN_POINT ( 'NONE',  ( -1.653543307086613234, -0.1870078740157479769, 0.3641732283464567677 ) ) ;
#54893 = CARTESIAN_POINT ( 'NONE',  ( -0.1958661417322836995, 0.3392501089628017219, -0.4823027803487682785 ) ) ;
#54894 = CARTESIAN_POINT ( 'NONE',  ( 0.1509186351706042484, -0.3162353388693405765, 0.4822834645669290543 ) ) ;
#54895 = CARTESIAN_POINT ( 'NONE',  ( 0.4091458600556403535, 0.2362204724409449896, -2.097769028871391050 ) ) ;
#54896 = CARTESIAN_POINT ( 'NONE',  ( -1.384514435695537005, 0.2952755905511811885, 0.1292274648535926551 ) ) ;
#54897 = CARTESIAN_POINT ( 'NONE',  ( -0.7020997375328076329, -0.2845877964562161244, -0.3641732283464567121 ) ) ;
#54898 = CARTESIAN_POINT ( 'NONE',  ( -0.4855643044619415427, 0.009842519685039147898, -0.3409548833797004797 ) ) ;
#54899 = CARTESIAN_POINT ( 'NONE',  ( -0.03280839895013062252, 0.2952755905511810774, -0.1292274648535930714 ) ) ;
#54900 = CARTESIAN_POINT ( 'NONE',  ( 0.5839895013123367340, 0.1771653543307087630, 0.09757992244046791164 ) ) ;
#54901 = CARTESIAN_POINT ( 'NONE',  ( -1.246719160104986512, -0.004921259842519576551, 0.3153832671262227771 ) ) ;
#54902 = CARTESIAN_POINT ( 'NONE',  ( -1.607611548556429737, -0.6692913385826771977, 0.1292274648535927661 ) ) ;
#54903 = CARTESIAN_POINT ( 'NONE',  ( -1.437007874015747477, -0.5400638737290844871, 0.3530559997133364547 ) ) ;
#54904 = CARTESIAN_POINT ( 'NONE',  ( 1.561679790026247350, 0.05413385826771626580, -0.4176697321401330321 ) ) ;
#54905 = CARTESIAN_POINT ( 'NONE',  ( -0.4724409448818917001, 0.1265901696524956710, -2.156824146981627610 ) ) ;
#54906 = CARTESIAN_POINT ( 'NONE',  ( 0.3937007874015754361, -0.1870078740157479769, 0.3641732283464567677 ) ) ;
#54907 = CARTESIAN_POINT ( 'NONE',  ( 0.7677165354330716118, 0.1660481256975883668, -0.3530559997133364547 ) ) ;
#54908 = LINE ( 'NONE', #28410, #34015 ) ;
#54909 = CARTESIAN_POINT ( 'NONE',  ( 1.404199475065617264, -0.3690944881889763329, 0.3153832671262228327 ) ) ;
#54910 = ORIENTED_EDGE ( 'NONE', *, *, #76274, .T. ) ;
#54911 = CARTESIAN_POINT ( 'NONE',  ( -1.154855643044618851, 0.2306618581243848609, 0.2411417322834645549 ) ) ;
#54912 = CARTESIAN_POINT ( 'NONE',  ( -0.6889763779527552368, 0.1660481256975885056, 0.3530559997133364547 ) ) ;
#54913 = CARTESIAN_POINT ( 'NONE',  ( 0.3018372703412079971, -0.4281496062992124485, 0.4176697321401328655 ) ) ;
#54914 = CARTESIAN_POINT ( 'NONE',  ( -0.3996062992125986035, -7.340648628747425578E-17, -0.03937007874015750059 ) ) ;
#54915 = CARTESIAN_POINT ( 'NONE',  ( -0.2925321140481930149, -0.2925321140481933480, -2.025590551181102317 ) ) ;
#54916 = CARTESIAN_POINT ( 'NONE',  ( 0.9186351706036751663, -0.6046776061558807314, 0.2411417322834647770 ) ) ;
#54917 = CARTESIAN_POINT ( 'NONE',  ( -1.706036745406823485, 0.2306618581243848609, 0.2411417322834645549 ) ) ;
#54918 = CARTESIAN_POINT ( 'NONE',  ( 0.5839895013123367340, 0.2952755905511811885, 0.1292274648535926551 ) ) ;
#54919 = CARTESIAN_POINT ( 'NONE',  ( 0.6102362204724416372, -0.5400638737290844871, 0.3530559997133364547 ) ) ;
#54920 = CARTESIAN_POINT ( 'NONE',  ( -0.2925321140481930704, -0.2925321140481933480, -1.948818897637795144 ) ) ;
#54921 = CARTESIAN_POINT ( 'NONE',  ( 0.3420746716998659953, 0.1974969037888705536, -1.233595800524934338 ) ) ;
#54922 = CARTESIAN_POINT ( 'NONE',  ( -0.2925321140481930704, -0.2925321140481933480, -2.263779527559055094 ) ) ;
#54923 = CARTESIAN_POINT ( 'NONE',  ( -0.1321325610835860087, -0.2642592750917004407, 0.1571896754257856577 ) ) ;
#54924 = CARTESIAN_POINT ( 'NONE',  ( 0.3917322834645669549, 0.1049643490035304660, -0.1167979002624671414 ) ) ;
#54925 = CARTESIAN_POINT ( 'NONE',  ( 0.05249343832021075018, 0.1283753931104746893, -0.1820866141732285504 ) ) ;
#54926 = CARTESIAN_POINT ( 'NONE',  ( -0.3018372703412066094, 0.05413385826771666132, 0.4176697321401328100 ) ) ;
#54927 = CARTESIAN_POINT ( 'NONE',  ( 0.9973753280839902091, 0.2306618581243847221, -0.2411417322834647770 ) ) ;
#54928 = CARTESIAN_POINT ( 'NONE',  ( -0.3949938075777408852, -0.1058382717557502933, -2.169947506561679784 ) ) ;
#54929 = CARTESIAN_POINT ( 'NONE',  ( -0.1312335958005241554, -0.5023911411419708095, -0.1820866141732282451 ) ) ;
#54930 = CARTESIAN_POINT ( 'NONE',  ( -1.135170603674539924, 0.2952755905511810774, -0.1292274648535930714 ) ) ;
#54931 = CARTESIAN_POINT ( 'NONE',  ( 1.404199475065617264, -0.4281496062992124485, 0.4176697321401328655 ) ) ;
#54932 = CARTESIAN_POINT ( 'NONE',  ( 0.4091458600556403535, 0.2362204724409449896, -2.650918635170603554 ) ) ;
#54933 = CARTESIAN_POINT ( 'NONE',  ( 0.1070741851644053527, 0.3996062992125986590, -1.725721784776903078 ) ) ;
#54934 = CARTESIAN_POINT ( 'NONE',  ( 0.3458507752293908943, 0.3458507752293908943, -2.734251968503936592 ) ) ;
#54935 = ADVANCED_FACE ( 'NONE', ( #22855 ), #18090, .F. ) ;
#54936 = ORIENTED_EDGE ( 'NONE', *, *, #19337, .F. ) ;
#54937 = CARTESIAN_POINT ( 'NONE',  ( 0.9186351706036751663, -0.6046776061558807314, 0.2411417322834647770 ) ) ;
#54938 = CARTESIAN_POINT ( 'NONE',  ( 1.404199475065617264, -0.3690944881889763329, 0.3153832671262228327 ) ) ;
#54940 = CARTESIAN_POINT ( 'NONE',  ( 1.555118110236221041, -0.5400638737290844871, 0.3530559997133364547 ) ) ;
#54939 = CARTESIAN_POINT ( 'NONE',  ( 1.535433070866142558, 0.2952755905511811885, 0.000000000000000000 ) ) ;
#54941 = CARTESIAN_POINT ( 'NONE',  ( -0.1049643490035302024, -0.3917322834645671215, 0.1581364829396324501 ) ) ;
#54942 = CARTESIAN_POINT ( 'NONE',  ( 0.4709442531824356015, 0.03757601356358734185, -1.929133858267717549 ) ) ;
#54943 = CARTESIAN_POINT ( 'NONE',  ( 1.272965879265092637, -0.4281496062992127816, -0.4176697321401328100 ) ) ;
#54944 = CARTESIAN_POINT ( 'NONE',  ( 0.1265901696524990572, -0.4724409448818897017, -2.447506561679789527 ) ) ;
#54945 = CARTESIAN_POINT ( 'NONE',  ( -0.07217847769028813698, -0.3162353388693409650, -0.4822834645669289433 ) ) ;
#54946 = CARTESIAN_POINT ( 'NONE',  ( -0.6102362204724400829, 0.1660481256975885056, 0.3530559997133364547 ) ) ;
#54947 = CARTESIAN_POINT ( 'NONE',  ( -1.509186351706035767, -0.4281496062992124485, 0.4176697321401328655 ) ) ;
#54948 = CARTESIAN_POINT ( 'NONE',  ( 0.1958661417322836440, -0.3392501089628017219, -0.1765091863517061210 ) ) ;
#54949 = CARTESIAN_POINT ( 'NONE',  ( 0.2690288713910767848, -0.6692913385826773087, -0.1292274648535924053 ) ) ;
#54950 = CARTESIAN_POINT ( 'NONE',  ( -0.1049643490035302024, -0.3917322834645671215, -2.426509186351705427 ) ) ;
#54951 = CARTESIAN_POINT ( 'NONE',  ( 1.535433070866142558, 0.2952755905511811885, 0.000000000000000000 ) ) ;
#54952 = ORIENTED_EDGE ( 'NONE', *, *, #39809, .T. ) ;
#54953 = CARTESIAN_POINT ( 'NONE',  ( -0.3949938075777409408, -0.1058382717557502933, -2.723097112860892732 ) ) ;
#54954 = ORIENTED_EDGE ( 'NONE', *, *, #65662, .F. ) ;
#54955 = CARTESIAN_POINT ( 'NONE',  ( -2.154527559055114061, 0.03937007874015747977, -0.4677827689125148014 ) ) ;
#54956 = CARTESIAN_POINT ( 'NONE',  ( 1.607611548556431069, 0.1771653543307087630, 0.09757992244046791164 ) ) ;
#54957 = CARTESIAN_POINT ( 'NONE',  ( 0.3996062992125986035, 0.1070741851644054776, -0.9120734908136483021 ) ) ;
#54958 = DIRECTION ( 'NONE',  ( 0.000000000000000000, 1.000000000000000000, 0.000000000000000000 ) ) ;
#54959 = CARTESIAN_POINT ( 'NONE',  ( 0.2362204724409451007, -0.4091458600556402980, -0.7985564304461942875 ) ) ;
#54960 = CARTESIAN_POINT ( 'NONE',  ( 0.4624320255261049062, 8.471767977567108961E-16, -0.4445507791589058955 ) ) ;
#54961 = CARTESIAN_POINT ( 'NONE',  ( 1.614173228346456712, 2.401574803149606474, -0.1372047244094476703 ) ) ;
#54962 = CARTESIAN_POINT ( 'NONE',  ( -0.2867679344610364334, -0.2867679344610367109, 0.01377952755905502598 ) ) ;
#54963 = CARTESIAN_POINT ( 'NONE',  ( -0.1706036745406816491, -0.004921259842519870586, -0.3153832671262229437 ) ) ;
#54964 = CARTESIAN_POINT ( 'NONE',  ( -1.299212598425196097, -0.5511811023622047445, 6.969142054262312111E-17 ) ) ;
#54965 = CARTESIAN_POINT ( 'NONE',  ( -1.030183727034119867, -0.3162353388693405765, 0.4822834645669290543 ) ) ;
#54966 = CARTESIAN_POINT ( 'NONE',  ( 0.6627296587926515548, 0.2952755905511811885, 0.1292274648535926551 ) ) ;
#54967 = CARTESIAN_POINT ( 'NONE',  ( -1.135170603674539924, 0.2952755905511810774, -0.1292274648535930714 ) ) ;
#54968 = CARTESIAN_POINT ( 'NONE',  ( 0.3917322834645670104, 2.398668435337828261E-17, 0.04724409448818902429 ) ) ;
#54969 = ORIENTED_EDGE ( 'NONE', *, *, #57249, .T. ) ;
#54970 = CARTESIAN_POINT ( 'NONE',  ( -1.358267716535432434, -0.5400638737290844871, 0.3530559997133364547 ) ) ;
#54971 = CARTESIAN_POINT ( 'NONE',  ( 0.000000000000000000, 0.000000000000000000, -2.755905511811024056 ) ) ;
#54972 = CARTESIAN_POINT ( 'NONE',  ( -0.3458507752293906723, -0.3458507752293910609, -1.633858267716534973 ) ) ;
#54973 = DIRECTION ( 'NONE',  ( -0.000000000000000000, -1.000000000000000000, -0.000000000000000000 ) ) ;
#54974 = CARTESIAN_POINT ( 'NONE',  ( -0.1049643490035307020, 0.3917322834645669549, -0.7860892388451442558 ) ) ;
#54975 = CARTESIAN_POINT ( 'NONE',  ( 0.09156050430091122738, 0.3808816823641256732, -2.755905511811024056 ) ) ;
#54976 = CARTESIAN_POINT ( 'NONE',  ( -0.7414698162729651543, -0.6692913385826771977, 0.1292274648535927661 ) ) ;
#54977 = CARTESIAN_POINT ( 'NONE',  ( 1.528871391076116026, 0.2952755905511811885, 0.1292274648535926551 ) ) ;
#54979 = FACE_OUTER_BOUND ( 'NONE', #61226, .T. ) ;
#54978 = CARTESIAN_POINT ( 'NONE',  ( -1.574803149606298636, -0.1870078740157479769, 0.4822834645669291653 ) ) ;
#54980 = CARTESIAN_POINT ( 'NONE',  ( 1.502624671916010790, -0.05778040916215522460, 0.4822834645669289988 ) ) ;
#54981 = CARTESIAN_POINT ( 'NONE',  ( -0.8005249343832013809, -0.4281496062992124485, 0.4176697321401328655 ) ) ;
#54982 = CARTESIAN_POINT ( 'NONE',  ( 0.1958661417322836162, -0.3392501089628018329, -0.01441637975621864153 ) ) ;
#54983 = CARTESIAN_POINT ( 'NONE',  ( -0.1377952755905504645, 0.07958543189024085140, 0.2665933059059887866 ) ) ;
#54984 = CARTESIAN_POINT ( 'NONE',  ( -0.3392501089628017219, -0.1958661417322836718, -0.2946194225721785465 ) ) ;
#54985 = CARTESIAN_POINT ( 'NONE',  ( -0.2165354330708654795, 0.07958543189024085140, 0.2665933059059887866 ) ) ;
#54986 = CARTESIAN_POINT ( 'NONE',  ( 0.8267716535433077274, 0.1771653543307087630, 0.000000000000000000 ) ) ;
#54987 = CARTESIAN_POINT ( 'NONE',  ( 0.4724409448818904789, -0.1870078740157479769, 0.4822834645669291653 ) ) ;
#54988 = CARTESIAN_POINT ( 'NONE',  ( -0.3937007874015740483, -0.1870078740157479769, 0.3641732283464567677 ) ) ;
#54989 = CARTESIAN_POINT ( 'NONE',  ( 0.3917322834645670104, 2.398668435337828261E-17, -2.472440944881889813 ) ) ;
#54990 = CARTESIAN_POINT ( 'NONE',  ( 1.614173228346457378, 0.2952755905511811885, 0.000000000000000000 ) ) ;
#54991 = CARTESIAN_POINT ( 'NONE',  ( -1.463254593175852492, 0.1771653543307087630, 0.09757992244046791164 ) ) ;
#54992 = CARTESIAN_POINT ( 'NONE',  ( -0.3458507752293909498, 0.3458507752293907833, -0.8838582677165351953 ) ) ;
#54993 = CARTESIAN_POINT ( 'NONE',  ( 0.07874015748031558404, -0.1870078740157480879, -0.4822834645669291653 ) ) ;
#54994 = CARTESIAN_POINT ( 'NONE',  ( -0.3149606299212590610, -0.1870078740157480879, -0.4822834645669291653 ) ) ;
#54995 = CARTESIAN_POINT ( 'NONE',  ( -2.543486866223389153, 2.716535433070866645, 0.5314960629921260393 ) ) ;
#54996 = CARTESIAN_POINT ( 'NONE',  ( 0.07217847769028949700, -0.08942795157528024563, -0.3641732283464568787 ) ) ;
#54997 = CARTESIAN_POINT ( 'NONE',  ( -0.4199475065616791736, 0.2306618581243847221, -0.2411417322834647770 ) ) ;
#54998 = CARTESIAN_POINT ( 'NONE',  ( -0.5643044619422565855, -0.4281496062992124485, 0.4176697321401328655 ) ) ;
#54999 = CARTESIAN_POINT ( 'NONE',  ( 1.572991167713778227, 1.535433070866141447, 0.1227090857360984416 ) ) ;
#55000 = CARTESIAN_POINT ( 'NONE',  ( -0.7478466213799872531, 2.204724409448818978, 0.5309055118110236338 ) ) ;
#55001 = CARTESIAN_POINT ( 'NONE',  ( 0.1509186351706045259, -0.05778040916215560624, -0.4822834645669293319 ) ) ;
#55002 = ORIENTED_EDGE ( 'NONE', *, *, #11630, .F. ) ;
#55003 = CARTESIAN_POINT ( 'NONE',  ( -0.3996062992125986590, 0.1070741851644051723, -1.841863517060367439 ) ) ;
#55004 = CARTESIAN_POINT ( 'NONE',  ( -0.3149606299212590610, -0.1870078740157479769, 0.3641732283464567677 ) ) ;
#55005 = CARTESIAN_POINT ( 'NONE',  ( -0.4724409448818890911, -0.1870078740157479769, 0.4822834645669291653 ) ) ;
#55006 = CARTESIAN_POINT ( 'NONE',  ( 1.660104986876641320, -0.05778040916215522460, 0.4822834645669289988 ) ) ;
#55007 = CARTESIAN_POINT ( 'NONE',  ( 1.325459317585302665, -0.4281496062992124485, 0.4176697321401328655 ) ) ;
#55008 = CARTESIAN_POINT ( 'NONE',  ( -1.450131233595799651, 0.2952755905511810774, -0.1292274648535930714 ) ) ;
#55009 = CARTESIAN_POINT ( 'NONE',  ( -0.8464566929133852113, -0.4536011799217368745, -0.2665933059059886201 ) ) ;
#55010 = CARTESIAN_POINT ( 'NONE',  ( 0.3460692066303958092, 0.1998031496062993018, -0.2080052493438320771 ) ) ;
#55011 = CARTESIAN_POINT ( 'NONE',  ( 0.1070741851644054915, -0.3996062992125986035, -0.4002624671916010235 ) ) ;
#55012 = CARTESIAN_POINT ( 'NONE',  ( -0.3392501089628019995, 0.1958661417322831999, -2.857630864338269738 ) ) ;
#55013 = CARTESIAN_POINT ( 'NONE',  ( 1.463254593175853824, -0.5511811023622046335, 0.09757992244046803654 ) ) ;
#55014 = CARTESIAN_POINT ( 'NONE',  ( 1.141732283464567566, 0.1771653543307087630, 0.000000000000000000 ) ) ;
#55015 = CARTESIAN_POINT ( 'NONE',  ( 0.9251968503937015864, -0.5400638737290844871, 0.3530559997133364547 ) ) ;
#55016 = CARTESIAN_POINT ( 'NONE',  ( 0.4527559055118117182, 0.1012011053420775880, -0.2882089793578256898 ) ) ;
#55017 = CARTESIAN_POINT ( 'NONE',  ( 0.7480314960629927956, -0.6692913385826771977, 8.415575281601705876E-17 ) ) ;
#55018 = CARTESIAN_POINT ( 'NONE',  ( 0.1058382717557499880, 0.3949938075777409408, -0.8576115485564304031 ) ) ;
#55019 = CARTESIAN_POINT ( 'NONE',  ( 1.299212598425197429, -0.5511811023622047445, 6.969142054262312111E-17 ) ) ;
#55020 = ADVANCED_FACE ( 'NONE', ( #36309 ), #26119, .T. ) ;
#55021 = CARTESIAN_POINT ( 'NONE',  ( 0.3018372703412079971, 0.05413385826771626580, -0.4176697321401330321 ) ) ;
#55022 = CARTESIAN_POINT ( 'NONE',  ( -0.7939632545931750718, -0.05778040916215560624, -0.4822834645669293319 ) ) ;
#55023 = CARTESIAN_POINT ( 'NONE',  ( 1.272965879265092637, -0.4281496062992127816, -0.4176697321401328100 ) ) ;
#55024 = CARTESIAN_POINT ( 'NONE',  ( 0.3458507752293908943, 0.3458507752293908943, -1.082677165354330562 ) ) ;
#55025 = CARTESIAN_POINT ( 'NONE',  ( -0.2925321140481930704, -0.2925321140481933480, -2.421259842519684735 ) ) ;
#55026 = CARTESIAN_POINT ( 'NONE',  ( 0.5052493438320215802, 0.1771653543307087630, 0.09757992244046791164 ) ) ;
#55027 = ORIENTED_EDGE ( 'NONE', *, *, #15607, .F. ) ;
#55028 = CARTESIAN_POINT ( 'NONE',  ( 0.1049643490035303967, 0.3917322834645670659, -0.6200980559393196589 ) ) ;
#55029 = ORIENTED_EDGE ( 'NONE', *, *, #81012, .F. ) ;
#55030 = EDGE_CURVE ( 'NONE', #44550, #29599, #47271, .T. ) ;
#55031 = CARTESIAN_POINT ( 'NONE',  ( -0.4593175853018366950, 0.05413385826771666132, 0.4176697321401328100 ) ) ;
#55032 = CARTESIAN_POINT ( 'NONE',  ( -0.3805774278215216522, 0.05413385826771666132, 0.4176697321401328100 ) ) ;
#55033 = CARTESIAN_POINT ( 'NONE',  ( -0.4790026246719152336, -0.05778040916215560624, -0.4822834645669293319 ) ) ;
#55034 = CARTESIAN_POINT ( 'NONE',  ( 0.9908136482939640111, -0.6692913385826771977, 0.1292274648535927661 ) ) ;
#55035 = CARTESIAN_POINT ( 'NONE',  ( -0.7545931758530176614, -0.6692913385826773087, -0.1292274648535924053 ) ) ;
#55036 = CARTESIAN_POINT ( 'NONE',  ( -0.5380577427821514602, -0.4281496062992127816, -0.4176697321401328100 ) ) ;
#55037 = CARTESIAN_POINT ( 'NONE',  ( 1.240157480314961314, -0.5400638737290844871, 0.3530559997133364547 ) ) ;
#55038 = CARTESIAN_POINT ( 'NONE',  ( 0.4133858267716541968, -0.5400638737290845981, -0.3530559997133363437 ) ) ;
#55039 = CARTESIAN_POINT ( 'NONE',  ( 0.6496062992125991586, -0.5400638737290845981, -0.3530559997133363437 ) ) ;
#55040 = CARTESIAN_POINT ( 'NONE',  ( 0.2867679344610365999, -0.2867679344610365444, -0.8779527559055116948 ) ) ;
#55041 = CARTESIAN_POINT ( 'NONE',  ( 0.1181102362204730916, 0.1771653543307087630, 0.000000000000000000 ) ) ;
#55042 = VERTEX_POINT ( 'NONE', #22447 ) ;
#55043 = CARTESIAN_POINT ( 'NONE',  ( 0.3949938075777409963, 2.418639510665530435E-17, -0.9055118110236219930 ) ) ;
#55044 = ORIENTED_EDGE ( 'NONE', *, *, #7150, .T. ) ;
#55045 = CARTESIAN_POINT ( 'NONE',  ( -0.6889763779527552368, -0.4536011799217368745, -0.2665933059059886201 ) ) ;
#55046 = CARTESIAN_POINT ( 'NONE',  ( -0.5708661417322825615, -0.5400638737290844871, 0.3530559997133364547 ) ) ;
#55047 = CARTESIAN_POINT ( 'NONE',  ( -0.3149606299212734384, 2.755905511811024056, 3.924389226575467404 ) ) ;
#55048 = CARTESIAN_POINT ( 'NONE',  ( -0.5905511811023615998, 0.2952755905511811885, 0.000000000000000000 ) ) ;
#55049 = CARTESIAN_POINT ( 'NONE',  ( -0.6496062992125976043, -0.5400638737290844871, 0.3530559997133364547 ) ) ;
#55050 = CARTESIAN_POINT ( 'NONE',  ( -1.279527559055116948, 0.1660481256975883668, -0.3530559997133364547 ) ) ;
#55051 = CARTESIAN_POINT ( 'NONE',  ( -1.220472440944881054, 0.2952755905511811885, 0.000000000000000000 ) ) ;
#55052 = CARTESIAN_POINT ( 'NONE',  ( 1.049868766404200349, 0.1283753931104748280, 0.1820866141732283561 ) ) ;
#55053 = CARTESIAN_POINT ( 'NONE',  ( 0.2746809754671078463, 0.1088096450009770899, 5.561685372298315500 ) ) ;
#55054 = CARTESIAN_POINT ( 'NONE',  ( 0.6167979002624678353, -0.3690944881889763329, 0.3153832671262228327 ) ) ;
#55055 = CARTESIAN_POINT ( 'NONE',  ( 0.09842519685039434474, 0.1660481256975885056, 0.3530559997133364547 ) ) ;
#55056 = CARTESIAN_POINT ( 'NONE',  ( -0.08530183727034056085, -0.3162353388693405765, 0.4822834645669290543 ) ) ;
#55057 = ORIENTED_EDGE ( 'NONE', *, *, #27581, .F. ) ;
#55058 = CARTESIAN_POINT ( 'NONE',  ( -0.3996062992125986035, -7.340648628747425578E-17, -1.771653543307086576 ) ) ;
#55059 = CARTESIAN_POINT ( 'NONE',  ( -0.4724409448818898682, -8.678599364036362592E-17, -0.3543307086614173040 ) ) ;
#55060 = VERTEX_POINT ( 'NONE', #35908 ) ;
#55061 = CARTESIAN_POINT ( 'NONE',  ( -9.787531504996566615E-17, 0.3996062992125985480, -1.336614173228346303 ) ) ;
#55062 = CARTESIAN_POINT ( 'NONE',  ( -0.1936066689571366572, 0.2229926280064455923, 0.1399704324547694501 ) ) ;
#55063 = CARTESIAN_POINT ( 'NONE',  ( -0.9055118110236215490, 0.1771653543307087630, 0.000000000000000000 ) ) ;
#55064 = CARTESIAN_POINT ( 'NONE',  ( -0.9711286089238838626, -0.6046776061558807314, 0.2411417322834647770 ) ) ;
#55065 = CARTESIAN_POINT ( 'NONE',  ( -0.1265901696524986964, -0.4724409448818899238, -0.3871391076115485719 ) ) ;
#55066 = CARTESIAN_POINT ( 'NONE',  ( 0.3392501089628018329, 0.1958661417322835607, -2.735564304461941987 ) ) ;
#55067 = CARTESIAN_POINT ( 'NONE',  ( 1.587926509186352586, -0.4281496062992127816, -0.4176697321401328100 ) ) ;
#55068 = CARTESIAN_POINT ( 'NONE',  ( 0.5839895013123367340, -0.6692913385826773087, -0.1292274648535924053 ) ) ;
#55069 = CARTESIAN_POINT ( 'NONE',  ( 0.5118110236220480003, -0.6692913385826771977, 8.415575281601705876E-17 ) ) ;
#55070 = CARTESIAN_POINT ( 'NONE',  ( -0.7677165354330699465, -0.4536011799217368745, -0.2665933059059886201 ) ) ;
#55071 = CARTESIAN_POINT ( 'NONE',  ( 0.2362204724409456558, -0.1870078740157480879, -0.4822834645669291653 ) ) ;
#55072 = CARTESIAN_POINT ( 'NONE',  ( 0.3458507752293908943, 0.3458507752293908943, -2.419291338582676865 ) ) ;
#55073 = CARTESIAN_POINT ( 'NONE',  ( -0.6233595800524928121, -0.05778040916215522460, 0.4822834645669289988 ) ) ;
#55074 = CARTESIAN_POINT ( 'NONE',  ( -0.1974969037888706924, 0.3420746716998658843, -1.822178477690288512 ) ) ;
#55075 = CARTESIAN_POINT ( 'NONE',  ( 1.332020997375328974, -0.08942795157528024563, -0.3641732283464568787 ) ) ;
#55076 = CARTESIAN_POINT ( 'NONE',  ( 0.2887139107611556010, -0.5023911411419708095, 0.1820866141732285504 ) ) ;
#55077 = CARTESIAN_POINT ( 'NONE',  ( 1.062992125984252745, 0.1771653543307087630, 0.000000000000000000 ) ) ;
#55078 = CARTESIAN_POINT ( 'NONE',  ( -1.246719160104986512, 0.05413385826771666132, 0.4176697321401328100 ) ) ;
#55079 = CARTESIAN_POINT ( 'NONE',  ( -1.318897637795274802, 0.07958543189024085140, 0.2665933059059887866 ) ) ;
#55080 = CARTESIAN_POINT ( 'NONE',  ( 5.785732909357575061E-17, -0.4724409448818898682, -2.202755905511811108 ) ) ;
#55081 = CARTESIAN_POINT ( 'NONE',  ( -1.161417322834644716, -0.5400638737290845981, -0.3530559997133363437 ) ) ;
#55082 = CARTESIAN_POINT ( 'NONE',  ( -0.5249343832020990641, 0.2306618581243848609, 0.2411417322834645549 ) ) ;
#55083 = CARTESIAN_POINT ( 'NONE',  ( 0.4199475065616805614, 0.2306618581243848609, 0.2411417322834645549 ) ) ;
#55084 = CARTESIAN_POINT ( 'NONE',  ( -0.2867679344610364334, -0.2867679344610368219, -2.343812705215535974 ) ) ;
#55085 = CARTESIAN_POINT ( 'NONE',  ( 0.5314960629920851831, 2.677165354330708791, 3.900966923095595451 ) ) ;
#55086 = CARTESIAN_POINT ( 'NONE',  ( 0.4527559055118117182, 0.07958543189024071263, -0.2665933059059888421 ) ) ;
#55087 = CARTESIAN_POINT ( 'NONE',  ( 0.9120734908136489683, -0.6692913385826771977, 0.1292274648535927661 ) ) ;
#55088 = CARTESIAN_POINT ( 'NONE',  ( -1.581364829396324945, -0.2845877964562159024, 0.3641732283464567677 ) ) ;
#55089 = CARTESIAN_POINT ( 'NONE',  ( 0.9317585301837276734, 0.05413385826771626580, -0.4176697321401330321 ) ) ;
#55090 = CARTESIAN_POINT ( 'NONE',  ( -1.614173228346456268, -0.5511811023622047445, 6.969142054262312111E-17 ) ) ;
#55091 = CARTESIAN_POINT ( 'NONE',  ( -1.417322834645668772, -0.1870078740157479769, 0.4822834645669291653 ) ) ;
#55092 = EDGE_CURVE ( 'NONE', #74087, #66780, #78615, .T. ) ;
#55093 = CARTESIAN_POINT ( 'NONE',  ( -0.8727034120734901146, -0.05778040916215560624, -0.4822834645669293319 ) ) ;
#55094 = CARTESIAN_POINT ( 'NONE',  ( 0.01968503937007957949, -0.4536011799217368745, -0.2665933059059886201 ) ) ;
#55095 = CARTESIAN_POINT ( 'NONE',  ( 1.614173228346457378, 0.2753471884572480932, -0.1372047244094471152 ) ) ;
#55096 = CARTESIAN_POINT ( 'NONE',  ( 0.8070866141732288002, 0.07958543189024085140, 0.2665933059059887866 ) ) ;
#55097 = B_SPLINE_CURVE_WITH_KNOTS ( 'NONE', 1,
 ( #49199, #4585 ),
 .UNSPECIFIED., .F., .F.,
 ( 2, 2 ),
 ( 0.000000000000000000, 0.001849999999999997480 ),
 .UNSPECIFIED. ) ;
#55098 = CARTESIAN_POINT ( 'NONE',  ( -0.1181102362204717315, -0.6692913385826771977, 8.415575281601705876E-17 ) ) ;
#55099 = CARTESIAN_POINT ( 'NONE',  ( 0.1070741851644053388, 0.3996062992125986035, -0.3851706036745406458 ) ) ;
#55100 = CARTESIAN_POINT ( 'NONE',  ( -1.299212598425196097, -0.6692913385826771977, 8.415575281601705876E-17 ) ) ;
#55101 = CARTESIAN_POINT ( 'NONE',  ( -0.1049643490035302024, -0.3917322834645671215, -1.731627296587926468 ) ) ;
#55102 = CARTESIAN_POINT ( 'NONE',  ( 0.8595800524934390507, -0.08942795157528024563, -0.3641732283464568787 ) ) ;
#55103 = CARTESIAN_POINT ( 'NONE',  ( 0.1049868766404206816, 0.2306618581243848609, 0.2411417322834645549 ) ) ;
#55104 = CARTESIAN_POINT ( 'NONE',  ( -0.2296587926509179312, -0.05778040916215522460, 0.4822834645669289988 ) ) ;
#55105 = CARTESIAN_POINT ( 'NONE',  ( -0.5380577427821514602, -0.004921259842519576551, 0.3153832671262227771 ) ) ;
#55106 = CARTESIAN_POINT ( 'NONE',  ( 1.003937007874016185, 0.1012011053420775880, -0.2882089793578257453 ) ) ;
#55107 = CARTESIAN_POINT ( 'NONE',  ( -0.4790026246719152336, -0.08942795157528024563, -0.3641732283464568787 ) ) ;
#55108 = CARTESIAN_POINT ( 'NONE',  ( 0.2690288713910767848, 0.2952755905511811885, 0.1292274648535926551 ) ) ;
#55109 = CARTESIAN_POINT ( 'NONE',  ( -1.351706036745406347, -0.004921259842519870586, -0.3153832671262229437 ) ) ;
#55110 = CARTESIAN_POINT ( 'NONE',  ( 0.3996062992125985480, 2.446882876249141654E-17, -1.454724409448818978 ) ) ;
#55111 = CARTESIAN_POINT ( 'NONE',  ( -1.620734908136482577, 0.2952755905511811885, 0.1292274648535926551 ) ) ;
#55112 = CARTESIAN_POINT ( 'NONE',  ( 0.4724409448818898682, 2.892866454678787531E-17, -2.557086614173228689 ) ) ;
#55113 = VERTEX_POINT ( 'NONE', #41790 ) ;
#55114 = CARTESIAN_POINT ( 'NONE',  ( -1.666666666666665853, -0.004921259842519870586, -0.3153832671262229437 ) ) ;
#55115 = CARTESIAN_POINT ( 'NONE',  ( -0.6233595800524928121, -0.05778040916215522460, 0.4822834645669289988 ) ) ;
#55116 = CARTESIAN_POINT ( 'NONE',  ( -1.266404199475064773, -0.05778040916215560624, -0.4822834645669293319 ) ) ;
#55117 = CARTESIAN_POINT ( 'NONE',  ( -0.3917322834645670104, -7.196005306013484475E-17, -1.541338582677165503 ) ) ;
#55118 = CARTESIAN_POINT ( 'NONE',  ( -0.4091458600556402980, -0.2362204724409451284, -2.099737532808398921 ) ) ;
#55119 = CARTESIAN_POINT ( 'NONE',  ( 1.463254593175853824, -0.6692913385826771977, 0.1292274648535927661 ) ) ;
#55120 = CARTESIAN_POINT ( 'NONE',  ( 0.5118110236220480003, -0.6692913385826771977, 8.415575281601705876E-17 ) ) ;
#55121 = PLANE ( 'NONE',  #44841 ) ;
#55122 = CARTESIAN_POINT ( 'NONE',  ( 0.1070741851644054637, -0.3996062992125984925, -2.524278215223096478 ) ) ;
#55123 = CARTESIAN_POINT ( 'NONE',  ( 1.528871391076116026, -0.5511811023622048555, -0.09757992244046775898 ) ) ;
#55124 = CARTESIAN_POINT ( 'NONE',  ( 0.3996062992125986035, 0.1070741851644054776, -0.9120734908136483021 ) ) ;
#55125 = ORIENTED_EDGE ( 'NONE', *, *, #30797, .T. ) ;
#55126 = CARTESIAN_POINT ( 'NONE',  ( -0.7939632545931750718, -0.08942795157528024563, -0.3641732283464568787 ) ) ;
#55127 = CARTESIAN_POINT ( 'NONE',  ( -9.594673741351313045E-17, 0.3917322834645670104, -2.354330708661417138 ) ) ;
#55128 = ORIENTED_EDGE ( 'NONE', *, *, #51138, .T. ) ;
#55129 = CARTESIAN_POINT ( 'NONE',  ( 0.9645669291338588858, 0.1660481256975885056, 0.3530559997133364547 ) ) ;
#55130 = CARTESIAN_POINT ( 'NONE',  ( -0.5380577427821514602, -0.4281496062992127816, -0.4176697321401328100 ) ) ;
#55131 = CARTESIAN_POINT ( 'NONE',  ( -1.003937007874014853, 0.1660481256975885056, 0.3530559997133364547 ) ) ;
#55132 = CARTESIAN_POINT ( 'NONE',  ( 1.167979002624672580, -0.4281496062992124485, 0.4176697321401328655 ) ) ;
#55133 = CARTESIAN_POINT ( 'NONE',  ( -1.358267716535432434, -0.4536011799217367080, 0.2665933059059888421 ) ) ;
#55134 = FACE_OUTER_BOUND ( 'NONE', #51626, .T. ) ;
#55135 = CARTESIAN_POINT ( 'NONE',  ( 0.1771653543307093182, -0.5400638737290845981, -0.3530559997133363437 ) ) ;
#55136 = CARTESIAN_POINT ( 'NONE',  ( -0.8661417322834640276, -0.1870078740157479769, 0.4822834645669291653 ) ) ;
#55137 = CARTESIAN_POINT ( 'NONE',  ( 0.2867679344610365999, 0.2867679344610365999, -1.477670972932071614 ) ) ;
#55138 = CARTESIAN_POINT ( 'NONE',  ( -1.220472440944881054, -0.6692913385826771977, 8.415575281601705876E-17 ) ) ;
#55139 = DIRECTION ( 'NONE',  ( -1.000000000000000000, -9.738798461624180871E-16, 0.000000000000000000 ) ) ;
#55140 = CARTESIAN_POINT ( 'NONE',  ( 1.049868766404200349, 0.2306618581243848609, 0.2411417322834645549 ) ) ;
#55141 = CARTESIAN_POINT ( 'NONE',  ( -0.3392501089628017219, -0.1958661417322836718, -2.656824146981627166 ) ) ;
#55142 = CARTESIAN_POINT ( 'NONE',  ( 1.194225721784777594, -0.004921259842519576551, 0.3153832671262227771 ) ) ;
#55143 = VERTEX_POINT ( 'NONE', #79712 ) ;
#55144 = CARTESIAN_POINT ( 'NONE',  ( -0.3392501089628019995, 0.1958661417322831999, -2.700150549377639653 ) ) ;
#55145 = CARTESIAN_POINT ( 'NONE',  ( -0.2165354330708654795, 0.1660481256975885056, 0.3530559997133364547 ) ) ;
#55146 = ORIENTED_EDGE ( 'NONE', *, *, #3457, .F. ) ;
#55147 = CARTESIAN_POINT ( 'NONE',  ( 0.3018372703412079971, -0.3690944881889763329, 0.3153832671262228327 ) ) ;
#55148 = CARTESIAN_POINT ( 'NONE',  ( -1.627296587926508442, -0.6046776061558809534, -0.2411417322834644161 ) ) ;
#55149 = CARTESIAN_POINT ( 'NONE',  ( 0.6299212598425204535, -0.1870078740157479769, 0.4822834645669291653 ) ) ;
#55150 = CARTESIAN_POINT ( 'NONE',  ( 0.7349081364829402885, -0.6046776061558809534, -0.2411417322834644161 ) ) ;
#55151 = CARTESIAN_POINT ( 'NONE',  ( -0.2034120734908131112, -0.6692913385826773087, -0.1292274648535924053 ) ) ;
#55152 = CARTESIAN_POINT ( 'NONE',  ( -0.3392501089628019995, 0.1958661417322831999, -1.440308029692600522 ) ) ;
#55153 = CARTESIAN_POINT ( 'NONE',  ( -0.7283464566929126471, -0.5400638737290844871, 0.3530559997133364547 ) ) ;
#55154 = CARTESIAN_POINT ( 'NONE',  ( 0.3917322834645669549, 0.1049643490035304660, -2.414041994750655729 ) ) ;
#55155 = CARTESIAN_POINT ( 'NONE',  ( -1.673228346456691717, 0.1660481256975883668, -0.3530559997133364547 ) ) ;
#55156 = CARTESIAN_POINT ( 'NONE',  ( -0.8661417322834640276, -0.1870078740157479769, 0.4822834645669291653 ) ) ;
#55157 = CARTESIAN_POINT ( 'NONE',  ( 1.220472440944882608, 0.2952755905511811885, 0.000000000000000000 ) ) ;
#55158 = CARTESIAN_POINT ( 'NONE',  ( 1.167979002624672580, -0.4281496062992124485, 0.4176697321401328655 ) ) ;
#55159 = EDGE_CURVE ( 'NONE', #47997, #12829, #31071, .T. ) ;
#55160 = CARTESIAN_POINT ( 'NONE',  ( -0.2925321140481930704, -0.2925321140481933480, -0.5314960629921260393 ) ) ;
#55161 = CARTESIAN_POINT ( 'NONE',  ( -1.115485564304461219, -0.4281496062992124485, 0.4176697321401328655 ) ) ;
#55162 = CARTESIAN_POINT ( 'NONE',  ( -0.3460692066303960313, 0.1998031496062989965, 0.05446194225721784354 ) ) ;
#55163 = CARTESIAN_POINT ( 'NONE',  ( 0.3280839895013130669, 0.05413385826771666132, 0.4176697321401328100 ) ) ;
#55164 = CARTESIAN_POINT ( 'NONE',  ( 0.2925321140481932369, 0.2925321140481932369, -2.185039370078739829 ) ) ;
#55165 = B_SPLINE_CURVE_WITH_KNOTS ( 'NONE', 1,
 ( #33011, #76398 ),
 .UNSPECIFIED., .F., .F.,
 ( 2, 2 ),
 ( 0.000000000000000000, 0.001849999999999997480 ),
 .UNSPECIFIED. ) ;
#55166 = CARTESIAN_POINT ( 'NONE',  ( -0.3740157480314953431, 0.1660481256975885056, 0.3530559997133364547 ) ) ;
#55167 = CARTESIAN_POINT ( 'NONE',  ( -1.482939632545930975, -0.004921259842519576551, 0.3153832671262227771 ) ) ;
#55168 = CARTESIAN_POINT ( 'NONE',  ( 0.7349081364829403995, 0.1283753931104748280, 0.1820866141732283561 ) ) ;
#55169 = CARTESIAN_POINT ( 'NONE',  ( 1.135170603674541256, 0.2952755905511811885, 0.1292274648535926551 ) ) ;
#55170 = CARTESIAN_POINT ( 'NONE',  ( -0.2362204724409451284, 0.4091458600556402425, -0.8772965879265091083 ) ) ;
#55171 = CARTESIAN_POINT ( 'NONE',  ( 0.6955380577427828781, -0.3690944881889763329, 0.3153832671262228327 ) ) ;
#55172 = CARTESIAN_POINT ( 'NONE',  ( 0.7020997375328090762, -0.05778040916215560624, -0.4822834645669293319 ) ) ;
#55173 = CARTESIAN_POINT ( 'NONE',  ( 4.837279021331061486E-17, -0.3949938075777409963, -0.4704724409448818867 ) ) ;
#55174 = CARTESIAN_POINT ( 'NONE',  ( -0.4790026246719154557, -0.3162353388693405765, 0.4822834645669290543 ) ) ;
#55175 = DIRECTION ( 'NONE',  ( 3.491481338843132961E-15, 0.000000000000000000, -1.000000000000000000 ) ) ;
#55176 = CARTESIAN_POINT ( 'NONE',  ( 1.167979002624672580, -0.004921259842519870586, -0.3153832671262229437 ) ) ;
#55177 = CARTESIAN_POINT ( 'NONE',  ( -0.5774278215223089816, 0.2306618581243847221, -0.2411417322834647770 ) ) ;
#55178 = CARTESIAN_POINT ( 'NONE',  ( 0.06561679790026316017, 0.05413385826771626580, -0.4176697321401330321 ) ) ;
#55179 = CARTESIAN_POINT ( 'NONE',  ( -2.795275590551184575, 0.7480314960629931287, -3.317813449798768424E-16 ) ) ;
#55180 = CARTESIAN_POINT ( 'NONE',  ( 0.1837270341207354329, 0.2306618581243848609, 0.2411417322834645549 ) ) ;
#55181 = CARTESIAN_POINT ( 'NONE',  ( 0.5249343832021005074, -0.5023911411419708095, 0.1820866141732285504 ) ) ;
#55182 = CARTESIAN_POINT ( 'NONE',  ( -0.4107360162338847265, 1.299495150281466227, -1.044197310779563237 ) ) ;
#55183 = EDGE_CURVE ( 'NONE', #1571, #34573, #11341, .T. ) ;
#55184 = CARTESIAN_POINT ( 'NONE',  ( -0.1509186351706028884, -0.2845877964562161244, -0.3641732283464567121 ) ) ;
#55185 = CARTESIAN_POINT ( 'NONE',  ( 0.6561679790026253567, 0.1283753931104748280, 0.1820866141732283561 ) ) ;
#55186 = FACE_OUTER_BOUND ( 'NONE', #81983, .T. ) ;
#55187 = CARTESIAN_POINT ( 'NONE',  ( 0.3996062992125986035, -0.1070741851644052972, -1.920603674540682260 ) ) ;
#55188 = CARTESIAN_POINT ( 'NONE',  ( 0.1312335958005257930, 0.2306618581243847221, -0.2411417322834647770 ) ) ;
#55189 = ADVANCED_FACE ( 'NONE', ( #31222 ), #63630, .F. ) ;
#55190 = CARTESIAN_POINT ( 'NONE',  ( 0.3917322834645670104, 2.398668435337828261E-17, -1.212598425196850238 ) ) ;
#55191 = CARTESIAN_POINT ( 'NONE',  ( 1.482939632545932307, -0.3690944881889763329, 0.3153832671262228327 ) ) ;
#55192 = CARTESIAN_POINT ( 'NONE',  ( 0.1443569553805781891, 0.05413385826771626580, -0.4176697321401330321 ) ) ;
#55193 = CARTESIAN_POINT ( 'NONE',  ( 0.1902887139107617975, 0.1771653543307087630, 0.09757992244046791164 ) ) ;
#55194 = CARTESIAN_POINT ( 'NONE',  ( 0.2887139107611556010, 0.2306618581243847221, -0.2411417322834647770 ) ) ;
#55195 = CARTESIAN_POINT ( 'NONE',  ( 1.384514435695538559, 0.1771653543307087075, -0.09757992244046823083 ) ) ;
#55196 = CARTESIAN_POINT ( 'NONE',  ( -1.187664041994750175, -0.08942795157528024563, -0.3641732283464568787 ) ) ;
#55197 = CARTESIAN_POINT ( 'NONE',  ( -1.568241469816272105, -0.05778040916215522460, 0.4822834645669289988 ) ) ;
#55198 = CARTESIAN_POINT ( 'NONE',  ( 0.2821522309711292364, 0.2952755905511810774, -0.1292274648535930714 ) ) ;
#55199 = CARTESIAN_POINT ( 'NONE',  ( 1.036745406824147731, 0.05413385826771666132, 0.4176697321401328100 ) ) ;
#55200 = DIRECTION ( 'NONE',  ( 0.000000000000000000, -0.4999999999999998335, 0.8660254037844385966 ) ) ;
#55201 = CARTESIAN_POINT ( 'NONE',  ( 0.3083989501312343062, -0.3162353388693405765, 0.4822834645669290543 ) ) ;
#55202 = CARTESIAN_POINT ( 'NONE',  ( 1.246719160104987623, 0.05413385826771626580, -0.4176697321401330321 ) ) ;
#55203 = CARTESIAN_POINT ( 'NONE',  ( 0.8136482939632553313, -0.6046776061558809534, -0.2411417322834644161 ) ) ;
#55204 = CARTESIAN_POINT ( 'NONE',  ( -1.595398199321655275, 2.136509776695170615, -0.1559797534342494130 ) ) ;
#55205 = CARTESIAN_POINT ( 'NONE',  ( 0.7480314960629927956, 0.1771653543307087630, 0.000000000000000000 ) ) ;
#55206 = CARTESIAN_POINT ( 'NONE',  ( -1.535433070866141225, -0.5511811023622047445, 6.969142054262312111E-17 ) ) ;
#55207 = CARTESIAN_POINT ( 'NONE',  ( 0.3018372703412079971, -0.3690944881889763329, 0.3153832671262228327 ) ) ;
#55208 = CARTESIAN_POINT ( 'NONE',  ( 0.1771653543307093182, -0.5400638737290845981, -0.3530559997133363437 ) ) ;
#55209 = CARTESIAN_POINT ( 'NONE',  ( 0.5511811023622054106, -0.1870078740157480879, -0.4822834645669291653 ) ) ;
#55210 = CARTESIAN_POINT ( 'NONE',  ( -0.2755905511811015396, -0.6692913385826771977, 8.415575281601705876E-17 ) ) ;
#55211 = CARTESIAN_POINT ( 'NONE',  ( -0.1049643490035307158, 0.3917322834645670104, -2.208024565125671135 ) ) ;
#55212 = CARTESIAN_POINT ( 'NONE',  ( -0.1115485564304456306, 0.1771653543307087075, -0.09757992244046823083 ) ) ;
#55213 = CIRCLE ( 'NONE', #63270, 0.09842519685039372024 ) ;
#55214 = CARTESIAN_POINT ( 'NONE',  ( 0.6167979002624678353, -0.4281496062992124485, 0.4176697321401328655 ) ) ;
#55215 = CARTESIAN_POINT ( 'NONE',  ( 1.056430446194226658, 0.1771653543307087630, 0.09757992244046791164 ) ) ;
#55216 = DIRECTION ( 'NONE',  ( 0.000000000000000000, 0.000000000000000000, 1.000000000000000000 ) ) ;
#55218 = CARTESIAN_POINT ( 'NONE',  ( 0.1181102362204724532, -0.04921259842519688094, 0.08523872084492505052 ) ) ;
#55217 = CARTESIAN_POINT ( 'NONE',  ( -1.082677165354329896, 0.1660481256975885056, 0.3530559997133364547 ) ) ;
#55219 = DIRECTION ( 'NONE',  ( 0.000000000000000000, 1.000000000000000000, -0.000000000000000000 ) ) ;
#55220 = CARTESIAN_POINT ( 'NONE',  ( -1.089238845144356427, -0.4281496062992127816, -0.4176697321401328100 ) ) ;
#55221 = CARTESIAN_POINT ( 'NONE',  ( -0.4199475065616791736, 0.2306618581243847221, -0.2411417322834647770 ) ) ;
#55222 = CARTESIAN_POINT ( 'NONE',  ( -0.1070741851644056997, 0.3996062992125986035, -2.841207349081364963 ) ) ;
#55223 = CARTESIAN_POINT ( 'NONE',  ( 0.3949938075777409408, 0.1058382717557500574, -2.329396325459317740 ) ) ;
#55224 = ORIENTED_EDGE ( 'NONE', *, *, #35564, .F. ) ;
#55225 = CARTESIAN_POINT ( 'NONE',  ( 0.1706036745406830368, -0.3690944881889765550, -0.3153832671262227771 ) ) ;
#55226 = CARTESIAN_POINT ( 'NONE',  ( -0.1958661417322836718, 0.3392501089628017219, -1.107611548556430403 ) ) ;
#55227 = CARTESIAN_POINT ( 'NONE',  ( 1.246719160104987623, -0.4281496062992124485, 0.4176697321401328655 ) ) ;
#55228 = CARTESIAN_POINT ( 'NONE',  ( -0.2362204724409451284, 0.4091458600556402425, -2.375328083989501238 ) ) ;
#55229 = DIRECTION ( 'NONE',  ( -0.000000000000000000, -1.000000000000000000, -0.000000000000000000 ) ) ;
#55231 = CIRCLE ( 'NONE', #45791, 1.968503937007874072 ) ;
#55230 = CARTESIAN_POINT ( 'NONE',  ( -0.2462293917967295909, -2.567464376874931580E-15, -0.4445507791589072832 ) ) ;
#55232 = CARTESIAN_POINT ( 'NONE',  ( -0.06312602682716046687, 1.066946945958372028, 1.120379939242540868 ) ) ;
#55233 = CARTESIAN_POINT ( 'NONE',  ( 1.272965879265092637, -0.004921259842519576551, 0.3153832671262227771 ) ) ;
#55234 = CARTESIAN_POINT ( 'NONE',  ( 0.2230971128608932319, -0.4281496062992124485, 0.4176697321401328655 ) ) ;
#55235 = CARTESIAN_POINT ( 'NONE',  ( -0.3917322834645669549, -7.196005306013483243E-17, -0.4343638863178984622 ) ) ;
#55236 = ADVANCED_FACE ( 'NONE', ( #81361 ), #12297, .F. ) ;
#55237 = CARTESIAN_POINT ( 'NONE',  ( -0.006561679790025524116, -0.05778040916215560624, -0.4822834645669293319 ) ) ;
#55238 = CARTESIAN_POINT ( 'NONE',  ( -1.076115485564303809, 0.1283753931104748280, 0.1820866141732283561 ) ) ;
#55239 = CARTESIAN_POINT ( 'NONE',  ( 0.3412073490813655186, 0.2306618581243848609, 0.2411417322834645549 ) ) ;
#55240 = CARTESIAN_POINT ( 'NONE',  ( -0.09186351706036689768, 0.05413385826771626580, -0.4176697321401330321 ) ) ;
#55241 = DIRECTION ( 'NONE',  ( 1.000000000000000000, -0.000000000000000000, 0.000000000000000000 ) ) ;
#55242 = CARTESIAN_POINT ( 'NONE',  ( 0.3460692066303959757, -0.1998031496062991907, -2.939632545931758489 ) ) ;
#55243 = CARTESIAN_POINT ( 'NONE',  ( 0.3917322834645670659, -0.1049643490035303273, -1.683090181923571294 ) ) ;
#55244 = CARTESIAN_POINT ( 'NONE',  ( 0.8530183727034128527, -0.4281496062992124485, 0.4176697321401328655 ) ) ;
#55245 = CARTESIAN_POINT ( 'NONE',  ( -0.2559055118110230564, 0.1660481256975883668, -0.3530559997133364547 ) ) ;
#55246 = CARTESIAN_POINT ( 'NONE',  ( -1.128608923884513837, 0.2306618581243847221, -0.2411417322834647770 ) ) ;
#55247 = CARTESIAN_POINT ( 'NONE',  ( 1.167979002624672580, 0.05413385826771626580, -0.4176697321401330321 ) ) ;
#55248 = CARTESIAN_POINT ( 'NONE',  ( 0.4527559055118117182, 0.1660481256975883668, -0.3530559997133364547 ) ) ;
#55249 = CARTESIAN_POINT ( 'NONE',  ( 0.3392501089628018884, -0.1958661417322834220, -0.9770341207349081403 ) ) ;
#55250 = CARTESIAN_POINT ( 'NONE',  ( -0.5577427821522301654, -0.05778040916215560624, -0.4822834645669293319 ) ) ;
#55251 = CARTESIAN_POINT ( 'NONE',  ( 0.2296587926509192634, -0.3162353388693405765, 0.4822834645669290543 ) ) ;
#55252 = CARTESIAN_POINT ( 'NONE',  ( -0.5971128608923877978, -0.6692913385826773087, -0.1292274648535924053 ) ) ;
#55253 = CARTESIAN_POINT ( 'NONE',  ( 0.1640419947506569498, -0.2845877964562161244, -0.3641732283464567121 ) ) ;
#55254 = CARTESIAN_POINT ( 'NONE',  ( 1.633858267716535639, -0.4536011799217367080, 0.2665933059059888421 ) ) ;
#55255 = CARTESIAN_POINT ( 'NONE',  ( -0.2516608251556126663, 1.134091190147785699, -2.808839726227330580 ) ) ;
#55256 = CARTESIAN_POINT ( 'NONE',  ( 0.2559055118110243332, -0.5400638737290845981, -0.3530559997133363437 ) ) ;
#55257 = CARTESIAN_POINT ( 'NONE',  ( 1.509186351706037543, -0.4281496062992127816, -0.4176697321401328100 ) ) ;
#55258 = CARTESIAN_POINT ( 'NONE',  ( 0.3917322834645669549, 0.1049643490035304660, -2.164041994750655729 ) ) ;
#55259 = ORIENTED_EDGE ( 'NONE', *, *, #65662, .T. ) ;
#55260 = ORIENTED_EDGE ( 'NONE', *, *, #33761, .T. ) ;
#55261 = CARTESIAN_POINT ( 'NONE',  ( 0.6824146981627303710, -0.6046776061558807314, 0.2411417322834647770 ) ) ;
#55262 = CARTESIAN_POINT ( 'NONE',  ( 0.4133858267716541968, -0.4536011799217368745, -0.2665933059059886201 ) ) ;
#55264 = LINE ( 'NONE', #10678, #62594 ) ;
#55263 = FACE_OUTER_BOUND ( 'NONE', #31660, .T. ) ;
#55265 = CARTESIAN_POINT ( 'NONE',  ( 0.3917322834645670104, 2.398668435337828261E-17, -0.6751968503937009203 ) ) ;
#55266 = CARTESIAN_POINT ( 'NONE',  ( 0.2362204724409451007, -0.4091458600556402980, -0.01115485564304462100 ) ) ;
#55267 = DIRECTION ( 'NONE',  ( -1.000000000000000000, 0.000000000000000000, -0.000000000000000000 ) ) ;
#55268 = CARTESIAN_POINT ( 'NONE',  ( 0.3460692066303958092, 0.1998031496062993018, -2.570209973753280863 ) ) ;
#55269 = CARTESIAN_POINT ( 'NONE',  ( 0.7874015748031503170, -0.1870078740157479769, 0.4822834645669291653 ) ) ;
#55270 = CARTESIAN_POINT ( 'NONE',  ( -0.6233595800524928121, -0.3162353388693409650, -0.4822834645669289433 ) ) ;
#55271 = CARTESIAN_POINT ( 'NONE',  ( -0.7217847769028863381, 0.05413385826771626580, -0.4176697321401330321 ) ) ;
#55272 = CARTESIAN_POINT ( 'NONE',  ( 0.4855643044619428750, 0.05413385826771666132, 0.4176697321401328100 ) ) ;
#55273 = VECTOR ( 'NONE', #6187, 39.37007874015748143 ) ;
#55274 = CARTESIAN_POINT ( 'NONE',  ( 1.404199475065617264, -0.4281496062992124485, 0.4176697321401328655 ) ) ;
#55275 = CARTESIAN_POINT ( 'NONE',  ( -1.022479694362532499, 1.428910228063043686, 0.4621002115169275393 ) ) ;
#55276 = ITEM_DEFINED_TRANSFORMATION ( 'NONE', 'NONE', #24836,  #22098 ) ;
#55277 = CARTESIAN_POINT ( 'NONE',  ( 1.213910761154856299, 0.1771653543307087630, 0.09757992244046791164 ) ) ;
#55278 = DIRECTION ( 'NONE',  ( -0.7071067811865495711, -0.000000000000000000, 0.7071067811865454633 ) ) ;
#55279 = CARTESIAN_POINT ( 'NONE',  ( -1.161417322834644716, 0.07958543189024085140, 0.2665933059059887866 ) ) ;
#55280 = LINE ( 'NONE', #80169, #3312 ) ;
#55281 = CARTESIAN_POINT ( 'NONE',  ( 0.1706036745406830368, -0.4281496062992127816, -0.4176697321401328100 ) ) ;
#55283 = CARTESIAN_POINT ( 'NONE',  ( -1.076935383196057527, 2.165354330708661568, -0.3149606299212600047 ) ) ;
#55282 = CARTESIAN_POINT ( 'NONE',  ( 1.115485564304462551, -0.4281496062992127816, -0.4176697321401328100 ) ) ;
#55284 = CARTESIAN_POINT ( 'NONE',  ( -1.174540682414697335, -0.2845877964562161244, -0.3641732283464567121 ) ) ;
#55285 = CARTESIAN_POINT ( 'NONE',  ( 0.4593175853018380828, 0.05413385826771626580, -0.4176697321401330321 ) ) ;
#55286 = CARTESIAN_POINT ( 'NONE',  ( 1.437007874015748810, 0.07958543189024085140, 0.2665933059059887866 ) ) ;
#55287 = CARTESIAN_POINT ( 'NONE',  ( 0.1958661417322834497, 0.3392501089628018329, -1.641712967682728008 ) ) ;
#55288 = CARTESIAN_POINT ( 'NONE',  ( -1.384514435695537005, 0.1771653543307087630, 0.09757992244046791164 ) ) ;
#55289 = CARTESIAN_POINT ( 'NONE',  ( 1.489501312335958172, -0.3162353388693405765, 0.4822834645669290543 ) ) ;
#55290 = ADVANCED_FACE ( 'NONE', ( #69942 ), #44659, .T. ) ;
#55291 = CARTESIAN_POINT ( 'NONE',  ( 2.611754389584936220, 1.697151583350149595, -0.4469586986359051495 ) ) ;
#55292 = CARTESIAN_POINT ( 'NONE',  ( -0.2559055118110230564, 0.07958543189024071263, -0.2665933059059888421 ) ) ;
#55293 = CARTESIAN_POINT ( 'NONE',  ( 0.02624671916010564918, 0.2306618581243848609, 0.2411417322834645549 ) ) ;
#55294 = CARTESIAN_POINT ( 'NONE',  ( -1.174540682414697335, -0.08942795157527998196, 0.3641732283464567121 ) ) ;
#55295 = CARTESIAN_POINT ( 'NONE',  ( -0.9055118110236215490, 0.2952755905511811885, 0.000000000000000000 ) ) ;
#55296 = CARTESIAN_POINT ( 'NONE',  ( 1.167979002624672580, -0.4281496062992124485, 0.4176697321401328655 ) ) ;
#55297 = CARTESIAN_POINT ( 'NONE',  ( -0.1958661417322836995, 0.3392501089628017219, -0.6397830953093982531 ) ) ;
#55298 =( BOUNDED_SURFACE ( )  B_SPLINE_SURFACE ( 1, 2, ( 
 ( #35964, #11947, #56540, #55711, #81835, #61207, #10713, #80600, #49408, #17449, #75102, #30873, #3975, #11536, #29639, #30466, #81420, #11120, #24146, #37193, #42260, #23736, #24560, #61634, #36370, #82241, #3563, #62044, #36777, #4381, #55300, #29229, #42676, #43490, #81008, #67955, #56129, #50226, #17855, #62453, #43079, #62873, #5209, #75922, #30049, #49816, #23322, #68374, #68776, #4789, #48577, #18261, #74690, #69186, #43903, #75516, #16618, #22909, #69600, #74274, #10298, #48992, #17036, #77157, #38844, #25794, #83054, #63690, #71261, #19489, #32530, #38014, #63276, #44311, #25377, #19916, #45566, #987, #82645, #51040, #12772, #18666, #13607, #6446, #58194, #57359, #44719, #51454, #38429, #24959, #52296, #76741, #77583, #64943, #64524, #76336, #71678, #39261, #45142, #70417, #70846, #7283, #13196, #6861, #562, #19071, #6029, #32953, #26215, #51877, #31700, #5616, #70001, #64112, #58619, #26642, #78002, #50631, #32117, #57775, #12356, #20330, #45982, #138, #37602, #31283, #56948, #27889, #73347, #67033, #7713, #2224, #33380, #53549, #65793, #21990, #78839, #72095, #52712, #79257, #72923, #14454, #33792, #40105, #3050, #9365, #1398, #59457, #54379, #72512, #41352, #60701, #8127, #15275, #1808, #59044, #40523, #27054, #35036, #27470, #21572, #78424, #46821, #14030, #65378, #39686, #15694, #53128, #48066, #28716, #8541, #34627, #20752, #14861, #46402, #47234, #40936, #66615, #80089, #21165, #47651, #66202, #8952, #34207, #60291, #2641, #22410, #59870, #28298, #53960, #79673, #23222, #43385, #73769, #48892, #23632, #74593, #48474, #16103, #55201, #56027, #10199, #80501, #68675, #69086, #30358, #49304, #55609, #24044, #49715, #11434, #68279, #75005, #67443, #42980, #81735, #37089, #29538, #62775, #75411, #67862, #16937, #42577, #81320, #35868, #35448, #61113, #5109, #17755, #61534, #10614, #24455, #17352, #36271, #54798, #61942, #3465, #11016, #22817, #3879, #36673, #30776, #62349, #4283, #56437, #29945, #4687, #74176, #82140, #41748, #16522, #80909, #9776, #29131, #42167, #70736, #43793, #18567, #71158, #69900, #35, #64419, #31179, #32426, #12666, #13090, #77052, #56844, #76233, #12254, #38743, #37911, #57251, #77474, #58517, #6754, #38326, #82542, #39154, #58089, #45460, #75820, #454, #63999, #24860, #6341, #32013, #82954, #25272, #51771, #13498, #26110, #19385, #45037, #11848, #76636, #63588, #19811, #70311, #64839, #57673, #7177, #50121, #32848, #880, #18162, #5923, #37501, #25688, #50527, #69499, #63176, #5514, #44210, #31595, #50939, #18967, #51349, #44616, #1709, #65696, #66099, #15591, #60190, #60603, #71574, #45876, #65271, #33689, #28199, #1300, #21060, #66937, #71996, #46721, #8026, #27364, #27786, #72413, #14762, #2121, #20228, #79157, #66515, #47550, #59350, #79570, #8847, #20649, #53025, #78738, #8435, #46302, #13925, #39582, #41249, #53858, #14349, #40418, #26540, #59766, #34105, #7607, #53449, #33281, #21474, #58942, #40009, #47132, #73242, #15173, #72823, #2541, #40830, #34524, #26949, #21886, #9269, #52612, #34940, #52193, #77897, #78318, #24667, #79991, #54695, #25071, #22716, #37309, #18377, #67346, #69711, #48792, #50335, #30980, #9679, #29027, #48375, #76032, #74074, #10097, #31392, #12461, #44017, #74490, #35350, #76443, #12055, #82749, #28617, #37712, #16837, #61012, #43600, #69302, #35761, #61428, #5721, #50745, #63386, #56648, #82348, #47965, #29441, #16420, #57057, #23124, #18772, #11651, #44415, #2952, #70110, #38123, #54275, #42066, #73667, #62983, #3363, #22305, #16009, #41655, #80404, #67761, #3778, #55100, #5322, #80809, #38951, #19595, #20022, #52824, #14143, #14564, #25483, #83164, #19178, #70954, #65490, #38540, #58305, #20859, #25902, #670, #45258, #64635, #65058, #26325, #70524, #44827, #77692, #39795, #33489, #57470, #51987, #51150, #45673, #32226, #71789, #13299, #64220, #12880, #71369, #39372, #6554, #250, #57883, #78536, #59151, #76844, #51563, #46511, #6970, #7822, #27161, #77266, #7395, #32641, #13719, #33063, #58734, #1508, #1096, #26747, #52402, #78111, #63797, #31810, #6135, #72212, #20443, #46097 ),
 ( #34740, #14969, #15384, #29245, #21273, #47345, #48181, #22519, #67144, #60810, #33899, #8649, #61224, #59982, #73459, #54491, #46928, #73878, #2751, #3163, #9474, #72621, #66309, #2340, #28827, #27997, #73034, #67556, #48592, #80202, #28411, #40627, #54909, #16217, #35561, #65898, #41864, #54070, #34320, #79785, #22101, #41046, #66731, #9891, #3578, #80615, #35147, #22927, #1920, #9069, #53656, #74289, #60401, #40216, #47761, #8234, #59564, #27583, #53239, #78955, #79364, #21683, #15810, #41460, #82255, #63292, #69616, #50647, #10728, #36385, #74706, #5631, #11961, #3991, #62059, #56962, #75119, #43918, #31298, #42692, #17870, #17051, #61650, #43095, #29655, #37617, #68389, #30481, #55317, #49424, #16633, #67972, #42275, #75937, #4398, #10315, #82660, #11136, #37208, #35980, #17464, #81025, #4805, #56147, #81850, #24974, #30065, #50241, #55728, #69204, #36795, #49831, #62888, #18278, #23338, #62470, #49007, #81436, #68791, #23751, #24162, #75530, #43504, #11552, #5224, #30887, #56555, #24574, #12787, #83071, #71273, #71692, #32966, #26228, #58208, #26655, #52309, #14044, #45156, #13622, #38443, #154, #64538, #51468, #63704, #7726, #6461, #58633, #20344, #77596, #31716, #27068, #78016, #6875, #25807, #575, #45995, #32544, #19930, #51892, #64125, #19086, #39700, #45580, #39274, #76755, #18681, #25391, #32131, #1001, #65391, #33395, #38029, #57788, #77170, #57375, #59057, #64959, #51055, #19502, #44734, #70430, #7296, #1412, #76350, #70017, #44325, #12370, #6044, #70859, #13210, #38857, #27483, #8140, #40949, #28312, #53141, #9377, #2654, #34640, #3061, #28729, #73779, #21585, #73358, #72526, #59883, #66628, #27902, #40119, #67454, #66215, #35047, #80101, #53973, #33805, #3475, #54390, #8966, #2237, #60305, #22420, #79686, #22003, #47663, #14875, #78853, #48077, #15706, #41363, #21179, #78438, #59470, #40536, #60712, #16115, #41760, #14467, #8554, #53562, #1823, #9788, #67044, #46834, #34221, #79271, #47248, #35459, #61124, #52726, #46416, #20765, #72109, #65807, #72937, #15289, #10626, #3890, #67872, #17363, #4698, #29550, #48904, #55212, #18174, #82152, #16533, #74605, #69511, #4294, #56450, #75833, #80920, #30371, #23235, #74187, #55622, #42178, #24468, #16948, #42991, #10210, #61954, #29142, #80512, #54808, #5120, #42590, #63188, #50134, #23645, #49726, #22827, #29957, #48485, #68685, #11028, #36685, #43807, #68290, #62786, #36282, #81746, #49316, #62360, #75423, #30787, #35878, #75017, #11860, #81331, #56038, #37513, #61546, #24056, #17766, #43398, #69097, #11445, #37101, #71171, #25284, #12266, #468, #897, #5527, #52207, #77911, #45890, #18980, #76245, #13102, #69912, #13512, #20242, #58531, #39597, #82966, #32439, #71588, #38756, #6768, #64014, #44629, #45050, #13940, #39168, #31192, #50541, #24873, #44222, #12681, #7191, #63601, #48, #56858, #50952, #25701, #70325, #6355, #58102, #51362, #77066, #64433, #82555, #26124, #45474, #26554, #38339, #18579, #64853, #76649, #32026, #57686, #70751, #19399, #37924, #5937, #31607, #32863, #51785, #77489, #57268, #19824, #34120, #46317, #27803, #52627, #60205, #72010, #27380, #72837, #28633, #53872, #79171, #41265, #40433, #59781, #40023, #66114, #54290, #14366, #72428, #73257, #47564, #8861, #2555, #58956, #33704, #2966, #1723, #15187, #79586, #65711, #15605, #53463, #28213, #34539, #8041, #59364, #53041, #21900, #78753, #14778, #9283, #73682, #66951, #21488, #21078, #80006, #34954, #60617, #7624, #22319, #47147, #46736, #40844, #66530, #8449, #2135, #47982, #16022, #65286, #33296, #1314, #26963, #78333, #20664, #30273, #61856, #10930, #4197, #82056, #17266, #35364, #36586, #81651, #62684, #80823, #11348, #23962, #35775, #74505, #68190, #23548, #61445, #3378, #29041, #56358, #68996, #29456, #42487, #75736, #74922, #10529, #22730, #29860, #54712, #62265, #48389, #3792, #49216, #5026, #55936, #55523, #17668, #16852, #36184, #16434, #81232, #30694, #74088, #48806, #49628, #75322, #68589, #4602, #61029, #10114, #24370, #55114, #42895, #43299, #42080, #37006, #50040, #41669, #67360, #67775, #23137, #9693 ) ),
 .UNSPECIFIED., .F., .F., .F. ) 
 B_SPLINE_SURFACE_WITH_KNOTS ( ( 2, 2 ),
 ( 3, 2, 2, 2, 2, 2, 2, 2, 2, 2, 2, 2, 2, 2, 2, 2, 2, 2, 2, 2, 2, 2, 2, 2, 2, 2, 2, 2, 2, 2, 2, 2, 2, 2, 2, 2, 2, 2, 2, 2, 2, 2, 2, 2, 2, 2, 2, 2, 2, 2, 2, 2, 2, 2, 2, 2, 2, 2, 2, 2, 2, 2, 2, 2, 2, 2, 2, 2, 2, 2, 2, 2, 2, 2, 2, 2, 2, 2, 2, 2, 2, 2, 2, 2, 2, 2, 2, 2, 2, 2, 2, 2, 2, 2, 2, 2, 2, 2, 2, 2, 2, 2, 2, 2, 2, 2, 2, 2, 2, 2, 2, 2, 2, 2, 2, 2, 2, 2, 2, 2, 2, 2, 2, 2, 2, 2, 2, 2, 2, 2, 2, 2, 2, 2, 2, 2, 2, 2, 2, 2, 2, 2, 2, 2, 2, 2, 2, 2, 2, 2, 2, 2, 2, 2, 2, 2, 2, 2, 2, 2, 2, 2, 2, 2, 2, 2, 2, 2, 2, 2, 2, 2, 2, 2, 2, 2, 2, 2, 2, 2, 2, 2, 2, 2, 2, 2, 2, 2, 2, 2, 2, 2, 2, 2, 2, 2, 2, 2, 2, 2, 2, 2, 2, 2, 2, 2, 2, 2, 2, 2, 2, 2, 2, 2, 2, 2, 2, 2, 2, 2, 2, 2, 2, 2, 2, 2, 2, 2, 2, 2, 2, 2, 2, 2, 2, 2, 2, 2, 2, 2, 2, 2, 2, 2, 2, 2, 2, 2, 2, 2, 2, 2, 2, 2, 2, 3 ),
 ( 0.000000000000000000, 1.000000000000000000 ),
 ( 0.000000000000000000, 0.003787878787878787984, 0.007575757575757575968, 0.01136363636363636395, 0.01515151515151515194, 0.01893939393939393992, 0.02272727272727272790, 0.02651515151515151589, 0.03030303030303030387, 0.03409090909090908839, 0.03787878787878787984, 0.04166666666666666435, 0.04545454545454545581, 0.04924242424242424032, 0.05303030303030303177, 0.05681818181818181629, 0.06060606060606060774, 0.06439393939393939226, 0.06818181818181817677, 0.07196969696969697516, 0.07575757575757575968, 0.07954545454545454419, 0.08333333333333332871, 0.08712121212121212710, 0.09090909090909091161, 0.09469696969696969613, 0.09848484848484848064, 0.1022727272727272790, 0.1060606060606060635, 0.1098484848484848481, 0.1136363636363636326, 0.1174242424242424310, 0.1212121212121212155, 0.1250000000000000000, 0.1287878787878787845, 0.1325757575757575690, 0.1363636363636363535, 0.1401515151515151381, 0.1439393939393939503, 0.1477272727272727348, 0.1515151515151515194, 0.1553030303030303039, 0.1590909090909090884, 0.1628787878787878729, 0.1666666666666666574, 0.1704545454545454419, 0.1742424242424242542, 0.1780303030303030387, 0.1818181818181818232, 0.1856060606060606077, 0.1893939393939393923, 0.1931818181818181768, 0.1969696969696969613, 0.2007575757575757458, 0.2045454545454545581, 0.2083333333333333426, 0.2121212121212121271, 0.2159090909090909116, 0.2196969696969696961, 0.2234848484848484806, 0.2272727272727272652, 0.2310606060606060497, 0.2348484848484848619, 0.2386363636363636465, 0.2424242424242424310, 0.2462121212121212155, 0.2500000000000000000, 0.2537878787878787845, 0.2575757575757575690, 0.2613636363636363535, 0.2651515151515151381, 0.2689393939393939226, 0.2727272727272727071, 0.2765151515151514916, 0.2803030303030302761, 0.2840909090909091161, 0.2878787878787879007, 0.2916666666666666852, 0.2954545454545454697, 0.2992424242424242542, 0.3030303030303030387, 0.3068181818181818232, 0.3106060606060606077, 0.3143939393939393923, 0.3181818181818181768, 0.3219696969696969613, 0.3257575757575757458, 0.3295454545454545303, 0.3333333333333333148, 0.3371212121212120993, 0.3409090909090908839, 0.3446969696969697239, 0.3484848484848485084, 0.3522727272727272929, 0.3560606060606060774, 0.3598484848484848619, 0.3636363636363636465, 0.3674242424242424310, 0.3712121212121212155, 0.3750000000000000000, 0.3787878787878787845, 0.3825757575757575690, 0.3863636363636363535, 0.3901515151515151381, 0.3939393939393939226, 0.3977272727272727071, 0.4015151515151514916, 0.4053030303030302761, 0.4090909090909091161, 0.4128787878787879007, 0.4166666666666666852, 0.4204545454545454697, 0.4242424242424242542, 0.4280303030303030387, 0.4318181818181818232, 0.4356060606060606077, 0.4393939393939393923, 0.4431818181818181768, 0.4469696969696969613, 0.4507575757575757458, 0.4545454545454545303, 0.4583333333333333148, 0.4621212121212120993, 0.4659090909090908839, 0.4696969696969697239, 0.4734848484848485084, 0.4772727272727272929, 0.4810606060606060774, 0.4848484848484848619, 0.4886363636363636465, 0.4924242424242424310, 0.4962121212121212155, 0.5000000000000000000, 0.5037878787878787845, 0.5075757575757575690, 0.5113636363636363535, 0.5151515151515151381, 0.5189393939393939226, 0.5227272727272727071, 0.5265151515151514916, 0.5303030303030302761, 0.5340909090909090606, 0.5378787878787878451, 0.5416666666666666297, 0.5454545454545454142, 0.5492424242424241987, 0.5530303030303029832, 0.5568181818181817677, 0.5606060606060605522, 0.5643939393939394478, 0.5681818181818182323, 0.5719696969696970168, 0.5757575757575758013, 0.5795454545454545858, 0.5833333333333333703, 0.5871212121212121549, 0.5909090909090909394, 0.5946969696969697239, 0.5984848484848485084, 0.6022727272727272929, 0.6060606060606060774, 0.6098484848484848619, 0.6136363636363636465, 0.6174242424242424310, 0.6212121212121212155, 0.6250000000000000000, 0.6287878787878787845, 0.6325757575757575690, 0.6363636363636363535, 0.6401515151515151381, 0.6439393939393939226, 0.6477272727272727071, 0.6515151515151514916, 0.6553030303030302761, 0.6590909090909090606, 0.6628787878787878451, 0.6666666666666666297, 0.6704545454545454142, 0.6742424242424241987, 0.6780303030303029832, 0.6818181818181817677, 0.6856060606060605522, 0.6893939393939394478, 0.6931818181818182323, 0.6969696969696970168, 0.7007575757575758013, 0.7045454545454545858, 0.7083333333333333703, 0.7121212121212121549, 0.7159090909090909394, 0.7196969696969697239, 0.7234848484848485084, 0.7272727272727272929, 0.7310606060606060774, 0.7348484848484848619, 0.7386363636363636465, 0.7424242424242424310, 0.7462121212121212155, 0.7500000000000000000, 0.7537878787878787845, 0.7575757575757575690, 0.7613636363636363535, 0.7651515151515151381, 0.7689393939393939226, 0.7727272727272727071, 0.7765151515151514916, 0.7803030303030302761, 0.7840909090909090606, 0.7878787878787878451, 0.7916666666666666297, 0.7954545454545454142, 0.7992424242424241987, 0.8030303030303029832, 0.8068181818181817677, 0.8106060606060605522, 0.8143939393939394478, 0.8181818181818182323, 0.8219696969696970168, 0.8257575757575758013, 0.8295454545454545858, 0.8333333333333333703, 0.8371212121212121549, 0.8409090909090909394, 0.8446969696969697239, 0.8484848484848485084, 0.8522727272727272929, 0.8560606060606060774, 0.8598484848484848619, 0.8636363636363636465, 0.8674242424242424310, 0.8712121212121212155, 0.8750000000000000000, 0.8787878787878787845, 0.8825757575757575690, 0.8863636363636363535, 0.8901515151515151381, 0.8939393939393939226, 0.8977272727272727071, 0.9015151515151514916, 0.9053030303030302761, 0.9090909090909090606, 0.9128787878787878451, 0.9166666666666666297, 0.9204545454545454142, 0.9242424242424241987, 0.9280303030303029832, 0.9318181818181817677, 0.9356060606060605522, 0.9393939393939394478, 0.9431818181818182323, 0.9469696969696970168, 0.9507575757575758013, 0.9545454545454545858, 0.9583333333333333703, 0.9621212121212121549, 0.9659090909090909394 ),
 .UNSPECIFIED. ) 
 GEOMETRIC_REPRESENTATION_ITEM ( )  RATIONAL_B_SPLINE_SURFACE ( (
 ( 1.000000000000000000, 0.9659258262890683122, 1.000000000000000000, 0.9659258262890683122, 1.000000000000000000, 0.9659258262890683122, 1.000000000000000000, 0.9659258262890683122, 1.000000000000000000, 0.9659258262890683122, 1.000000000000000000, 0.9659258262890683122, 1.000000000000000000, 0.9659258262890683122, 1.000000000000000000, 0.9659258262890683122, 1.000000000000000000, 0.9659258262890683122, 1.000000000000000000, 0.9659258262890683122, 1.000000000000000000, 0.9659258262890683122, 1.000000000000000000, 0.9659258262890683122, 1.000000000000000000, 0.9659258262890683122, 1.000000000000000000, 0.9659258262890683122, 1.000000000000000000, 0.9659258262890683122, 1.000000000000000000, 0.9659258262890683122, 1.000000000000000000, 0.9659258262890683122, 1.000000000000000000, 0.9659258262890683122, 1.000000000000000000, 0.9659258262890683122, 1.000000000000000000, 0.9659258262890683122, 1.000000000000000000, 0.9659258262890683122, 1.000000000000000000, 0.9659258262890683122, 1.000000000000000000, 0.9659258262890683122, 1.000000000000000000, 0.9659258262890683122, 1.000000000000000000, 0.9659258262890683122, 1.000000000000000000, 0.9659258262890683122, 1.000000000000000000, 0.9659258262890683122, 1.000000000000000000, 0.9659258262890683122, 1.000000000000000000, 0.9659258262890683122, 1.000000000000000000, 0.9659258262890683122, 1.000000000000000000, 0.9659258262890683122, 1.000000000000000000, 0.9659258262890683122, 1.000000000000000000, 0.9659258262890683122, 1.000000000000000000, 0.9659258262890683122, 1.000000000000000000, 0.9659258262890683122, 1.000000000000000000, 0.9659258262890683122, 1.000000000000000000, 0.9659258262890683122, 1.000000000000000000, 0.9659258262890683122, 1.000000000000000000, 0.9659258262890683122, 1.000000000000000000, 0.9659258262890683122, 1.000000000000000000, 0.9659258262890683122, 1.000000000000000000, 0.9659258262890683122, 1.000000000000000000, 0.9659258262890683122, 1.000000000000000000, 0.9659258262890683122, 1.000000000000000000, 0.9659258262890683122, 1.000000000000000000, 0.9659258262890683122, 1.000000000000000000, 0.9659258262890683122, 1.000000000000000000, 0.9659258262890683122, 1.000000000000000000, 0.9659258262890683122, 1.000000000000000000, 0.9659258262890683122, 1.000000000000000000, 0.9659258262890683122, 1.000000000000000000, 0.9659258262890683122, 1.000000000000000000, 0.9659258262890683122, 1.000000000000000000, 0.9659258262890683122, 1.000000000000000000, 0.9659258262890683122, 1.000000000000000000, 0.9659258262890683122, 1.000000000000000000, 0.9659258262890683122, 1.000000000000000000, 0.9659258262890683122, 1.000000000000000000, 0.9659258262890683122, 1.000000000000000000, 0.9659258262890683122, 1.000000000000000000, 0.9659258262890683122, 1.000000000000000000, 0.9659258262890683122, 1.000000000000000000, 0.9659258262890683122, 1.000000000000000000, 0.9659258262890683122, 1.000000000000000000, 0.9659258262890683122, 1.000000000000000000, 0.9659258262890683122, 1.000000000000000000, 0.9659258262890683122, 1.000000000000000000, 0.9659258262890683122, 1.000000000000000000, 0.9659258262890683122, 1.000000000000000000, 0.9659258262890683122, 1.000000000000000000, 0.9659258262890683122, 1.000000000000000000, 0.9659258262890683122, 1.000000000000000000, 0.9659258262890683122, 1.000000000000000000, 0.9659258262890683122, 1.000000000000000000, 0.9659258262890683122, 1.000000000000000000, 0.9659258262890683122, 1.000000000000000000, 0.9659258262890683122, 1.000000000000000000, 0.9659258262890683122, 1.000000000000000000, 0.9659258262890683122, 1.000000000000000000, 0.9659258262890683122, 1.000000000000000000, 0.9659258262890683122, 1.000000000000000000, 0.9659258262890683122, 1.000000000000000000, 0.9659258262890683122, 1.000000000000000000, 0.9659258262890683122, 1.000000000000000000, 0.9659258262890683122, 1.000000000000000000, 0.9659258262890683122, 1.000000000000000000, 0.9659258262890683122, 1.000000000000000000, 0.9659258262890683122, 1.000000000000000000, 0.9659258262890683122, 1.000000000000000000, 0.9659258262890683122, 1.000000000000000000, 0.9659258262890683122, 1.000000000000000000, 0.9659258262890683122, 1.000000000000000000, 0.9659258262890683122, 1.000000000000000000, 0.9659258262890683122, 1.000000000000000000, 0.9659258262890683122, 1.000000000000000000, 0.9659258262890683122, 1.000000000000000000, 0.9659258262890683122, 1.000000000000000000, 0.9659258262890683122, 1.000000000000000000, 0.9659258262890683122, 1.000000000000000000, 0.9659258262890683122, 1.000000000000000000, 0.9659258262890683122, 1.000000000000000000, 0.9659258262890683122, 1.000000000000000000, 0.9659258262890683122, 1.000000000000000000, 0.9659258262890683122, 1.000000000000000000, 0.9659258262890683122, 1.000000000000000000, 0.9659258262890683122, 1.000000000000000000, 0.9659258262890683122, 1.000000000000000000, 0.9659258262890683122, 1.000000000000000000, 0.9659258262890683122, 1.000000000000000000, 0.9659258262890683122, 1.000000000000000000, 0.9659258262890683122, 1.000000000000000000, 0.9659258262890683122, 1.000000000000000000, 0.9659258262890683122, 1.000000000000000000, 0.9659258262890683122, 1.000000000000000000, 0.9659258262890683122, 1.000000000000000000, 0.9659258262890683122, 1.000000000000000000, 0.9659258262890683122, 1.000000000000000000, 0.9659258262890683122, 1.000000000000000000, 0.9659258262890683122, 1.000000000000000000, 0.9659258262890683122, 1.000000000000000000, 0.9659258262890683122, 1.000000000000000000, 0.9659258262890683122, 1.000000000000000000, 0.9659258262890683122, 1.000000000000000000, 0.9659258262890683122, 1.000000000000000000, 0.9659258262890683122, 1.000000000000000000, 0.9659258262890683122, 1.000000000000000000, 0.9659258262890683122, 1.000000000000000000, 0.9659258262890683122, 1.000000000000000000, 0.9659258262890683122, 1.000000000000000000, 0.9659258262890683122, 1.000000000000000000, 0.9659258262890683122, 1.000000000000000000, 0.9659258262890683122, 1.000000000000000000, 0.9659258262890683122, 1.000000000000000000, 0.9659258262890683122, 1.000000000000000000, 0.9659258262890683122, 1.000000000000000000, 0.9659258262890683122, 1.000000000000000000, 0.9659258262890683122, 1.000000000000000000, 0.9659258262890683122, 1.000000000000000000, 0.9659258262890683122, 1.000000000000000000, 0.9659258262890683122, 1.000000000000000000, 0.9659258262890683122, 1.000000000000000000, 0.9659258262890683122, 1.000000000000000000, 0.9659258262890683122, 1.000000000000000000, 0.9659258262890683122, 1.000000000000000000, 0.9659258262890683122, 1.000000000000000000, 0.9659258262890683122, 1.000000000000000000, 0.9659258262890683122, 1.000000000000000000, 0.9659258262890683122, 1.000000000000000000, 0.9659258262890683122, 1.000000000000000000, 0.9659258262890683122, 1.000000000000000000, 0.9659258262890683122, 1.000000000000000000, 0.9659258262890683122, 1.000000000000000000, 0.9659258262890683122, 1.000000000000000000, 0.9659258262890683122, 1.000000000000000000, 0.9659258262890683122, 1.000000000000000000, 0.9659258262890683122, 1.000000000000000000, 0.9659258262890683122, 1.000000000000000000, 0.9659258262890683122, 1.000000000000000000, 0.9659258262890683122, 1.000000000000000000, 0.9659258262890683122, 1.000000000000000000, 0.9659258262890683122, 1.000000000000000000, 0.9659258262890683122, 1.000000000000000000, 0.9659258262890683122, 1.000000000000000000, 0.9659258262890683122, 1.000000000000000000, 0.9659258262890683122, 1.000000000000000000, 0.9659258262890683122, 1.000000000000000000, 0.9659258262890683122, 1.000000000000000000, 0.9659258262890683122, 1.000000000000000000, 0.9659258262890683122, 1.000000000000000000, 0.9659258262890683122, 1.000000000000000000, 0.9659258262890683122, 1.000000000000000000, 0.9659258262890683122, 1.000000000000000000, 0.9659258262890683122, 1.000000000000000000, 0.9659258262890683122, 1.000000000000000000, 0.9659258262890683122, 1.000000000000000000, 0.9659258262890683122, 1.000000000000000000, 0.9659258262890683122, 1.000000000000000000, 0.9659258262890683122, 1.000000000000000000, 0.9659258262890683122, 1.000000000000000000, 0.9659258262890683122, 1.000000000000000000, 0.9659258262890683122, 1.000000000000000000, 0.9659258262890683122, 1.000000000000000000, 0.9659258262890683122, 1.000000000000000000, 0.9659258262890683122, 1.000000000000000000, 0.9659258262890683122, 1.000000000000000000, 0.9659258262890683122, 1.000000000000000000, 0.9659258262890683122, 1.000000000000000000, 0.9659258262890683122, 1.000000000000000000, 0.9659258262890683122, 1.000000000000000000, 0.9659258262890683122, 1.000000000000000000, 0.9659258262890683122, 1.000000000000000000, 0.9659258262890683122, 1.000000000000000000, 0.9659258262890683122, 1.000000000000000000, 0.9659258262890683122, 1.000000000000000000, 0.9659258262890683122, 1.000000000000000000, 0.9659258262890683122, 1.000000000000000000, 0.9659258262890683122, 1.000000000000000000, 0.9659258262890683122, 1.000000000000000000, 0.9659258262890683122, 1.000000000000000000, 0.9659258262890683122, 1.000000000000000000, 0.9659258262890683122, 1.000000000000000000, 0.9659258262890683122, 1.000000000000000000, 0.9659258262890683122, 1.000000000000000000, 0.9659258262890683122, 1.000000000000000000, 0.9659258262890683122, 1.000000000000000000, 0.9659258262890683122, 1.000000000000000000, 0.9659258262890683122, 1.000000000000000000, 0.9659258262890683122, 1.000000000000000000, 0.9659258262890683122, 1.000000000000000000, 0.9659258262890683122, 1.000000000000000000, 0.9659258262890683122, 1.000000000000000000, 0.9659258262890683122, 1.000000000000000000, 0.9659258262890683122, 1.000000000000000000, 0.9659258262890683122, 1.000000000000000000, 0.9659258262890683122, 1.000000000000000000, 0.9659258262890683122, 1.000000000000000000, 0.9659258262890683122, 1.000000000000000000, 0.9659258262890683122, 1.000000000000000000, 0.9659258262890683122, 1.000000000000000000, 0.9659258262890683122, 1.000000000000000000, 0.9659258262890683122, 1.000000000000000000, 0.9659258262890683122, 1.000000000000000000, 0.9659258262890683122, 1.000000000000000000, 0.9659258262890683122, 1.000000000000000000, 0.9659258262890683122, 1.000000000000000000, 0.9659258262890683122, 1.000000000000000000, 0.9659258262890683122, 1.000000000000000000, 0.9659258262890683122, 1.000000000000000000, 0.9659258262890683122, 1.000000000000000000, 0.9659258262890683122, 1.000000000000000000, 0.9659258262890683122, 1.000000000000000000, 0.9659258262890683122, 1.000000000000000000, 0.9659258262890683122, 1.000000000000000000, 0.9659258262890683122, 1.000000000000000000, 0.9659258262890683122, 1.000000000000000000, 0.9659258262890683122, 1.000000000000000000, 0.9659258262890683122, 1.000000000000000000, 0.9659258262890683122, 1.000000000000000000, 0.9659258262890683122, 1.000000000000000000, 0.9659258262890683122, 1.000000000000000000, 0.9659258262890683122, 1.000000000000000000, 0.9659258262890683122, 1.000000000000000000, 0.9659258262890683122, 1.000000000000000000, 0.9659258262890683122, 1.000000000000000000, 0.9659258262890683122, 1.000000000000000000, 0.9659258262890683122, 1.000000000000000000, 0.9659258262890683122, 1.000000000000000000, 0.9659258262890683122, 1.000000000000000000, 0.9659258262890683122, 1.000000000000000000, 0.9659258262890683122, 1.000000000000000000, 0.9659258262890683122, 1.000000000000000000, 0.9659258262890683122, 1.000000000000000000, 0.9659258262890683122, 1.000000000000000000, 0.9659258262890683122, 1.000000000000000000, 0.9659258262890683122, 1.000000000000000000),
 ( 1.000000000000000000, 0.9659258262890683122, 1.000000000000000000, 0.9659258262890683122, 1.000000000000000000, 0.9659258262890683122, 1.000000000000000000, 0.9659258262890683122, 1.000000000000000000, 0.9659258262890683122, 1.000000000000000000, 0.9659258262890683122, 1.000000000000000000, 0.9659258262890683122, 1.000000000000000000, 0.9659258262890683122, 1.000000000000000000, 0.9659258262890683122, 1.000000000000000000, 0.9659258262890683122, 1.000000000000000000, 0.9659258262890683122, 1.000000000000000000, 0.9659258262890683122, 1.000000000000000000, 0.9659258262890683122, 1.000000000000000000, 0.9659258262890683122, 1.000000000000000000, 0.9659258262890683122, 1.000000000000000000, 0.9659258262890683122, 1.000000000000000000, 0.9659258262890683122, 1.000000000000000000, 0.9659258262890683122, 1.000000000000000000, 0.9659258262890683122, 1.000000000000000000, 0.9659258262890683122, 1.000000000000000000, 0.9659258262890683122, 1.000000000000000000, 0.9659258262890683122, 1.000000000000000000, 0.9659258262890683122, 1.000000000000000000, 0.9659258262890683122, 1.000000000000000000, 0.9659258262890683122, 1.000000000000000000, 0.9659258262890683122, 1.000000000000000000, 0.9659258262890683122, 1.000000000000000000, 0.9659258262890683122, 1.000000000000000000, 0.9659258262890683122, 1.000000000000000000, 0.9659258262890683122, 1.000000000000000000, 0.9659258262890683122, 1.000000000000000000, 0.9659258262890683122, 1.000000000000000000, 0.9659258262890683122, 1.000000000000000000, 0.9659258262890683122, 1.000000000000000000, 0.9659258262890683122, 1.000000000000000000, 0.9659258262890683122, 1.000000000000000000, 0.9659258262890683122, 1.000000000000000000, 0.9659258262890683122, 1.000000000000000000, 0.9659258262890683122, 1.000000000000000000, 0.9659258262890683122, 1.000000000000000000, 0.9659258262890683122, 1.000000000000000000, 0.9659258262890683122, 1.000000000000000000, 0.9659258262890683122, 1.000000000000000000, 0.9659258262890683122, 1.000000000000000000, 0.9659258262890683122, 1.000000000000000000, 0.9659258262890683122, 1.000000000000000000, 0.9659258262890683122, 1.000000000000000000, 0.9659258262890683122, 1.000000000000000000, 0.9659258262890683122, 1.000000000000000000, 0.9659258262890683122, 1.000000000000000000, 0.9659258262890683122, 1.000000000000000000, 0.9659258262890683122, 1.000000000000000000, 0.9659258262890683122, 1.000000000000000000, 0.9659258262890683122, 1.000000000000000000, 0.9659258262890683122, 1.000000000000000000, 0.9659258262890683122, 1.000000000000000000, 0.9659258262890683122, 1.000000000000000000, 0.9659258262890683122, 1.000000000000000000, 0.9659258262890683122, 1.000000000000000000, 0.9659258262890683122, 1.000000000000000000, 0.9659258262890683122, 1.000000000000000000, 0.9659258262890683122, 1.000000000000000000, 0.9659258262890683122, 1.000000000000000000, 0.9659258262890683122, 1.000000000000000000, 0.9659258262890683122, 1.000000000000000000, 0.9659258262890683122, 1.000000000000000000, 0.9659258262890683122, 1.000000000000000000, 0.9659258262890683122, 1.000000000000000000, 0.9659258262890683122, 1.000000000000000000, 0.9659258262890683122, 1.000000000000000000, 0.9659258262890683122, 1.000000000000000000, 0.9659258262890683122, 1.000000000000000000, 0.9659258262890683122, 1.000000000000000000, 0.9659258262890683122, 1.000000000000000000, 0.9659258262890683122, 1.000000000000000000, 0.9659258262890683122, 1.000000000000000000, 0.9659258262890683122, 1.000000000000000000, 0.9659258262890683122, 1.000000000000000000, 0.9659258262890683122, 1.000000000000000000, 0.9659258262890683122, 1.000000000000000000, 0.9659258262890683122, 1.000000000000000000, 0.9659258262890683122, 1.000000000000000000, 0.9659258262890683122, 1.000000000000000000, 0.9659258262890683122, 1.000000000000000000, 0.9659258262890683122, 1.000000000000000000, 0.9659258262890683122, 1.000000000000000000, 0.9659258262890683122, 1.000000000000000000, 0.9659258262890683122, 1.000000000000000000, 0.9659258262890683122, 1.000000000000000000, 0.9659258262890683122, 1.000000000000000000, 0.9659258262890683122, 1.000000000000000000, 0.9659258262890683122, 1.000000000000000000, 0.9659258262890683122, 1.000000000000000000, 0.9659258262890683122, 1.000000000000000000, 0.9659258262890683122, 1.000000000000000000, 0.9659258262890683122, 1.000000000000000000, 0.9659258262890683122, 1.000000000000000000, 0.9659258262890683122, 1.000000000000000000, 0.9659258262890683122, 1.000000000000000000, 0.9659258262890683122, 1.000000000000000000, 0.9659258262890683122, 1.000000000000000000, 0.9659258262890683122, 1.000000000000000000, 0.9659258262890683122, 1.000000000000000000, 0.9659258262890683122, 1.000000000000000000, 0.9659258262890683122, 1.000000000000000000, 0.9659258262890683122, 1.000000000000000000, 0.9659258262890683122, 1.000000000000000000, 0.9659258262890683122, 1.000000000000000000, 0.9659258262890683122, 1.000000000000000000, 0.9659258262890683122, 1.000000000000000000, 0.9659258262890683122, 1.000000000000000000, 0.9659258262890683122, 1.000000000000000000, 0.9659258262890683122, 1.000000000000000000, 0.9659258262890683122, 1.000000000000000000, 0.9659258262890683122, 1.000000000000000000, 0.9659258262890683122, 1.000000000000000000, 0.9659258262890683122, 1.000000000000000000, 0.9659258262890683122, 1.000000000000000000, 0.9659258262890683122, 1.000000000000000000, 0.9659258262890683122, 1.000000000000000000, 0.9659258262890683122, 1.000000000000000000, 0.9659258262890683122, 1.000000000000000000, 0.9659258262890683122, 1.000000000000000000, 0.9659258262890683122, 1.000000000000000000, 0.9659258262890683122, 1.000000000000000000, 0.9659258262890683122, 1.000000000000000000, 0.9659258262890683122, 1.000000000000000000, 0.9659258262890683122, 1.000000000000000000, 0.9659258262890683122, 1.000000000000000000, 0.9659258262890683122, 1.000000000000000000, 0.9659258262890683122, 1.000000000000000000, 0.9659258262890683122, 1.000000000000000000, 0.9659258262890683122, 1.000000000000000000, 0.9659258262890683122, 1.000000000000000000, 0.9659258262890683122, 1.000000000000000000, 0.9659258262890683122, 1.000000000000000000, 0.9659258262890683122, 1.000000000000000000, 0.9659258262890683122, 1.000000000000000000, 0.9659258262890683122, 1.000000000000000000, 0.9659258262890683122, 1.000000000000000000, 0.9659258262890683122, 1.000000000000000000, 0.9659258262890683122, 1.000000000000000000, 0.9659258262890683122, 1.000000000000000000, 0.9659258262890683122, 1.000000000000000000, 0.9659258262890683122, 1.000000000000000000, 0.9659258262890683122, 1.000000000000000000, 0.9659258262890683122, 1.000000000000000000, 0.9659258262890683122, 1.000000000000000000, 0.9659258262890683122, 1.000000000000000000, 0.9659258262890683122, 1.000000000000000000, 0.9659258262890683122, 1.000000000000000000, 0.9659258262890683122, 1.000000000000000000, 0.9659258262890683122, 1.000000000000000000, 0.9659258262890683122, 1.000000000000000000, 0.9659258262890683122, 1.000000000000000000, 0.9659258262890683122, 1.000000000000000000, 0.9659258262890683122, 1.000000000000000000, 0.9659258262890683122, 1.000000000000000000, 0.9659258262890683122, 1.000000000000000000, 0.9659258262890683122, 1.000000000000000000, 0.9659258262890683122, 1.000000000000000000, 0.9659258262890683122, 1.000000000000000000, 0.9659258262890683122, 1.000000000000000000, 0.9659258262890683122, 1.000000000000000000, 0.9659258262890683122, 1.000000000000000000, 0.9659258262890683122, 1.000000000000000000, 0.9659258262890683122, 1.000000000000000000, 0.9659258262890683122, 1.000000000000000000, 0.9659258262890683122, 1.000000000000000000, 0.9659258262890683122, 1.000000000000000000, 0.9659258262890683122, 1.000000000000000000, 0.9659258262890683122, 1.000000000000000000, 0.9659258262890683122, 1.000000000000000000, 0.9659258262890683122, 1.000000000000000000, 0.9659258262890683122, 1.000000000000000000, 0.9659258262890683122, 1.000000000000000000, 0.9659258262890683122, 1.000000000000000000, 0.9659258262890683122, 1.000000000000000000, 0.9659258262890683122, 1.000000000000000000, 0.9659258262890683122, 1.000000000000000000, 0.9659258262890683122, 1.000000000000000000, 0.9659258262890683122, 1.000000000000000000, 0.9659258262890683122, 1.000000000000000000, 0.9659258262890683122, 1.000000000000000000, 0.9659258262890683122, 1.000000000000000000, 0.9659258262890683122, 1.000000000000000000, 0.9659258262890683122, 1.000000000000000000, 0.9659258262890683122, 1.000000000000000000, 0.9659258262890683122, 1.000000000000000000, 0.9659258262890683122, 1.000000000000000000, 0.9659258262890683122, 1.000000000000000000, 0.9659258262890683122, 1.000000000000000000, 0.9659258262890683122, 1.000000000000000000, 0.9659258262890683122, 1.000000000000000000, 0.9659258262890683122, 1.000000000000000000, 0.9659258262890683122, 1.000000000000000000, 0.9659258262890683122, 1.000000000000000000, 0.9659258262890683122, 1.000000000000000000, 0.9659258262890683122, 1.000000000000000000, 0.9659258262890683122, 1.000000000000000000, 0.9659258262890683122, 1.000000000000000000, 0.9659258262890683122, 1.000000000000000000, 0.9659258262890683122, 1.000000000000000000, 0.9659258262890683122, 1.000000000000000000, 0.9659258262890683122, 1.000000000000000000, 0.9659258262890683122, 1.000000000000000000, 0.9659258262890683122, 1.000000000000000000, 0.9659258262890683122, 1.000000000000000000, 0.9659258262890683122, 1.000000000000000000, 0.9659258262890683122, 1.000000000000000000, 0.9659258262890683122, 1.000000000000000000, 0.9659258262890683122, 1.000000000000000000, 0.9659258262890683122, 1.000000000000000000, 0.9659258262890683122, 1.000000000000000000, 0.9659258262890683122, 1.000000000000000000, 0.9659258262890683122, 1.000000000000000000, 0.9659258262890683122, 1.000000000000000000, 0.9659258262890683122, 1.000000000000000000, 0.9659258262890683122, 1.000000000000000000, 0.9659258262890683122, 1.000000000000000000, 0.9659258262890683122, 1.000000000000000000, 0.9659258262890683122, 1.000000000000000000, 0.9659258262890683122, 1.000000000000000000, 0.9659258262890683122, 1.000000000000000000, 0.9659258262890683122, 1.000000000000000000, 0.9659258262890683122, 1.000000000000000000, 0.9659258262890683122, 1.000000000000000000, 0.9659258262890683122, 1.000000000000000000, 0.9659258262890683122, 1.000000000000000000, 0.9659258262890683122, 1.000000000000000000, 0.9659258262890683122, 1.000000000000000000, 0.9659258262890683122, 1.000000000000000000, 0.9659258262890683122, 1.000000000000000000, 0.9659258262890683122, 1.000000000000000000, 0.9659258262890683122, 1.000000000000000000, 0.9659258262890683122, 1.000000000000000000, 0.9659258262890683122, 1.000000000000000000, 0.9659258262890683122, 1.000000000000000000, 0.9659258262890683122, 1.000000000000000000, 0.9659258262890683122, 1.000000000000000000, 0.9659258262890683122, 1.000000000000000000, 0.9659258262890683122, 1.000000000000000000, 0.9659258262890683122, 1.000000000000000000, 0.9659258262890683122, 1.000000000000000000, 0.9659258262890683122, 1.000000000000000000, 0.9659258262890683122, 1.000000000000000000, 0.9659258262890683122, 1.000000000000000000, 0.9659258262890683122, 1.000000000000000000, 0.9659258262890683122, 1.000000000000000000, 0.9659258262890683122, 1.000000000000000000, 0.9659258262890683122, 1.000000000000000000, 0.9659258262890683122, 1.000000000000000000, 0.9659258262890683122, 1.000000000000000000, 0.9659258262890683122, 1.000000000000000000, 0.9659258262890683122, 1.000000000000000000) ) ) 
 REPRESENTATION_ITEM ( '' )  SURFACE ( )  );
#55299 = CARTESIAN_POINT ( 'NONE',  ( 0.4497697399585466882, 1.386499259343020762, -1.566055164954403889 ) ) ;
#55300 = CARTESIAN_POINT ( 'NONE',  ( 1.417322834645670104, -0.1870078740157479769, 0.4822834645669291653 ) ) ;
#55301 = CARTESIAN_POINT ( 'NONE',  ( -0.4724409448818895907, -0.1265901696524993070, -2.169947506561679340 ) ) ;
#55302 = CARTESIAN_POINT ( 'NONE',  ( -1.417322834645668772, -0.1870078740157479769, 0.4822834645669291653 ) ) ;
#55303 = CARTESIAN_POINT ( 'NONE',  ( -1.259842519685038686, -0.1870078740157480601, -0.3641732283464567677 ) ) ;
#55304 = CARTESIAN_POINT ( 'NONE',  ( -0.7217847769028863381, -0.004921259842519870586, -0.3153832671262229437 ) ) ;
#55305 = EDGE_CURVE ( 'NONE', #13510, #11614, #27437, .T. ) ;
#55306 = CARTESIAN_POINT ( 'NONE',  ( -1.313877454013331780, 1.062992125984252079, 0.8967544760595740350 ) ) ;
#55307 = CARTESIAN_POINT ( 'NONE',  ( 0.08530183727034192087, -0.05778040916215522460, 0.4822834645669289988 ) ) ;
#55308 = CARTESIAN_POINT ( 'NONE',  ( -0.1902887139107604098, 0.1771653543307087075, -0.09757992244046823083 ) ) ;
#55309 = CARTESIAN_POINT ( 'NONE',  ( -1.062992125984250968, 0.1771653543307087630, 0.000000000000000000 ) ) ;
#55310 = CARTESIAN_POINT ( 'NONE',  ( -1.568241469816272105, -0.05778040916215522460, 0.4822834645669289988 ) ) ;
#55311 = CARTESIAN_POINT ( 'NONE',  ( 1.161417322834646271, 0.07958543189024071263, -0.2665933059059888421 ) ) ;
#55312 = CARTESIAN_POINT ( 'NONE',  ( 1.345144356955381593, -0.05778040916215522460, 0.4822834645669289988 ) ) ;
#55313 = CARTESIAN_POINT ( 'NONE',  ( 0.4732412630952341770, 1.503056026428866598, 2.167282348326871055 ) ) ;
#55314 = CARTESIAN_POINT ( 'NONE',  ( 0.2559055118110243332, 0.07958543189024085140, 0.2665933059059887866 ) ) ;
#55315 = CARTESIAN_POINT ( 'NONE',  ( 0.8398950131233602345, -0.6046776061558807314, 0.2411417322834647770 ) ) ;
#55316 = EDGE_CURVE ( 'NONE', #23166, #32357, #15398, .T. ) ;
#55317 = CARTESIAN_POINT ( 'NONE',  ( 1.036745406824147508, -0.3690944881889765550, -0.3153832671262227771 ) ) ;
#55318 = EDGE_LOOP ( 'NONE', ( #45737, #17583, #54746, #40277, #47258, #46872, #23995, #6084 ) ) ;
#55319 = CARTESIAN_POINT ( 'NONE',  ( -1.312335958005248715, 0.2306618581243848609, 0.2411417322834645549 ) ) ;
#55320 = CARTESIAN_POINT ( 'NONE',  ( -1.017060367454067249, -0.05778040916215522460, 0.4822834645669289988 ) ) ;
#55321 = CARTESIAN_POINT ( 'NONE',  ( -0.1837270341207343505, -0.6046776061558807314, 0.2411417322834647770 ) ) ;
#55322 = CARTESIAN_POINT ( 'NONE',  ( -2.094141031014932874, 1.724409448818898127, -0.4359958488159723644 ) ) ;
#55323 = CARTESIAN_POINT ( 'NONE',  ( 0.1998031496062994128, -0.3460692066303957537, -2.373359580052493367 ) ) ;
#55324 = CARTESIAN_POINT ( 'NONE',  ( 0.8727034120734912248, -0.3162353388693409650, -0.4822834645669289433 ) ) ;
#55325 = CARTESIAN_POINT ( 'NONE',  ( 1.614173228346457378, 0.1771653543307087630, 0.000000000000000000 ) ) ;
#55326 = CARTESIAN_POINT ( 'NONE',  ( 0.06561679790026316017, -0.4281496062992124485, 0.4176697321401328655 ) ) ;
#55327 = CARTESIAN_POINT ( 'NONE',  ( 0.9580052493438326877, 0.05413385826771666132, 0.4176697321401328100 ) ) ;
#55328 = CARTESIAN_POINT ( 'NONE',  ( -9.787531504996567848E-17, 0.3996062992125986035, -1.732283464566929165 ) ) ;
#55329 = CARTESIAN_POINT ( 'NONE',  ( 0.3420746716998659953, 0.1974969037888705536, -1.076115485564304475 ) ) ;
#55330 = CARTESIAN_POINT ( 'NONE',  ( 0.1070741851644053527, 0.3996062992125986590, -2.513123359580052174 ) ) ;
#55331 = CARTESIAN_POINT ( 'NONE',  ( -0.2087913723976026203, -0.2087913723976025926, 0.1248231986745540339 ) ) ;
#55332 = CARTESIAN_POINT ( 'NONE',  ( 0.3917322834645669549, 0.1049643490035304660, -0.7467191601049868455 ) ) ;
#55333 = CARTESIAN_POINT ( 'NONE',  ( -0.2952755905511804668, 0.07958543189024085140, 0.2665933059059887866 ) ) ;
#55334 = CARTESIAN_POINT ( 'NONE',  ( -0.7283464566929126471, 0.1660481256975883668, -0.3530559997133364547 ) ) ;
#55335 = CARTESIAN_POINT ( 'NONE',  ( 0.9842519685039375910, 0.2952755905511811885, 0.000000000000000000 ) ) ;
#55336 = CARTESIAN_POINT ( 'NONE',  ( 0.2891555358219910499, 0.2891555358219910499, -2.104330708661417138 ) ) ;
#55337 = EDGE_CURVE ( 'NONE', #49469, #29384, #62420, .T. ) ;
#55338 = CARTESIAN_POINT ( 'NONE',  ( -0.2952755905511803003, -0.4536011799217368745, -0.2665933059059886201 ) ) ;
#55339 = CARTESIAN_POINT ( 'NONE',  ( 1.568241469816273437, -0.3162353388693405765, 0.4822834645669290543 ) ) ;
#55340 = CARTESIAN_POINT ( 'NONE',  ( 1.023622047244095112, -0.1870078740157480879, -0.4822834645669291653 ) ) ;
#55341 = CARTESIAN_POINT ( 'NONE',  ( 0.2362204724409449064, 0.4091458600556404646, -2.349081364829396446 ) ) ;
#55342 = CARTESIAN_POINT ( 'NONE',  ( 0.1070741851644053527, 0.3996062992125986590, -1.568241469816272993 ) ) ;
#55343 = CARTESIAN_POINT ( 'NONE',  ( 1.614173228346457378, 1.055049524192302357, 0.1372047244094478369 ) ) ;
#55344 = CARTESIAN_POINT ( 'NONE',  ( 0.9120734908136489683, -0.6692913385826771977, 0.1292274648535927661 ) ) ;
#55345 = EDGE_CURVE ( 'NONE', #78599, #38787, #4728, .T. ) ;
#55346 = CARTESIAN_POINT ( 'NONE',  ( 1.167979002624672580, -0.004921259842519870586, -0.3153832671262229437 ) ) ;
#55348 = CARTESIAN_POINT ( 'NONE',  ( -1.594488188976377119, 0.1660481256975883668, -0.3530559997133364547 ) ) ;
#55347 = CARTESIAN_POINT ( 'NONE',  ( 1.627296587926509996, -0.6046776061558807314, 0.2411417322834647770 ) ) ;
#55349 = CARTESIAN_POINT ( 'NONE',  ( 0.1049643490035303689, 0.3917322834645670104, 0.07939632545931750440 ) ) ;
#55350 = CARTESIAN_POINT ( 'NONE',  ( -0.3983403474834782965, -0.03178304480584832892, -1.220472440944881942 ) ) ;
#55351 = CARTESIAN_POINT ( 'NONE',  ( 0.9383202099737538715, -0.05778040916215560624, -0.4822834645669293319 ) ) ;
#55352 = CARTESIAN_POINT ( 'NONE',  ( -1.614173228346456268, -0.6692913385826771977, 8.415575281601705876E-17 ) ) ;
#55353 = CARTESIAN_POINT ( 'NONE',  ( -0.6561679790026240244, -0.6046776061558807314, 0.2411417322834647770 ) ) ;
#55354 = CARTESIAN_POINT ( 'NONE',  ( -0.5839895013123351797, 0.2952755905511810774, -0.1292274648535930714 ) ) ;
#55355 = CARTESIAN_POINT ( 'NONE',  ( -1.535433070866141225, -0.6692913385826771977, 8.415575281601705876E-17 ) ) ;
#55356 = CARTESIAN_POINT ( 'NONE',  ( 0.3917322834645670104, 2.398668435337828261E-17, -0.3602362204724410266 ) ) ;
#55357 = CARTESIAN_POINT ( 'NONE',  ( 0.1706036745406830368, 0.05413385826771666132, 0.4176697321401328100 ) ) ;
#55358 = CARTESIAN_POINT ( 'NONE',  ( 0.1049643490035303689, 0.3917322834645670104, -2.190288713910760521 ) ) ;
#55359 = EDGE_CURVE ( 'NONE', #79849, #66112, #57524, .T. ) ;
#55360 = CARTESIAN_POINT ( 'NONE',  ( -1.633858267716534529, 0.07958543189024085140, 0.2665933059059887866 ) ) ;
#55361 = ORIENTED_EDGE ( 'NONE', *, *, #77077, .F. ) ;
#55362 = CARTESIAN_POINT ( 'NONE',  ( 0.1974969037888706369, -0.3420746716998659953, -2.769028871391075786 ) ) ;
#55363 = VERTEX_POINT ( 'NONE', #24086 ) ;
#55364 = CARTESIAN_POINT ( 'NONE',  ( -1.559171609364246924, 0.4110443821404751730, 0.5949441279213820710 ) ) ;
#55365 = CARTESIAN_POINT ( 'NONE',  ( -1.437007874015747477, -0.5400638737290844871, 0.3530559997133364547 ) ) ;
#55366 = CARTESIAN_POINT ( 'NONE',  ( 0.3996062992125986035, 0.1070741851644054776, -1.069553805774278166 ) ) ;
#55367 = LINE ( 'NONE', #49056, #80150 ) ;
#55368 = FACE_OUTER_BOUND ( 'NONE', #13033, .T. ) ;
#55369 = DIRECTION ( 'NONE',  ( -1.000000000000000000, 0.000000000000000000, 0.000000000000000000 ) ) ;
#55370 = CARTESIAN_POINT ( 'NONE',  ( 0.0008564280371968460877, -0.3986795681651700840, -2.755905511811023612 ) ) ;
#55371 = CARTESIAN_POINT ( 'NONE',  ( -0.2867679344610365999, 0.2867679344610364889, -0.2618110236220473341 ) ) ;
#55372 = CARTESIAN_POINT ( 'NONE',  ( -0.2887139107611542133, -0.5023911411419708095, -0.1820866141732282451 ) ) ;
#55373 = CARTESIAN_POINT ( 'NONE',  ( -1.187664041994750175, -0.08942795157528024563, -0.3641732283464568787 ) ) ;
#55374 = CARTESIAN_POINT ( 'NONE',  ( -1.653543307086613234, -0.1870078740157479769, 0.4822834645669291653 ) ) ;
#55375 = CARTESIAN_POINT ( 'NONE',  ( 0.5118110236220478892, 0.2952755905511811885, 0.000000000000000000 ) ) ;
#55376 = CARTESIAN_POINT ( 'NONE',  ( -1.522309711286088607, -0.6046776061558807314, 0.2411417322834647770 ) ) ;
#55377 = CARTESIAN_POINT ( 'NONE',  ( -9.594673741351313045E-17, 0.3917322834645670104, -0.3070866141732283006 ) ) ;
#55378 = ORIENTED_EDGE ( 'NONE', *, *, #38275, .F. ) ;
#55379 = CARTESIAN_POINT ( 'NONE',  ( -1.640419947506561060, 0.05413385826771666132, 0.4176697321401328100 ) ) ;
#55380 = DIRECTION ( 'NONE',  ( 0.000000000000000000, -0.000000000000000000, -1.000000000000000000 ) ) ;
#55381 = CARTESIAN_POINT ( 'NONE',  ( -0.4724409448818899238, 0.1265901696524986686, -1.607611548556430403 ) ) ;
#55382 = CARTESIAN_POINT ( 'NONE',  ( 0.1228903193441468061, 0.2686849592492765448, 0.1574803149606299191 ) ) ;
#55383 = CARTESIAN_POINT ( 'NONE',  ( -0.2867679344610364334, -0.2867679344610367109, -2.663385826771653253 ) ) ;
#55384 = CARTESIAN_POINT ( 'NONE',  ( -0.7677165354330699465, -0.5400638737290845981, -0.3530559997133363437 ) ) ;
#55385 = CARTESIAN_POINT ( 'NONE',  ( 1.555118110236221041, 0.1660481256975883668, -0.3530559997133364547 ) ) ;
#55387 = CARTESIAN_POINT ( 'NONE',  ( 1.614173228346456712, 0.9921945702958890889, 0.1372047244094478646 ) ) ;
#55386 = DIRECTION ( 'NONE',  ( 0.000000000000000000, 0.000000000000000000, 1.000000000000000000 ) ) ;
#55388 = CARTESIAN_POINT ( 'NONE',  ( -1.686351706036744558, 0.2952755905511810774, -0.1292274648535930714 ) ) ;
#55389 = CARTESIAN_POINT ( 'NONE',  ( -0.6102362204724400829, 0.1660481256975885056, 0.3530559997133364547 ) ) ;
#55390 = CARTESIAN_POINT ( 'NONE',  ( -0.3917322834645670659, 0.1049643490035301607, -0.5852825214885022387 ) ) ;
#55391 = CARTESIAN_POINT ( 'NONE',  ( 0.1574803149606306130, -0.1870078740157479769, 0.3641732283464567677 ) ) ;
#55392 = CARTESIAN_POINT ( 'NONE',  ( -0.1958661417322834220, -0.3392501089628018884, -0.6227034120734910028 ) ) ;
#55393 = CARTESIAN_POINT ( 'NONE',  ( -0.09842519685039295696, -0.4536011799217367080, 0.2665933059059888421 ) ) ;
#55394 = CARTESIAN_POINT ( 'NONE',  ( 0.7086614173228352742, -0.1870078740157480601, -0.3641732283464567677 ) ) ;
#55395 = CARTESIAN_POINT ( 'NONE',  ( 0.3477690288713918276, 0.2952755905511811885, 0.1292274648535926551 ) ) ;
#55396 = VECTOR ( 'NONE', #3895, 39.37007874015748143 ) ;
#55397 = CARTESIAN_POINT ( 'NONE',  ( -0.4265091863517051496, -0.5511811023622046335, 0.09757992244046803654 ) ) ;
#55398 = CARTESIAN_POINT ( 'NONE',  ( -9.594673741351313045E-17, 0.3917322834645670104, -2.511811023622047223 ) ) ;
#55399 = CARTESIAN_POINT ( 'NONE',  ( 1.522309711286089939, -0.6046776061558809534, -0.2411417322834644161 ) ) ;
#55400 = CARTESIAN_POINT ( 'NONE',  ( -1.181102362204723644, -0.1870078740157479769, 0.4822834645669291653 ) ) ;
#55401 = CARTESIAN_POINT ( 'NONE',  ( 0.4724409448818897572, -0.1265901696524988906, -0.8182414698162727706 ) ) ;
#55402 = CARTESIAN_POINT ( 'NONE',  ( -0.006561679790025524116, -0.3162353388693405765, 0.4822834645669290543 ) ) ;
#55403 = ADVANCED_FACE ( 'NONE', ( #37543 ), #75045, .T. ) ;
#55404 = CARTESIAN_POINT ( 'NONE',  ( -0.6364829396325453192, -0.05778040916215560624, -0.4822834645669293319 ) ) ;
#55405 = CARTESIAN_POINT ( 'NONE',  ( 1.515748031496063408, 0.07958543189024085140, 0.2665933059059887866 ) ) ;
#55406 = CARTESIAN_POINT ( 'NONE',  ( 5.463695987328526437E-16, -0.1870078740157479769, 0.3641732283464567677 ) ) ;
#55407 = CARTESIAN_POINT ( 'NONE',  ( -0.2887139107611542133, 0.2306618581243848609, 0.2411417322834645549 ) ) ;
#55408 = CARTESIAN_POINT ( 'NONE',  ( -0.6036745406824141069, -0.6046776061558809534, -0.2411417322834644161 ) ) ;
#55409 = CARTESIAN_POINT ( 'NONE',  ( 0.000000000000000000, 0.000000000000000000, -2.755905511811024056 ) ) ;
#55410 = CARTESIAN_POINT ( 'NONE',  ( 1.660104986876641320, -0.08942795157527998196, 0.3641732283464567121 ) ) ;
#55411 = CARTESIAN_POINT ( 'NONE',  ( 0.3149606299212606708, -0.1870078740157480879, -0.4822834645669291653 ) ) ;
#55412 = ORIENTED_EDGE ( 'NONE', *, *, #35732, .F. ) ;
#55413 = CARTESIAN_POINT ( 'NONE',  ( 0.2925321140481932369, 0.2925321140481932369, -1.789370078740157410 ) ) ;
#55414 = CARTESIAN_POINT ( 'NONE',  ( 1.030183727034121421, -0.3162353388693409650, -0.4822834645669289433 ) ) ;
#55415 = CARTESIAN_POINT ( 'NONE',  ( -0.4855643044619415427, -0.3690944881889763329, 0.3153832671262228327 ) ) ;
#55416 = CARTESIAN_POINT ( 'NONE',  ( -0.7480314960629914633, 0.2952755905511811885, 0.000000000000000000 ) ) ;
#55417 = CARTESIAN_POINT ( 'NONE',  ( 1.207349081364829990, 0.2306618581243848609, 0.2411417322834645549 ) ) ;
#55418 = CARTESIAN_POINT ( 'NONE',  ( 1.161417322834646493, -0.5400638737290844871, 0.3530559997133364547 ) ) ;
#55419 = CARTESIAN_POINT ( 'NONE',  ( -1.620734908136482577, 0.2952755905511811885, 0.1292274648535926551 ) ) ;
#55420 = CARTESIAN_POINT ( 'NONE',  ( -0.9645669291338575535, -0.4536011799217367080, 0.2665933059059888421 ) ) ;
#55421 = CARTESIAN_POINT ( 'NONE',  ( 0.1070741851644054637, -0.3996062992125984925, -0.1620734908136483299 ) ) ;
#55422 = CARTESIAN_POINT ( 'NONE',  ( 0.3996062992125986590, -0.1070741851644053111, -0.4265091863517060933 ) ) ;
#55423 = CARTESIAN_POINT ( 'NONE',  ( -0.2867679344610367109, 0.2867679344610365444, -2.851069184548242763 ) ) ;
#55424 = CARTESIAN_POINT ( 'NONE',  ( 1.476377952755906442, -0.4536011799217367080, 0.2665933059059888421 ) ) ;
#55425 = CARTESIAN_POINT ( 'NONE',  ( 1.102362204724410155, -0.1870078740157479769, 0.3641732283464567677 ) ) ;
#55426 = CARTESIAN_POINT ( 'NONE',  ( 0.3937007874015754361, -0.1870078740157480879, -0.4822834645669291653 ) ) ;
#55427 = CARTESIAN_POINT ( 'NONE',  ( -1.706036745406823485, 0.2306618581243848609, 0.2411417322834645549 ) ) ;
#55428 = CARTESIAN_POINT ( 'NONE',  ( -0.3949938075777411073, 0.1058382717557497660, -1.054461942257217899 ) ) ;
#55429 = CARTESIAN_POINT ( 'NONE',  ( 0.6233595800524942554, -0.08942795157528024563, -0.3641732283464568787 ) ) ;
#55430 = CARTESIAN_POINT ( 'NONE',  ( -0.5118110236220466680, 0.2952755905511811885, 0.000000000000000000 ) ) ;
#55431 = CARTESIAN_POINT ( 'NONE',  ( -0.7349081364829387342, -0.6046776061558807314, 0.2411417322834647770 ) ) ;
#55432 = CARTESIAN_POINT ( 'NONE',  ( 1.161417322834646493, -0.5400638737290844871, 0.3530559997133364547 ) ) ;
#55433 = CARTESIAN_POINT ( 'NONE',  ( 0.2362204724409449064, 0.4091458600556404646, -1.246719160104986734 ) ) ;
#55434 = CARTESIAN_POINT ( 'NONE',  ( 4.893765752498283924E-17, -0.3996062992125986035, -2.125984251968504157 ) ) ;
#55435 = CARTESIAN_POINT ( 'NONE',  ( 0.3149606299212603933, -0.1870078740157479769, 0.3641732283464567677 ) ) ;
#55436 = ORIENTED_EDGE ( 'NONE', *, *, #61689, .F. ) ;
#55437 = CARTESIAN_POINT ( 'NONE',  ( -9.594673741351313045E-17, 0.3917322834645670659, -0.6266597357293457460 ) ) ;
#55438 = ORIENTED_EDGE ( 'NONE', *, *, #6944, .T. ) ;
#55439 = CONICAL_SURFACE ( 'NONE', #70222, 2.637795275590551380, 0.7853981633974500554 ) ;
#55440 = CARTESIAN_POINT ( 'NONE',  ( -0.7611548556430438595, 0.2306618581243848609, 0.2411417322834645549 ) ) ;
#55441 = CARTESIAN_POINT ( 'NONE',  ( -0.03937007874015669567, 0.2952755905511811885, 0.000000000000000000 ) ) ;
#55442 = CARTESIAN_POINT ( 'NONE',  ( -0.3937007874015740483, -0.1870078740157479769, 0.4822834645669291653 ) ) ;
#55443 = CARTESIAN_POINT ( 'NONE',  ( 0.8923884514435703741, 0.2306618581243848609, 0.2411417322834645549 ) ) ;
#55444 = CARTESIAN_POINT ( 'NONE',  ( -1.161417322834644716, 0.1660481256975885056, 0.3530559997133364547 ) ) ;
#55445 = CARTESIAN_POINT ( 'NONE',  ( -0.4002624671916004129, -0.05778040916215560624, -0.4822834645669293319 ) ) ;
#55446 = CARTESIAN_POINT ( 'NONE',  ( 0.6364829396325465405, -0.05778040916215522460, 0.4822834645669289988 ) ) ;
#55447 = CARTESIAN_POINT ( 'NONE',  ( 0.3674540682414705883, 0.2306618581243847221, -0.2411417322834647770 ) ) ;
#55448 = CARTESIAN_POINT ( 'NONE',  ( -9.594673741351313045E-17, 0.3917322834645670104, -1.094488188976378007 ) ) ;
#55449 = CARTESIAN_POINT ( 'NONE',  ( -0.4002624671916004129, -0.2845877964562159024, 0.3641732283464567677 ) ) ;
#55450 = VERTEX_POINT ( 'NONE', #64045 ) ;
#55451 = CARTESIAN_POINT ( 'NONE',  ( -0.3949938075777411628, 0.1058382717557497937, -1.292650918635170676 ) ) ;
#55452 = ORIENTED_EDGE ( 'NONE', *, *, #44019, .T. ) ;
#55453 = CARTESIAN_POINT ( 'NONE',  ( -1.227034120734907585, 0.1771653543307087630, 0.09757992244046791164 ) ) ;
#55454 = CARTESIAN_POINT ( 'NONE',  ( -0.3937007874015740483, -0.1870078740157479769, 0.4822834645669291653 ) ) ;
#55455 = DIRECTION ( 'NONE',  ( 0.000000000000000000, 1.000000000000000000, 0.000000000000000000 ) ) ;
#55456 = CARTESIAN_POINT ( 'NONE',  ( -0.7742782152230965886, 0.05413385826771666132, 0.4176697321401328100 ) ) ;
#55457 = CARTESIAN_POINT ( 'NONE',  ( -0.7217847769028863381, 0.05413385826771626580, -0.4176697321401330321 ) ) ;
#55458 = CARTESIAN_POINT ( 'NONE',  ( -1.437007874015747477, 0.1660481256975883668, -0.3530559997133364547 ) ) ;
#55459 = CARTESIAN_POINT ( 'NONE',  ( 0.1181102362204724532, 0.04921259842519689481, -0.08523872084492506440 ) ) ;
#55460 = CARTESIAN_POINT ( 'NONE',  ( 0.8070866141732289112, -0.4536011799217368745, -0.2665933059059886201 ) ) ;
#55461 = CARTESIAN_POINT ( 'NONE',  ( 0.4744094488188941861, 1.553443221530653728, 1.016821367227985329 ) ) ;
#55462 = CARTESIAN_POINT ( 'NONE',  ( -9.594673741351313045E-17, 0.3917322834645670104, -0.08464566929133868212 ) ) ;
#55463 = CARTESIAN_POINT ( 'NONE',  ( 0.2165354330708668673, 0.07958543189024071263, -0.2665933059059888421 ) ) ;
#55464 = CARTESIAN_POINT ( 'NONE',  ( -0.3937007874015740483, -0.1870078740157479769, 0.4822834645669291653 ) ) ;
#55465 = CARTESIAN_POINT ( 'NONE',  ( 0.07874015748031558404, -0.1870078740157479769, 0.4822834645669291653 ) ) ;
#55466 = ORIENTED_EDGE ( 'NONE', *, *, #68728, .F. ) ;
#55467 = CARTESIAN_POINT ( 'NONE',  ( 0.1998031496062994405, -0.3460692066303958092, -2.139107611548556331 ) ) ;
#55468 = CARTESIAN_POINT ( 'NONE',  ( -0.03443470937339727228, 1.062992125984252079, -1.438590695389362573 ) ) ;
#55469 = ORIENTED_EDGE ( 'NONE', *, *, #61540, .F. ) ;
#55470 = CARTESIAN_POINT ( 'NONE',  ( -0.3996062992125985480, -7.340648628747423112E-17, -1.533464566929133799 ) ) ;
#55471 = DIRECTION ( 'NONE',  ( 1.000000000000000000, 1.408710688920637755E-15, 0.000000000000000000 ) ) ;
#55472 = CARTESIAN_POINT ( 'NONE',  ( -0.8070866141732276899, -0.4536011799217367080, 0.2665933059059888421 ) ) ;
#55473 = CARTESIAN_POINT ( 'NONE',  ( -1.122047244094487306, -0.5400638737290844871, 0.3530559997133364547 ) ) ;
#55474 = CARTESIAN_POINT ( 'NONE',  ( 5.785732909357575061E-17, -0.4724409448818898682, -0.3937007874015748254 ) ) ;
#55475 = FACE_OUTER_BOUND ( 'NONE', #14508, .T. ) ;
#55476 = CARTESIAN_POINT ( 'NONE',  ( 0.2867679344610365999, 0.2867679344610365999, -2.584645669291338876 ) ) ;
#55477 = CARTESIAN_POINT ( 'NONE',  ( 1.338582677165355062, -0.1870078740157479769, 0.4822834645669291653 ) ) ;
#55478 = CARTESIAN_POINT ( 'NONE',  ( 0.6561679790026253567, 0.2306618581243848609, 0.2411417322834645549 ) ) ;
#55479 = CARTESIAN_POINT ( 'NONE',  ( 0.4265091863517067594, 0.2952755905511811885, 0.1292274648535926551 ) ) ;
#55480 = CARTESIAN_POINT ( 'NONE',  ( -0.8267716535433065062, 0.1771653543307087630, 0.000000000000000000 ) ) ;
#55481 = B_SPLINE_CURVE_WITH_KNOTS ( 'NONE', 3,
 ( #43966, #63338, #82703, #36431 ),
 .UNSPECIFIED., .F., .F.,
 ( 4, 4 ),
 ( 3.593986969192262371E-07, 0.001287825409103120775 ),
 .UNSPECIFIED. ) ;
#55482 = CARTESIAN_POINT ( 'NONE',  ( -0.4527559055118102749, 0.1660481256975885056, 0.3530559997133364547 ) ) ;
#55483 = CARTESIAN_POINT ( 'NONE',  ( -0.3458507752293909498, 0.3458507752293907833, -2.458661417322834719 ) ) ;
#55484 = CARTESIAN_POINT ( 'NONE',  ( -0.3412073490813641308, -0.6046776061558807314, 0.2411417322834647770 ) ) ;
#55485 = CARTESIAN_POINT ( 'NONE',  ( -0.3420746716998662729, 0.1974969037888702206, -1.992782152230971882 ) ) ;
#55486 = CARTESIAN_POINT ( 'NONE',  ( 1.482939632545932307, -0.004921259842519870586, -0.3153832671262229437 ) ) ;
#55487 = CARTESIAN_POINT ( 'NONE',  ( -0.4658792650918627265, -0.08942795157527998196, 0.3641732283464567121 ) ) ;
#55488 = AXIS2_PLACEMENT_3D ( 'NONE', #54065, #53235, #59560 ) ;
#55489 = CARTESIAN_POINT ( 'NONE',  ( 1.338582677165355062, -0.1870078740157479769, 0.3641732283464567677 ) ) ;
#55490 = CARTESIAN_POINT ( 'NONE',  ( -1.154855643044618851, -0.6046776061558809534, -0.2411417322834644161 ) ) ;
#55491 = CARTESIAN_POINT ( 'NONE',  ( -0.9973753280839886548, 0.1283753931104748280, 0.1820866141732283561 ) ) ;
#55492 = CARTESIAN_POINT ( 'NONE',  ( -0.1938976377952756625, 0.1938976377952755792, 0.1574803149606299191 ) ) ;
#55493 = CARTESIAN_POINT ( 'NONE',  ( -1.286089238845143479, -0.6046776061558807314, 0.2411417322834647770 ) ) ;
#55494 = CARTESIAN_POINT ( 'NONE',  ( -0.4265091863517051496, -0.6692913385826771977, 0.1292274648535927661 ) ) ;
#55495 = CARTESIAN_POINT ( 'NONE',  ( 0.4658792650918641698, -0.05778040916215560624, -0.4822834645669293319 ) ) ;
#55496 = CARTESIAN_POINT ( 'NONE',  ( 0.1958661417322834497, 0.3392501089628018329, -2.429114542485877770 ) ) ;
#55497 = CARTESIAN_POINT ( 'NONE',  ( -2.167277156196906418, 1.503024749832831741, 0.4732391302016646928 ) ) ;
#55498 = CARTESIAN_POINT ( 'NONE',  ( 0.2230971128608932319, -0.3690944881889763329, 0.3153832671262228327 ) ) ;
#55499 = CARTESIAN_POINT ( 'NONE',  ( -1.633858267716534529, -0.4536011799217368745, -0.2665933059059886201 ) ) ;
#55500 = CARTESIAN_POINT ( 'NONE',  ( 0.7349081364829403995, 0.2306618581243848609, 0.2411417322834645549 ) ) ;
#55501 = CARTESIAN_POINT ( 'NONE',  ( -1.587926509186350810, -0.3690944881889763329, 0.3153832671262228327 ) ) ;
#55502 = AXIS2_PLACEMENT_3D ( 'NONE', #65281, #25281, #19396 ) ;
#55503 = CARTESIAN_POINT ( 'NONE',  ( 1.437007874015748810, 0.07958543189024085140, 0.2665933059059887866 ) ) ;
#55504 = CARTESIAN_POINT ( 'NONE',  ( -1.036745406824146176, 0.05413385826771626580, -0.4176697321401330321 ) ) ;
#55505 = CARTESIAN_POINT ( 'NONE',  ( -0.1115485564304453947, -0.5511811023622046335, 0.09757992244046803654 ) ) ;
#55506 = DIRECTION ( 'NONE',  ( 1.000000000000000000, -0.000000000000000000, -0.000000000000000000 ) ) ;
#55507 = CARTESIAN_POINT ( 'NONE',  ( 0.08530183727034192087, -0.2845877964562161244, -0.3641732283464567121 ) ) ;
#55508 = CARTESIAN_POINT ( 'NONE',  ( -0.2559055118110227234, -0.5400638737290844871, 0.3530559997133364547 ) ) ;
#55509 = CARTESIAN_POINT ( 'NONE',  ( -0.1998031496062994405, 0.3460692066303957537, -0.7198162729658792447 ) ) ;
#55510 = CARTESIAN_POINT ( 'NONE',  ( 0.2867679344610365999, -0.2867679344610365444, -1.915354330708661124 ) ) ;
#55511 = CARTESIAN_POINT ( 'NONE',  ( 0.4461942257217855201, -0.5023911411419708095, 0.1820866141732285504 ) ) ;
#55512 = CARTESIAN_POINT ( 'NONE',  ( 0.1443569553805781891, 0.05413385826771626580, -0.4176697321401330321 ) ) ;
#55513 = CARTESIAN_POINT ( 'NONE',  ( -0.5183727034120726440, 0.2952755905511811885, 0.1292274648535926551 ) ) ;
#55514 = CARTESIAN_POINT ( 'NONE',  ( -0.7217847769028863381, -0.3690944881889763329, 0.3153832671262228327 ) ) ;
#55515 = CYLINDRICAL_SURFACE ( 'NONE', #17239, 0.1771653543307085410 ) ;
#55516 = CARTESIAN_POINT ( 'NONE',  ( -0.5249343832020990641, 0.1283753931104748280, 0.1820866141732283561 ) ) ;
#55517 = CARTESIAN_POINT ( 'NONE',  ( 0.09842519685039434474, 0.1660481256975885056, 0.3530559997133364547 ) ) ;
#55518 = CARTESIAN_POINT ( 'NONE',  ( -1.200787401574802349, 0.07958543189024071263, -0.2665933059059888421 ) ) ;
#55519 = CARTESIAN_POINT ( 'NONE',  ( -0.3996062992125985480, -7.340648628747423112E-17, -1.533464566929134021 ) ) ;
#55520 = CARTESIAN_POINT ( 'NONE',  ( 1.515748031496063186, -0.5400638737290845981, -0.3530559997133363437 ) ) ;
#55521 = CARTESIAN_POINT ( 'NONE',  ( 0.4609447788686172331, 1.990046790791744833E-15, -0.3791475997938225651 ) ) ;
#55522 = ORIENTED_EDGE ( 'NONE', *, *, #79988, .T. ) ;
#55523 = CARTESIAN_POINT ( 'NONE',  ( -1.561679790026246017, -0.004921259842519576551, 0.3153832671262227771 ) ) ;
#55524 = CARTESIAN_POINT ( 'NONE',  ( -0.2887139107611542133, 0.2306618581243848609, 0.2411417322834645549 ) ) ;
#55525 = CARTESIAN_POINT ( 'NONE',  ( -1.299212598425196097, 0.2952755905511811885, 0.000000000000000000 ) ) ;
#55526 = CARTESIAN_POINT ( 'NONE',  ( -0.1049643490035307020, 0.3917322834645669549, -1.508530183727033736 ) ) ;
#55527 = CARTESIAN_POINT ( 'NONE',  ( 0.2362204724409451007, -0.4091458600556402980, -2.139107611548556331 ) ) ;
#55528 = CARTESIAN_POINT ( 'NONE',  ( 1.561679790026247350, 0.05413385826771626580, -0.4176697321401330321 ) ) ;
#55529 = CARTESIAN_POINT ( 'NONE',  ( 0.3543307086614181922, -0.6692913385826771977, 8.415575281601705876E-17 ) ) ;
#55530 = DIRECTION ( 'NONE',  ( 0.000000000000000000, 0.000000000000000000, 1.000000000000000000 ) ) ;
#55531 = CARTESIAN_POINT ( 'NONE',  ( 0.3996062992125985480, -0.1070741851644052972, -2.235564304461942431 ) ) ;
#55532 = CARTESIAN_POINT ( 'NONE',  ( 1.463254593175853824, 0.1771653543307087075, -0.09757992244046823083 ) ) ;
#55533 = CARTESIAN_POINT ( 'NONE',  ( -0.1998031496062994683, 0.3460692066303958092, -0.8005249343832020470 ) ) ;
#55534 = VERTEX_POINT ( 'NONE', #49756 ) ;
#55535 = CARTESIAN_POINT ( 'NONE',  ( -1.017060367454067249, -0.08942795157527998196, 0.3641732283464567121 ) ) ;
#55536 = CARTESIAN_POINT ( 'NONE',  ( -0.2867679344610365999, 0.2867679344610364889, -2.846456692913385655 ) ) ;
#55537 = ORIENTED_EDGE ( 'NONE', *, *, #43837, .F. ) ;
#55538 = CARTESIAN_POINT ( 'NONE',  ( 0.3280839895013130669, 0.05413385826771666132, 0.4176697321401328100 ) ) ;
#55539 = CARTESIAN_POINT ( 'NONE',  ( -0.4002624671916004129, -0.05778040916215560624, -0.4822834645669293319 ) ) ;
#55540 = CARTESIAN_POINT ( 'NONE',  ( -1.122047244094487306, 0.1660481256975883668, -0.3530559997133364547 ) ) ;
#55541 = CARTESIAN_POINT ( 'NONE',  ( 1.062992125984252745, 0.2952755905511811885, 0.000000000000000000 ) ) ;
#55542 = CIRCLE ( 'NONE', #38121, 3.405511811023621771 ) ;
#55543 = CARTESIAN_POINT ( 'NONE',  ( -1.404199475065615932, -0.3690944881889765550, -0.3153832671262227771 ) ) ;
#55544 = FACE_OUTER_BOUND ( 'NONE', #74101, .T. ) ;
#55545 = CARTESIAN_POINT ( 'NONE',  ( 0.08530183727034192087, -0.05778040916215522460, 0.4822834645669289988 ) ) ;
#55546 = CARTESIAN_POINT ( 'NONE',  ( -0.9908136482939626788, 0.2952755905511811885, 0.1292274648535926551 ) ) ;
#55547 = CARTESIAN_POINT ( 'NONE',  ( -0.3917322834645670659, 0.1049643490035301607, -1.845125041173541369 ) ) ;
#55548 = CARTESIAN_POINT ( 'NONE',  ( -1.581364829396324945, -0.05778040916215560624, -0.4822834645669293319 ) ) ;
#55549 = DIRECTION ( 'NONE',  ( -0.000000000000000000, -1.000000000000000000, -0.000000000000000000 ) ) ;
#55550 = CARTESIAN_POINT ( 'NONE',  ( -0.3917322834645671215, 0.1049643490035301469, 0.1325459317585302443 ) ) ;
#55551 = CARTESIAN_POINT ( 'NONE',  ( 1.043307086614173818, 0.07958543189024085140, 0.2665933059059887866 ) ) ;
#55552 = VERTEX_POINT ( 'NONE', #17794 ) ;
#55553 = CARTESIAN_POINT ( 'NONE',  ( -0.2891555358219908833, -0.2891555358219912164, -0.05905511811023628904 ) ) ;
#55554 = CARTESIAN_POINT ( 'NONE',  ( -0.8333333333333323711, 0.2952755905511811885, 0.1292274648535926551 ) ) ;
#55555 = EDGE_LOOP ( 'NONE', ( #31943, #18613, #52446, #36955 ) ) ;
#55556 = CARTESIAN_POINT ( 'NONE',  ( 0.3674540682414705883, 0.1283753931104746893, -0.1820866141732285504 ) ) ;
#55557 = CARTESIAN_POINT ( 'NONE',  ( -1.679790026246718693, 0.2306618581243847221, -0.2411417322834647770 ) ) ;
#55558 = CARTESIAN_POINT ( 'NONE',  ( 0.7414698162729663755, -0.6692913385826773087, -0.1292274648535924053 ) ) ;
#55559 = CARTESIAN_POINT ( 'NONE',  ( 0.4986876640419954376, 0.2306618581243848609, 0.2411417322834645549 ) ) ;
#55560 = CARTESIAN_POINT ( 'NONE',  ( -0.2362204724409442680, -0.1870078740157480879, -0.4822834645669291653 ) ) ;
#55561 = VECTOR ( 'NONE', #18608, 39.37007874015748143 ) ;
#55562 = CARTESIAN_POINT ( 'NONE',  ( -0.2867679344610367109, 0.2867679344610365444, -1.276266034941944127 ) ) ;
#55563 = CARTESIAN_POINT ( 'NONE',  ( -0.9776902887139098386, 0.2952755905511810774, -0.1292274648535930714 ) ) ;
#55564 = CARTESIAN_POINT ( 'NONE',  ( 0.2867679344610365999, 0.2867679344610365999, -2.112204724409449064 ) ) ;
#55565 = CARTESIAN_POINT ( 'NONE',  ( 1.430446194225722500, -0.004921259842519576551, 0.3153832671262227771 ) ) ;
#55566 = CARTESIAN_POINT ( 'NONE',  ( -1.154855643044618851, 0.2306618581243848609, 0.2411417322834645549 ) ) ;
#55567 = CARTESIAN_POINT ( 'NONE',  ( 1.200787401574803681, 0.1660481256975885056, 0.3530559997133364547 ) ) ;
#55568 = CARTESIAN_POINT ( 'NONE',  ( 1.325459317585302665, -0.4281496062992124485, 0.4176697321401328655 ) ) ;
#55569 = CARTESIAN_POINT ( 'NONE',  ( -0.3996062992125986035, -7.340648628747425578E-17, -0.3543307086614173040 ) ) ;
#55570 = CARTESIAN_POINT ( 'NONE',  ( -0.7283464566929126471, 0.1660481256975883668, -0.3530559997133364547 ) ) ;
#55571 = CARTESIAN_POINT ( 'NONE',  ( 0.1070741851644054776, -0.3996062992125984925, -0.004593175853018378711 ) ) ;
#55572 = CARTESIAN_POINT ( 'NONE',  ( 0.1115485564304467270, -0.6692913385826773087, -0.1292274648535924053 ) ) ;
#55573 = CARTESIAN_POINT ( 'NONE',  ( 0.2925321140481932369, 0.2925321140481932369, -2.342519685039369914 ) ) ;
#55574 = CARTESIAN_POINT ( 'NONE',  ( -0.4461942257217840213, -0.6046776061558809534, -0.2411417322834644161 ) ) ;
#55575 = CARTESIAN_POINT ( 'NONE',  ( -1.555118110236219930, -0.4536011799217368745, -0.2665933059059886201 ) ) ;
#55576 = CARTESIAN_POINT ( 'NONE',  ( 0.7086614173228353852, -0.1870078740157479769, 0.3641732283464567677 ) ) ;
#55577 = CARTESIAN_POINT ( 'NONE',  ( 1.148293963254593653, 0.2952755905511810774, -0.1292274648535930714 ) ) ;
#55578 = CARTESIAN_POINT ( 'NONE',  ( -0.1265901696524986964, -0.4724409448818899238, -1.093832020997375087 ) ) ;
#55579 = CARTESIAN_POINT ( 'NONE',  ( 0.9186351706036752773, 0.1283753931104746893, -0.1820866141732285504 ) ) ;
#55580 = CARTESIAN_POINT ( 'NONE',  ( 1.003937007874016185, 0.1660481256975883668, -0.3530559997133364547 ) ) ;
#55581 = CARTESIAN_POINT ( 'NONE',  ( -0.1974969037888706924, 0.3420746716998658843, -0.7198162729658792447 ) ) ;
#55582 = CARTESIAN_POINT ( 'NONE',  ( -0.6364829396325453192, -0.3162353388693405765, 0.4822834645669290543 ) ) ;
#55583 = FACE_OUTER_BOUND ( 'NONE', #2696, .T. ) ;
#55584 = CARTESIAN_POINT ( 'NONE',  ( 1.535433070866142335, -0.5511811023622047445, 6.969142054262312111E-17 ) ) ;
#55585 = CARTESIAN_POINT ( 'NONE',  ( -0.4790026246719154557, -0.3162353388693405765, 0.4822834645669290543 ) ) ;
#55586 = CARTESIAN_POINT ( 'NONE',  ( -0.006561679790025524116, -0.3162353388693405765, 0.4822834645669290543 ) ) ;
#55587 = CARTESIAN_POINT ( 'NONE',  ( -3.264097702071373064, 2.755905511811024056, 0.5314960629921260393 ) ) ;
#55588 = CARTESIAN_POINT ( 'NONE',  ( 0.1443569553805781891, -0.4281496062992124485, 0.4176697321401328655 ) ) ;
#55589 = CARTESIAN_POINT ( 'NONE',  ( 0.1181102362204730916, 0.1771653543307087630, 0.000000000000000000 ) ) ;
#55590 = CARTESIAN_POINT ( 'NONE',  ( -2.867114984585481974, 1.070443199938759138, 0.08545185031214221072 ) ) ;
#55591 = CARTESIAN_POINT ( 'NONE',  ( 0.05905511811023709395, -0.4536011799217367080, 0.2665933059059888421 ) ) ;
#55592 = CARTESIAN_POINT ( 'NONE',  ( 0.6496062992125991586, 0.07958543189024085140, 0.2665933059059887866 ) ) ;
#55593 = CARTESIAN_POINT ( 'NONE',  ( -0.7426113562971995430, 2.793565526369265584, -0.5309055118110234117 ) ) ;
#55594 = CARTESIAN_POINT ( 'NONE',  ( -0.3460692066303957537, -0.1998031496062994405, -1.546587926509186639 ) ) ;
#55595 = CARTESIAN_POINT ( 'NONE',  ( 0.4133858267716541968, 0.1660481256975885056, 0.3530559997133364547 ) ) ;
#55596 = EDGE_CURVE ( 'NONE', #79730, #32076, #26381, .T. ) ;
#55597 = CARTESIAN_POINT ( 'NONE',  ( 0.3917322834645669549, 0.1049643490035304660, -1.691601049868766360 ) ) ;
#55598 = CARTESIAN_POINT ( 'NONE',  ( 1.391076115485564868, 0.1283753931104746893, -0.1820866141732285504 ) ) ;
#55599 = CARTESIAN_POINT ( 'NONE',  ( -0.3876764156950357476, -0.05722014593895402568, 1.721458645558463398E-17 ) ) ;
#55600 = CARTESIAN_POINT ( 'NONE',  ( -0.2099737532808391705, -0.5023911411419708095, -0.1820866141732282451 ) ) ;
#55601 = CARTESIAN_POINT ( 'NONE',  ( -0.3871391076115476282, -0.05778040916215522460, 0.4822834645669289988 ) ) ;
#55602 = CARTESIAN_POINT ( 'NONE',  ( 0.9973753280839902091, -0.5023911411419708095, 0.1820866141732285504 ) ) ;
#55603 = CARTESIAN_POINT ( 'NONE',  ( -1.614173228346456268, -0.5511811023622047445, 6.969142054262312111E-17 ) ) ;
#55604 = CARTESIAN_POINT ( 'NONE',  ( -1.358267716535432434, 0.1660481256975883668, -0.3530559997133364547 ) ) ;
#55605 = VECTOR ( 'NONE', #34547, 39.37007874015748143 ) ;
#55606 = CARTESIAN_POINT ( 'NONE',  ( 8.195543980992789655E-16, -0.1870078740157480879, -0.4822834645669291653 ) ) ;
#55607 = CARTESIAN_POINT ( 'NONE',  ( 1.233595800524935227, 0.2306618581243847221, -0.2411417322834647770 ) ) ;
#55608 = CARTESIAN_POINT ( 'NONE',  ( 0.4606671848300903926, 1.422950954677614011, -2.139052088108191807 ) ) ;
#55609 = CARTESIAN_POINT ( 'NONE',  ( 0.2559055118110243332, -0.5400638737290845981, -0.3530559997133363437 ) ) ;
#55610 = CARTESIAN_POINT ( 'NONE',  ( 1.417322834645670104, -0.1870078740157480879, -0.4822834645669291653 ) ) ;
#55611 = CARTESIAN_POINT ( 'NONE',  ( 0.7742782152230979209, 0.05413385826771626580, -0.4176697321401330321 ) ) ;
#55612 = CARTESIAN_POINT ( 'NONE',  ( -1.666666666666665853, -0.004921259842519870586, -0.3153832671262229437 ) ) ;
#55613 = CARTESIAN_POINT ( 'NONE',  ( 0.5905511811023629321, 0.1771653543307087630, 0.000000000000000000 ) ) ;
#55614 = CARTESIAN_POINT ( 'NONE',  ( 1.627296587926509996, -0.6046776061558807314, 0.2411417322834647770 ) ) ;
#55615 = CARTESIAN_POINT ( 'NONE',  ( 0.2362204724409456558, -0.1870078740157480601, -0.3641732283464567677 ) ) ;
#55616 = CIRCLE ( 'NONE', #48899, 3.937007874015748143 ) ;
#55617 = CARTESIAN_POINT ( 'NONE',  ( -0.4068241469816264999, -0.4281496062992124485, 0.4176697321401328655 ) ) ;
#55618 = CARTESIAN_POINT ( 'NONE',  ( 0.5314960629921264834, 0.1660481256975883668, -0.3530559997133364547 ) ) ;
#55619 = CARTESIAN_POINT ( 'NONE',  ( -0.3608923884514428360, 0.2952755905511811885, 0.1292274648535926551 ) ) ;
#55620 = ADVANCED_FACE ( 'NONE', ( #32895 ), #72458, .F. ) ;
#55621 = CARTESIAN_POINT ( 'NONE',  ( -0.3917322834645671770, 0.1049643490035302024, -2.234271284285776371 ) ) ;
#55622 = CARTESIAN_POINT ( 'NONE',  ( -0.1968503937007867743, -0.5511811023622047445, 6.969142054262312111E-17 ) ) ;
#55623 = CARTESIAN_POINT ( 'NONE',  ( 0.9055118110236227702, -0.6692913385826771977, 8.415575281601705876E-17 ) ) ;
#55624 = CARTESIAN_POINT ( 'NONE',  ( 0.8923884514435703741, 0.1283753931104748280, 0.1820866141732283561 ) ) ;
#55625 = CARTESIAN_POINT ( 'NONE',  ( 0.2427821522309719648, -0.05778040916215522460, 0.4822834645669289988 ) ) ;
#55626 = CARTESIAN_POINT ( 'NONE',  ( -1.607431655553806182, 1.132464663736809873, 0.2471720702981345663 ) ) ;
#55628 = CARTESIAN_POINT ( 'NONE',  ( -0.3460692066303960868, 0.1998031496062990242, -1.128608923884514503 ) ) ;
#55627 = CARTESIAN_POINT ( 'NONE',  ( 1.600415083108465142, 1.509172534626478823, 0.1324231768467332149 ) ) ;
#55629 = CARTESIAN_POINT ( 'NONE',  ( 0.3917322834645670104, -0.1049643490035303273, -2.150918635170603554 ) ) ;
#55630 = CARTESIAN_POINT ( 'NONE',  ( -1.417322834645668772, -0.1870078740157480879, -0.4822834645669291653 ) ) ;
#55631 = CARTESIAN_POINT ( 'NONE',  ( -0.5446194225721777693, -0.3162353388693409650, -0.4822834645669289433 ) ) ;
#55632 = CARTESIAN_POINT ( 'NONE',  ( -0.3996062992125987146, 0.1070741851644051862, -2.867454068241469756 ) ) ;
#55633 = CARTESIAN_POINT ( 'NONE',  ( 0.1058382717557499880, 0.3949938075777411073, -2.828083989501312345 ) ) ;
#55634 = EDGE_LOOP ( 'NONE', ( #51098, #79495, #62818, #66027 ) ) ;
#55635 = CARTESIAN_POINT ( 'NONE',  ( 0.3871391076115493490, -0.2845877964562159024, 0.3641732283464567677 ) ) ;
#55636 = CARTESIAN_POINT ( 'NONE',  ( 0.2867679344610365999, -0.2867679344610365444, -1.192913385826771755 ) ) ;
#55637 = CARTESIAN_POINT ( 'NONE',  ( 1.272965879265092637, 0.05413385826771666132, 0.4176697321401328100 ) ) ;
#55638 = CARTESIAN_POINT ( 'NONE',  ( -0.4724409448818898682, -8.678599364036362592E-17, -2.401574803149606474 ) ) ;
#55639 = CARTESIAN_POINT ( 'NONE',  ( 1.003937007874016185, 0.1660481256975883391, -0.3530559997133364547 ) ) ;
#55640 = FILL_AREA_STYLE ('',( #48923 ) ) ;
#55641 = CARTESIAN_POINT ( 'NONE',  ( 1.692913385826772421, 0.2952755905511811885, 0.000000000000000000 ) ) ;
#55642 = CARTESIAN_POINT ( 'NONE',  ( 1.187664041994751285, -0.2845877964562161244, -0.3641732283464567121 ) ) ;
#55643 = CARTESIAN_POINT ( 'NONE',  ( 0.4461942257217856311, 0.2306618581243847221, -0.2411417322834647770 ) ) ;
#55644 = CARTESIAN_POINT ( 'NONE',  ( -0.1958661417322834497, -0.3392501089628018884, -0.3031302905173735573 ) ) ;
#55645 = CARTESIAN_POINT ( 'NONE',  ( -0.5118110236220466680, 0.2952755905511811885, 0.000000000000000000 ) ) ;
#55646 = CARTESIAN_POINT ( 'NONE',  ( -0.7677165354330699465, 0.07958543189024085140, 0.2665933059059887866 ) ) ;
#55647 = ADVANCED_FACE ( 'NONE', ( #71619 ), #1753, .T. ) ;
#55648 = CARTESIAN_POINT ( 'NONE',  ( 0.3608923884514443348, 0.2952755905511810774, -0.1292274648535930714 ) ) ;
#55649 = CARTESIAN_POINT ( 'NONE',  ( -0.2690288713910754526, 0.2952755905511810774, -0.1292274648535930714 ) ) ;
#55650 = DIRECTION ( 'NONE',  ( 0.000000000000000000, 0.000000000000000000, 1.000000000000000000 ) ) ;
#55651 = DIRECTION ( 'NONE',  ( 0.000000000000000000, 0.000000000000000000, 1.000000000000000000 ) ) ;
#55652 = CARTESIAN_POINT ( 'NONE',  ( -0.1049643490035302301, -0.3917322834645671770, -1.801200418144043969 ) ) ;
#55653 = CARTESIAN_POINT ( 'NONE',  ( 0.8070866141732289112, -0.5400638737290845981, -0.3530559997133363437 ) ) ;
#55654 = CARTESIAN_POINT ( 'NONE',  ( -0.4199475065616791736, 0.2306618581243847221, -0.2411417322834647770 ) ) ;
#55655 = CARTESIAN_POINT ( 'NONE',  ( -1.384514435695537005, -0.6692913385826773087, -0.1292274648535924053 ) ) ;
#55656 = CARTESIAN_POINT ( 'NONE',  ( 1.194225721784777594, -0.4281496062992127816, -0.4176697321401328100 ) ) ;
#55657 = CARTESIAN_POINT ( 'NONE',  ( 0.3805774278215230400, -0.4281496062992124485, 0.4176697321401328655 ) ) ;
#55658 = CARTESIAN_POINT ( 'NONE',  ( -0.1958661417322834220, -0.3392501089628018884, -0.7801837270341208663 ) ) ;
#55659 = CARTESIAN_POINT ( 'NONE',  ( -0.2624671916010490880, 0.2306618581243847221, -0.2411417322834647770 ) ) ;
#55660 = CARTESIAN_POINT ( 'NONE',  ( 0.3346456692913393205, -0.5400638737290845981, -0.3530559997133363437 ) ) ;
#55661 = CARTESIAN_POINT ( 'NONE',  ( -0.5118110236220466680, 0.2952755905511811885, 0.000000000000000000 ) ) ;
#55662 = VECTOR ( 'NONE', #76417, 39.37007874015748143 ) ;
#55663 = CARTESIAN_POINT ( 'NONE',  ( 0.3871391076115493490, -0.2845877964562159024, 0.3641732283464567677 ) ) ;
#55664 = CARTESIAN_POINT ( 'NONE',  ( 1.607611548556431069, -0.5511811023622048555, -0.09757992244046775898 ) ) ;
#55665 = CARTESIAN_POINT ( 'NONE',  ( -0.3006999498584465025, 1.170162153792019710, -2.776607427673829509 ) ) ;
#55666 = CARTESIAN_POINT ( 'NONE',  ( 0.2821522309711292364, -0.6692913385826771977, 0.1292274648535927661 ) ) ;
#55667 = SURFACE_STYLE_USAGE ( .BOTH. , #10253 ) ;
#55668 = CARTESIAN_POINT ( 'NONE',  ( 1.437007874015748810, 0.1660481256975885056, 0.3530559997133364547 ) ) ;
#55669 = CARTESIAN_POINT ( 'NONE',  ( -0.1049643490035302024, -0.3917322834645671215, -2.898950131233595684 ) ) ;
#55670 = ORIENTED_EDGE ( 'NONE', *, *, #17268, .T. ) ;
#55671 = VERTEX_POINT ( 'NONE', #51816 ) ;
#55672 = CARTESIAN_POINT ( 'NONE',  ( 0.8858267716535438430, 0.1660481256975885056, 0.3530559997133364547 ) ) ;
#55673 = CARTESIAN_POINT ( 'NONE',  ( 0.08530183727034192087, -0.2845877964562161244, -0.3641732283464567121 ) ) ;
#55675 = CARTESIAN_POINT ( 'NONE',  ( -1.220472440944882386, -0.1870078740157480046, 1.254653134982923898E-17 ) ) ;
#55674 = CARTESIAN_POINT ( 'NONE',  ( 0.9573014326657177664, 0.000000000000000000, 0.3464511005275205946 ) ) ;
#55676 = CARTESIAN_POINT ( 'NONE',  ( 0.3917322834645669549, 0.1049643490035304660, -0.8392388451443569819 ) ) ;
#55677 = CARTESIAN_POINT ( 'NONE',  ( -0.9555810825238836292, -3.764720552277026557E-15, -0.4118477457933000796 ) ) ;
#55678 = CARTESIAN_POINT ( 'NONE',  ( 0.4623158380715545746, 0.02617651024168223331, -2.142213561789874543 ) ) ;
#55679 = VECTOR ( 'NONE', #75744, 39.37007874015748143 ) ;
#55680 = CARTESIAN_POINT ( 'NONE',  ( 4.893765752498283308E-17, -0.3996062992125985480, -2.517716535433071279 ) ) ;
#55681 =( REPRESENTATION_RELATIONSHIP ('NONE','NONE', #79348, #7298 ) REPRESENTATION_RELATIONSHIP_WITH_TRANSFORMATION ( #80579 )SHAPE_REPRESENTATION_RELATIONSHIP( ) );
#55682 = CARTESIAN_POINT ( 'NONE',  ( 0.5971128608923890191, -0.6692913385826771977, 0.1292274648535927661 ) ) ;
#55683 = CARTESIAN_POINT ( 'NONE',  ( -0.9383202099737524282, -0.3162353388693409650, -0.4822834645669289433 ) ) ;
#55684 = CARTESIAN_POINT ( 'NONE',  ( -0.8923884514435688198, 0.2306618581243847221, -0.2411417322834647770 ) ) ;
#55685 = CARTESIAN_POINT ( 'NONE',  ( 0.7086614173228352742, -0.1870078740157480879, -0.4822834645669291653 ) ) ;
#55686 = CARTESIAN_POINT ( 'NONE',  ( 1.522309711286089939, -0.6046776061558809534, -0.2411417322834644161 ) ) ;
#55687 = CARTESIAN_POINT ( 'NONE',  ( 1.220472440944882608, 0.1771653543307087630, 0.000000000000000000 ) ) ;
#55688 = CARTESIAN_POINT ( 'NONE',  ( 1.450131233595801428, -0.5511811023622048555, -0.09757992244046775898 ) ) ;
#55689 = CARTESIAN_POINT ( 'NONE',  ( -0.9317585301837263412, -0.4281496062992127816, -0.4176697321401328100 ) ) ;
#55690 = CARTESIAN_POINT ( 'NONE',  ( -9.787531504996566615E-17, 0.3996062992125985480, -0.5492125984251968740 ) ) ;
#55691 = CARTESIAN_POINT ( 'NONE',  ( 1.430446194225722500, -0.4281496062992127816, -0.4176697321401328100 ) ) ;
#55692 = DIRECTION ( 'NONE',  ( 0.000000000000000000, 1.000000000000000000, 0.000000000000000000 ) ) ;
#55693 = CARTESIAN_POINT ( 'NONE',  ( -0.3280839895013117347, 0.05413385826771626580, -0.4176697321401330321 ) ) ;
#55695 = CARTESIAN_POINT ( 'NONE',  ( -0.7478466213799878082, 1.968503937007873850, 0.5309055118110236338 ) ) ;
#55694 = CARTESIAN_POINT ( 'NONE',  ( 1.128608923884515169, -0.6046776061558809534, -0.2411417322834644161 ) ) ;
#55696 = CARTESIAN_POINT ( 'NONE',  ( -1.062992125984250968, 0.1771653543307087630, 0.000000000000000000 ) ) ;
#55697 = CARTESIAN_POINT ( 'NONE',  ( 0.4724409448818904789, -0.1870078740157480879, -0.4822834645669291653 ) ) ;
#55698 = CARTESIAN_POINT ( 'NONE',  ( 0.7283464566929140904, -0.4536011799217368745, -0.2665933059059886201 ) ) ;
#55699 = CARTESIAN_POINT ( 'NONE',  ( 0.3392501089628018329, -0.1958661417322834497, -1.602342888942570154 ) ) ;
#55700 = CARTESIAN_POINT ( 'NONE',  ( -1.292650918635170010, -0.5511811023622046335, 0.09757992244046803654 ) ) ;
#55701 = CARTESIAN_POINT ( 'NONE',  ( 1.561679790026247350, 0.05413385826771626580, -0.4176697321401330321 ) ) ;
#55702 = DIRECTION ( 'NONE',  ( 0.000000000000000000, 0.000000000000000000, 1.000000000000000000 ) ) ;
#55703 = CARTESIAN_POINT ( 'NONE',  ( -0.1640419947506555343, -0.2845877964562159024, 0.3641732283464567677 ) ) ;
#55704 = CARTESIAN_POINT ( 'NONE',  ( -0.09186351706036689768, 0.05413385826771626580, -0.4176697321401330321 ) ) ;
#55705 = CARTESIAN_POINT ( 'NONE',  ( -1.227034120734907141, -0.5511811023622048555, -0.09757992244046775898 ) ) ;
#55706 = CARTESIAN_POINT ( 'NONE',  ( -0.7414698162729651543, 0.2952755905511810774, -0.1292274648535930714 ) ) ;
#55707 = CARTESIAN_POINT ( 'NONE',  ( 1.332020997375329197, -0.3162353388693405765, 0.4822834645669290543 ) ) ;
#55708 = CARTESIAN_POINT ( 'NONE',  ( 0.3392501089628018884, -0.1958661417322833942, -0.4166859824485057984 ) ) ;
#55709 = CARTESIAN_POINT ( 'NONE',  ( -0.9120734908136475250, -0.5511811023622048555, -0.09757992244046775898 ) ) ;
#55710 = DIRECTION ( 'NONE',  ( 1.000000000000000000, 0.000000000000000000, -1.692413147294446216E-16 ) ) ;
#55711 = CARTESIAN_POINT ( 'NONE',  ( 1.594488188976378673, 0.1660481256975885056, 0.3530559997133364547 ) ) ;
#55712 = CARTESIAN_POINT ( 'NONE',  ( 5.785732909357575061E-17, -0.4724409448818898682, -2.202755905511811108 ) ) ;
#55713 = CARTESIAN_POINT ( 'NONE',  ( -1.017060367454067249, -0.3162353388693409650, -0.4822834645669289433 ) ) ;
#55714 = CARTESIAN_POINT ( 'NONE',  ( -1.272965879265091305, -0.004921259842519870586, -0.3153832671262229437 ) ) ;
#55715 = CARTESIAN_POINT ( 'NONE',  ( -0.7283464566929126471, 0.07958543189024071263, -0.2665933059059888421 ) ) ;
#55716 = LINE ( 'NONE', #81426, #16493 ) ;
#55717 = CARTESIAN_POINT ( 'NONE',  ( 0.09842519685039434474, 0.1660481256975885056, 0.3530559997133364547 ) ) ;
#55718 = CARTESIAN_POINT ( 'NONE',  ( -0.1968503937007867743, 0.1771653543307087630, 0.000000000000000000 ) ) ;
#55719 = CARTESIAN_POINT ( 'NONE',  ( -1.325459317585300889, -0.3690944881889765550, -0.3153832671262227771 ) ) ;
#55720 = CARTESIAN_POINT ( 'NONE',  ( -1.338582677165353729, -0.1870078740157480879, -0.4822834645669291653 ) ) ;
#55721 = CARTESIAN_POINT ( 'NONE',  ( 1.312335958005249825, 0.1283753931104746893, -0.1820866141732285504 ) ) ;
#55722 = CARTESIAN_POINT ( 'NONE',  ( 0.7611548556430454138, 0.2306618581243847221, -0.2411417322834647770 ) ) ;
#55723 = CARTESIAN_POINT ( 'NONE',  ( 0.4124503923812352646, 1.301275207309030346, 2.058161246854230519 ) ) ;
#55724 = CARTESIAN_POINT ( 'NONE',  ( 0.2427821522309719648, -0.08942795157527998196, 0.3641732283464567121 ) ) ;
#55725 = VECTOR ( 'NONE', #22868, 39.37007874015748854 ) ;
#55726 = CARTESIAN_POINT ( 'NONE',  ( 0.7611548556430454138, 0.2306618581243847221, -0.2411417322834647770 ) ) ;
#55727 = EDGE_CURVE ( 'NONE', #51415, #52887, #74585, .T. ) ;
#55728 = CARTESIAN_POINT ( 'NONE',  ( 0.9055118110236227702, -0.5511811023622047445, 6.969142054262312111E-17 ) ) ;
#55729 = VERTEX_POINT ( 'NONE', #19429 ) ;
#55730 = CARTESIAN_POINT ( 'NONE',  ( -1.351706036745406347, -0.4281496062992124485, 0.4176697321401328655 ) ) ;
#55731 = ADVANCED_FACE ( 'NONE', ( #57716 ), #3071, .F. ) ;
#55732 = CARTESIAN_POINT ( 'NONE',  ( -0.8136482939632537770, 0.2306618581243847221, -0.2411417322834647770 ) ) ;
#55733 = CARTESIAN_POINT ( 'NONE',  ( -0.2427821522309703550, -0.05778040916215560624, -0.4822834645669293319 ) ) ;
#55734 = CARTESIAN_POINT ( 'NONE',  ( -1.699475065616797398, 0.1771653543307087630, 0.09757992244046791164 ) ) ;
#55735 = CARTESIAN_POINT ( 'NONE',  ( 0.2925321140481932369, 0.2925321140481932369, -2.419291338582676865 ) ) ;
#55736 = CARTESIAN_POINT ( 'NONE',  ( 1.082677165354331228, -0.5400638737290844871, 0.3530559997133364547 ) ) ;
#55737 = CARTESIAN_POINT ( 'NONE',  ( 1.496062992125984703, -0.1870078740157480601, -0.3641732283464567677 ) ) ;
#55738 = CARTESIAN_POINT ( 'NONE',  ( -0.06561679790026180015, 0.05413385826771666132, 0.4176697321401328100 ) ) ;
#55739 = CARTESIAN_POINT ( 'NONE',  ( 0.7283464566929140904, -0.5400638737290845981, -0.3530559997133363437 ) ) ;
#55740 = CARTESIAN_POINT ( 'NONE',  ( -0.1070741851644056997, 0.3996062992125986035, -1.738845144356955696 ) ) ;
#55741 = CARTESIAN_POINT ( 'NONE',  ( 0.3420746716998660508, -0.1974969037888703871, -1.679790026246719359 ) ) ;
#55742 = LINE ( 'NONE', #75543, #31265 ) ;
#55743 = CARTESIAN_POINT ( 'NONE',  ( -1.614173228346456712, 0.9921945702958917535, -0.1372047244094478091 ) ) ;
#55744 = CARTESIAN_POINT ( 'NONE',  ( 0.1958661417322836440, -0.3392501089628017219, -0.5564304461942257696 ) ) ;
#55745 = CARTESIAN_POINT ( 'NONE',  ( -0.5905511811023615998, 0.1771653543307087630, 0.000000000000000000 ) ) ;
#55746 = CARTESIAN_POINT ( 'NONE',  ( -0.7874015748031489847, -0.1870078740157479769, 0.4822834645669291653 ) ) ;
#55747 = CARTESIAN_POINT ( 'NONE',  ( 0.6561679790026253567, 0.2306618581243848609, 0.2411417322834645549 ) ) ;
#55748 = CARTESIAN_POINT ( 'NONE',  ( -0.3949938075777409963, -7.255918531996591613E-17, -2.163385826771653697 ) ) ;
#55749 = ADVANCED_FACE ( 'NONE', ( #68025 ), #42326, .F. ) ;
#55750 = CARTESIAN_POINT ( 'NONE',  ( -1.364829396325458521, -0.6046776061558807314, 0.2411417322834647770 ) ) ;
#55751 = CARTESIAN_POINT ( 'NONE',  ( 1.207349081364829990, -0.6046776061558809534, -0.2411417322834644161 ) ) ;
#55752 = CARTESIAN_POINT ( 'NONE',  ( -0.2362204724409447953, -0.4091458600556404646, -2.270341207349081181 ) ) ;
#55753 = CARTESIAN_POINT ( 'NONE',  ( -0.1070741851644056997, 0.3996062992125986035, -1.581364829396325389 ) ) ;
#55754 = CARTESIAN_POINT ( 'NONE',  ( 0.3307086614173228023, 0.3647102339900947787, 0.000000000000000000 ) ) ;
#55755 = EDGE_CURVE ( 'NONE', #38486, #41807, #75891, .T. ) ;
#55756 = CARTESIAN_POINT ( 'NONE',  ( 0.7939632545931766261, -0.05778040916215522460, 0.4822834645669289988 ) ) ;
#55757 = CARTESIAN_POINT ( 'NONE',  ( 0.6430446194225728496, 0.05413385826771666132, 0.4176697321401328100 ) ) ;
#55758 = CARTESIAN_POINT ( 'NONE',  ( 1.358267716535433323, -0.4536011799217368745, -0.2665933059059886201 ) ) ;
#55760 = CARTESIAN_POINT ( 'NONE',  ( 1.607611548556431069, 0.2952755905511811885, 0.1292274648535926551 ) ) ;
#55759 = CARTESIAN_POINT ( 'NONE',  ( -1.541994750656167090, -0.5511811023622048555, -0.09757992244046775898 ) ) ;
#55761 = CARTESIAN_POINT ( 'NONE',  ( 0.3392501089628018329, 0.1958661417322835052, -2.730951812827084435 ) ) ;
#55762 = CARTESIAN_POINT ( 'NONE',  ( 1.017060367454068803, -0.3162353388693405765, 0.4822834645669290543 ) ) ;
#55763 = CARTESIAN_POINT ( 'NONE',  ( 2.795275590551181910, 1.535433070866142335, 0.000000000000000000 ) ) ;
#55764 = CARTESIAN_POINT ( 'NONE',  ( -0.4790026246719154557, -0.3162353388693405765, 0.4822834645669290543 ) ) ;
#55765 = CARTESIAN_POINT ( 'NONE',  ( -0.7414698162729651543, 0.2952755905511810774, -0.1292274648535930714 ) ) ;
#55766 = CARTESIAN_POINT ( 'NONE',  ( -1.515748031496062076, -0.5400638737290844871, 0.3530559997133364547 ) ) ;
#55767 = CARTESIAN_POINT ( 'NONE',  ( -0.2867679344610364334, -0.2867679344610367109, -0.1437007874015748810 ) ) ;
#55768 = CARTESIAN_POINT ( 'NONE',  ( 0.2296587926509192634, -0.05778040916215560624, -0.4822834645669293319 ) ) ;
#55769 = CARTESIAN_POINT ( 'NONE',  ( 0.2867679344610365999, 0.2867679344610365999, -2.492125984251968518 ) ) ;
#55770 = CARTESIAN_POINT ( 'NONE',  ( 1.489501312335958172, -0.3162353388693405765, 0.4822834645669290543 ) ) ;
#55771 = ORIENTED_EDGE ( 'NONE', *, *, #61540, .T. ) ;
#55772 = CARTESIAN_POINT ( 'NONE',  ( -0.1058382717557497937, -0.3949938075777411628, -2.906824146981628054 ) ) ;
#55773 = ORIENTED_EDGE ( 'NONE', *, *, #23955, .F. ) ;
#55774 = FACE_OUTER_BOUND ( 'NONE', #9604, .T. ) ;
#55775 = CARTESIAN_POINT ( 'NONE',  ( 1.279527559055118724, 0.07958543189024085140, 0.2665933059059887866 ) ) ;
#55776 = CARTESIAN_POINT ( 'NONE',  ( 0.3460692066303959757, -0.1998031496062991907, -1.207349081364829324 ) ) ;
#55777 = LINE ( 'NONE', #42738, #41135 ) ;
#55778 = CARTESIAN_POINT ( 'NONE',  ( -0.1312335958005241554, 0.1539470093639523085, 0.1968503937007873850 ) ) ;
#55779 = CARTESIAN_POINT ( 'NONE',  ( 0.5314960629921396951, 2.559055118110236560, -3.937007874015760578 ) ) ;
#55780 = CARTESIAN_POINT ( 'NONE',  ( -0.3005583989984065840, 1.777033769787525808, 0.08778744816744185608 ) ) ;
#55781 = CARTESIAN_POINT ( 'NONE',  ( -0.2867679344610364334, -0.2867679344610367109, -0.4586614173228347746 ) ) ;
#55782 = CARTESIAN_POINT ( 'NONE',  ( -0.6627296587926501115, 0.1771653543307087075, -0.09757992244046823083 ) ) ;
#55783 = CARTESIAN_POINT ( 'NONE',  ( -1.377952755905511140, 0.1771653543307087630, 0.000000000000000000 ) ) ;
#55784 = AXIS2_PLACEMENT_3D ( 'NONE', #58269, #8610, #65861 ) ;
#55785 = CARTESIAN_POINT ( 'NONE',  ( -1.646981627296586703, -0.05778040916215522460, 0.4822834645669289988 ) ) ;
#55786 = EDGE_CURVE ( 'NONE', #42092, #24707, #82711, .T. ) ;
#55787 = CARTESIAN_POINT ( 'NONE',  ( 0.6167979002624678353, -0.4281496062992124485, 0.4176697321401328655 ) ) ;
#55788 = CARTESIAN_POINT ( 'NONE',  ( -1.174540682414697335, -0.05778040916215522460, 0.4822834645669289988 ) ) ;
#55789 = CARTESIAN_POINT ( 'NONE',  ( -0.1049643490035302024, -0.3917322834645671215, -0.2217847769028870319 ) ) ;
#55790 = ORIENTED_EDGE ( 'NONE', *, *, #68271, .F. ) ;
#55791 = CARTESIAN_POINT ( 'NONE',  ( 1.410761154855643795, -0.3162353388693405765, 0.4822834645669290543 ) ) ;
#55792 = CARTESIAN_POINT ( 'NONE',  ( 1.455672919077434579E-16, 0.4374015748031496176, 1.178877988035069047 ) ) ;
#55793 = CARTESIAN_POINT ( 'NONE',  ( -0.1265901696524993347, 0.4724409448818895907, -1.581364829396325389 ) ) ;
#55794 = CYLINDRICAL_SURFACE ( 'NONE', #42525, 2.362204724409449508 ) ;
#55795 = CARTESIAN_POINT ( 'NONE',  ( -0.6430446194225712953, 0.05413385826771626580, -0.4176697321401330321 ) ) ;
#55796 = CARTESIAN_POINT ( 'NONE',  ( 1.633858267716535639, -0.5400638737290844871, 0.3530559997133364547 ) ) ;
#55798 = CARTESIAN_POINT ( 'NONE',  ( 0.6561679790026253567, 0.1539470093639523085, 0.1968503937007873850 ) ) ;
#55797 = DIRECTION ( 'NONE',  ( 0.000000000000000000, 0.000000000000000000, -1.000000000000000000 ) ) ;
#55799 = CARTESIAN_POINT ( 'NONE',  ( 1.620734908136483465, -0.6692913385826771977, 0.1292274648535927661 ) ) ;
#55800 = CARTESIAN_POINT ( 'NONE',  ( -0.8858267716535425107, 0.1660481256975883668, -0.3530559997133364547 ) ) ;
#55801 = CIRCLE ( 'NONE', #12798, 3.307086614173228689 ) ;
#55802 = CARTESIAN_POINT ( 'NONE',  ( -9.594673741351310580E-17, 0.3917322834645669549, -0.3949938075777409963 ) ) ;
#55803 = CARTESIAN_POINT ( 'NONE',  ( 0.1377952755905518800, -0.4536011799217367080, 0.2665933059059888421 ) ) ;
#55804 = CARTESIAN_POINT ( 'NONE',  ( 0.3917322834645670104, -0.1049643490035303273, -0.5111548556430446366 ) ) ;
#55805 = CARTESIAN_POINT ( 'NONE',  ( -0.1443569553805765515, -0.3690944881889765550, -0.3153832671262227771 ) ) ;
#55806 = CARTESIAN_POINT ( 'NONE',  ( 0.4593175853018379162, -0.3690944881889763329, 0.3153832671262228327 ) ) ;
#55807 = CARTESIAN_POINT ( 'NONE',  ( 0.6430446194225728496, 0.05413385826771666132, 0.4176697321401328100 ) ) ;
#55808 = CARTESIAN_POINT ( 'NONE',  ( -0.6824146981627288167, 0.1283753931104748280, 0.1820866141732283561 ) ) ;
#55809 = CARTESIAN_POINT ( 'NONE',  ( 0.3917322834645669549, 0.1049643490035304660, -2.164041994750655729 ) ) ;
#55810 = CARTESIAN_POINT ( 'NONE',  ( -1.581364829396324945, -0.05778040916215560624, -0.4822834645669293319 ) ) ;
#55811 = EDGE_CURVE ( 'NONE', #78599, #43641, #54542, .T. ) ;
#55812 = CARTESIAN_POINT ( 'NONE',  ( -1.017060367454067249, -0.05778040916215522460, 0.4822834645669289988 ) ) ;
#55813 = CARTESIAN_POINT ( 'NONE',  ( -0.4724409448818895907, -0.1265901696524993070, -0.9101049868766404316 ) ) ;
#55814 = CARTESIAN_POINT ( 'NONE',  ( 0.2427821522309716595, -0.3162353388693409650, -0.4822834645669289433 ) ) ;
#55815 = CARTESIAN_POINT ( 'NONE',  ( -0.3805774278215216522, 0.05413385826771666132, 0.4176697321401328100 ) ) ;
#55816 = CARTESIAN_POINT ( 'NONE',  ( 1.049868766404200349, 0.1283753931104748280, 0.1820866141732283561 ) ) ;
#55817 = CARTESIAN_POINT ( 'NONE',  ( -0.006561679790025524116, -0.2845877964562159024, 0.3641732283464567677 ) ) ;
#55818 = CARTESIAN_POINT ( 'NONE',  ( -0.05905511811023545637, -0.5400638737290845981, -0.3530559997133363437 ) ) ;
#55819 = CARTESIAN_POINT ( 'NONE',  ( -1.135170603674539924, 0.2952755905511810774, -0.1292274648535930714 ) ) ;
#55820 = CARTESIAN_POINT ( 'NONE',  ( 0.2460629921259842590, 1.566969329617675860E-17, -0.1279527559055117503 ) ) ;
#55821 = CARTESIAN_POINT ( 'NONE',  ( -1.011689015874862818, -4.014535696949182149E-15, 0.3627989612356152249 ) ) ;
#55822 = CARTESIAN_POINT ( 'NONE',  ( 0.05249343832021075018, -0.6046776061558807314, 0.2411417322834647770 ) ) ;
#55823 = ORIENTED_EDGE ( 'NONE', *, *, #35062, .F. ) ;
#55824 = CARTESIAN_POINT ( 'NONE',  ( 0.1070741851644053388, 0.3996062992125986035, -1.802493438320209584 ) ) ;
#55825 = EDGE_CURVE ( 'NONE', #18415, #21240, #22574, .T. ) ;
#55826 = CARTESIAN_POINT ( 'NONE',  ( 1.279527559055118724, 0.1660481256975885056, 0.3530559997133364547 ) ) ;
#55827 = CARTESIAN_POINT ( 'NONE',  ( -0.7283464566929126471, 0.07958543189024071263, -0.2665933059059888421 ) ) ;
#55828 = CARTESIAN_POINT ( 'NONE',  ( -0.3674540682414692561, -0.6046776061558809534, -0.2411417322834644161 ) ) ;
#55829 = CARTESIAN_POINT ( 'NONE',  ( 1.450131233595801428, -0.6692913385826773087, -0.1292274648535924053 ) ) ;
#55830 = CARTESIAN_POINT ( 'NONE',  ( 0.7283464566929143125, 0.1660481256975885056, 0.3530559997133364547 ) ) ;
#55831 = CARTESIAN_POINT ( 'NONE',  ( 1.141392835773559211, 0.3937007874015748254, 1.141392835773562764 ) ) ;
#55832 = CARTESIAN_POINT ( 'NONE',  ( -1.115485564304461219, -0.3690944881889763329, 0.3153832671262228327 ) ) ;
#55833 = CARTESIAN_POINT ( 'NONE',  ( 0.1070741851644053527, 0.3996062992125985480, -0.3851706036745407014 ) ) ;
#55834 = CARTESIAN_POINT ( 'NONE',  ( -0.3996062992125986035, -0.1070741851644056997, -0.3608923884514435576 ) ) ;
#55835 = CARTESIAN_POINT ( 'NONE',  ( 0.3420746716998659953, 0.1974969037888705536, 0.02624671916010492753 ) ) ;
#55836 = CARTESIAN_POINT ( 'NONE',  ( 1.660104986876641320, -0.08942795157527998196, 0.3641732283464567121 ) ) ;
#55837 = CARTESIAN_POINT ( 'NONE',  ( 0.8727034120734912248, -0.2845877964562161244, -0.3641732283464567121 ) ) ;
#55838 = CARTESIAN_POINT ( 'NONE',  ( 0.5839895013123367340, -0.6692913385826773087, -0.1292274648535924053 ) ) ;
#55839 = CARTESIAN_POINT ( 'NONE',  ( 0.4091458600556404646, -0.2362204724409448231, -2.386482939632545985 ) ) ;
#55840 = CARTESIAN_POINT ( 'NONE',  ( -0.1058382717557503072, 0.3949938075777408852, -0.7132545931758530466 ) ) ;
#55841 = CARTESIAN_POINT ( 'NONE',  ( 0.7545931758530189937, 0.1771653543307087075, -0.09757992244046823083 ) ) ;
#55842 = CARTESIAN_POINT ( 'NONE',  ( -0.1246719160104980823, -0.6692913385826773087, -0.1292274648535924053 ) ) ;
#55843 = CARTESIAN_POINT ( 'NONE',  ( -0.9383202099737524282, -0.3162353388693409650, -0.4822834645669289433 ) ) ;
#55844 = CARTESIAN_POINT ( 'NONE',  ( 1.325459317585302665, -0.4281496062992124485, 0.4176697321401328655 ) ) ;
#55845 = CARTESIAN_POINT ( 'NONE',  ( 5.785732909357575061E-17, -0.4724409448818898682, -1.338582677165354173 ) ) ;
#55846 = CARTESIAN_POINT ( 'NONE',  ( 0.3460692066303959202, 0.1998031496062993295, -2.493438320209973469 ) ) ;
#55847 = VECTOR ( 'NONE', #8909, 39.37007874015748143 ) ;
#55848 = CARTESIAN_POINT ( 'NONE',  ( -0.1574803149606292529, -0.1870078740157479769, 0.3641732283464567677 ) ) ;
#55849 = ORIENTED_EDGE ( 'NONE', *, *, #48124, .F. ) ;
#55850 = CARTESIAN_POINT ( 'NONE',  ( -0.3392501089628019995, 0.1958661417322831999, -0.6529064548894508713 ) ) ;
#55851 = VERTEX_POINT ( 'NONE', #73090 ) ;
#55852 = CARTESIAN_POINT ( 'NONE',  ( -0.7939632545931754048, -0.3162353388693405765, 0.4822834645669290543 ) ) ;
#55853 = CARTESIAN_POINT ( 'NONE',  ( -0.05905511811023545637, 0.1660481256975885056, 0.3530559997133364547 ) ) ;
#55854 = CARTESIAN_POINT ( 'NONE',  ( -0.4527559055118102749, -0.5400638737290845981, -0.3530559997133363437 ) ) ;
#55855 = CARTESIAN_POINT ( 'NONE',  ( 0.4658792650918641698, -0.05778040916215560624, -0.4822834645669293319 ) ) ;
#55856 = CARTESIAN_POINT ( 'NONE',  ( -0.3018372703412066094, -0.4281496062992127816, -0.4176697321401328100 ) ) ;
#55857 = CARTESIAN_POINT ( 'NONE',  ( -1.233595800524933894, -0.6046776061558809534, -0.2411417322834644161 ) ) ;
#55858 = CARTESIAN_POINT ( 'NONE',  ( -0.8333333333333323711, -0.6692913385826773087, -0.1292274648535924053 ) ) ;
#55859 = CARTESIAN_POINT ( 'NONE',  ( 0.8202099737532813073, 0.2952755905511811885, 0.1292274648535926551 ) ) ;
#55860 = CARTESIAN_POINT ( 'NONE',  ( 0.5971128608923890191, -0.6692913385826771977, 0.1292274648535927661 ) ) ;
#55861 = CARTESIAN_POINT ( 'NONE',  ( -0.3917322834645670104, -7.196005306013484475E-17, -0.9763779527559053317 ) ) ;
#55862 = CARTESIAN_POINT ( 'NONE',  ( -0.3543307086614165824, 0.1771653543307087630, 0.000000000000000000 ) ) ;
#55863 = ORIENTED_EDGE ( 'NONE', *, *, #70014, .F. ) ;
#55864 = CARTESIAN_POINT ( 'NONE',  ( -0.3420746716998659953, -0.1974969037888706647, -1.469816272965879245 ) ) ;
#55865 = VERTEX_POINT ( 'NONE', #80667 ) ;
#55866 = CARTESIAN_POINT ( 'NONE',  ( -1.338582677165353729, -0.1870078740157480601, -0.3641732283464567677 ) ) ;
#55867 = CARTESIAN_POINT ( 'NONE',  ( -0.2887139107611542133, -0.6046776061558809534, -0.2411417322834644161 ) ) ;
#55868 = DIRECTION ( 'NONE',  ( 0.000000000000000000, 0.000000000000000000, 1.000000000000000000 ) ) ;
#55869 = CARTESIAN_POINT ( 'NONE',  ( -0.6430446194225716283, -0.4281496062992124485, 0.4176697321401328655 ) ) ;
#55870 = CARTESIAN_POINT ( 'NONE',  ( -0.8398950131233589023, -0.6046776061558809534, -0.2411417322834644161 ) ) ;
#55871 = CARTESIAN_POINT ( 'NONE',  ( -2.362204724409448620, 1.929133858267716661, -2.474278114140802984E-14 ) ) ;
#55872 = EDGE_CURVE ( 'NONE', #24385, #50887, #2394, .T. ) ;
#55873 = CARTESIAN_POINT ( 'NONE',  ( -1.653543307086613234, -0.1870078740157480879, -0.4822834645669291653 ) ) ;
#55874 = CARTESIAN_POINT ( 'NONE',  ( 1.135170603674541256, -0.5511811023622048555, -0.09757992244046775898 ) ) ;
#55875 = CARTESIAN_POINT ( 'NONE',  ( -0.4827800718432839200, -5.134928753749862370E-15, -0.4281989832122469752 ) ) ;
#55876 = CARTESIAN_POINT ( 'NONE',  ( -0.3392501089628017219, -0.1958661417322836718, -0.1371391076115486551 ) ) ;
#55877 = CARTESIAN_POINT ( 'NONE',  ( -0.1049868766404193215, 0.1283753931104746893, -0.1820866141732285504 ) ) ;
#55878 = CARTESIAN_POINT ( 'NONE',  ( -0.2362204724409440182, -0.1870078740157479769, 0.4822834645669291653 ) ) ;
#55879 = ADVANCED_FACE ( 'NONE', ( #48234 ), #19459, .F. ) ;
#55880 = CARTESIAN_POINT ( 'NONE',  ( 3.909792448225465566, 1.429026188080324333, 0.4621293626231841034 ) ) ;
#55881 = CARTESIAN_POINT ( 'NONE',  ( 0.03937007874015833325, -0.6692913385826771977, 8.415575281601705876E-17 ) ) ;
#55882 = VERTEX_POINT ( 'NONE', #47399 ) ;
#55883 = CARTESIAN_POINT ( 'NONE',  ( -0.1998031496062991907, -0.3460692066303959757, -2.112860892388451539 ) ) ;
#55884 = CARTESIAN_POINT ( 'NONE',  ( -0.7998211177050861265, -2.609869883881465018E-15, -0.3464511005275220379 ) ) ;
#55885 = ORIENTED_EDGE ( 'NONE', *, *, #9262, .F. ) ;
#55886 = CARTESIAN_POINT ( 'NONE',  ( -0.3996062992125986590, 0.1070741851644051723, -1.526902887139107490 ) ) ;
#55887 = CARTESIAN_POINT ( 'NONE',  ( 0.000000000000000000, 2.755905511811024056, 0.000000000000000000 ) ) ;
#55888 = CARTESIAN_POINT ( 'NONE',  ( -0.6627296587926503335, -0.5511811023622046335, 0.09757992244046803654 ) ) ;
#55889 = CARTESIAN_POINT ( 'NONE',  ( -0.9120734908136475250, 0.2952755905511811885, 0.1292274648535926551 ) ) ;
#55890 = CARTESIAN_POINT ( 'NONE',  ( 0.1265901696524989462, 0.4724409448818897572, -0.4658792650918635592 ) ) ;
#55891 = LINE ( 'NONE', #63050, #81535 ) ;
#55892 = CARTESIAN_POINT ( 'NONE',  ( -9.594673741351313045E-17, 0.3917322834645670104, 0.1653543307086614844 ) ) ;
#55893 = CARTESIAN_POINT ( 'NONE',  ( 1.181102362204725198, -0.1870078740157479769, 0.4822834645669291653 ) ) ;
#55894 = CARTESIAN_POINT ( 'NONE',  ( 0.4002624671916016896, -0.3162353388693409650, -0.4822834645669289433 ) ) ;
#55895 = CARTESIAN_POINT ( 'NONE',  ( 0.4658792650918641698, -0.05778040916215560624, -0.4822834645669293319 ) ) ;
#55896 = CARTESIAN_POINT ( 'NONE',  ( -0.4658792650918627265, -0.2845877964562161244, -0.3641732283464567121 ) ) ;
#55897 = VECTOR ( 'NONE', #71467, 39.37007874015748143 ) ;
#55898 = CIRCLE ( 'NONE', #18305, 1.122047244094488194 ) ;
#55899 = CARTESIAN_POINT ( 'NONE',  ( -0.2624671916010490880, 0.2306618581243847221, -0.2411417322834647770 ) ) ;
#55900 = CARTESIAN_POINT ( 'NONE',  ( 0.3458507752293908943, -0.3458507752293908943, -2.222440944881889813 ) ) ;
#55901 = CARTESIAN_POINT ( 'NONE',  ( -1.043307086614172707, 0.1660481256975883668, -0.3530559997133364547 ) ) ;
#55902 = CARTESIAN_POINT ( 'NONE',  ( 4.837279021331061486E-17, -0.3949938075777409963, -2.202755905511811108 ) ) ;
#55903 = CARTESIAN_POINT ( 'NONE',  ( 1.463254593175853824, 0.1771653543307087075, -0.09757992244046823083 ) ) ;
#55904 = CARTESIAN_POINT ( 'NONE',  ( -0.3608923884514428360, -0.5511811023622048555, -0.09757992244046775898 ) ) ;
#55905 = CARTESIAN_POINT ( 'NONE',  ( 1.200787401574803681, 0.07958543189024085140, 0.2665933059059887866 ) ) ;
#55906 = CARTESIAN_POINT ( 'NONE',  ( 1.594488188976378673, 0.07958543189024085140, 0.2665933059059887866 ) ) ;
#55907 = CARTESIAN_POINT ( 'NONE',  ( -1.174540682414697335, -0.08942795157527998196, 0.3641732283464567121 ) ) ;
#55908 = CARTESIAN_POINT ( 'NONE',  ( 0.000000000000000000, 0.7086614173228346081, -0.3129921259842521897 ) ) ;
#55909 = CARTESIAN_POINT ( 'NONE',  ( 0.6955380577427828781, -0.3690944881889763329, 0.3153832671262228327 ) ) ;
#55910 = CARTESIAN_POINT ( 'NONE',  ( -0.4330708661417315697, -0.6692913385826771977, 8.415575281601705876E-17 ) ) ;
#55911 = VECTOR ( 'NONE', #32595, 39.37007874015748143 ) ;
#55912 = CARTESIAN_POINT ( 'NONE',  ( 1.092353285368624860, -4.408777212815537393E-16, -0.4445507791589063395 ) ) ;
#55913 = CARTESIAN_POINT ( 'NONE',  ( -0.2624671916010490880, -0.5023911411419708095, 0.1820866141732285504 ) ) ;
#55914 = FACE_OUTER_BOUND ( 'NONE', #64752, .T. ) ;
#55915 = CARTESIAN_POINT ( 'NONE',  ( 0.6824146981627303710, -0.6046776061558807314, 0.2411417322834647770 ) ) ;
#55916 = CARTESIAN_POINT ( 'NONE',  ( 0.6758530183727039509, 0.2952755905511810219, -0.1292274648535930437 ) ) ;
#55917 = CARTESIAN_POINT ( 'NONE',  ( 1.187664041994751285, -0.2845877964562161244, -0.3641732283464567121 ) ) ;
#55918 = CARTESIAN_POINT ( 'NONE',  ( -0.9251968503937002541, 0.1660481256975885056, 0.3530559997133364547 ) ) ;
#55919 = CARTESIAN_POINT ( 'NONE',  ( -0.1574803149606292529, -0.1870078740157480601, -0.3641732283464567677 ) ) ;
#55920 = CARTESIAN_POINT ( 'NONE',  ( 1.033961166703849965, -2.398893483443748302E-16, 0.4281993546915529580 ) ) ;
#55921 = CARTESIAN_POINT ( 'NONE',  ( 0.4330708661417329575, -0.5511811023622047445, 6.969142054262312111E-17 ) ) ;
#55922 = CARTESIAN_POINT ( 'NONE',  ( -0.7020997375328074108, -0.05778040916215522460, 0.4822834645669289988 ) ) ;
#55923 = CARTESIAN_POINT ( 'NONE',  ( -0.3460692066303960313, 0.1998031496062989965, -0.7329396325459317518 ) ) ;
#55924 = CARTESIAN_POINT ( 'NONE',  ( 4.797336870675656522E-17, -0.3917322834645670104, -2.210629921259842590 ) ) ;
#55925 = CARTESIAN_POINT ( 'NONE',  ( 0.4855643044619428750, -0.004921259842519576551, 0.3153832671262227771 ) ) ;
#55926 = CARTESIAN_POINT ( 'NONE',  ( -0.2624671916010490880, -0.6046776061558807314, 0.2411417322834647770 ) ) ;
#55927 = CARTESIAN_POINT ( 'NONE',  ( -0.8398950131233585692, 0.2306618581243848609, 0.2411417322834645549 ) ) ;
#55928 = CARTESIAN_POINT ( 'NONE',  ( -0.9186351706036736120, -0.5023911411419708095, -0.1820866141732282451 ) ) ;
#55929 = DIRECTION ( 'NONE',  ( -3.096699300667737957E-16, 1.000000000000000000, -0.000000000000000000 ) ) ;
#55930 = CARTESIAN_POINT ( 'NONE',  ( -0.9251968503937002541, -0.4536011799217368745, -0.2665933059059886201 ) ) ;
#55931 = CARTESIAN_POINT ( 'NONE',  ( -0.1181102362204717315, -0.6692913385826771977, 8.415575281601705876E-17 ) ) ;
#55932 = CARTESIAN_POINT ( 'NONE',  ( -1.141732283464566011, -0.5511811023622047445, 6.969142054262312111E-17 ) ) ;
#55933 = CARTESIAN_POINT ( 'NONE',  ( -1.515748031496062076, -0.5400638737290844871, 0.3530559997133364547 ) ) ;
#55934 = CARTESIAN_POINT ( 'NONE',  ( 0.01241954290193841674, 0.000000000000000000, 0.3464511005275205946 ) ) ;
#55935 = ORIENTED_EDGE ( 'NONE', *, *, #27502, .T. ) ;
#55936 = CARTESIAN_POINT ( 'NONE',  ( -1.555118110236219930, 0.07958543189024085140, 0.2665933059059887866 ) ) ;
#55937 = CARTESIAN_POINT ( 'NONE',  ( -0.7545931758530177724, 0.2952755905511811885, 0.1292274648535926551 ) ) ;
#55938 = CARTESIAN_POINT ( 'NONE',  ( -0.5577427821522301654, -0.05778040916215560624, -0.4822834645669293319 ) ) ;
#55939 = CARTESIAN_POINT ( 'NONE',  ( -1.095800524934382292, -0.3162353388693409650, -0.4822834645669289433 ) ) ;
#55940 = CARTESIAN_POINT ( 'NONE',  ( -0.1958661417322836718, 0.3392501089628017219, -1.515091863517060489 ) ) ;
#55941 = CARTESIAN_POINT ( 'NONE',  ( 0.000000000000000000, 2.165354330708661568, 0.000000000000000000 ) ) ;
#55942 = CARTESIAN_POINT ( 'NONE',  ( 0.8005249343832028242, -0.4281496062992127816, -0.4176697321401328100 ) ) ;
#55943 = CARTESIAN_POINT ( 'NONE',  ( 0.5314960629921267055, -0.5400638737290844871, 0.3530559997133364547 ) ) ;
#55944 = CARTESIAN_POINT ( 'NONE',  ( -3.937007874015748143, 2.165354330708661568, -0.3149606299212600047 ) ) ;
#55945 = CIRCLE ( 'NONE', #19668, 0.5120078740157480990 ) ;
#55946 = CONICAL_SURFACE ( 'NONE', #43864, 1.181102362204724310, 0.7853981633974621568 ) ;
#55948 = AXIS2_PLACEMENT_3D ( 'NONE', #13269, #72171, #78914 ) ;
#55947 = CARTESIAN_POINT ( 'NONE',  ( 0.3996062992125984925, 0.1070741851644054499, -2.563648293963254776 ) ) ;
#55949 = CARTESIAN_POINT ( 'NONE',  ( 1.384514435695538337, -0.5511811023622046335, 0.09757992244046803654 ) ) ;
#55950 = CARTESIAN_POINT ( 'NONE',  ( -9.787531504996567848E-17, 0.3996062992125986035, -0.9448818897637796255 ) ) ;
#55951 = VERTEX_POINT ( 'NONE', #16687 ) ;
#55952 = CARTESIAN_POINT ( 'NONE',  ( -0.9317585301837263412, -0.3690944881889765550, -0.3153832671262227771 ) ) ;
#55953 = CARTESIAN_POINT ( 'NONE',  ( -0.1958661417322836718, 0.3392501089628017219, -2.682414698162729483 ) ) ;
#55954 = ORIENTED_EDGE ( 'NONE', *, *, #73105, .T. ) ;
#55955 = CARTESIAN_POINT ( 'NONE',  ( 0.2296587926509192634, -0.05778040916215560624, -0.4822834645669293319 ) ) ;
#55956 = CARTESIAN_POINT ( 'NONE',  ( -0.3674540682414692561, -0.6046776061558809534, -0.2411417322834644161 ) ) ;
#55957 = CARTESIAN_POINT ( 'NONE',  ( -1.069553805774277722, -0.6692913385826773087, -0.1292274648535924053 ) ) ;
#55958 = CARTESIAN_POINT ( 'NONE',  ( 1.194225721784777594, 0.05413385826771666132, 0.4176697321401328100 ) ) ;
#55959 = CARTESIAN_POINT ( 'NONE',  ( -1.463254593175852492, 0.1771653543307087630, 0.09757992244046791164 ) ) ;
#55960 = CARTESIAN_POINT ( 'NONE',  ( 0.1181102362204724532, -0.04921259842519685318, -0.08523872084492505052 ) ) ;
#55961 = CARTESIAN_POINT ( 'NONE',  ( -0.1049868766404193215, -0.6046776061558807314, 0.2411417322834647770 ) ) ;
#55962 = CARTESIAN_POINT ( 'NONE',  ( -1.345144356955379816, -0.3162353388693405765, 0.4822834645669290543 ) ) ;
#55963 = CARTESIAN_POINT ( 'NONE',  ( 0.2867679344610365999, -0.2867679344610365999, -1.910741839073804016 ) ) ;
#55964 = DIRECTION ( 'NONE',  ( 0.000000000000000000, 0.000000000000000000, 1.000000000000000000 ) ) ;
#55965 = FACE_OUTER_BOUND ( 'NONE', #6520, .T. ) ;
#55966 = CARTESIAN_POINT ( 'NONE',  ( -9.594673741351313045E-17, 0.3917322834645670104, 0.1653543307086614844 ) ) ;
#55967 = CARTESIAN_POINT ( 'NONE',  ( 0.7611548556430454138, 0.1283753931104746893, -0.1820866141732285504 ) ) ;
#55968 = ORIENTED_EDGE ( 'NONE', *, *, #14716, .F. ) ;
#55969 = CARTESIAN_POINT ( 'NONE',  ( 0.3420746716998660508, -0.1974969037888703871, -0.1049868766404199877 ) ) ;
#55970 = CARTESIAN_POINT ( 'NONE',  ( -0.7480314960629914633, -0.6692913385826771977, 8.415575281601705876E-17 ) ) ;
#55971 = ORIENTED_EDGE ( 'NONE', *, *, #62649, .T. ) ;
#55973 = AXIS2_PLACEMENT_3D ( 'NONE', #1776, #66168, #8508 ) ;
#55972 = CARTESIAN_POINT ( 'NONE',  ( -0.06561679790026180015, -0.3690944881889765550, -0.3153832671262227771 ) ) ;
#55974 = DIRECTION ( 'NONE',  ( 0.000000000000000000, -0.4999999999999998335, -0.8660254037844385966 ) ) ;
#55975 = CARTESIAN_POINT ( 'NONE',  ( 0.6955380577427828781, 0.05413385826771626580, -0.4176697321401330321 ) ) ;
#55976 = CARTESIAN_POINT ( 'NONE',  ( 0.3412073490813655186, 0.2306618581243848609, 0.2411417322834645549 ) ) ;
#55977 = EDGE_CURVE ( 'NONE', #18348, #55450, #29298, .T. ) ;
#55978 = CARTESIAN_POINT ( 'NONE',  ( -0.5643044619422565855, 0.05413385826771626580, -0.4176697321401330321 ) ) ;
#55979 = CARTESIAN_POINT ( 'NONE',  ( 0.1958661417322834775, 0.3392501089628018884, -1.243457635991812582 ) ) ;
#55980 = CARTESIAN_POINT ( 'NONE',  ( -0.7020997375328074108, -0.05778040916215522460, 0.4822834645669289988 ) ) ;
#55981 = CARTESIAN_POINT ( 'NONE',  ( -0.1049643490035307020, 0.3917322834645669549, -2.768372703412072866 ) ) ;
#55982 = CARTESIAN_POINT ( 'NONE',  ( 1.148293963254593653, 0.1771653543307087075, -0.09757992244046823083 ) ) ;
#55983 = CARTESIAN_POINT ( 'NONE',  ( -0.9711286089238838626, 0.2306618581243847221, -0.2411417322834647770 ) ) ;
#55984 = CARTESIAN_POINT ( 'NONE',  ( 0.8858267716535438430, 0.1660481256975885056, 0.3530559997133364547 ) ) ;
#55985 = CARTESIAN_POINT ( 'NONE',  ( 1.200787401574803681, 0.1660481256975885056, 0.3530559997133364547 ) ) ;
#55986 = CARTESIAN_POINT ( 'NONE',  ( -0.3996062992125987146, 0.1070741851644051862, -0.9776902887139107268 ) ) ;
#55987 = CARTESIAN_POINT ( 'NONE',  ( -1.502624671916009680, -0.05778040916215560624, -0.4822834645669293319 ) ) ;
#55988 = CARTESIAN_POINT ( 'NONE',  ( 0.3460692066303959202, -0.1998031496062991630, -0.3392388451443569819 ) ) ;
#55989 = CARTESIAN_POINT ( 'NONE',  ( 0.1902887139107617975, 0.2952755905511811885, 0.1292274648535926551 ) ) ;
#55990 = CARTESIAN_POINT ( 'NONE',  ( -0.1998031496062994683, 0.3460692066303958092, -2.375328083989501238 ) ) ;
#55991 = CARTESIAN_POINT ( 'NONE',  ( -1.614173228346455824, 0.1771653543307087630, 0.000000000000000000 ) ) ;
#55992 = CARTESIAN_POINT ( 'NONE',  ( 0.4986876640419954376, -0.5023911411419708095, -0.1820866141732282451 ) ) ;
#55993 = CARTESIAN_POINT ( 'NONE',  ( 0.7808398950131240079, -0.3162353388693405765, 0.4822834645669290543 ) ) ;
#55994 = CARTESIAN_POINT ( 'NONE',  ( 0.2362204724409449064, 0.4091458600556404646, -1.008530183727034180 ) ) ;
#55995 = CARTESIAN_POINT ( 'NONE',  ( 0.6233595800524942554, -0.08942795157528024563, -0.3641732283464568787 ) ) ;
#55996 = CARTESIAN_POINT ( 'NONE',  ( 0.5577427821522314977, -0.3162353388693409650, -0.4822834645669289433 ) ) ;
#55997 = B_SPLINE_CURVE_WITH_KNOTS ( 'NONE', 3,
 ( #38078, #31768, #4862, #36437 ),
 .UNSPECIFIED., .F., .F.,
 ( 4, 4 ),
 ( 0.02951359255738795345, 0.02980295909189879799 ),
 .UNSPECIFIED. ) ;
#55998 = CARTESIAN_POINT ( 'NONE',  ( 0.3949938075777409963, 2.418639510665530743E-17, -0.8248031496062994128 ) ) ;
#55999 = CARTESIAN_POINT ( 'NONE',  ( -0.6167979002624665030, 0.05413385826771666132, 0.4176697321401328100 ) ) ;
#56000 = CARTESIAN_POINT ( 'NONE',  ( 0.4724409448818898127, -0.1265901696524988629, -1.133202099737532720 ) ) ;
#56001 = CARTESIAN_POINT ( 'NONE',  ( 0.8136482939632553313, 0.1283753931104748280, 0.1820866141732283561 ) ) ;
#56002 = CARTESIAN_POINT ( 'NONE',  ( 0.08530183727034192087, -0.3162353388693409650, -0.4822834645669289433 ) ) ;
#56003 = PLANE ( 'NONE',  #42622 ) ;
#56004 = CARTESIAN_POINT ( 'NONE',  ( -0.4921259842519677963, -0.5400638737290844871, 0.3530559997133364547 ) ) ;
#56005 = CARTESIAN_POINT ( 'NONE',  ( 0.05249343832021075018, -0.5023911411419708095, 0.1820866141732285504 ) ) ;
#56006 = CARTESIAN_POINT ( 'NONE',  ( -2.822823420596379140, 1.118719813955001863, -0.2236424093447015315 ) ) ;
#56007 = CARTESIAN_POINT ( 'NONE',  ( 0.02624671916010564918, -0.5023911411419708095, -0.1820866141732282451 ) ) ;
#56008 = CARTESIAN_POINT ( 'NONE',  ( 0.6889763779527563470, 0.07958543189024071263, -0.2665933059059888421 ) ) ;
#56009 = DIRECTION ( 'NONE',  ( -1.000000000000000000, -0.000000000000000000, -0.000000000000000000 ) ) ;
#56010 = CARTESIAN_POINT ( 'NONE',  ( 0.3996062992125984925, 0.1070741851644054637, -1.776246719160104570 ) ) ;
#56011 = CARTESIAN_POINT ( 'NONE',  ( 0.3083989501312343062, -0.05778040916215560624, -0.4822834645669293319 ) ) ;
#56012 = AXIS2_PLACEMENT_3D ( 'NONE', #63259, #12341, #124 ) ;
#56013 = CARTESIAN_POINT ( 'NONE',  ( -0.1958661417322834220, -0.3392501089628018884, -1.475065616797900381 ) ) ;
#56014 = CIRCLE ( 'NONE', #17125, 0.5118110236220472231 ) ;
#56015 = VECTOR ( 'NONE', #81595, 39.37007874015748143 ) ;
#56016 = CARTESIAN_POINT ( 'NONE',  ( 1.181102362204725198, -0.1870078740157479769, 0.3641732283464567677 ) ) ;
#56017 = CARTESIAN_POINT ( 'NONE',  ( -0.1674892343164145203, -2.567464376874931580E-15, -0.4445507791589072832 ) ) ;
#56018 = CARTESIAN_POINT ( 'NONE',  ( -0.5249343832020990641, -0.5023911411419708095, -0.1820866141732282451 ) ) ;
#56019 = CARTESIAN_POINT ( 'NONE',  ( -0.2755905511811018171, 0.1771653543307087630, 0.000000000000000000 ) ) ;
#56020 = CARTESIAN_POINT ( 'NONE',  ( -0.3149606299212590610, -0.1870078740157480879, -0.4822834645669291653 ) ) ;
#56021 = CARTESIAN_POINT ( 'NONE',  ( 0.8070866141732289112, -0.4536011799217368745, -0.2665933059059886201 ) ) ;
#56022 = CARTESIAN_POINT ( 'NONE',  ( 0.4257251611738756547, 1.325776663396805555, -1.038227845120437642 ) ) ;
#56023 = CARTESIAN_POINT ( 'NONE',  ( 1.286089238845145033, 0.1283753931104748280, 0.1820866141732283561 ) ) ;
#56024 = CARTESIAN_POINT ( 'NONE',  ( -0.02624671916010428221, 0.2306618581243847221, -0.2411417322834647770 ) ) ;
#56025 = CARTESIAN_POINT ( 'NONE',  ( 1.318897637795276356, -0.5400638737290844871, 0.3530559997133364547 ) ) ;
#56026 = CARTESIAN_POINT ( 'NONE',  ( 0.1990279662527742466, -0.1990279662527742466, 0.1112963449492364726 ) ) ;
#56027 = CARTESIAN_POINT ( 'NONE',  ( 0.3018372703412079971, -0.4281496062992124485, 0.4176697321401328655 ) ) ;
#56028 = CARTESIAN_POINT ( 'NONE',  ( -0.2867679344610365999, 0.2867679344610364889, -1.049212598425196763 ) ) ;
#56029 = CARTESIAN_POINT ( 'NONE',  ( 1.049868766404200349, 0.2306618581243848609, 0.2411417322834645549 ) ) ;
#56030 = CARTESIAN_POINT ( 'NONE',  ( 0.6299212598425204535, -0.1870078740157480879, -0.4822834645669291653 ) ) ;
#56031 = CARTESIAN_POINT ( 'NONE',  ( -0.7137454485294952855, 2.362204724409448620, 0.4917280318828573527 ) ) ;
#56032 = CARTESIAN_POINT ( 'NONE',  ( 0.7545931758530189937, 0.1771653543307087075, -0.09757992244046823083 ) ) ;
#56033 = CARTESIAN_POINT ( 'NONE',  ( 1.062992125984252745, 0.2952755905511811885, 0.000000000000000000 ) ) ;
#56034 = CARTESIAN_POINT ( 'NONE',  ( 0.2690288713910767848, -0.5511811023622048555, -0.09757992244046775898 ) ) ;
#56035 = CARTESIAN_POINT ( 'NONE',  ( -0.1968503937007867743, 0.2952755905511811885, 0.000000000000000000 ) ) ;
#56036 = CARTESIAN_POINT ( 'NONE',  ( 0.4461942257217855201, -0.6046776061558807314, 0.2411417322834647770 ) ) ;
#56037 = CARTESIAN_POINT ( 'NONE',  ( -0.6036745406824141069, -0.6046776061558809534, -0.2411417322834644161 ) ) ;
#56038 = CARTESIAN_POINT ( 'NONE',  ( -0.4265091863517051496, 0.1771653543307087075, -0.09757992244046823083 ) ) ;
#56039 = CARTESIAN_POINT ( 'NONE',  ( 0.7217847769028878924, -0.4281496062992127816, -0.4176697321401328100 ) ) ;
#56040 = CARTESIAN_POINT ( 'NONE',  ( 0.9645669291338591078, -0.4536011799217368745, -0.2665933059059886201 ) ) ;
#56041 = CARTESIAN_POINT ( 'NONE',  ( 0.2362204724409456558, -0.1870078740157479769, 0.4822834645669291653 ) ) ;
#56042 = CARTESIAN_POINT ( 'NONE',  ( -0.4724409448818891466, -0.1265901696525000564, -0.5183727034120735322 ) ) ;
#56044 = DIRECTION ( 'NONE',  ( 0.000000000000000000, 0.000000000000000000, -1.000000000000000000 ) ) ;
#56043 = CARTESIAN_POINT ( 'NONE',  ( 0.1938976377952755792, -0.1938976377952756069, -0.3740157480314971750 ) ) ;
#56045 = DIRECTION ( 'NONE',  ( 0.000000000000000000, 0.000000000000000000, -1.000000000000000000 ) ) ;
#56046 = CARTESIAN_POINT ( 'NONE',  ( 0.1958661417322836440, -0.3392501089628017219, -1.973753280839895208 ) ) ;
#56047 = CARTESIAN_POINT ( 'NONE',  ( -1.122047244094487306, 0.1660481256975883668, -0.3530559997133364547 ) ) ;
#56048 = CARTESIAN_POINT ( 'NONE',  ( -0.9580052493438311334, -0.4281496062992124485, 0.4176697321401328655 ) ) ;
#56049 = CARTESIAN_POINT ( 'NONE',  ( -0.4724409448818899238, 0.1265901696524986686, -0.1902887139107611314 ) ) ;
#56050 = CARTESIAN_POINT ( 'NONE',  ( 0.3420746716998660508, -0.1974969037888703871, -2.939632545931758489 ) ) ;
#56051 = ORIENTED_EDGE ( 'NONE', *, *, #51081, .T. ) ;
#56052 = CARTESIAN_POINT ( 'NONE',  ( 0.4461942257217856311, 0.1283753931104746893, -0.1820866141732285504 ) ) ;
#56053 = CARTESIAN_POINT ( 'NONE',  ( -0.3917322834645671215, 0.1049643490035301469, -1.284776902887139194 ) ) ;
#56054 = CARTESIAN_POINT ( 'NONE',  ( 0.8136482939632553313, 0.2306618581243848609, 0.2411417322834645549 ) ) ;
#56055 = CARTESIAN_POINT ( 'NONE',  ( -0.3458507752293909498, 0.3458507752293907833, -2.539370078740157410 ) ) ;
#56056 = CARTESIAN_POINT ( 'NONE',  ( 1.603475055217291612, 0.7166759647713492054, -0.04573490813648244807 ) ) ;
#56057 = CARTESIAN_POINT ( 'NONE',  ( 1.095800524934383846, -0.05778040916215560624, -0.4822834645669293319 ) ) ;
#56058 = CARTESIAN_POINT ( 'NONE',  ( 1.213910761154856299, -0.5511811023622048555, -0.09757992244046775898 ) ) ;
#56059 = CARTESIAN_POINT ( 'NONE',  ( 0.04593175853018440641, -0.6692913385826771977, 0.1292274648535927661 ) ) ;
#56060 = AXIS2_PLACEMENT_3D ( 'NONE', #18598, #23663, #75035 ) ;
#56061 = CARTESIAN_POINT ( 'NONE',  ( 0.3392501089628018329, 0.1958661417322835052, -0.6837077183388958757 ) ) ;
#56062 = CARTESIAN_POINT ( 'NONE',  ( -0.4461942257217840213, -0.6046776061558809534, -0.2411417322834644161 ) ) ;
#56063 = CARTESIAN_POINT ( 'NONE',  ( -0.9776902887139098386, -0.5511811023622046335, 0.09757992244046803654 ) ) ;
#56065 = EDGE_CURVE ( 'NONE', #37713, #56774, #71397, .T. ) ;
#56064 = CARTESIAN_POINT ( 'NONE',  ( 0.6102362204724416372, -0.5400638737290844871, 0.3530559997133364547 ) ) ;
#56066 = CARTESIAN_POINT ( 'NONE',  ( -0.2887139107611542133, 0.2306618581243848609, 0.2411417322834645549 ) ) ;
#56067 = LINE ( 'NONE', #50164, #55561 ) ;
#56068 = AXIS2_PLACEMENT_3D ( 'NONE', #78298, #16401, #46702 ) ;
#56069 = CARTESIAN_POINT ( 'NONE',  ( 0.4556364815871513096, 1.768811104126938094, -0.5309055118110237448 ) ) ;
#56070 = ORIENTED_EDGE ( 'NONE', *, *, #4271, .T. ) ;
#56071 = CARTESIAN_POINT ( 'NONE',  ( -0.3917322834645670659, -7.196005306013484475E-17, -2.240832964075802458 ) ) ;
#56072 = CARTESIAN_POINT ( 'NONE',  ( 0.4265091863517067594, 0.2952755905511811885, 0.1292274648535926551 ) ) ;
#56073 = VECTOR ( 'NONE', #60637, 39.37007874015748143 ) ;
#56074 = CARTESIAN_POINT ( 'NONE',  ( -0.2362204724409442680, -0.1870078740157480879, -0.4822834645669291653 ) ) ;
#56075 = CARTESIAN_POINT ( 'NONE',  ( -1.594488188976377119, 0.1660481256975883668, -0.3530559997133364547 ) ) ;
#56076 = CARTESIAN_POINT ( 'NONE',  ( 0.7742782152230978099, -0.4281496062992124485, 0.4176697321401328655 ) ) ;
#56077 = ADVANCED_FACE ( 'NONE', ( #40679, #66364 ), #8702, .T. ) ;
#56078 = CARTESIAN_POINT ( 'NONE',  ( 0.4068241469816281097, 0.05413385826771666132, 0.4176697321401328100 ) ) ;
#56079 = CARTESIAN_POINT ( 'NONE',  ( -0.1958661417322836718, 0.3392501089628017219, -1.515091863517060489 ) ) ;
#56080 = CARTESIAN_POINT ( 'NONE',  ( -0.6955380577427815458, -0.4281496062992127816, -0.4176697321401328100 ) ) ;
#56081 = CARTESIAN_POINT ( 'NONE',  ( 0.1902887139107617975, -0.6692913385826773087, -0.1292274648535924053 ) ) ;
#56082 = CARTESIAN_POINT ( 'NONE',  ( -0.2624671916010490880, -0.6046776061558807314, 0.2411417322834647770 ) ) ;
#56083 = CARTESIAN_POINT ( 'NONE',  ( 0.1115485564304470323, 0.1771653543307087630, 0.09757992244046791164 ) ) ;
#56084 = CARTESIAN_POINT ( 'NONE',  ( -1.555118110236219930, 0.1660481256975885056, 0.3530559997133364547 ) ) ;
#56085 = CARTESIAN_POINT ( 'NONE',  ( -0.2362214119660041856, -0.1771641016305865735, 5.695982005544458993 ) ) ;
#56086 = CARTESIAN_POINT ( 'NONE',  ( -0.2624671916010490880, 0.2306618581243847221, -0.2411417322834647770 ) ) ;
#56087 = CARTESIAN_POINT ( 'NONE',  ( 1.150409065943327258, 0.2755905511811023723, 0.8265612839971842041 ) ) ;
#56088 = CARTESIAN_POINT ( 'NONE',  ( -1.541994750656167090, -0.6692913385826773087, -0.1292274648535924053 ) ) ;
#56089 = CARTESIAN_POINT ( 'NONE',  ( 0.3392501089628018884, -0.1958661417322834220, -2.616797900262466836 ) ) ;
#56090 = ORIENTED_EDGE ( 'NONE', *, *, #18680, .F. ) ;
#56091 = VERTEX_POINT ( 'NONE', #67199 ) ;
#56092 = CARTESIAN_POINT ( 'NONE',  ( 0.6758530183727039509, -0.6692913385826771977, 0.1292274648535927661 ) ) ;
#56093 = CARTESIAN_POINT ( 'NONE',  ( -0.006561679790025524116, -0.2845877964562159024, 0.3641732283464567677 ) ) ;
#56095 = CARTESIAN_POINT ( 'NONE',  ( 3.937007874015748143, 1.724409448818898127, 0.6299212598425202314 ) ) ;
#56094 = DIRECTION ( 'NONE',  ( 0.000000000000000000, 0.000000000000000000, -1.000000000000000000 ) ) ;
#56096 = CARTESIAN_POINT ( 'NONE',  ( 4.797336870675656522E-17, -0.3917322834645670104, -0.7933070866141732624 ) ) ;
#56097 = CARTESIAN_POINT ( 'NONE',  ( -0.1265901696524986964, -0.4724409448818899238, 0.1660104986876640432 ) ) ;
#56098 = CARTESIAN_POINT ( 'NONE',  ( 0.7197590744588134859, 1.521610601467410833E-15, 0.3954985857520055270 ) ) ;
#56099 = CARTESIAN_POINT ( 'NONE',  ( 0.3996062992125984925, 0.1070741851644054637, -2.563648293963254776 ) ) ;
#56100 = CARTESIAN_POINT ( 'NONE',  ( 0.4002624671916016896, -0.3162353388693409650, -0.4822834645669289433 ) ) ;
#56101 = CARTESIAN_POINT ( 'NONE',  ( -1.371391076115484609, -0.6692913385826771977, 0.1292274648535927661 ) ) ;
#56102 = CARTESIAN_POINT ( 'NONE',  ( -1.358267716535432434, 0.1660481256975883668, -0.3530559997133364547 ) ) ;
#56103 = CARTESIAN_POINT ( 'NONE',  ( 0.7874015748031503170, -0.1870078740157479769, 0.4822834645669291653 ) ) ;
#56104 = CARTESIAN_POINT ( 'NONE',  ( 1.450131233595801428, 0.2952755905511811885, 0.1292274648535926551 ) ) ;
#56105 = CARTESIAN_POINT ( 'NONE',  ( 1.332020997375329197, -0.2845877964562159024, 0.3641732283464567677 ) ) ;
#56106 = CARTESIAN_POINT ( 'NONE',  ( 1.338582677165355062, -0.1870078740157479769, 0.3641732283464567677 ) ) ;
#56107 = CARTESIAN_POINT ( 'NONE',  ( -0.9383202099737524282, -0.3162353388693409650, -0.4822834645669289433 ) ) ;
#56108 = CARTESIAN_POINT ( 'NONE',  ( -0.2925321140481930149, -0.2925321140481933480, -0.6082677165354329896 ) ) ;
#56109 = CARTESIAN_POINT ( 'NONE',  ( -1.614173228346455824, 0.1771653543307087630, 0.000000000000000000 ) ) ;
#56110 = CARTESIAN_POINT ( 'NONE',  ( -0.2867679344610364334, -0.2867679344610367109, -0.05118110236220468900 ) ) ;
#56111 = CARTESIAN_POINT ( 'NONE',  ( -0.1181102362204717315, -0.6692913385826771977, 8.415575281601705876E-17 ) ) ;
#56113 = DIRECTION ( 'NONE',  ( -0.000000000000000000, -1.000000000000000000, -0.000000000000000000 ) ) ;
#56112 = CARTESIAN_POINT ( 'NONE',  ( 1.305774278215223960, -0.6692913385826771977, 0.1292274648535927661 ) ) ;
#56114 = CARTESIAN_POINT ( 'NONE',  ( -1.154855643044618851, -0.5023911411419708095, -0.1820866141732282451 ) ) ;
#56115 = CARTESIAN_POINT ( 'NONE',  ( 0.5052493438320218022, -0.6692913385826773087, -0.1292274648535924053 ) ) ;
#56116 = CARTESIAN_POINT ( 'NONE',  ( 0.8136482939632553313, 0.1283753931104748280, 0.1820866141732283561 ) ) ;
#56117 = CARTESIAN_POINT ( 'NONE',  ( -0.3392501089628018329, -0.1958661417322836440, -1.549849450622360791 ) ) ;
#56118 = CARTESIAN_POINT ( 'NONE',  ( -1.187664041994750175, -0.08942795157528024563, -0.3641732283464568787 ) ) ;
#56119 = CARTESIAN_POINT ( 'NONE',  ( 0.8464566929133866546, -0.5400638737290844871, 0.3530559997133364547 ) ) ;
#56120 = CARTESIAN_POINT ( 'NONE',  ( -3.937007874015748143, 1.537401574803149984, -2.901595197523589142E-16 ) ) ;
#56121 = CARTESIAN_POINT ( 'NONE',  ( -0.3215223097112853146, -0.2845877964562159024, 0.3641732283464567677 ) ) ;
#56122 = CARTESIAN_POINT ( 'NONE',  ( -0.6299212598425188991, -0.1870078740157479769, 0.4822834645669291653 ) ) ;
#56123 = CARTESIAN_POINT ( 'NONE',  ( -1.515748031496062076, -0.4536011799217367080, 0.2665933059059888421 ) ) ;
#56124 = CARTESIAN_POINT ( 'NONE',  ( -0.9251968503937002541, 0.1660481256975885056, 0.3530559997133364547 ) ) ;
#56125 = CARTESIAN_POINT ( 'NONE',  ( 1.502624671916010790, -0.05778040916215522460, 0.4822834645669289988 ) ) ;
#56126 = CARTESIAN_POINT ( 'NONE',  ( 0.1958661417322834775, 0.3392501089628018884, -0.9284970060705530770 ) ) ;
#56127 = CARTESIAN_POINT ( 'NONE',  ( -0.7545931758530176614, -0.5511811023622048555, -0.09757992244046775898 ) ) ;
#56128 = CARTESIAN_POINT ( 'NONE',  ( 1.122050806839039794, 1.062983699574960195, -0.01543924256646982823 ) ) ;
#56129 = CARTESIAN_POINT ( 'NONE',  ( 1.377952755905512472, -0.6692913385826771977, 8.415575281601705876E-17 ) ) ;
#56130 = TOROIDAL_SURFACE ( 'NONE', #69546, 0.1279527559055117503, 0.009842519685039369942 ) ;
#56131 = CARTESIAN_POINT ( 'NONE',  ( 0.4724409448818898682, 2.892866454678787531E-17, -1.927165354330708569 ) ) ;
#56132 = CARTESIAN_POINT ( 'NONE',  ( -1.286089238845143479, -0.6046776061558807314, 0.2411417322834647770 ) ) ;
#56133 = CARTESIAN_POINT ( 'NONE',  ( -1.358267716535432434, -0.4536011799217367080, 0.2665933059059888421 ) ) ;
#56134 = CARTESIAN_POINT ( 'NONE',  ( -0.4986876640419942164, -0.5023911411419708095, 0.1820866141732285504 ) ) ;
#56135 = LINE ( 'NONE', #10303, #15165 ) ;
#56136 = CARTESIAN_POINT ( 'NONE',  ( -0.3608923884514428360, 0.2952755905511811885, 0.1292274648535926551 ) ) ;
#56137 = CARTESIAN_POINT ( 'NONE',  ( 0.1049868766404206816, 0.1283753931104748280, 0.1820866141732283561 ) ) ;
#56138 = CARTESIAN_POINT ( 'NONE',  ( -1.318897637795274802, -0.4536011799217368745, -0.2665933059059886201 ) ) ;
#56139 = CARTESIAN_POINT ( 'NONE',  ( -1.305774278215222184, -0.6692913385826773087, -0.1292274648535924053 ) ) ;
#56140 = CARTESIAN_POINT ( 'NONE',  ( 1.377952755905512472, -0.5511811023622047445, 6.969142054262312111E-17 ) ) ;
#56141 = CARTESIAN_POINT ( 'NONE',  ( 1.102362204724410155, -0.1870078740157480879, -0.4822834645669291653 ) ) ;
#56142 = CARTESIAN_POINT ( 'NONE',  ( 0.2512006810191718675, 1.134651008203187761, 1.916017364051557426 ) ) ;
#56143 = CARTESIAN_POINT ( 'NONE',  ( 0.3740157480314966754, -0.4536011799217367080, 0.2665933059059888421 ) ) ;
#56144 = EDGE_CURVE ( 'NONE', #74332, #77294, #50386, .T. ) ;
#56145 = DIMENSIONAL_EXPONENTS ( 1.000000000000000000, 0.000000000000000000, 0.000000000000000000, 0.000000000000000000, 0.000000000000000000, 0.000000000000000000, 0.000000000000000000 ) ;
#56146 = CARTESIAN_POINT ( 'NONE',  ( 0.4855643044619430415, -0.4281496062992127816, -0.4176697321401328100 ) ) ;
#56147 = CARTESIAN_POINT ( 'NONE',  ( 0.9383202099737536495, -0.2845877964562159024, 0.3641732283464567677 ) ) ;
#56148 = ORIENTED_EDGE ( 'NONE', *, *, #77992, .F. ) ;
#56149 = CARTESIAN_POINT ( 'NONE',  ( -1.128608923884513837, 0.2306618581243847221, -0.2411417322834647770 ) ) ;
#56150 = CARTESIAN_POINT ( 'NONE',  ( -0.8464566929133852113, 0.1660481256975885056, 0.3530559997133364547 ) ) ;
#56151 = CARTESIAN_POINT ( 'NONE',  ( -0.2624671916010490880, 0.2306618581243847221, -0.2411417322834647770 ) ) ;
#56152 = CARTESIAN_POINT ( 'NONE',  ( 0.000000000000000000, 2.755905511811024056, 0.000000000000000000 ) ) ;
#56153 = CARTESIAN_POINT ( 'NONE',  ( 0.1998031496062994128, -0.3460692066303957537, -2.688320209973753538 ) ) ;
#56154 = CARTESIAN_POINT ( 'NONE',  ( 0.5511811023622054106, -0.1870078740157480879, -0.4822834645669291653 ) ) ;
#56155 = CARTESIAN_POINT ( 'NONE',  ( -1.660104986876639543, -0.05778040916215560624, -0.4822834645669293319 ) ) ;
#56156 = CARTESIAN_POINT ( 'NONE',  ( -0.1115485564304453947, -0.6692913385826771977, 0.1292274648535927661 ) ) ;
#56157 = CARTESIAN_POINT ( 'NONE',  ( 0.5774278215223103139, -0.6046776061558809534, -0.2411417322834644161 ) ) ;
#56158 = CARTESIAN_POINT ( 'NONE',  ( -0.3996062992125986035, -7.340648628747425578E-17, -2.401574803149606474 ) ) ;
#56159 = CARTESIAN_POINT ( 'NONE',  ( 0.1058382717557499880, 0.3949938075777411073, -1.568241469816272993 ) ) ;
#56160 = CARTESIAN_POINT ( 'NONE',  ( 0.3460692066303959757, -0.1998031496062991907, -2.782152230971128848 ) ) ;
#56161 = CARTESIAN_POINT ( 'NONE',  ( -0.5314960629921197111, 2.755905511811024056, -1.813482582612295557 ) ) ;
#56162 = CARTESIAN_POINT ( 'NONE',  ( -0.3917322834645669549, -0.1049643490035306603, -0.6679790026246718027 ) ) ;
#56163 = CARTESIAN_POINT ( 'NONE',  ( -0.6627296587926503335, -0.5511811023622046335, 0.09757992244046803654 ) ) ;
#56164 = CARTESIAN_POINT ( 'NONE',  ( -0.9251968503937002541, 0.1660481256975885056, 0.3530559997133364547 ) ) ;
#56165 = CARTESIAN_POINT ( 'NONE',  ( 0.4986876640419954376, 0.2306618581243848609, 0.2411417322834645549 ) ) ;
#56166 = CARTESIAN_POINT ( 'NONE',  ( -0.1058382717557497660, -0.3949938075777411073, -2.668635170603674833 ) ) ;
#56167 = CARTESIAN_POINT ( 'NONE',  ( 0.8792650918635177559, 0.05413385826771666132, 0.4176697321401328100 ) ) ;
#56168 = CARTESIAN_POINT ( 'NONE',  ( -1.437007874015747477, 0.1660481256975883668, -0.3530559997133364547 ) ) ;
#56169 = CARTESIAN_POINT ( 'NONE',  ( 1.161417322834646271, 0.1660481256975883668, -0.3530559997133364547 ) ) ;
#56170 = CARTESIAN_POINT ( 'NONE',  ( -0.2362204724409447953, -0.4091458600556404646, -2.585301837270341352 ) ) ;
#56171 = CARTESIAN_POINT ( 'NONE',  ( 4.893765752498283924E-17, -0.3996062992125986035, -2.283464566929133799 ) ) ;
#56172 = CARTESIAN_POINT ( 'NONE',  ( 1.581364829396326277, -0.3162353388693409650, -0.4822834645669289433 ) ) ;
#56173 = CARTESIAN_POINT ( 'NONE',  ( 0.8136482939632553313, 0.2306618581243848609, 0.2411417322834645549 ) ) ;
#56174 = CARTESIAN_POINT ( 'NONE',  ( 0.4330708661417329575, -0.6692913385826771977, 8.415575281601705876E-17 ) ) ;
#56175 = CARTESIAN_POINT ( 'NONE',  ( 1.246719160104987623, -0.3690944881889763329, 0.3153832671262228327 ) ) ;
#56177 = CARTESIAN_POINT ( 'NONE',  ( 1.614173228346457378, 0.2952755905511811885, 0.000000000000000000 ) ) ;
#56176 = CARTESIAN_POINT ( 'NONE',  ( 1.620734908136483465, -0.6692913385826771977, 0.1292274648535927661 ) ) ;
#56178 = CARTESIAN_POINT ( 'NONE',  ( -0.1049643490035301746, -0.3917322834645670659, -2.671896694716848764 ) ) ;
#56179 = CARTESIAN_POINT ( 'NONE',  ( -0.4037097067573596210, -2.567464376874931580E-15, -0.4445507791589072832 ) ) ;
#56180 = CARTESIAN_POINT ( 'NONE',  ( 0.6627296587926517768, -0.6692913385826773087, -0.1292274648535924053 ) ) ;
#56181 = CARTESIAN_POINT ( 'NONE',  ( 1.384514435695538559, 0.1771653543307087075, -0.09757992244046823083 ) ) ;
#56182 = CARTESIAN_POINT ( 'NONE',  ( -0.3149606299212590610, -0.1870078740157479769, 0.4822834645669291653 ) ) ;
#56183 = CARTESIAN_POINT ( 'NONE',  ( -0.3805774278215216522, -0.4281496062992127816, -0.4176697321401328100 ) ) ;
#56184 = CARTESIAN_POINT ( 'NONE',  ( -1.555118110236219930, -0.5400638737290845981, -0.3530559997133363437 ) ) ;
#56185 = CARTESIAN_POINT ( 'NONE',  ( -9.594673741351313045E-17, 0.3917322834645670104, -0.5570866141732284671 ) ) ;
#56186 = B_SPLINE_CURVE_WITH_KNOTS ( 'NONE', 3,
 ( #35933, #34271, #61176, #14919 ),
 .UNSPECIFIED., .F., .F.,
 ( 4, 4 ),
 ( 0.03408779003946453556, 0.03433871283135704611 ),
 .UNSPECIFIED. ) ;
#56187 = CARTESIAN_POINT ( 'NONE',  ( -0.2867679344610365999, 0.2867679344610364889, -1.586614173228346747 ) ) ;
#56188 = CARTESIAN_POINT ( 'NONE',  ( -0.3392501089628017219, -0.1958661417322836718, -2.249343832020997525 ) ) ;
#56189 = CARTESIAN_POINT ( 'NONE',  ( 1.561679790026247350, 0.05413385826771626580, -0.4176697321401330321 ) ) ;
#56190 = ORIENTED_EDGE ( 'NONE', *, *, #11815, .T. ) ;
#56191 = CARTESIAN_POINT ( 'NONE',  ( 0.1974969037888706369, -0.3420746716998659953, -2.611548556430445700 ) ) ;
#56192 = ORIENTED_EDGE ( 'NONE', *, *, #40980, .T. ) ;
#56193 = CARTESIAN_POINT ( 'NONE',  ( -0.7137454485294953965, 2.244094488188976388, -0.4917280318828581298 ) ) ;
#56194 = CIRCLE ( 'NONE', #14532, 0.2755905511811031494 ) ;
#56195 = CARTESIAN_POINT ( 'NONE',  ( 1.391076115485564868, -0.5023911411419708095, 0.1820866141732285504 ) ) ;
#56196 = CARTESIAN_POINT ( 'NONE',  ( -0.1070741851644051862, -0.3996062992125987146, -1.646981627296587591 ) ) ;
#56197 = CARTESIAN_POINT ( 'NONE',  ( 1.620734908136483465, -0.5511811023622046335, 0.09757992244046803654 ) ) ;
#56198 = CARTESIAN_POINT ( 'NONE',  ( -0.09115970038225217065, 2.409604939980833412E-17, -0.3464511005275205946 ) ) ;
#56199 = DIRECTION ( 'NONE',  ( 1.000000000000000000, 0.000000000000000000, 0.000000000000000000 ) ) ;
#56200 = CARTESIAN_POINT ( 'NONE',  ( -0.1502557399355928802, 1.937763785080233836, 0.2750001312974072465 ) ) ;
#56201 = CARTESIAN_POINT ( 'NONE',  ( -0.1958661417322834220, -0.3392501089628018884, -0.3077427821522311091 ) ) ;
#56202 = CARTESIAN_POINT ( 'NONE',  ( -0.7414698162729651543, -0.5511811023622046335, 0.09757992244046803654 ) ) ;
#56203 = CARTESIAN_POINT ( 'NONE',  ( -1.279527559055116948, -0.4536011799217367080, 0.2665933059059888421 ) ) ;
#56204 = CARTESIAN_POINT ( 'NONE',  ( 0.1640419947506569498, -0.05778040916215522460, 0.4822834645669289988 ) ) ;
#56205 = CARTESIAN_POINT ( 'NONE',  ( -1.312335958005248715, 0.2306618581243848609, 0.2411417322834645549 ) ) ;
#56206 = CARTESIAN_POINT ( 'NONE',  ( 0.3392501089628018884, -0.1958661417322834220, -0.09711286089238840846 ) ) ;
#56207 = ORIENTED_EDGE ( 'NONE', *, *, #41448, .F. ) ;
#56208 = EDGE_CURVE ( 'NONE', #23435, #32357, #69259, .T. ) ;
#56209 = CARTESIAN_POINT ( 'NONE',  ( 1.476377952755906220, 0.1660481256975883668, -0.3530559997133364547 ) ) ;
#56210 = CARTESIAN_POINT ( 'NONE',  ( -1.607029103917716251, 0.2931852734392842996, 0.04634085041582033243 ) ) ;
#56212 = EDGE_CURVE ( 'NONE', #43140, #66780, #8949, .T. ) ;
#56211 = CARTESIAN_POINT ( 'NONE',  ( 0.2362204724409451007, -0.4091458600556402980, -1.509186351706036655 ) ) ;
#56213 = DIRECTION ( 'NONE',  ( 0.000000000000000000, -0.000000000000000000, -1.000000000000000000 ) ) ;
#56214 =( BOUNDED_CURVE ( )  B_SPLINE_CURVE ( 2, ( #78637, #46619, #28922, #54590, #9167, #72314, #60499, #80300, #28099, #22614, #14661, #48274, #15488 ),
 .UNSPECIFIED., .F., .F. ) 
 B_SPLINE_CURVE_WITH_KNOTS ( ( 3, 2, 2, 2, 2, 2, 3 ),
 ( 0.6881378855240347647, 0.6916666666666666519, 0.6958333333333333037, 0.6999999999999999556, 0.7041666666666666075, 0.7083333333333332593, 0.7124999999999999112 ),
 .UNSPECIFIED. ) 
 CURVE ( )  GEOMETRIC_REPRESENTATION_ITEM ( )  RATIONAL_B_SPLINE_CURVE ( ( 0.9911642120907970810, 0.9711423276059441001, 1.000000000000000000, 0.9659258262890683122, 1.000000000000000000, 0.9659258262890683122, 1.000000000000000000, 0.9659258262890683122, 1.000000000000000000, 0.9659258262890683122, 1.000000000000000000, 0.9659258262890692004, 0.9999999999999991118 ) ) 
 REPRESENTATION_ITEM ( '' )  );
#56215 = CARTESIAN_POINT ( 'NONE',  ( -0.5839895013123351797, -0.5511811023622046335, 0.09757992244046803654 ) ) ;
#56216 = EDGE_CURVE ( 'NONE', #60118, #80363, #26185, .T. ) ;
#56217 = CARTESIAN_POINT ( 'NONE',  ( 3.900966923095589678, 2.559055118110236560, 0.5314960629921260393 ) ) ;
#56218 = CARTESIAN_POINT ( 'NONE',  ( -1.253280839895012377, -0.3162353388693409650, -0.4822834645669289433 ) ) ;
#56219 = CARTESIAN_POINT ( 'NONE',  ( 1.089238845144357759, 0.05413385826771626580, -0.4176697321401330321 ) ) ;
#56220 = ORIENTED_EDGE ( 'NONE', *, *, #31371, .F. ) ;
#56222 = CARTESIAN_POINT ( 'NONE',  ( 0.6889763779527563470, 0.1012011053420775880, -0.2882089793578257453 ) ) ;
#56221 = CARTESIAN_POINT ( 'NONE',  ( 0.7758157084527484981, 0.02791078216816508459, -0.4328096321851889194 ) ) ;
#56223 = CARTESIAN_POINT ( 'NONE',  ( 1.614173228346457378, -0.6692913385826771977, 8.415575281601705876E-17 ) ) ;
#56224 = CARTESIAN_POINT ( 'NONE',  ( -1.358267716535432434, 0.1660481256975883668, -0.3530559997133364547 ) ) ;
#56225 = CARTESIAN_POINT ( 'NONE',  ( -0.1049643490035301746, -0.3917322834645670659, -0.4671722852680298410 ) ) ;
#56226 = CARTESIAN_POINT ( 'NONE',  ( 0.1115485564304467270, -0.5511811023622048555, -0.09757992244046775898 ) ) ;
#56227 = CARTESIAN_POINT ( 'NONE',  ( -0.2867679344610366554, 0.2867679344610365444, -1.049212598425196985 ) ) ;
#56228 = CARTESIAN_POINT ( 'NONE',  ( 0.02624671916010564918, -0.5023911411419708095, -0.1820866141732282451 ) ) ;
#56229 = CARTESIAN_POINT ( 'NONE',  ( 0.4068241469816279987, -0.3690944881889765550, -0.3153832671262227771 ) ) ;
#56230 = CARTESIAN_POINT ( 'NONE',  ( 0.5511811023622054106, -0.1870078740157480879, -0.4822834645669291653 ) ) ;
#56231 = CARTESIAN_POINT ( 'NONE',  ( -0.9251968503937002541, -0.4536011799217368745, -0.2665933059059886201 ) ) ;
#56232 = CARTESIAN_POINT ( 'NONE',  ( 0.3917322834645670104, 2.398668435337828261E-17, -2.314960629921259727 ) ) ;
#56233 = CARTESIAN_POINT ( 'NONE',  ( 1.515748031496063186, -0.5400638737290845981, -0.3530559997133363437 ) ) ;
#56234 = ADVANCED_FACE ( 'NONE', ( #49058 ), #81487, .F. ) ;
#56235 = CARTESIAN_POINT ( 'NONE',  ( -0.8858267716535425107, -0.5400638737290844871, 0.3530559997133364547 ) ) ;
#56236 = CARTESIAN_POINT ( 'NONE',  ( 0.4724409448818898682, 2.892866454678787531E-17, -0.6673228346456693272 ) ) ;
#56237 = CARTESIAN_POINT ( 'NONE',  ( 0.03937007874015806264, 0.2952755905511811885, 0.000000000000000000 ) ) ;
#56238 = CARTESIAN_POINT ( 'NONE',  ( -0.7217847769028863381, -0.4281496062992124485, 0.4176697321401328655 ) ) ;
#56239 = CARTESIAN_POINT ( 'NONE',  ( 1.227034120734908917, 0.1771653543307087075, -0.09757992244046823083 ) ) ;
#56240 = CARTESIAN_POINT ( 'NONE',  ( 0.2821522309711292364, -0.5511811023622046335, 0.09757992244046803654 ) ) ;
#56241 = CARTESIAN_POINT ( 'NONE',  ( -0.1706036745406816491, -0.4281496062992124485, 0.4176697321401328655 ) ) ;
#56242 = CARTESIAN_POINT ( 'NONE',  ( -0.9973753280839886548, 0.2306618581243848609, 0.2411417322834645549 ) ) ;
#56243 = CARTESIAN_POINT ( 'NONE',  ( -0.3503937007874015630, 0.000000000000000000, -0.3051181102362204856 ) ) ;
#56244 = FACE_OUTER_BOUND ( 'NONE', #43566, .T. ) ;
#56245 = CARTESIAN_POINT ( 'NONE',  ( -0.07874015748031421014, -0.1870078740157479769, 0.4822834645669291653 ) ) ;
#56246 = ORIENTED_EDGE ( 'NONE', *, *, #83089, .T. ) ;
#56247 = CARTESIAN_POINT ( 'NONE',  ( -0.3996062992125985480, -7.340648628747423112E-17, -2.005905511811023612 ) ) ;
#56248 = CARTESIAN_POINT ( 'NONE',  ( 1.266404199475066328, -0.05778040916215522460, 0.4822834645669289988 ) ) ;
#56249 = CARTESIAN_POINT ( 'NONE',  ( -0.8333333333333323711, -0.5511811023622048555, -0.09757992244046775898 ) ) ;
#56250 = CARTESIAN_POINT ( 'NONE',  ( -0.7086614173228339419, -0.1870078740157480879, -0.4822834645669291653 ) ) ;
#56251 = CARTESIAN_POINT ( 'NONE',  ( 1.443569553805774897, -0.6046776061558809534, -0.2411417322834644161 ) ) ;
#56252 = CARTESIAN_POINT ( 'NONE',  ( 1.010498687664042716, -0.4281496062992124485, 0.4176697321401328655 ) ) ;
#56253 = CARTESIAN_POINT ( 'NONE',  ( -1.594488188976377119, 0.1660481256975883668, -0.3530559997133364547 ) ) ;
#56254 = CARTESIAN_POINT ( 'NONE',  ( -1.036745406824146176, -0.004921259842519870586, -0.3153832671262229437 ) ) ;
#56255 = CARTESIAN_POINT ( 'NONE',  ( 0.1070741851644054637, -0.3996062992125984925, -0.6345144356955381149 ) ) ;
#56256 = CARTESIAN_POINT ( 'NONE',  ( -0.3996062992125986035, -7.340648628747425578E-17, -0.5118110236220472231 ) ) ;
#56257 = CARTESIAN_POINT ( 'NONE',  ( 0.1058382717557500713, -0.3949938075777409408, -0.08530183727034125474 ) ) ;
#56258 = CARTESIAN_POINT ( 'NONE',  ( 0.2733222648309123204, 1.149615049381084608, -1.456396182690151031 ) ) ;
#56259 = CARTESIAN_POINT ( 'NONE',  ( 0.9776902887139113929, -0.5511811023622048555, -0.09757992244046775898 ) ) ;
#56260 = CARTESIAN_POINT ( 'NONE',  ( 0.5971128608923890191, -0.5511811023622046335, 0.09757992244046803654 ) ) ;
#56261 = CARTESIAN_POINT ( 'NONE',  ( 0.3215223097112867578, -0.05778040916215522460, 0.4822834645669289988 ) ) ;
#56262 = CARTESIAN_POINT ( 'NONE',  ( 0.1265901696524990572, -0.4724409448818897017, -2.366797900262467280 ) ) ;
#56263 = CARTESIAN_POINT ( 'NONE',  ( -0.1974969037888706924, 0.3420746716998658843, -0.7198162729658792447 ) ) ;
#56264 = CARTESIAN_POINT ( 'NONE',  ( 0.6758530183727039509, -0.5511811023622046335, 0.09757992244046803654 ) ) ;
#56265 = CARTESIAN_POINT ( 'NONE',  ( -0.2034120734908128059, 0.2952755905511811885, 0.1292274648535926551 ) ) ;
#56266 = CARTESIAN_POINT ( 'NONE',  ( -0.9120734908136475250, -0.6692913385826773087, -0.1292274648535924053 ) ) ;
#56267 = CARTESIAN_POINT ( 'NONE',  ( 1.089238845144357759, 0.05413385826771626580, -0.4176697321401330321 ) ) ;
#56268 = CARTESIAN_POINT ( 'NONE',  ( -0.3458507752293906723, -0.3458507752293910609, -1.318897637795275690 ) ) ;
#56269 = CARTESIAN_POINT ( 'NONE',  ( 0.3460692066303959757, -0.1998031496062991907, -2.152230971128608950 ) ) ;
#56270 = CARTESIAN_POINT ( 'NONE',  ( 0.06561679790026316017, -0.004921259842519870586, -0.3153832671262229437 ) ) ;
#56271 = EDGE_LOOP ( 'NONE', ( #11894, #789, #44367, #47159 ) ) ;
#56272 = CARTESIAN_POINT ( 'NONE',  ( -0.1958661417322833942, -0.3392501089628018884, -0.6922765336296082817 ) ) ;
#56273 = ORIENTED_EDGE ( 'NONE', *, *, #82019, .F. ) ;
#56274 = CARTESIAN_POINT ( 'NONE',  ( -0.8464566929133852113, -0.5400638737290845981, -0.3530559997133363437 ) ) ;
#56275 = CARTESIAN_POINT ( 'NONE',  ( -0.2755905511811015396, -0.6692913385826771977, 8.415575281601705876E-17 ) ) ;
#56276 = CARTESIAN_POINT ( 'NONE',  ( -0.5380577427821514602, 0.05413385826771666132, 0.4176697321401328100 ) ) ;
#56277 = CARTESIAN_POINT ( 'NONE',  ( 0.4790026246719168435, -0.3162353388693409650, -0.4822834645669289433 ) ) ;
#56278 = CARTESIAN_POINT ( 'NONE',  ( -0.3477690288713902178, 0.2952755905511810774, -0.1292274648535930714 ) ) ;
#56279 = CARTESIAN_POINT ( 'NONE',  ( -1.220472440944881054, -0.6692913385826771977, 8.415575281601705876E-17 ) ) ;
#56280 = CARTESIAN_POINT ( 'NONE',  ( -0.9317585301837263412, 0.05413385826771666132, 0.4176697321401328100 ) ) ;
#56281 = CARTESIAN_POINT ( 'NONE',  ( 0.6692913385826777528, 0.2952755905511811885, 0.000000000000000000 ) ) ;
#56282 = ADVANCED_FACE ( 'NONE', ( #4452 ), #76399, .F. ) ;
#56283 =( BOUNDED_SURFACE ( )  B_SPLINE_SURFACE ( 1, 2, ( 
 ( #55641, #23254, #67892, #35478, #74624, #67061, #81352, #36300, #60322, #74205, #42607, #73375, #15304, #35065, #61142, #9394, #80534, #22845, #3909, #48505, #60730, #16132, #4313, #29159, #3082, #2671, #28746, #28330, #48924, #22437, #54408, #10229, #53992, #35896, #79704, #16968, #80119, #73796, #48097, #29977, #3494, #40967, #22020, #66649, #8985, #41779, #64037, #63622, #70347, #43420, #75447, #30806, #6376, #31629, #43012, #12702, #62807, #25307, #81767, #82575, #63210, #24894, #50972, #32048, #37945, #38361, #57707, #5141, #11465, #37534, #5550, #68707, #70, #82987, #25724, #17785, #50157, #11882, #69117, #75036, #17382, #44244, #76669, #37123, #19002, #31214, #76266, #30392, #56471, #56882, #18601, #56057, #11048, #24077, #36706, #50563, #69933, #18195, #62380, #82174, #4718, #24490, #12289, #75853, #57289, #43828, #49746, #5959, #44651, #69532, #14388, #72032, #26147, #65310, #7215, #8065, #77934, #45497, #58981, #58125, #6790, #33726, #20264, #59804, #45073, #2158, #32463, #64455, #71194, #59388, #13536, #492, #46338, #46758, #1746, #1336, #33319, #70776, #7649, #52231, #32886, #45914, #51808, #40046, #77513, #71611, #77089, #72451, #19848, #19421, #26986, #58555, #14800, #39192, #13127, #65732, #27403, #38778, #921, #53063, #13964, #34143, #78775, #64876, #66136, #26578, #8474, #40457, #52650, #39620, #78355, #51384, #20686, #21099, #72861, #73281, #2989, #40870, #53485, #73703, #41286, #15210, #22751, #42102, #79609, #74111, #42511, #9305, #16874, #66552, #8885, #35387, #61052, #54314, #79195, #28236, #34561, #47587, #67381, #53895, #10136, #21926, #21511, #3402, #29065, #15629, #16457, #48411, #2577, #41689, #66972, #67799, #80025, #34975, #54736, #60227, #60638, #35800, #22344, #36208, #47169, #61877, #28655, #48004, #16043, #61467, #9716, #80441, #3815, #23158, #29476, #55135, #80845, #48827, #74528, #68213, #10550, #27825, #10951, #50467, #30295, #82079, #29882, #82893, #42916, #55545, #69437, #43320, #25213, #68611, #81254, #18508, #76171, #23569, #11371, #44151, #30717, #70247, #5859, #4624, #18907, #49240, #44557, #50879, #43733, #74943, #17288, #12603, #23985, #76579, #36608, #49652, #62710, #62287, #55961, #50063, #17691, #81674, #82484, #69843, #75344, #12193, #38260, #69020, #75758, #11790, #37850, #4218, #63528, #37028, #5048, #56380, #24392, #18100, #37443, #63117, #5455, #31535, #31116, #56784, #24799, #57191, #32363, #52960, #78674, #33213, #65630, #58025, #7961, #77832, #65204, #19320, #389, #20162, #7541, #44972, #46236, #26047, #70668, #58877, #59286, #20584, #13857, #45812, #83302, #71510, #64773, #19742, #32783, #13024, #26884, #6693, #58452, #6274, #1643, #38678, #31950, #39516, #45396, #27301, #64356, #57611, #78253, #52544, #25624, #71093, #71932, #7112, #46657, #33623, #51705, #20995, #51287, #72351, #14698, #1235, #76990, #77407, #63938, #13436, #39092, #811, #26474, #52124, #14281, #39945, #2886, #53790, #27718, #35282, #54624, #8782, #3295, #55035, #21816, #28548, #47892, #74006, #80742, #28959, #35692, #61357, #79501, #60124, #54204, #79921, #34037, #23056, #48309, #3711, #66446, #15523, #60535, #34455, #29374, #48724, #9612, #41997, #2475, #67692, #22237, #41589, #79092, #28134, #73600, #67279, #21411, #74421, #47064, #2054, #15942, #60944, #66871, #8371, #40761, #53385, #47480, #80335, #73173, #22650, #41181, #59699, #16353, #10027, #9201, #40354, #66033, #15105, #72756, #34874, #56683, #43221, #10851, #24290, #23469, #55444, #82384, #68919, #25108, #10449, #50781, #81153, #29782, #36512, #56279, #17589, #55857, #11269, #49136, #63018, #42817, #36928, #42405, #12091, #74840, #68103, #81976, #81567, #37747, #17184, #36105, #31014, #5355, #61776, #23885, #24701, #62605, #82787, #18410, #68511, #31429, #4117, #57091, #63422, #49962, #62188, #4525, #16768, #30195, #5759, #49550, #75245, #4946, #30616, #75659, #18000, #43634, #69337, #11687, #50370, #37345, #76068, #44053, #69745, #65833, #1851, #27931, #34673, #40561, #72966, #15317, #7757, #14076, #40149, #8166, #70146, #60336, #2268, #40982, #20374, #52758 ),
 ( #63834, #1439, #59913, #21205, #12498, #6171, #14901, #53589, #14496, #28344, #46026, #39728, #78884, #31846, #65423, #27513, #57509, #76482, #9001, #46860, #72554, #66242, #20791, #71720, #2684, #33423, #38160, #18809, #33831, #8580, #59084, #66662, #27096, #78466, #53169, #44455, #83200, #78045, #79298, #59498, #34252, #21616, #25522, #46447, #72140, #47276, #52338, #49353, #75050, #67486, #73811, #16566, #42211, #47694, #36721, #61990, #17397, #80133, #29177, #74221, #22454, #43027, #68722, #23269, #55656, #48113, #81366, #67907, #55247, #9408, #16148, #10243, #80954, #35078, #11063, #60744, #15740, #61580, #3925, #80548, #22033, #54423, #67076, #41795, #35914, #9821, #36315, #35492, #73389, #29584, #48938, #61157, #16982, #74640, #28760, #42625, #3508, #10660, #22860, #54844, #68322, #3096, #48521, #4327, #29993, #62397, #41394, #4736, #23679, #54005, #79717, #12717, #50173, #37138, #25323, #25740, #70362, #63637, #12304, #49762, #69949, #31229, #69549, #82591, #62823, #76685, #56487, #24910, #56076, #51401, #69132, #81782, #37960, #11897, #77105, #11484, #24093, #44666, #19018, #75462, #37550, #38377, #56897, #13144, #32063, #30822, #45088, #17801, #70792, #19437, #5975, #43435, #5157, #38795, #75868, #64471, #82189, #18211, #5565, #24506, #43846, #76285, #63225, #50578, #50987, #64053, #18616, #6393, #30409, #44259, #31646, #57304, #57724, #83002, #87, #33743, #13553, #32903, #52246, #53079, #58571, #59404, #40060, #46354, #47186, #14816, #1761, #27003, #66153, #7231, #72878, #27841, #51825, #65747, #34159, #39209, #15226, #26594, #58996, #64892, #72049, #14406, #78791, #8080, #936, #7664, #59820, #20703, #77951, #77530, #20280, #19865, #21116, #13979, #45929, #27418, #45514, #46776, #71210, #72467, #71627, #65327, #39636, #79211, #52665, #53503, #33335, #40475, #8492, #2175, #21527, #40886, #6808, #1352, #78371, #32479, #58141, #510, #26164, #4233, #54331, #16890, #73297, #74128, #16473, #42529, #53912, #61892, #23174, #67815, #61067, #36223, #80041, #79626, #66988, #15646, #68231, #42119, #48843, #35818, #29492, #29897, #21943, #73719, #74545, #10152, #2594, #47603, #3832, #10565, #3418, #17304, #9320, #28670, #61483, #41302, #22360, #55151, #34990, #66568, #81269, #80862, #55560, #23585, #9732, #60655, #49256, #48019, #60246, #74958, #54751, #8902, #16058, #34578, #3004, #41704, #28252, #67397, #35402, #29081, #80457, #22766, #48428, #36625, #25640, #50892, #6290, #69034, #18113, #63130, #11385, #31965, #57626, #12207, #44571, #37042, #70262, #56797, #44164, #81689, #62724, #82497, #69857, #24000, #59825, #49668, #4639, #50480, #76184, #69452, #10966, #43334, #55978, #5062, #24813, #30731, #25227, #56393, #62302, #18521, #37865, #82092, #5873, #63541, #17706, #31548, #24406, #82906, #11802, #50076, #57205, #75358, #75771, #76592, #37457, #51303, #30310, #77005, #43746, #5468, #31131, #18922, #12617, #38276, #63953, #42931, #68626, #52560, #1253, #38693, #58893, #20177, #58468, #71526, #26062, #65647, #45412, #13873, #44988, #14715, #58041, #70687, #26901, #831, #40370, #406, #13040, #33641, #7977, #64371, #26490, #59303, #45827, #2071, #21013, #19759, #34053, #6708, #59716, #66051, #78269, #32377, #51721, #27737, #39107, #8388, #77424, #64789, #77848, #71108, #13451, #65221, #32800, #7127, #14301, #1660, #52142, #27317, #53402, #39532, #7559, #20600, #52976, #19336, #78690, #33230, #46252, #71948, #39961, #46674, #72367, #15959, #55051, #79520, #36120, #16784, #40778, #54643, #23072, #28152, #4133, #15541, #47912, #53807, #35299, #60961, #42015, #3311, #21835, #79939, #48740, #9629, #66888, #66463, #73190, #8799, #67708, #2903, #9218, #48325, #34475, #28976, #60141, #61378, #34891, #54223, #47498, #68122, #41606, #42422, #2492, #35708, #80758, #74438, #10467, #10044, #61793, #41200, #60553, #28567, #29798, #3727, #47082, #79110, #22254, #29391, #73617, #80353, #22666, #21428, #67295, #72773, #15124, #74022, #16368, #25126, #68935, #42833, #55873, #4540, #57107, #31032, #37764, #24717, #18427, #76497, #68526, #62621, #63439, #82399, #74858 ) ),
 .UNSPECIFIED., .F., .F., .F. ) 
 B_SPLINE_SURFACE_WITH_KNOTS ( ( 2, 2 ),
 ( 3, 2, 2, 2, 2, 2, 2, 2, 2, 2, 2, 2, 2, 2, 2, 2, 2, 2, 2, 2, 2, 2, 2, 2, 2, 2, 2, 2, 2, 2, 2, 2, 2, 2, 2, 2, 2, 2, 2, 2, 2, 2, 2, 2, 2, 2, 2, 2, 2, 2, 2, 2, 2, 2, 2, 2, 2, 2, 2, 2, 2, 2, 2, 2, 2, 2, 2, 2, 2, 2, 2, 2, 2, 2, 2, 2, 2, 2, 2, 2, 2, 2, 2, 2, 2, 2, 2, 2, 2, 2, 2, 2, 2, 2, 2, 2, 2, 2, 2, 2, 2, 2, 2, 2, 2, 2, 2, 2, 2, 2, 2, 2, 2, 2, 2, 2, 2, 2, 2, 2, 2, 2, 2, 2, 2, 2, 2, 2, 2, 2, 2, 2, 2, 2, 2, 2, 2, 2, 2, 2, 2, 2, 2, 2, 2, 2, 2, 2, 2, 2, 2, 2, 2, 2, 2, 2, 2, 2, 2, 2, 2, 2, 2, 2, 2, 2, 2, 2, 2, 2, 2, 2, 2, 2, 2, 2, 2, 2, 2, 2, 2, 2, 2, 2, 2, 2, 2, 2, 2, 2, 2, 2, 2, 2, 2, 2, 2, 2, 2, 2, 2, 2, 2, 2, 2, 2, 2, 2, 2, 2, 2, 2, 2, 2, 2, 2, 2, 2, 2, 2, 2, 2, 2, 2, 2, 2, 2, 2, 2, 2, 2, 2, 2, 2, 2, 2, 2, 2, 2, 2, 2, 2, 2, 2, 2, 2, 2, 2, 2, 2, 2, 2, 2, 2, 2, 3 ),
 ( 0.000000000000000000, 1.000000000000000000 ),
 ( 0.000000000000000000, 0.003787878787878787984, 0.007575757575757575968, 0.01136363636363636395, 0.01515151515151515194, 0.01893939393939393992, 0.02272727272727272790, 0.02651515151515151589, 0.03030303030303030387, 0.03409090909090908839, 0.03787878787878787984, 0.04166666666666666435, 0.04545454545454545581, 0.04924242424242424032, 0.05303030303030303177, 0.05681818181818181629, 0.06060606060606060774, 0.06439393939393939226, 0.06818181818181817677, 0.07196969696969697516, 0.07575757575757575968, 0.07954545454545454419, 0.08333333333333332871, 0.08712121212121212710, 0.09090909090909091161, 0.09469696969696969613, 0.09848484848484848064, 0.1022727272727272790, 0.1060606060606060635, 0.1098484848484848481, 0.1136363636363636326, 0.1174242424242424310, 0.1212121212121212155, 0.1250000000000000000, 0.1287878787878787845, 0.1325757575757575690, 0.1363636363636363535, 0.1401515151515151381, 0.1439393939393939503, 0.1477272727272727348, 0.1515151515151515194, 0.1553030303030303039, 0.1590909090909090884, 0.1628787878787878729, 0.1666666666666666574, 0.1704545454545454419, 0.1742424242424242542, 0.1780303030303030387, 0.1818181818181818232, 0.1856060606060606077, 0.1893939393939393923, 0.1931818181818181768, 0.1969696969696969613, 0.2007575757575757458, 0.2045454545454545581, 0.2083333333333333426, 0.2121212121212121271, 0.2159090909090909116, 0.2196969696969696961, 0.2234848484848484806, 0.2272727272727272652, 0.2310606060606060497, 0.2348484848484848619, 0.2386363636363636465, 0.2424242424242424310, 0.2462121212121212155, 0.2500000000000000000, 0.2537878787878787845, 0.2575757575757575690, 0.2613636363636363535, 0.2651515151515151381, 0.2689393939393939226, 0.2727272727272727071, 0.2765151515151514916, 0.2803030303030302761, 0.2840909090909091161, 0.2878787878787879007, 0.2916666666666666852, 0.2954545454545454697, 0.2992424242424242542, 0.3030303030303030387, 0.3068181818181818232, 0.3106060606060606077, 0.3143939393939393923, 0.3181818181818181768, 0.3219696969696969613, 0.3257575757575757458, 0.3295454545454545303, 0.3333333333333333148, 0.3371212121212120993, 0.3409090909090908839, 0.3446969696969697239, 0.3484848484848485084, 0.3522727272727272929, 0.3560606060606060774, 0.3598484848484848619, 0.3636363636363636465, 0.3674242424242424310, 0.3712121212121212155, 0.3750000000000000000, 0.3787878787878787845, 0.3825757575757575690, 0.3863636363636363535, 0.3901515151515151381, 0.3939393939393939226, 0.3977272727272727071, 0.4015151515151514916, 0.4053030303030302761, 0.4090909090909091161, 0.4128787878787879007, 0.4166666666666666852, 0.4204545454545454697, 0.4242424242424242542, 0.4280303030303030387, 0.4318181818181818232, 0.4356060606060606077, 0.4393939393939393923, 0.4431818181818181768, 0.4469696969696969613, 0.4507575757575757458, 0.4545454545454545303, 0.4583333333333333148, 0.4621212121212120993, 0.4659090909090908839, 0.4696969696969697239, 0.4734848484848485084, 0.4772727272727272929, 0.4810606060606060774, 0.4848484848484848619, 0.4886363636363636465, 0.4924242424242424310, 0.4962121212121212155, 0.5000000000000000000, 0.5037878787878787845, 0.5075757575757575690, 0.5113636363636363535, 0.5151515151515151381, 0.5189393939393939226, 0.5227272727272727071, 0.5265151515151514916, 0.5303030303030302761, 0.5340909090909090606, 0.5378787878787878451, 0.5416666666666666297, 0.5454545454545454142, 0.5492424242424241987, 0.5530303030303029832, 0.5568181818181817677, 0.5606060606060605522, 0.5643939393939394478, 0.5681818181818182323, 0.5719696969696970168, 0.5757575757575758013, 0.5795454545454545858, 0.5833333333333333703, 0.5871212121212121549, 0.5909090909090909394, 0.5946969696969697239, 0.5984848484848485084, 0.6022727272727272929, 0.6060606060606060774, 0.6098484848484848619, 0.6136363636363636465, 0.6174242424242424310, 0.6212121212121212155, 0.6250000000000000000, 0.6287878787878787845, 0.6325757575757575690, 0.6363636363636363535, 0.6401515151515151381, 0.6439393939393939226, 0.6477272727272727071, 0.6515151515151514916, 0.6553030303030302761, 0.6590909090909090606, 0.6628787878787878451, 0.6666666666666666297, 0.6704545454545454142, 0.6742424242424241987, 0.6780303030303029832, 0.6818181818181817677, 0.6856060606060605522, 0.6893939393939394478, 0.6931818181818182323, 0.6969696969696970168, 0.7007575757575758013, 0.7045454545454545858, 0.7083333333333333703, 0.7121212121212121549, 0.7159090909090909394, 0.7196969696969697239, 0.7234848484848485084, 0.7272727272727272929, 0.7310606060606060774, 0.7348484848484848619, 0.7386363636363636465, 0.7424242424242424310, 0.7462121212121212155, 0.7500000000000000000, 0.7537878787878787845, 0.7575757575757575690, 0.7613636363636363535, 0.7651515151515151381, 0.7689393939393939226, 0.7727272727272727071, 0.7765151515151514916, 0.7803030303030302761, 0.7840909090909090606, 0.7878787878787878451, 0.7916666666666666297, 0.7954545454545454142, 0.7992424242424241987, 0.8030303030303029832, 0.8068181818181817677, 0.8106060606060605522, 0.8143939393939394478, 0.8181818181818182323, 0.8219696969696970168, 0.8257575757575758013, 0.8295454545454545858, 0.8333333333333333703, 0.8371212121212121549, 0.8409090909090909394, 0.8446969696969697239, 0.8484848484848485084, 0.8522727272727272929, 0.8560606060606060774, 0.8598484848484848619, 0.8636363636363636465, 0.8674242424242424310, 0.8712121212121212155, 0.8750000000000000000, 0.8787878787878787845, 0.8825757575757575690, 0.8863636363636363535, 0.8901515151515151381, 0.8939393939393939226, 0.8977272727272727071, 0.9015151515151514916, 0.9053030303030302761, 0.9090909090909090606, 0.9128787878787878451, 0.9166666666666666297, 0.9204545454545454142, 0.9242424242424241987, 0.9280303030303029832, 0.9318181818181817677, 0.9356060606060605522, 0.9393939393939394478, 0.9431818181818182323, 0.9469696969696970168, 0.9507575757575758013, 0.9545454545454545858, 0.9583333333333333703, 0.9621212121212121549, 0.9659090909090909394 ),
 .UNSPECIFIED. ) 
 GEOMETRIC_REPRESENTATION_ITEM ( )  RATIONAL_B_SPLINE_SURFACE ( (
 ( 1.000000000000000000, 0.9659258262890683122, 1.000000000000000000, 0.9659258262890683122, 1.000000000000000000, 0.9659258262890683122, 1.000000000000000000, 0.9659258262890683122, 1.000000000000000000, 0.9659258262890683122, 1.000000000000000000, 0.9659258262890683122, 1.000000000000000000, 0.9659258262890683122, 1.000000000000000000, 0.9659258262890683122, 1.000000000000000000, 0.9659258262890683122, 1.000000000000000000, 0.9659258262890683122, 1.000000000000000000, 0.9659258262890683122, 1.000000000000000000, 0.9659258262890683122, 1.000000000000000000, 0.9659258262890683122, 1.000000000000000000, 0.9659258262890683122, 1.000000000000000000, 0.9659258262890683122, 1.000000000000000000, 0.9659258262890683122, 1.000000000000000000, 0.9659258262890683122, 1.000000000000000000, 0.9659258262890683122, 1.000000000000000000, 0.9659258262890683122, 1.000000000000000000, 0.9659258262890683122, 1.000000000000000000, 0.9659258262890683122, 1.000000000000000000, 0.9659258262890683122, 1.000000000000000000, 0.9659258262890683122, 1.000000000000000000, 0.9659258262890683122, 1.000000000000000000, 0.9659258262890683122, 1.000000000000000000, 0.9659258262890683122, 1.000000000000000000, 0.9659258262890683122, 1.000000000000000000, 0.9659258262890683122, 1.000000000000000000, 0.9659258262890683122, 1.000000000000000000, 0.9659258262890683122, 1.000000000000000000, 0.9659258262890683122, 1.000000000000000000, 0.9659258262890683122, 1.000000000000000000, 0.9659258262890683122, 1.000000000000000000, 0.9659258262890683122, 1.000000000000000000, 0.9659258262890683122, 1.000000000000000000, 0.9659258262890683122, 1.000000000000000000, 0.9659258262890683122, 1.000000000000000000, 0.9659258262890683122, 1.000000000000000000, 0.9659258262890683122, 1.000000000000000000, 0.9659258262890683122, 1.000000000000000000, 0.9659258262890683122, 1.000000000000000000, 0.9659258262890683122, 1.000000000000000000, 0.9659258262890683122, 1.000000000000000000, 0.9659258262890683122, 1.000000000000000000, 0.9659258262890683122, 1.000000000000000000, 0.9659258262890683122, 1.000000000000000000, 0.9659258262890683122, 1.000000000000000000, 0.9659258262890683122, 1.000000000000000000, 0.9659258262890683122, 1.000000000000000000, 0.9659258262890683122, 1.000000000000000000, 0.9659258262890683122, 1.000000000000000000, 0.9659258262890683122, 1.000000000000000000, 0.9659258262890683122, 1.000000000000000000, 0.9659258262890683122, 1.000000000000000000, 0.9659258262890683122, 1.000000000000000000, 0.9659258262890683122, 1.000000000000000000, 0.9659258262890683122, 1.000000000000000000, 0.9659258262890683122, 1.000000000000000000, 0.9659258262890683122, 1.000000000000000000, 0.9659258262890683122, 1.000000000000000000, 0.9659258262890683122, 1.000000000000000000, 0.9659258262890683122, 1.000000000000000000, 0.9659258262890683122, 1.000000000000000000, 0.9659258262890683122, 1.000000000000000000, 0.9659258262890683122, 1.000000000000000000, 0.9659258262890683122, 1.000000000000000000, 0.9659258262890683122, 1.000000000000000000, 0.9659258262890683122, 1.000000000000000000, 0.9659258262890683122, 1.000000000000000000, 0.9659258262890683122, 1.000000000000000000, 0.9659258262890683122, 1.000000000000000000, 0.9659258262890683122, 1.000000000000000000, 0.9659258262890683122, 1.000000000000000000, 0.9659258262890683122, 1.000000000000000000, 0.9659258262890683122, 1.000000000000000000, 0.9659258262890683122, 1.000000000000000000, 0.9659258262890683122, 1.000000000000000000, 0.9659258262890683122, 1.000000000000000000, 0.9659258262890683122, 1.000000000000000000, 0.9659258262890683122, 1.000000000000000000, 0.9659258262890683122, 1.000000000000000000, 0.9659258262890683122, 1.000000000000000000, 0.9659258262890683122, 1.000000000000000000, 0.9659258262890683122, 1.000000000000000000, 0.9659258262890683122, 1.000000000000000000, 0.9659258262890683122, 1.000000000000000000, 0.9659258262890683122, 1.000000000000000000, 0.9659258262890683122, 1.000000000000000000, 0.9659258262890683122, 1.000000000000000000, 0.9659258262890683122, 1.000000000000000000, 0.9659258262890683122, 1.000000000000000000, 0.9659258262890683122, 1.000000000000000000, 0.9659258262890683122, 1.000000000000000000, 0.9659258262890683122, 1.000000000000000000, 0.9659258262890683122, 1.000000000000000000, 0.9659258262890683122, 1.000000000000000000, 0.9659258262890683122, 1.000000000000000000, 0.9659258262890683122, 1.000000000000000000, 0.9659258262890683122, 1.000000000000000000, 0.9659258262890683122, 1.000000000000000000, 0.9659258262890683122, 1.000000000000000000, 0.9659258262890683122, 1.000000000000000000, 0.9659258262890683122, 1.000000000000000000, 0.9659258262890683122, 1.000000000000000000, 0.9659258262890683122, 1.000000000000000000, 0.9659258262890683122, 1.000000000000000000, 0.9659258262890683122, 1.000000000000000000, 0.9659258262890683122, 1.000000000000000000, 0.9659258262890683122, 1.000000000000000000, 0.9659258262890683122, 1.000000000000000000, 0.9659258262890683122, 1.000000000000000000, 0.9659258262890683122, 1.000000000000000000, 0.9659258262890683122, 1.000000000000000000, 0.9659258262890683122, 1.000000000000000000, 0.9659258262890683122, 1.000000000000000000, 0.9659258262890683122, 1.000000000000000000, 0.9659258262890683122, 1.000000000000000000, 0.9659258262890683122, 1.000000000000000000, 0.9659258262890683122, 1.000000000000000000, 0.9659258262890683122, 1.000000000000000000, 0.9659258262890683122, 1.000000000000000000, 0.9659258262890683122, 1.000000000000000000, 0.9659258262890683122, 1.000000000000000000, 0.9659258262890683122, 1.000000000000000000, 0.9659258262890683122, 1.000000000000000000, 0.9659258262890683122, 1.000000000000000000, 0.9659258262890683122, 1.000000000000000000, 0.9659258262890683122, 1.000000000000000000, 0.9659258262890683122, 1.000000000000000000, 0.9659258262890683122, 1.000000000000000000, 0.9659258262890683122, 1.000000000000000000, 0.9659258262890683122, 1.000000000000000000, 0.9659258262890683122, 1.000000000000000000, 0.9659258262890683122, 1.000000000000000000, 0.9659258262890683122, 1.000000000000000000, 0.9659258262890683122, 1.000000000000000000, 0.9659258262890683122, 1.000000000000000000, 0.9659258262890683122, 1.000000000000000000, 0.9659258262890683122, 1.000000000000000000, 0.9659258262890683122, 1.000000000000000000, 0.9659258262890683122, 1.000000000000000000, 0.9659258262890683122, 1.000000000000000000, 0.9659258262890683122, 1.000000000000000000, 0.9659258262890683122, 1.000000000000000000, 0.9659258262890683122, 1.000000000000000000, 0.9659258262890683122, 1.000000000000000000, 0.9659258262890683122, 1.000000000000000000, 0.9659258262890683122, 1.000000000000000000, 0.9659258262890683122, 1.000000000000000000, 0.9659258262890683122, 1.000000000000000000, 0.9659258262890683122, 1.000000000000000000, 0.9659258262890683122, 1.000000000000000000, 0.9659258262890683122, 1.000000000000000000, 0.9659258262890683122, 1.000000000000000000, 0.9659258262890683122, 1.000000000000000000, 0.9659258262890683122, 1.000000000000000000, 0.9659258262890683122, 1.000000000000000000, 0.9659258262890683122, 1.000000000000000000, 0.9659258262890683122, 1.000000000000000000, 0.9659258262890683122, 1.000000000000000000, 0.9659258262890683122, 1.000000000000000000, 0.9659258262890683122, 1.000000000000000000, 0.9659258262890683122, 1.000000000000000000, 0.9659258262890683122, 1.000000000000000000, 0.9659258262890683122, 1.000000000000000000, 0.9659258262890683122, 1.000000000000000000, 0.9659258262890683122, 1.000000000000000000, 0.9659258262890683122, 1.000000000000000000, 0.9659258262890683122, 1.000000000000000000, 0.9659258262890683122, 1.000000000000000000, 0.9659258262890683122, 1.000000000000000000, 0.9659258262890683122, 1.000000000000000000, 0.9659258262890683122, 1.000000000000000000, 0.9659258262890683122, 1.000000000000000000, 0.9659258262890683122, 1.000000000000000000, 0.9659258262890683122, 1.000000000000000000, 0.9659258262890683122, 1.000000000000000000, 0.9659258262890683122, 1.000000000000000000, 0.9659258262890683122, 1.000000000000000000, 0.9659258262890683122, 1.000000000000000000, 0.9659258262890683122, 1.000000000000000000, 0.9659258262890683122, 1.000000000000000000, 0.9659258262890683122, 1.000000000000000000, 0.9659258262890683122, 1.000000000000000000, 0.9659258262890683122, 1.000000000000000000, 0.9659258262890683122, 1.000000000000000000, 0.9659258262890683122, 1.000000000000000000, 0.9659258262890683122, 1.000000000000000000, 0.9659258262890683122, 1.000000000000000000, 0.9659258262890683122, 1.000000000000000000, 0.9659258262890683122, 1.000000000000000000, 0.9659258262890683122, 1.000000000000000000, 0.9659258262890683122, 1.000000000000000000, 0.9659258262890683122, 1.000000000000000000, 0.9659258262890683122, 1.000000000000000000, 0.9659258262890683122, 1.000000000000000000, 0.9659258262890683122, 1.000000000000000000, 0.9659258262890683122, 1.000000000000000000, 0.9659258262890683122, 1.000000000000000000, 0.9659258262890683122, 1.000000000000000000, 0.9659258262890683122, 1.000000000000000000, 0.9659258262890683122, 1.000000000000000000, 0.9659258262890683122, 1.000000000000000000, 0.9659258262890683122, 1.000000000000000000, 0.9659258262890683122, 1.000000000000000000, 0.9659258262890683122, 1.000000000000000000, 0.9659258262890683122, 1.000000000000000000, 0.9659258262890683122, 1.000000000000000000, 0.9659258262890683122, 1.000000000000000000, 0.9659258262890683122, 1.000000000000000000, 0.9659258262890683122, 1.000000000000000000, 0.9659258262890683122, 1.000000000000000000, 0.9659258262890683122, 1.000000000000000000, 0.9659258262890683122, 1.000000000000000000, 0.9659258262890683122, 1.000000000000000000, 0.9659258262890683122, 1.000000000000000000, 0.9659258262890683122, 1.000000000000000000, 0.9659258262890683122, 1.000000000000000000, 0.9659258262890683122, 1.000000000000000000, 0.9659258262890683122, 1.000000000000000000, 0.9659258262890683122, 1.000000000000000000, 0.9659258262890683122, 1.000000000000000000, 0.9659258262890683122, 1.000000000000000000, 0.9659258262890683122, 1.000000000000000000, 0.9659258262890683122, 1.000000000000000000, 0.9659258262890683122, 1.000000000000000000, 0.9659258262890683122, 1.000000000000000000, 0.9659258262890683122, 1.000000000000000000, 0.9659258262890683122, 1.000000000000000000, 0.9659258262890683122, 1.000000000000000000, 0.9659258262890683122, 1.000000000000000000, 0.9659258262890683122, 1.000000000000000000, 0.9659258262890683122, 1.000000000000000000, 0.9659258262890683122, 1.000000000000000000, 0.9659258262890683122, 1.000000000000000000, 0.9659258262890683122, 1.000000000000000000, 0.9659258262890683122, 1.000000000000000000, 0.9659258262890683122, 1.000000000000000000, 0.9659258262890683122, 1.000000000000000000, 0.9659258262890683122, 1.000000000000000000, 0.9659258262890683122, 1.000000000000000000, 0.9659258262890683122, 1.000000000000000000, 0.9659258262890683122, 1.000000000000000000, 0.9659258262890683122, 1.000000000000000000, 0.9659258262890683122, 1.000000000000000000, 0.9659258262890683122, 1.000000000000000000, 0.9659258262890683122, 1.000000000000000000, 0.9659258262890683122, 1.000000000000000000, 0.9659258262890683122, 1.000000000000000000, 0.9659258262890683122, 1.000000000000000000, 0.9659258262890683122, 1.000000000000000000, 0.9659258262890683122, 1.000000000000000000, 0.9659258262890683122, 1.000000000000000000, 0.9659258262890683122, 1.000000000000000000, 0.9659258262890683122, 1.000000000000000000),
 ( 1.000000000000000000, 0.9659258262890683122, 1.000000000000000000, 0.9659258262890683122, 1.000000000000000000, 0.9659258262890683122, 1.000000000000000000, 0.9659258262890683122, 1.000000000000000000, 0.9659258262890683122, 1.000000000000000000, 0.9659258262890683122, 1.000000000000000000, 0.9659258262890683122, 1.000000000000000000, 0.9659258262890683122, 1.000000000000000000, 0.9659258262890683122, 1.000000000000000000, 0.9659258262890683122, 1.000000000000000000, 0.9659258262890683122, 1.000000000000000000, 0.9659258262890683122, 1.000000000000000000, 0.9659258262890683122, 1.000000000000000000, 0.9659258262890683122, 1.000000000000000000, 0.9659258262890683122, 1.000000000000000000, 0.9659258262890683122, 1.000000000000000000, 0.9659258262890683122, 1.000000000000000000, 0.9659258262890683122, 1.000000000000000000, 0.9659258262890683122, 1.000000000000000000, 0.9659258262890683122, 1.000000000000000000, 0.9659258262890683122, 1.000000000000000000, 0.9659258262890683122, 1.000000000000000000, 0.9659258262890683122, 1.000000000000000000, 0.9659258262890683122, 1.000000000000000000, 0.9659258262890683122, 1.000000000000000000, 0.9659258262890683122, 1.000000000000000000, 0.9659258262890683122, 1.000000000000000000, 0.9659258262890683122, 1.000000000000000000, 0.9659258262890683122, 1.000000000000000000, 0.9659258262890683122, 1.000000000000000000, 0.9659258262890683122, 1.000000000000000000, 0.9659258262890683122, 1.000000000000000000, 0.9659258262890683122, 1.000000000000000000, 0.9659258262890683122, 1.000000000000000000, 0.9659258262890683122, 1.000000000000000000, 0.9659258262890683122, 1.000000000000000000, 0.9659258262890683122, 1.000000000000000000, 0.9659258262890683122, 1.000000000000000000, 0.9659258262890683122, 1.000000000000000000, 0.9659258262890683122, 1.000000000000000000, 0.9659258262890683122, 1.000000000000000000, 0.9659258262890683122, 1.000000000000000000, 0.9659258262890683122, 1.000000000000000000, 0.9659258262890683122, 1.000000000000000000, 0.9659258262890683122, 1.000000000000000000, 0.9659258262890683122, 1.000000000000000000, 0.9659258262890683122, 1.000000000000000000, 0.9659258262890683122, 1.000000000000000000, 0.9659258262890683122, 1.000000000000000000, 0.9659258262890683122, 1.000000000000000000, 0.9659258262890683122, 1.000000000000000000, 0.9659258262890683122, 1.000000000000000000, 0.9659258262890683122, 1.000000000000000000, 0.9659258262890683122, 1.000000000000000000, 0.9659258262890683122, 1.000000000000000000, 0.9659258262890683122, 1.000000000000000000, 0.9659258262890683122, 1.000000000000000000, 0.9659258262890683122, 1.000000000000000000, 0.9659258262890683122, 1.000000000000000000, 0.9659258262890683122, 1.000000000000000000, 0.9659258262890683122, 1.000000000000000000, 0.9659258262890683122, 1.000000000000000000, 0.9659258262890683122, 1.000000000000000000, 0.9659258262890683122, 1.000000000000000000, 0.9659258262890683122, 1.000000000000000000, 0.9659258262890683122, 1.000000000000000000, 0.9659258262890683122, 1.000000000000000000, 0.9659258262890683122, 1.000000000000000000, 0.9659258262890683122, 1.000000000000000000, 0.9659258262890683122, 1.000000000000000000, 0.9659258262890683122, 1.000000000000000000, 0.9659258262890683122, 1.000000000000000000, 0.9659258262890683122, 1.000000000000000000, 0.9659258262890683122, 1.000000000000000000, 0.9659258262890683122, 1.000000000000000000, 0.9659258262890683122, 1.000000000000000000, 0.9659258262890683122, 1.000000000000000000, 0.9659258262890683122, 1.000000000000000000, 0.9659258262890683122, 1.000000000000000000, 0.9659258262890683122, 1.000000000000000000, 0.9659258262890683122, 1.000000000000000000, 0.9659258262890683122, 1.000000000000000000, 0.9659258262890683122, 1.000000000000000000, 0.9659258262890683122, 1.000000000000000000, 0.9659258262890683122, 1.000000000000000000, 0.9659258262890683122, 1.000000000000000000, 0.9659258262890683122, 1.000000000000000000, 0.9659258262890683122, 1.000000000000000000, 0.9659258262890683122, 1.000000000000000000, 0.9659258262890683122, 1.000000000000000000, 0.9659258262890683122, 1.000000000000000000, 0.9659258262890683122, 1.000000000000000000, 0.9659258262890683122, 1.000000000000000000, 0.9659258262890683122, 1.000000000000000000, 0.9659258262890683122, 1.000000000000000000, 0.9659258262890683122, 1.000000000000000000, 0.9659258262890683122, 1.000000000000000000, 0.9659258262890683122, 1.000000000000000000, 0.9659258262890683122, 1.000000000000000000, 0.9659258262890683122, 1.000000000000000000, 0.9659258262890683122, 1.000000000000000000, 0.9659258262890683122, 1.000000000000000000, 0.9659258262890683122, 1.000000000000000000, 0.9659258262890683122, 1.000000000000000000, 0.9659258262890683122, 1.000000000000000000, 0.9659258262890683122, 1.000000000000000000, 0.9659258262890683122, 1.000000000000000000, 0.9659258262890683122, 1.000000000000000000, 0.9659258262890683122, 1.000000000000000000, 0.9659258262890683122, 1.000000000000000000, 0.9659258262890683122, 1.000000000000000000, 0.9659258262890683122, 1.000000000000000000, 0.9659258262890683122, 1.000000000000000000, 0.9659258262890683122, 1.000000000000000000, 0.9659258262890683122, 1.000000000000000000, 0.9659258262890683122, 1.000000000000000000, 0.9659258262890683122, 1.000000000000000000, 0.9659258262890683122, 1.000000000000000000, 0.9659258262890683122, 1.000000000000000000, 0.9659258262890683122, 1.000000000000000000, 0.9659258262890683122, 1.000000000000000000, 0.9659258262890683122, 1.000000000000000000, 0.9659258262890683122, 1.000000000000000000, 0.9659258262890683122, 1.000000000000000000, 0.9659258262890683122, 1.000000000000000000, 0.9659258262890683122, 1.000000000000000000, 0.9659258262890683122, 1.000000000000000000, 0.9659258262890683122, 1.000000000000000000, 0.9659258262890683122, 1.000000000000000000, 0.9659258262890683122, 1.000000000000000000, 0.9659258262890683122, 1.000000000000000000, 0.9659258262890683122, 1.000000000000000000, 0.9659258262890683122, 1.000000000000000000, 0.9659258262890683122, 1.000000000000000000, 0.9659258262890683122, 1.000000000000000000, 0.9659258262890683122, 1.000000000000000000, 0.9659258262890683122, 1.000000000000000000, 0.9659258262890683122, 1.000000000000000000, 0.9659258262890683122, 1.000000000000000000, 0.9659258262890683122, 1.000000000000000000, 0.9659258262890683122, 1.000000000000000000, 0.9659258262890683122, 1.000000000000000000, 0.9659258262890683122, 1.000000000000000000, 0.9659258262890683122, 1.000000000000000000, 0.9659258262890683122, 1.000000000000000000, 0.9659258262890683122, 1.000000000000000000, 0.9659258262890683122, 1.000000000000000000, 0.9659258262890683122, 1.000000000000000000, 0.9659258262890683122, 1.000000000000000000, 0.9659258262890683122, 1.000000000000000000, 0.9659258262890683122, 1.000000000000000000, 0.9659258262890683122, 1.000000000000000000, 0.9659258262890683122, 1.000000000000000000, 0.9659258262890683122, 1.000000000000000000, 0.9659258262890683122, 1.000000000000000000, 0.9659258262890683122, 1.000000000000000000, 0.9659258262890683122, 1.000000000000000000, 0.9659258262890683122, 1.000000000000000000, 0.9659258262890683122, 1.000000000000000000, 0.9659258262890683122, 1.000000000000000000, 0.9659258262890683122, 1.000000000000000000, 0.9659258262890683122, 1.000000000000000000, 0.9659258262890683122, 1.000000000000000000, 0.9659258262890683122, 1.000000000000000000, 0.9659258262890683122, 1.000000000000000000, 0.9659258262890683122, 1.000000000000000000, 0.9659258262890683122, 1.000000000000000000, 0.9659258262890683122, 1.000000000000000000, 0.9659258262890683122, 1.000000000000000000, 0.9659258262890683122, 1.000000000000000000, 0.9659258262890683122, 1.000000000000000000, 0.9659258262890683122, 1.000000000000000000, 0.9659258262890683122, 1.000000000000000000, 0.9659258262890683122, 1.000000000000000000, 0.9659258262890683122, 1.000000000000000000, 0.9659258262890683122, 1.000000000000000000, 0.9659258262890683122, 1.000000000000000000, 0.9659258262890683122, 1.000000000000000000, 0.9659258262890683122, 1.000000000000000000, 0.9659258262890683122, 1.000000000000000000, 0.9659258262890683122, 1.000000000000000000, 0.9659258262890683122, 1.000000000000000000, 0.9659258262890683122, 1.000000000000000000, 0.9659258262890683122, 1.000000000000000000, 0.9659258262890683122, 1.000000000000000000, 0.9659258262890683122, 1.000000000000000000, 0.9659258262890683122, 1.000000000000000000, 0.9659258262890683122, 1.000000000000000000, 0.9659258262890683122, 1.000000000000000000, 0.9659258262890683122, 1.000000000000000000, 0.9659258262890683122, 1.000000000000000000, 0.9659258262890683122, 1.000000000000000000, 0.9659258262890683122, 1.000000000000000000, 0.9659258262890683122, 1.000000000000000000, 0.9659258262890683122, 1.000000000000000000, 0.9659258262890683122, 1.000000000000000000, 0.9659258262890683122, 1.000000000000000000, 0.9659258262890683122, 1.000000000000000000, 0.9659258262890683122, 1.000000000000000000, 0.9659258262890683122, 1.000000000000000000, 0.9659258262890683122, 1.000000000000000000, 0.9659258262890683122, 1.000000000000000000, 0.9659258262890683122, 1.000000000000000000, 0.9659258262890683122, 1.000000000000000000, 0.9659258262890683122, 1.000000000000000000, 0.9659258262890683122, 1.000000000000000000, 0.9659258262890683122, 1.000000000000000000, 0.9659258262890683122, 1.000000000000000000, 0.9659258262890683122, 1.000000000000000000, 0.9659258262890683122, 1.000000000000000000, 0.9659258262890683122, 1.000000000000000000, 0.9659258262890683122, 1.000000000000000000, 0.9659258262890683122, 1.000000000000000000, 0.9659258262890683122, 1.000000000000000000, 0.9659258262890683122, 1.000000000000000000, 0.9659258262890683122, 1.000000000000000000, 0.9659258262890683122, 1.000000000000000000, 0.9659258262890683122, 1.000000000000000000, 0.9659258262890683122, 1.000000000000000000, 0.9659258262890683122, 1.000000000000000000, 0.9659258262890683122, 1.000000000000000000, 0.9659258262890683122, 1.000000000000000000, 0.9659258262890683122, 1.000000000000000000, 0.9659258262890683122, 1.000000000000000000, 0.9659258262890683122, 1.000000000000000000, 0.9659258262890683122, 1.000000000000000000, 0.9659258262890683122, 1.000000000000000000, 0.9659258262890683122, 1.000000000000000000, 0.9659258262890683122, 1.000000000000000000, 0.9659258262890683122, 1.000000000000000000, 0.9659258262890683122, 1.000000000000000000, 0.9659258262890683122, 1.000000000000000000, 0.9659258262890683122, 1.000000000000000000, 0.9659258262890683122, 1.000000000000000000, 0.9659258262890683122, 1.000000000000000000, 0.9659258262890683122, 1.000000000000000000, 0.9659258262890683122, 1.000000000000000000, 0.9659258262890683122, 1.000000000000000000, 0.9659258262890683122, 1.000000000000000000, 0.9659258262890683122, 1.000000000000000000, 0.9659258262890683122, 1.000000000000000000, 0.9659258262890683122, 1.000000000000000000, 0.9659258262890683122, 1.000000000000000000, 0.9659258262890683122, 1.000000000000000000, 0.9659258262890683122, 1.000000000000000000, 0.9659258262890683122, 1.000000000000000000, 0.9659258262890683122, 1.000000000000000000, 0.9659258262890683122, 1.000000000000000000, 0.9659258262890683122, 1.000000000000000000, 0.9659258262890683122, 1.000000000000000000, 0.9659258262890683122, 1.000000000000000000, 0.9659258262890683122, 1.000000000000000000, 0.9659258262890683122, 1.000000000000000000, 0.9659258262890683122, 1.000000000000000000, 0.9659258262890683122, 1.000000000000000000) ) ) 
 REPRESENTATION_ITEM ( '' )  SURFACE ( )  );
#56284 = CARTESIAN_POINT ( 'NONE',  ( -0.3392501089628019995, 0.1958661417322832277, -0.9632545931758529356 ) ) ;
#56285 = CARTESIAN_POINT ( 'NONE',  ( -0.5774278215223089816, -0.5023911411419708095, 0.1820866141732285504 ) ) ;
#56286 = ORIENTED_EDGE ( 'NONE', *, *, #27922, .F. ) ;
#56287 = CARTESIAN_POINT ( 'NONE',  ( -9.674558042662121740E-17, 0.3949938075777409963, -1.417322834645669216 ) ) ;
#56288 = ORIENTED_EDGE ( 'NONE', *, *, #41957, .T. ) ;
#56289 = CARTESIAN_POINT ( 'NONE',  ( -1.489501312335957062, -0.2845877964562161244, -0.3641732283464567121 ) ) ;
#56290 = CARTESIAN_POINT ( 'NONE',  ( -1.095800524934382292, -0.3162353388693409650, -0.4822834645669289433 ) ) ;
#56291 = CARTESIAN_POINT ( 'NONE',  ( -0.8202099737532799750, 0.2952755905511810774, -0.1292274648535930714 ) ) ;
#56292 = CARTESIAN_POINT ( 'NONE',  ( 0.3996062992125986590, -0.1070741851644053111, 0.04593175853018371946 ) ) ;
#56293 = CARTESIAN_POINT ( 'NONE',  ( -0.6824146981627291497, -0.6046776061558809534, -0.2411417322834644161 ) ) ;
#56294 = CARTESIAN_POINT ( 'NONE',  ( -0.8070866141732276899, -0.5400638737290844871, 0.3530559997133364547 ) ) ;
#56295 = DIRECTION ( 'NONE',  ( 0.000000000000000000, 0.000000000000000000, 1.000000000000000000 ) ) ;
#56296 = CARTESIAN_POINT ( 'NONE',  ( -0.4614843117558885544, 1.648562443335530370, -3.909868781823469419 ) ) ;
#56297 = CARTESIAN_POINT ( 'NONE',  ( 0.5380577427821529035, -0.3690944881889763329, 0.3153832671262228327 ) ) ;
#56298 = CARTESIAN_POINT ( 'NONE',  ( -1.736178228450298011, 1.299212598425196985, 0.4102808022082834460 ) ) ;
#56299 = CARTESIAN_POINT ( 'NONE',  ( -0.1049643490035302024, -0.3917322834645671215, 0.1581364829396324501 ) ) ;
#56300 = CARTESIAN_POINT ( 'NONE',  ( 0.2099737532808405305, 0.1283753931104746893, -0.1820866141732285504 ) ) ;
#56301 = CARTESIAN_POINT ( 'NONE',  ( -0.3346456692913377662, 0.1660481256975883668, -0.3530559997133364547 ) ) ;
#56302 = CARTESIAN_POINT ( 'NONE',  ( 1.574803149606299746, -0.1870078740157479769, 0.4822834645669291653 ) ) ;
#56303 = CARTESIAN_POINT ( 'NONE',  ( -0.1640419947506553400, -0.05778040916215560624, -0.4822834645669293319 ) ) ;
#56304 = ORIENTED_EDGE ( 'NONE', *, *, #69071, .F. ) ;
#56305 = CARTESIAN_POINT ( 'NONE',  ( -0.3996062992125986035, -0.1070741851644056997, -1.935695538057742526 ) ) ;
#56306 = CARTESIAN_POINT ( 'NONE',  ( 0.2481535038101765900, 6.903518153045088239E-16, 0.3627989612356144478 ) ) ;
#56307 = ORIENTED_EDGE ( 'NONE', *, *, #51203, .T. ) ;
#56308 = CARTESIAN_POINT ( 'NONE',  ( -0.1070741851644056997, 0.3996062992125984925, -1.658136482939632117 ) ) ;
#56309 = DIRECTION ( 'NONE',  ( 0.000000000000000000, -1.000000000000000000, 1.408710688920637755E-15 ) ) ;
#56310 = CARTESIAN_POINT ( 'NONE',  ( -1.246719160104986512, -0.004921259842519576551, 0.3153832671262227771 ) ) ;
#56311 = CARTESIAN_POINT ( 'NONE',  ( -1.062992125984250968, 0.2952755905511811885, 0.000000000000000000 ) ) ;
#56312 = CARTESIAN_POINT ( 'NONE',  ( -0.4724409448818895907, -0.1265901696524993070, -0.3608923884514435576 ) ) ;
#56313 = CARTESIAN_POINT ( 'NONE',  ( -1.614173228346456712, 2.401574803149606474, 0.1372047244094477536 ) ) ;
#56314 = CARTESIAN_POINT ( 'NONE',  ( -0.3917322834645670104, -7.196005306013484475E-17, 0.1259842519685039908 ) ) ;
#56315 = CARTESIAN_POINT ( 'NONE',  ( 1.364829396325460076, 0.2306618581243848609, 0.2411417322834645549 ) ) ;
#56316 = CARTESIAN_POINT ( 'NONE',  ( 0.5643044619422579178, -0.4281496062992127816, -0.4176697321401328100 ) ) ;
#56317 = CARTESIAN_POINT ( 'NONE',  ( 0.3608923884514443348, -0.6692913385826771977, 0.1292274648535927661 ) ) ;
#56318 = CARTESIAN_POINT ( 'NONE',  ( -1.128608923884513837, 0.1283753931104746893, -0.1820866141732285504 ) ) ;
#56319 = CARTESIAN_POINT ( 'NONE',  ( -0.5380577427821514602, -0.4281496062992127816, -0.4176697321401328100 ) ) ;
#56320 = CARTESIAN_POINT ( 'NONE',  ( 0.4091458600556404646, -0.2362204724409448231, -2.543963254593176071 ) ) ;
#56321 = CARTESIAN_POINT ( 'NONE',  ( -0.8005249343832013809, -0.4281496062992124485, 0.4176697321401328655 ) ) ;
#56322 = CARTESIAN_POINT ( 'NONE',  ( -0.2891555358219911054, 0.2891555358219909388, -2.301181102362205078 ) ) ;
#56323 = CARTESIAN_POINT ( 'NONE',  ( 1.476377952755906220, 0.07958543189024071263, -0.2665933059059888421 ) ) ;
#56324 = CARTESIAN_POINT ( 'NONE',  ( -0.5183727034120726440, -0.5511811023622048555, -0.09757992244046775898 ) ) ;
#56325 = CARTESIAN_POINT ( 'NONE',  ( 1.377952755905512472, 0.1771653543307087630, 0.000000000000000000 ) ) ;
#56326 = CARTESIAN_POINT ( 'NONE',  ( -1.450131233595799651, -0.6692913385826771977, 0.1292274648535927661 ) ) ;
#56327 = CARTESIAN_POINT ( 'NONE',  ( -0.9842519685039360366, 0.1771653543307087630, 0.000000000000000000 ) ) ;
#56328 = CARTESIAN_POINT ( 'NONE',  ( -0.3458507752293906723, -0.3458507752293910609, -2.183070866141731958 ) ) ;
#56329 = CARTESIAN_POINT ( 'NONE',  ( 0.5839895013123367340, 0.1771653543307087630, 0.09757992244046791164 ) ) ;
#56330 = CARTESIAN_POINT ( 'NONE',  ( -0.3477690288713902178, 0.2952755905511810774, -0.1292274648535930714 ) ) ;
#56331 = CARTESIAN_POINT ( 'NONE',  ( 0.5314960629920989499, 2.755905511811024056, 2.583694225513486042 ) ) ;
#56332 = CARTESIAN_POINT ( 'NONE',  ( 0.1049868766404206816, 0.1283753931104748280, 0.1820866141732283561 ) ) ;
#56333 = DIRECTION ( 'NONE',  ( -0.000000000000000000, -0.000000000000000000, 1.000000000000000000 ) ) ;
#56334 = CARTESIAN_POINT ( 'NONE',  ( 0.6430446194225729606, -0.4281496062992127816, -0.4176697321401328100 ) ) ;
#56335 = FACE_OUTER_BOUND ( 'NONE', #10858, .T. ) ;
#56336 = CARTESIAN_POINT ( 'NONE',  ( 1.476377952755906220, 0.07958543189024071263, -0.2665933059059888421 ) ) ;
#56337 = CARTESIAN_POINT ( 'NONE',  ( -1.141732283464566011, -0.6692913385826771977, 8.415575281601705876E-17 ) ) ;
#56338 = CARTESIAN_POINT ( 'NONE',  ( -0.2559055118110227234, -0.4536011799217367080, 0.2665933059059888421 ) ) ;
#56339 = DIRECTION ( 'NONE',  ( 3.096699300667737957E-16, -1.000000000000000000, 0.000000000000000000 ) ) ;
#56340 = CARTESIAN_POINT ( 'NONE',  ( 0.1968503937007881344, 0.1771653543307087630, 0.000000000000000000 ) ) ;
#56341 = CARTESIAN_POINT ( 'NONE',  ( -1.345144356955379816, -0.05778040916215560624, -0.4822834645669293319 ) ) ;
#56342 = CARTESIAN_POINT ( 'NONE',  ( -0.3215223097112853146, -0.05778040916215560624, -0.4822834645669293319 ) ) ;
#56343 = CARTESIAN_POINT ( 'NONE',  ( -0.1070741851644051862, -0.3996062992125986590, -0.7788713910761155823 ) ) ;
#56344 = CARTESIAN_POINT ( 'NONE',  ( 0.2867679344610365999, 0.2867679344610365999, -2.112204724409449064 ) ) ;
#56345 = CARTESIAN_POINT ( 'NONE',  ( 0.4396325459317590445, -0.5511811023622046335, 0.09757992244046803654 ) ) ;
#56346 = CARTESIAN_POINT ( 'NONE',  ( -0.5314960629921250401, 0.1660481256975885056, 0.3530559997133364547 ) ) ;
#56347 = CARTESIAN_POINT ( 'NONE',  ( -0.5971128608923877978, -0.6692913385826773087, -0.1292274648535924053 ) ) ;
#56348 = CARTESIAN_POINT ( 'NONE',  ( -0.6627296587926501115, 0.1771653543307087075, -0.09757992244046823083 ) ) ;
#56349 = DIRECTION ( 'NONE',  ( -0.5653208194167064216, -0.6006868920394703437, -0.5653208194167143041 ) ) ;
#56350 = CARTESIAN_POINT ( 'NONE',  ( 0.1509186351706045259, -0.05778040916215560624, -0.4822834645669293319 ) ) ;
#56351 = AXIS2_PLACEMENT_3D ( 'NONE', #59834, #66580, #21539 ) ;
#56352 = EDGE_CURVE ( 'NONE', #9951, #10674, #52154, .T. ) ;
#56353 = CARTESIAN_POINT ( 'NONE',  ( -1.135170603674539924, -0.5511811023622046335, 0.09757992244046803654 ) ) ;
#56354 = CARTESIAN_POINT ( 'NONE',  ( -1.627296587926508442, 0.2306618581243848609, 0.2411417322834645549 ) ) ;
#56355 = CARTESIAN_POINT ( 'NONE',  ( 0.4606732211678801203, 1.929133858267716439, -0.5309055118110237448 ) ) ;
#56356 = ORIENTED_EDGE ( 'NONE', *, *, #71970, .F. ) ;
#56357 = EDGE_CURVE ( 'NONE', #55363, #13254, #16847, .T. ) ;
#56358 = CARTESIAN_POINT ( 'NONE',  ( -1.456692913385826182, -0.5511811023622047445, 6.969142054262312111E-17 ) ) ;
#56359 = CARTESIAN_POINT ( 'NONE',  ( -1.213910761154854745, 0.2952755905511810774, -0.1292274648535930714 ) ) ;
#56360 = CARTESIAN_POINT ( 'NONE',  ( -1.003937007874015297, -0.5400638737290845981, -0.3530559997133363437 ) ) ;
#56361 = CARTESIAN_POINT ( 'NONE',  ( -1.601049868766403650, 0.2306618581243847221, -0.2411417322834647770 ) ) ;
#56362 = CARTESIAN_POINT ( 'NONE',  ( -0.1958661417322836718, 0.3392501089628017219, -1.357611548556430625 ) ) ;
#56363 = CARTESIAN_POINT ( 'NONE',  ( -0.09865214182458049985, 0.3796925558546804247, -1.220472440944881498 ) ) ;
#56364 = CARTESIAN_POINT ( 'NONE',  ( 1.003937007874016407, -0.5400638737290844871, 0.3530559997133364547 ) ) ;
#56365 = CARTESIAN_POINT ( 'NONE',  ( 0.4724409448818904789, -0.1870078740157480879, -0.4822834645669291653 ) ) ;
#56366 = CARTESIAN_POINT ( 'NONE',  ( 0.3458507752293908943, 0.3458507752293908943, -0.4527559055118110520 ) ) ;
#56367 = CARTESIAN_POINT ( 'NONE',  ( 0.2925321140481931814, -0.2925321140481931259, -2.537401574803149984 ) ) ;
#56368 = CARTESIAN_POINT ( 'NONE',  ( 1.266404199475066328, -0.08942795157527998196, 0.3641732283464567121 ) ) ;
#56369 = CARTESIAN_POINT ( 'NONE',  ( 0.3996062992125986035, 2.446882876249141962E-17, -0.7480314960629921295 ) ) ;
#56370 = EDGE_LOOP ( 'NONE', ( #35397, #44047, #51394, #27943 ) ) ;
#56371 = CARTESIAN_POINT ( 'NONE',  ( -0.9186351706036736120, -0.5023911411419708095, -0.1820866141732282451 ) ) ;
#56372 = CARTESIAN_POINT ( 'NONE',  ( 0.3392501089628018884, -0.1958661417322834220, -2.616797900262466836 ) ) ;
#56373 = ORIENTED_EDGE ( 'NONE', *, *, #6822, .T. ) ;
#56374 = CARTESIAN_POINT ( 'NONE',  ( 0.5314960629921264834, 0.1660481256975883668, -0.3530559997133364547 ) ) ;
#56375 = CARTESIAN_POINT ( 'NONE',  ( -0.6167979002624665030, 0.05413385826771666132, 0.4176697321401328100 ) ) ;
#56376 = CARTESIAN_POINT ( 'NONE',  ( -1.023622047244093558, -0.1870078740157479769, 0.4822834645669291653 ) ) ;
#56377 = CARTESIAN_POINT ( 'NONE',  ( 1.128608923884515169, -0.6046776061558809534, -0.2411417322834644161 ) ) ;
#56378 = CARTESIAN_POINT ( 'NONE',  ( 1.568241469816273659, -0.05778040916215560624, -0.4822834645669293319 ) ) ;
#56379 = CARTESIAN_POINT ( 'NONE',  ( 0.09067318884954675418, 5.832582624164717122E-16, 0.3627989612356145588 ) ) ;
#56380 = CARTESIAN_POINT ( 'NONE',  ( -0.2165354330708654795, 0.1660481256975885056, 0.3530559997133364547 ) ) ;
#56381 = CARTESIAN_POINT ( 'NONE',  ( -1.082677165354329896, -0.5400638737290845981, -0.3530559997133363437 ) ) ;
#56382 = CARTESIAN_POINT ( 'NONE',  ( -1.535433070866141225, -0.6692913385826771977, 8.415575281601705876E-17 ) ) ;
#56383 = CARTESIAN_POINT ( 'NONE',  ( 1.437007874015748810, -0.5400638737290845981, -0.3530559997133363437 ) ) ;
#56384 = CARTESIAN_POINT ( 'NONE',  ( -0.1049643490035302024, -0.3917322834645671215, -2.676509186351705871 ) ) ;
#56385 = CARTESIAN_POINT ( 'NONE',  ( 0.9580052493438327987, -0.3690944881889765550, -0.3153832671262227771 ) ) ;
#56386 = VERTEX_POINT ( 'NONE', #74757 ) ;
#56387 = CARTESIAN_POINT ( 'NONE',  ( -0.1058382717557503211, 0.3949938075777409408, -0.3215223097112862027 ) ) ;
#56388 = ORIENTED_EDGE ( 'NONE', *, *, #63677, .T. ) ;
#56389 = CARTESIAN_POINT ( 'NONE',  ( 0.09842519685039434474, -0.4536011799217368745, -0.2665933059059886201 ) ) ;
#56390 = CARTESIAN_POINT ( 'NONE',  ( -1.574803149606298636, -0.1870078740157479769, 0.4822834645669291653 ) ) ;
#56391 = CARTESIAN_POINT ( 'NONE',  ( 0.5839895013123367340, -0.6692913385826773087, -0.1292274648535924053 ) ) ;
#56392 = CARTESIAN_POINT ( 'NONE',  ( 0.5052493438320215802, 0.2952755905511811885, 0.1292274648535926551 ) ) ;
#56393 = CARTESIAN_POINT ( 'NONE',  ( -0.5971128608923877978, 0.2952755905511811885, 0.1292274648535926551 ) ) ;
#56394 = EDGE_CURVE ( 'NONE', #51414, #64697, #61156, .T. ) ;
#56395 = CARTESIAN_POINT ( 'NONE',  ( 0.3917322834645670659, 2.398668435337828261E-17, -1.689651861713597603 ) ) ;
#56396 = CARTESIAN_POINT ( 'NONE',  ( -1.082677165354329896, -0.5400638737290845981, -0.3530559997133363437 ) ) ;
#56397 = CARTESIAN_POINT ( 'NONE',  ( -9.594673741351313045E-17, 0.3917322834645670104, -2.446850393700787496 ) ) ;
#56398 = CARTESIAN_POINT ( 'NONE',  ( 1.299212598425197429, 0.1771653543307087630, 0.000000000000000000 ) ) ;
#56399 = CARTESIAN_POINT ( 'NONE',  ( -1.233595800524933894, -0.6046776061558809534, -0.2411417322834644161 ) ) ;
#56400 = CARTESIAN_POINT ( 'NONE',  ( 1.056430446194226658, 0.2952755905511811885, 0.1292274648535926551 ) ) ;
#56401 = CARTESIAN_POINT ( 'NONE',  ( 1.259842519685040019, -0.1870078740157480879, -0.4822834645669291653 ) ) ;
#56402 = CARTESIAN_POINT ( 'NONE',  ( -0.3460692066303960868, 0.1998031496062990242, -0.9711286089238845287 ) ) ;
#56403 = CARTESIAN_POINT ( 'NONE',  ( -1.430446194225721390, -0.4281496062992124485, 0.4176697321401328655 ) ) ;
#56404 = CARTESIAN_POINT ( 'NONE',  ( -0.3460692066303957537, -0.1998031496062994405, -0.1292650918635170620 ) ) ;
#56405 = CARTESIAN_POINT ( 'NONE',  ( 0.4921259842519691285, 0.1660481256975885056, 0.3530559997133364547 ) ) ;
#56406 = CARTESIAN_POINT ( 'NONE',  ( 0.1070741851644053527, 0.3996062992125986590, -2.198162729658792447 ) ) ;
#56407 = CARTESIAN_POINT ( 'NONE',  ( -0.1049643490035307020, 0.3917322834645669549, -1.823490813648294129 ) ) ;
#56408 = CARTESIAN_POINT ( 'NONE',  ( 1.673228346456693494, 0.1660481256975885056, 0.3530559997133364547 ) ) ;
#56409 = CARTESIAN_POINT ( 'NONE',  ( 0.2427821522309719648, -0.08942795157527998196, 0.3641732283464567121 ) ) ;
#56410 = CARTESIAN_POINT ( 'NONE',  ( 0.7545931758530188826, -0.6692913385826771977, 0.1292274648535927661 ) ) ;
#56411 = CARTESIAN_POINT ( 'NONE',  ( 0.3458507752293908943, -0.3458507752293908943, -0.9625984251968502381 ) ) ;
#56412 = CARTESIAN_POINT ( 'NONE',  ( 0.8923884514435703741, 0.1283753931104748280, 0.1820866141732283561 ) ) ;
#56413 = CARTESIAN_POINT ( 'NONE',  ( 0.4461942257217855201, -0.6046776061558807314, 0.2411417322834647770 ) ) ;
#56414 = CARTESIAN_POINT ( 'NONE',  ( 0.3949938075777409408, -0.1058382717557499186, -0.9757217847769031893 ) ) ;
#56415 = CARTESIAN_POINT ( 'NONE',  ( -0.9251968503937002541, 0.1660481256975885056, 0.3530559997133364547 ) ) ;
#56416 = LINE ( 'NONE', #68649, #41844 ) ;
#56417 = CARTESIAN_POINT ( 'NONE',  ( 1.023622047244095112, -0.1870078740157480601, -0.3641732283464567677 ) ) ;
#56418 = CARTESIAN_POINT ( 'NONE',  ( -1.122047244094487306, 0.1660481256975883391, -0.3530559997133364547 ) ) ;
#56419 = CARTESIAN_POINT ( 'NONE',  ( -0.1574803149606292529, -0.1870078740157479769, 0.4822834645669291653 ) ) ;
#56420 = CARTESIAN_POINT ( 'NONE',  ( 0.1574803149606306130, -0.1870078740157480601, -0.3641732283464567677 ) ) ;
#56421 = CARTESIAN_POINT ( 'NONE',  ( -0.03443470937339728616, 1.062992125984252079, -1.537015892239756099 ) ) ;
#56422 = CARTESIAN_POINT ( 'NONE',  ( -0.3543307086614165824, -0.6692913385826771977, 8.415575281601705876E-17 ) ) ;
#56423 = CARTESIAN_POINT ( 'NONE',  ( 0.6233595800524939223, -0.2845877964562159024, 0.3641732283464567677 ) ) ;
#56424 = CARTESIAN_POINT ( 'NONE',  ( -0.07518215644454619151, 1.068889330503016932, -1.616455086487287529 ) ) ;
#56425 = CARTESIAN_POINT ( 'NONE',  ( -0.3996062992125985480, -7.340648628747423112E-17, -1.690944881889763884 ) ) ;
#56426 = CARTESIAN_POINT ( 'NONE',  ( 0.2230971128608932319, -0.4281496062992124485, 0.4176697321401328655 ) ) ;
#56427 = CARTESIAN_POINT ( 'NONE',  ( 1.128608923884515169, -0.5023911411419708095, -0.1820866141732282451 ) ) ;
#56428 = CARTESIAN_POINT ( 'NONE',  ( -0.3346456692913377662, -0.4536011799217367080, 0.2665933059059888421 ) ) ;
#56429 = CARTESIAN_POINT ( 'NONE',  ( -0.8398950131233589023, -0.5023911411419708095, -0.1820866141732282451 ) ) ;
#56430 = CARTESIAN_POINT ( 'NONE',  ( -0.3215223097112853146, -0.05778040916215560624, -0.4822834645669293319 ) ) ;
#56431 = CARTESIAN_POINT ( 'NONE',  ( 0.5052493438320215802, 0.2952755905511811885, 0.1292274648535926551 ) ) ;
#56432 = CARTESIAN_POINT ( 'NONE',  ( 1.181102362204725198, -0.1870078740157479769, 0.3641732283464567677 ) ) ;
#56433 = CARTESIAN_POINT ( 'NONE',  ( 0.2770644220722718876, 1.151992524107844806, -1.087382630950603613 ) ) ;
#56434 = CARTESIAN_POINT ( 'NONE',  ( 1.509186351706037543, -0.3690944881889765550, -0.3153832671262227771 ) ) ;
#56435 = CARTESIAN_POINT ( 'NONE',  ( 0.8858267716535438430, 0.1660481256975885056, 0.3530559997133364547 ) ) ;
#56436 = DIRECTION ( 'NONE',  ( 0.000000000000000000, 0.000000000000000000, -1.000000000000000000 ) ) ;
#56437 = CARTESIAN_POINT ( 'NONE',  ( 0.01312335958005323398, 0.05413385826771666132, 0.4176697321401328100 ) ) ;
#56438 = CARTESIAN_POINT ( 'NONE',  ( 0.1958661417322834775, 0.3392501089628018884, -1.016404199475065662 ) ) ;
#56439 = CARTESIAN_POINT ( 'NONE',  ( 1.003937007874016407, -0.5400638737290844871, 0.3530559997133364547 ) ) ;
#56440 = CARTESIAN_POINT ( 'NONE',  ( 0.4199475065616805614, 0.2306618581243848609, 0.2411417322834645549 ) ) ;
#56441 = DIRECTION ( 'NONE',  ( 0.000000000000000000, 0.000000000000000000, 1.000000000000000000 ) ) ;
#56442 = CARTESIAN_POINT ( 'NONE',  ( 0.2690288713910767848, 0.1771653543307087630, 0.09757992244046791164 ) ) ;
#56443 = CARTESIAN_POINT ( 'NONE',  ( 1.036745406824147731, 0.05413385826771666132, 0.4176697321401328100 ) ) ;
#56444 = EDGE_CURVE ( 'NONE', #47058, #59607, #62109, .T. ) ;
#56445 = CARTESIAN_POINT ( 'NONE',  ( 0.1443569553805781891, -0.3690944881889763329, 0.3153832671262228327 ) ) ;
#56446 = CARTESIAN_POINT ( 'NONE',  ( -0.4330708661417315697, -0.6692913385826771977, 8.415575281601705876E-17 ) ) ;
#56447 = CARTESIAN_POINT ( 'NONE',  ( 0.5027385518334777093, 1.496062992125983815, -0.5309055118110237448 ) ) ;
#56448 = CARTESIAN_POINT ( 'NONE',  ( 0.1574803149606306130, -0.1870078740157479769, 0.4822834645669291653 ) ) ;
#56449 = CARTESIAN_POINT ( 'NONE',  ( -0.8398950131233585692, 0.2306618581243848609, 0.2411417322834645549 ) ) ;
#56450 = CARTESIAN_POINT ( 'NONE',  ( -0.1574803149606292529, -0.1870078740157479769, 0.3641732283464567677 ) ) ;
#56451 = CARTESIAN_POINT ( 'NONE',  ( 0.4527559055118117182, -0.5400638737290844871, 0.3530559997133364547 ) ) ;
#56453 = CARTESIAN_POINT ( 'NONE',  ( 0.8727034120734913358, -0.08942795157527998196, 0.3641732283464567121 ) ) ;
#56452 = ADVANCED_BREP_SHAPE_REPRESENTATION ( '', ( #6682, #22098 ), #65183 ) ;
#56454 = CARTESIAN_POINT ( 'NONE',  ( -0.2952755905511803003, -0.5400638737290845981, -0.3530559997133363437 ) ) ;
#56455 = LENGTH_MEASURE_WITH_UNIT ( LENGTH_MEASURE( 0.02539999999999999897 ), #12270 );
#56457 = CARTESIAN_POINT ( 'NONE',  ( 0.3996062992125986035, 2.446882876249141962E-17, -1.062992125984252079 ) ) ;
#56456 = CARTESIAN_POINT ( 'NONE',  ( 0.000000000000000000, 0.4177165354330708569, 0.000000000000000000 ) ) ;
#56458 = CARTESIAN_POINT ( 'NONE',  ( 0.1181102362204724116, -0.09842519685039370636, 0.000000000000000000 ) ) ;
#56459 = CARTESIAN_POINT ( 'NONE',  ( -0.2867679344610364334, -0.2867679344610367109, -1.940944881889763884 ) ) ;
#56460 = CARTESIAN_POINT ( 'NONE',  ( -1.135170603674539924, 0.2952755905511810774, -0.1292274648535930714 ) ) ;
#56461 = CARTESIAN_POINT ( 'NONE',  ( -0.9383202099737524282, -0.05778040916215522460, 0.4822834645669289988 ) ) ;
#56462 = CARTESIAN_POINT ( 'NONE',  ( -0.1265901696524986964, -0.4724409448818899238, -0.3871391076115485719 ) ) ;
#56463 = CARTESIAN_POINT ( 'NONE',  ( 0.3949938075777411073, -0.1058382717557499464, -2.788713910761155379 ) ) ;
#56464 = VERTEX_POINT ( 'NONE', #24624 ) ;
#56465 = CARTESIAN_POINT ( 'NONE',  ( 0.2099737532808405305, -0.5023911411419708095, 0.1820866141732285504 ) ) ;
#56466 = CARTESIAN_POINT ( 'NONE',  ( -0.3917322834645670104, -7.196005306013484475E-17, -1.448818897637795367 ) ) ;
#56467 = STYLED_ITEM ( 'NONE', ( #49374 ), #33697 ) ;
#56468 = CARTESIAN_POINT ( 'NONE',  ( 0.8070866141732288002, 0.1660481256975885056, 0.3530559997133364547 ) ) ;
#56469 = CARTESIAN_POINT ( 'NONE',  ( 0.1265901696524989462, 0.4724409448818897572, -2.355643044619422533 ) ) ;
#56470 = CARTESIAN_POINT ( 'NONE',  ( 0.000000000000000000, 0.000000000000000000, -3.444881889763779625 ) ) ;
#56471 = CARTESIAN_POINT ( 'NONE',  ( 1.115485564304462551, -0.4281496062992127816, -0.4176697321401328100 ) ) ;
#56472 = CARTESIAN_POINT ( 'NONE',  ( 1.141732283464567566, 0.1771653543307087630, 0.000000000000000000 ) ) ;
#56473 = CARTESIAN_POINT ( 'NONE',  ( 0.01968503937007957949, -0.5400638737290845981, -0.3530559997133363437 ) ) ;
#56474 = CARTESIAN_POINT ( 'NONE',  ( 0.1958661417322834497, 0.3392501089628018329, -0.5393507629583185192 ) ) ;
#56475 = CARTESIAN_POINT ( 'NONE',  ( -0.5643044619422565855, -0.4281496062992124485, 0.4176697321401328655 ) ) ;
#56476 = CARTESIAN_POINT ( 'NONE',  ( -1.417322834645668772, -0.1870078740157479769, 0.3641732283464567677 ) ) ;
#56477 = CARTESIAN_POINT ( 'NONE',  ( -0.6036745406824141069, 0.2306618581243848609, 0.2411417322834645549 ) ) ;
#56478 = CARTESIAN_POINT ( 'NONE',  ( 2.795275590551181466, 1.968503937007874738, 0.000000000000000000 ) ) ;
#56479 = CARTESIAN_POINT ( 'NONE',  ( -0.1807970329289189937, 1.098498331261037686, -1.883127487649877141 ) ) ;
#56480 = EDGE_LOOP ( 'NONE', ( #45527, #62004, #13446, #27818 ) ) ;
#56481 = CARTESIAN_POINT ( 'NONE',  ( 0.1049643490035304799, -0.3917322834645670104, -2.129284407645356314 ) ) ;
#56482 = CARTESIAN_POINT ( 'NONE',  ( 0.3412073490813655186, -0.6046776061558809534, -0.2411417322834644161 ) ) ;
#56483 = VERTEX_POINT ( 'NONE', #4861 ) ;
#56484 = CARTESIAN_POINT ( 'NONE',  ( -0.4790026246719154557, -0.3162353388693405765, 0.4822834645669290543 ) ) ;
#56485 = CARTESIAN_POINT ( 'NONE',  ( -1.476377952755905110, 0.1660481256975885056, 0.3530559997133364547 ) ) ;
#56486 = B_SPLINE_CURVE_WITH_KNOTS ( 'NONE', 3,
 ( #39080, #44543, #19306, #51274, #44958, #70234, #70654 ),
 .UNSPECIFIED., .F., .F.,
 ( 4, 3, 4 ),
 ( 5.727215236512864700E-17, 0.001246230184515613373, 0.002492489877932691465 ),
 .UNSPECIFIED. ) ;
#56487 = CARTESIAN_POINT ( 'NONE',  ( 0.7874015748031503170, -0.1870078740157479769, 0.4822834645669291653 ) ) ;
#56488 = CARTESIAN_POINT ( 'NONE',  ( -0.07217847769028787330, -0.05778040916215522460, 0.4822834645669289988 ) ) ;
#56489 = CARTESIAN_POINT ( 'NONE',  ( 0.3917322834645670104, -0.1049643490035303411, -1.456036745406824151 ) ) ;
#56490 = CARTESIAN_POINT ( 'NONE',  ( -0.5708661417322828946, 0.1660481256975883668, -0.3530559997133364547 ) ) ;
#56491 = CARTESIAN_POINT ( 'NONE',  ( 0.3608923884514443348, -0.6692913385826771977, 0.1292274648535927661 ) ) ;
#56492 = CARTESIAN_POINT ( 'NONE',  ( -0.3412073490813641308, 0.2306618581243847221, -0.2411417322834647770 ) ) ;
#56493 = CARTESIAN_POINT ( 'NONE',  ( 0.2493438320209980519, -0.004921259842519576551, 0.3153832671262227771 ) ) ;
#56494 = CARTESIAN_POINT ( 'NONE',  ( -0.2407687881342162883, -0.1709459579824098019, 5.655073192166721441 ) ) ;
#56495 = CARTESIAN_POINT ( 'NONE',  ( 0.05905511811023681640, 0.1660481256975883668, -0.3530559997133364547 ) ) ;
#56496 = CARTESIAN_POINT ( 'NONE',  ( 0.000000000000000000, 2.755905511811024056, 0.000000000000000000 ) ) ;
#56497 = CARTESIAN_POINT ( 'NONE',  ( 1.541994750656168645, -0.6692913385826771977, 0.1292274648535927661 ) ) ;
#56498 = CARTESIAN_POINT ( 'NONE',  ( -0.1958661417322834220, -0.3392501089628018884, -2.577427821522309426 ) ) ;
#56499 = ORIENTED_EDGE ( 'NONE', *, *, #34592, .T. ) ;
#56500 = EDGE_LOOP ( 'NONE', ( #43298, #58254, #18324, #23382 ) ) ;
#56501 = CARTESIAN_POINT ( 'NONE',  ( 0.8136482939632553313, -0.6046776061558809534, -0.2411417322834644161 ) ) ;
#56502 = CARTESIAN_POINT ( 'NONE',  ( 5.463695987328526437E-16, -0.1870078740157479769, 0.3641732283464567677 ) ) ;
#56504 = CARTESIAN_POINT ( 'NONE',  ( 5.818687728935708833E-24, 1.062992125984252745, -3.937007874015748143 ) ) ;
#56503 = CYLINDRICAL_SURFACE ( 'NONE', #9516, 0.1771653543307085410 ) ;
#56505 = CARTESIAN_POINT ( 'NONE',  ( 0.3392501089628018884, -0.1958661417322834220, -1.291994750656167978 ) ) ;
#56506 = CARTESIAN_POINT ( 'NONE',  ( -0.7480314960629916854, 2.362204724409448620, 0.000000000000000000 ) ) ;
#56507 = CARTESIAN_POINT ( 'NONE',  ( 0.3937007874015751585, 1.771653543307086354, 0.000000000000000000 ) ) ;
#56508 = CARTESIAN_POINT ( 'NONE',  ( -0.1058382717557497660, -0.3949938075777411073, 0.1660104986876640432 ) ) ;
#56509 = CARTESIAN_POINT ( 'NONE',  ( 0.5052493438320215802, 0.2952755905511811885, 0.1292274648535926551 ) ) ;
#56510 = CARTESIAN_POINT ( 'NONE',  ( -1.377952755905511140, -0.6692913385826771977, 8.415575281601705876E-17 ) ) ;
#56511 = CARTESIAN_POINT ( 'NONE',  ( -1.161417322834644716, -0.5400638737290845981, -0.3530559997133363437 ) ) ;
#56512 = CARTESIAN_POINT ( 'NONE',  ( 0.05905511811023681640, 0.1660481256975883668, -0.3530559997133364547 ) ) ;
#56513 = CARTESIAN_POINT ( 'NONE',  ( 1.036745406824147508, -0.4281496062992127816, -0.4176697321401328100 ) ) ;
#56514 = CARTESIAN_POINT ( 'NONE',  ( 1.207349081364829990, 0.1283753931104748280, 0.1820866141732283561 ) ) ;
#56515 = CARTESIAN_POINT ( 'NONE',  ( 1.253280839895013710, -0.08942795157528024563, -0.3641732283464568787 ) ) ;
#56516 = CARTESIAN_POINT ( 'NONE',  ( -0.7677165354330699465, -0.5400638737290845981, -0.3530559997133363437 ) ) ;
#56517 = CARTESIAN_POINT ( 'NONE',  ( -0.3460692066303960313, 0.1998031496062989965, -0.4179790026246719137 ) ) ;
#56518 = CARTESIAN_POINT ( 'NONE',  ( -1.620734908136482577, 0.1771653543307087630, 0.09757992244046791164 ) ) ;
#56519 =( BOUNDED_CURVE ( )  B_SPLINE_CURVE ( 2, ( #57848, #81910, #18341, #214, #64187, #24222, #32191, #43568, #37677, #69269, #25450, #6521, #12429 ),
 .UNSPECIFIED., .F., .F. ) 
 B_SPLINE_CURVE_WITH_KNOTS ( ( 3, 2, 2, 2, 2, 2, 3 ),
 ( 0.8103969023887780398, 0.8106060606060605522, 0.8143939393939394478, 0.8181818181818182323, 0.8219696969696970168, 0.8257575757575758013, 0.8259667339748583137 ),
 .UNSPECIFIED. ) 
 CURVE ( )  GEOMETRIC_REPRESENTATION_ITEM ( )  RATIONAL_B_SPLINE_CURVE ( ( 0.9964447847208419695, 0.9981185001348091834, 1.000000000000000000, 0.9659258262890683122, 1.000000000000000000, 0.9659258262890683122, 1.000000000000000000, 0.9659258262890683122, 1.000000000000000000, 0.9659258262890683122, 1.000000000000000000, 0.9981185001348091834, 0.9964447847208420805 ) ) 
 REPRESENTATION_ITEM ( '' )  );
#56520 = CARTESIAN_POINT ( 'NONE',  ( -0.3917322834645671215, 0.1049643490035301469, -0.1824146981627296216 ) ) ;
#56521 = CARTESIAN_POINT ( 'NONE',  ( -0.4461942257217840213, -0.6046776061558809534, -0.2411417322834644161 ) ) ;
#56523 = CARTESIAN_POINT ( 'NONE',  ( -0.4476898780827052726, 1.379730629998461522, 2.113977306180467863 ) ) ;
#56522 = CARTESIAN_POINT ( 'NONE',  ( 1.010498687664042716, -0.4281496062992124485, 0.4176697321401328655 ) ) ;
#56524 = CARTESIAN_POINT ( 'NONE',  ( -1.601049868766403650, -0.5023911411419708095, 0.1820866141732285504 ) ) ;
#56525 = CARTESIAN_POINT ( 'NONE',  ( 0.4986876640419954376, -0.6046776061558809534, -0.2411417322834644161 ) ) ;
#56526 = CARTESIAN_POINT ( 'NONE',  ( 0.7742782152230978099, -0.3690944881889763329, 0.3153832671262228327 ) ) ;
#56527 = CARTESIAN_POINT ( 'NONE',  ( -1.528871391076114250, 0.1771653543307087075, -0.09757992244046823083 ) ) ;
#56528 = CARTESIAN_POINT ( 'NONE',  ( 0.9711286089238851948, -0.6046776061558809534, -0.2411417322834644161 ) ) ;
#56529 = CARTESIAN_POINT ( 'NONE',  ( -1.171093442848938793, -2.191421614605370878E-15, 0.4445507791589071167 ) ) ;
#56530 = CARTESIAN_POINT ( 'NONE',  ( -0.5577427821522301654, -0.08942795157528024563, -0.3641732283464568787 ) ) ;
#56531 = CARTESIAN_POINT ( 'NONE',  ( -0.4986876640419942164, -0.6046776061558807314, 0.2411417322834647770 ) ) ;
#56532 = CARTESIAN_POINT ( 'NONE',  ( 1.692913385826772421, 0.2952755905511811885, 0.000000000000000000 ) ) ;
#56533 = CARTESIAN_POINT ( 'NONE',  ( -1.266404199475064773, -0.3162353388693405765, 0.4822834645669290543 ) ) ;
#56534 = AXIS2_PLACEMENT_3D ( 'NONE', #53809, #35301, #61795 ) ;
#56535 = CARTESIAN_POINT ( 'NONE',  ( 1.305774278215223960, -0.6692913385826771977, 0.1292274648535927661 ) ) ;
#56536 = CARTESIAN_POINT ( 'NONE',  ( -0.3917322834645670659, -7.196005306013484475E-17, -0.9809904443907629945 ) ) ;
#56537 = CARTESIAN_POINT ( 'NONE',  ( -1.509186351706035767, -0.3690944881889763329, 0.3153832671262228327 ) ) ;
#56538 = ADVANCED_FACE ( 'NONE', ( #42740 ), #30535, .T. ) ;
#56539 = CARTESIAN_POINT ( 'NONE',  ( 1.116858202696501046, 1.075390326517888351, -0.1088746120232600839 ) ) ;
#56540 = CARTESIAN_POINT ( 'NONE',  ( 1.601049868766404982, 0.2306618581243848609, 0.2411417322834645549 ) ) ;
#56541 = CARTESIAN_POINT ( 'NONE',  ( 0.2362204724409449064, 0.4091458600556404646, -1.953412073490813805 ) ) ;
#56542 = CARTESIAN_POINT ( 'NONE',  ( 0.4744094488188839720, 1.537401574803149984, 3.908320185825793658 ) ) ;
#56543 = CARTESIAN_POINT ( 'NONE',  ( -1.332020997375327642, -0.08942795157527998196, 0.3641732283464567121 ) ) ;
#56544 = CARTESIAN_POINT ( 'NONE',  ( -0.9448818897637790704, -0.1870078740157479769, 0.3641732283464567677 ) ) ;
#56545 = CARTESIAN_POINT ( 'NONE',  ( 1.692913385826772421, 0.1771653543307087630, 0.000000000000000000 ) ) ;
#56546 = CARTESIAN_POINT ( 'NONE',  ( -0.4396325459317577122, -0.6692913385826773087, -0.1292274648535924053 ) ) ;
#56547 = CARTESIAN_POINT ( 'NONE',  ( 0.03937007874015833325, -0.5511811023622047445, 6.969142054262312111E-17 ) ) ;
#56548 = CARTESIAN_POINT ( 'NONE',  ( -1.167979002624671470, -0.3690944881889765550, -0.3153832671262227771 ) ) ;
#56549 = CARTESIAN_POINT ( 'NONE',  ( 1.391076115485564868, -0.5023911411419708095, 0.1820866141732285504 ) ) ;
#56550 = CARTESIAN_POINT ( 'NONE',  ( 0.8136482939632553313, -0.6046776061558809534, -0.2411417322834644161 ) ) ;
#56551 = CARTESIAN_POINT ( 'NONE',  ( 1.515748031496063186, -0.5400638737290845981, -0.3530559997133363437 ) ) ;
#56552 = CARTESIAN_POINT ( 'NONE',  ( 0.5643044619422579178, -0.004921259842519576551, 0.3153832671262227771 ) ) ;
#56553 = CARTESIAN_POINT ( 'NONE',  ( 0.4330708661417329575, 0.2952755905511811885, 0.000000000000000000 ) ) ;
#56554 = CONICAL_SURFACE ( 'NONE', #40482, 0.3129921259842520787, 0.7853981633974533860 ) ;
#56555 = CARTESIAN_POINT ( 'NONE',  ( 0.7874015748031503170, -0.1870078740157479769, 0.3641732283464567677 ) ) ;
#56556 = ORIENTED_EDGE ( 'NONE', *, *, #7406, .F. ) ;
#56557 = CARTESIAN_POINT ( 'NONE',  ( -1.135170603674539924, 0.2952755905511810774, -0.1292274648535930714 ) ) ;
#56558 = CARTESIAN_POINT ( 'NONE',  ( -1.279527559055116948, 0.1660481256975883668, -0.3530559997133364547 ) ) ;
#56559 = CARTESIAN_POINT ( 'NONE',  ( -0.1640419947506555343, -0.3162353388693405765, 0.4822834645669290543 ) ) ;
#56560 = LINE ( 'NONE', #81442, #5649 ) ;
#56561 = CARTESIAN_POINT ( 'NONE',  ( 4.893765752498283308E-17, -0.3996062992125985480, -2.517716535433071279 ) ) ;
#56562 = CARTESIAN_POINT ( 'NONE',  ( 0.3543307086614179147, 0.2952755905511811885, 0.000000000000000000 ) ) ;
#56563 = CARTESIAN_POINT ( 'NONE',  ( 1.174540682414699111, -0.08942795157528024563, -0.3641732283464568787 ) ) ;
#56564 = CARTESIAN_POINT ( 'NONE',  ( -0.04593175853018302557, 0.2952755905511811885, 0.1292274648535926551 ) ) ;
#56565 = CARTESIAN_POINT ( 'NONE',  ( 0.2493438320209980519, -0.4281496062992127816, -0.4176697321401328100 ) ) ;
#56566 = CARTESIAN_POINT ( 'NONE',  ( -0.2925321140481932924, 0.2925321140481931814, -2.224409448818897239 ) ) ;
#56567 = CARTESIAN_POINT ( 'NONE',  ( 0.1974969037888706369, -0.3420746716998659953, -1.666666666666666741 ) ) ;
#56568 = CARTESIAN_POINT ( 'NONE',  ( -0.3767879474345934843, 1.247505695433910100, 1.057050330549203832 ) ) ;
#56569 = CARTESIAN_POINT ( 'NONE',  ( 1.141392835773559211, 0.3937007874015748254, 1.141392835773562764 ) ) ;
#56570 = CARTESIAN_POINT ( 'NONE',  ( -0.3392501089628019995, 0.1958661417322832277, -0.4908136482939632339 ) ) ;
#56571 = CARTESIAN_POINT ( 'NONE',  ( -0.6824146981627291497, -0.5023911411419708095, -0.1820866141732282451 ) ) ;
#56572 = CARTESIAN_POINT ( 'NONE',  ( -0.8136482939632537770, -0.6046776061558807314, 0.2411417322834647770 ) ) ;
#56573 = CARTESIAN_POINT ( 'NONE',  ( 0.2559055118110243332, -0.5400638737290845981, -0.3530559997133363437 ) ) ;
#56574 = CARTESIAN_POINT ( 'NONE',  ( -9.674558042662122972E-17, 0.3949938075777409963, -2.438976377952756014 ) ) ;
#56575 = CARTESIAN_POINT ( 'NONE',  ( 0.7677165354330716118, 0.1660481256975883668, -0.3530559997133364547 ) ) ;
#56576 = CARTESIAN_POINT ( 'NONE',  ( -1.541994750656167090, -0.6692913385826773087, -0.1292274648535924053 ) ) ;
#56577 = CARTESIAN_POINT ( 'NONE',  ( 0.7152230971128614723, -0.3162353388693409650, -0.4822834645669289433 ) ) ;
#56578 = CARTESIAN_POINT ( 'NONE',  ( 0.1265901696524989462, 0.4724409448818897572, -2.828083989501312345 ) ) ;
#56579 = CARTESIAN_POINT ( 'NONE',  ( -0.3996062992125987146, 0.1070741851644051862, -2.080052493438320216 ) ) ;
#56580 = CARTESIAN_POINT ( 'NONE',  ( 1.692913385826772421, 0.2952755905511811885, 0.000000000000000000 ) ) ;
#56581 = CARTESIAN_POINT ( 'NONE',  ( 0.9448818897637802916, -0.1870078740157479769, 0.4822834645669291653 ) ) ;
#56582 = CARTESIAN_POINT ( 'NONE',  ( 0.4002624671916016896, -0.3162353388693409650, -0.4822834645669289433 ) ) ;
#56583 = CARTESIAN_POINT ( 'NONE',  ( 1.174540682414699111, -0.08942795157528024563, -0.3641732283464568787 ) ) ;
#56584 = CARTESIAN_POINT ( 'NONE',  ( 1.561679790026247350, 0.05413385826771626580, -0.4176697321401330321 ) ) ;
#56585 = CARTESIAN_POINT ( 'NONE',  ( -0.3917322834645670104, -7.196005306013484475E-17, -0.2814960629921260393 ) ) ;
#56586 = FACE_OUTER_BOUND ( 'NONE', #76572, .T. ) ;
#56587 = CARTESIAN_POINT ( 'NONE',  ( 0.6496062992125991586, -0.5400638737290845981, -0.3530559997133363437 ) ) ;
#56588 = CARTESIAN_POINT ( 'NONE',  ( 1.601049868766404982, -0.5023911411419708095, -0.1820866141732282451 ) ) ;
#56589 = CARTESIAN_POINT ( 'NONE',  ( -0.4396325459317579898, 0.2952755905511811885, 0.1292274648535926551 ) ) ;
#56590 = CARTESIAN_POINT ( 'NONE',  ( -1.036745406824146176, 0.05413385826771626580, -0.4176697321401330321 ) ) ;
#56591 = AXIS2_PLACEMENT_3D ( 'NONE', #77386, #70645, #44949 ) ;
#56592 = CARTESIAN_POINT ( 'NONE',  ( 0.9973753280839902091, 0.2306618581243847221, -0.2411417322834647770 ) ) ;
#56593 = CARTESIAN_POINT ( 'NONE',  ( 0.1049643490035304938, -0.3917322834645669549, -0.6423884514435697080 ) ) ;
#56594 = CARTESIAN_POINT ( 'NONE',  ( -0.2867679344610365999, 0.2867679344610364889, -1.429133858267716661 ) ) ;
#56595 = CARTESIAN_POINT ( 'NONE',  ( 0.1049643490035303689, 0.3917322834645670104, -2.505249343832020248 ) ) ;
#56596 = CARTESIAN_POINT ( 'NONE',  ( -1.463254593175852492, 0.1771653543307087630, 0.09757992244046791164 ) ) ;
#56597 = EDGE_LOOP ( 'NONE', ( #36598, #60939, #21651, #64195, #21684, #78230, #65847, #37152, #19659, #60968, #2469, #81593, #12610, #13360 ) ) ;
#56598 = CARTESIAN_POINT ( 'NONE',  ( -0.1058382717557503211, 0.3949938075777409408, -2.683727034120735766 ) ) ;
#56599 = ORIENTED_EDGE ( 'NONE', *, *, #52769, .T. ) ;
#56600 = CARTESIAN_POINT ( 'NONE',  ( -0.7233831536535468842, 2.232734770847097039, -0.5048085489443572271 ) ) ;
#56601 = CARTESIAN_POINT ( 'NONE',  ( 1.246719160104987623, -0.3690944881889763329, 0.3153832671262228327 ) ) ;
#56602 = CARTESIAN_POINT ( 'NONE',  ( 0.2925321140481932369, 0.2925321140481932369, -1.397637795275590067 ) ) ;
#56603 = CARTESIAN_POINT ( 'NONE',  ( 1.482939632545932307, -0.3690944881889763329, 0.3153832671262228327 ) ) ;
#56604 = CARTESIAN_POINT ( 'NONE',  ( -0.4744094488188832504, 1.537401574803149984, -3.937007874015763687 ) ) ;
#56605 = CARTESIAN_POINT ( 'NONE',  ( -1.013613127888308485, -2.191421614605370878E-15, 0.4445507791589071167 ) ) ;
#56606 = CARTESIAN_POINT ( 'NONE',  ( -0.2003255369053823787, 1.919404900195578856, 0.2409235081687154112 ) ) ;
#56607 = CARTESIAN_POINT ( 'NONE',  ( 0.1958661417322836440, -0.3392501089628017219, -0.3339895013123360679 ) ) ;
#56608 = CARTESIAN_POINT ( 'NONE',  ( -0.6692913385826764205, 0.1771653543307087630, 0.000000000000000000 ) ) ;
#56609 = CARTESIAN_POINT ( 'NONE',  ( -1.135170603674539924, -0.5511811023622046335, 0.09757992244046803654 ) ) ;
#56610 = CARTESIAN_POINT ( 'NONE',  ( -1.259842519685038686, -0.1870078740157480879, -0.4822834645669291653 ) ) ;
#56611 = CARTESIAN_POINT ( 'NONE',  ( 0.06561679790026316017, 0.05413385826771626580, -0.4176697321401330321 ) ) ;
#56612 = CARTESIAN_POINT ( 'NONE',  ( 1.535433070866142335, -0.6692913385826771977, 8.415575281601705876E-17 ) ) ;
#56613 = VERTEX_POINT ( 'NONE', #81900 ) ;
#56614 = CARTESIAN_POINT ( 'NONE',  ( 1.332020997375328974, -0.05778040916215560624, -0.4822834645669293319 ) ) ;
#56615 = CARTESIAN_POINT ( 'NONE',  ( 2.118110236220470899, 0.000000000000000000, 0.4498537592782972383 ) ) ;
#56616 = CARTESIAN_POINT ( 'NONE',  ( 5.700590969322950841, 4.103338224919997224, 5.973313079581529017 ) ) ;
#56617 = CARTESIAN_POINT ( 'NONE',  ( -0.4724409448818898682, -8.678599364036362592E-17, -1.929133858267716439 ) ) ;
#56618 = CARTESIAN_POINT ( 'NONE',  ( 2.170146923806595574, 1.546132656481028933, 0.4744094488188977388 ) ) ;
#56619 = CARTESIAN_POINT ( 'NONE',  ( -0.5183727034120726440, 0.1771653543307087630, 0.09757992244046791164 ) ) ;
#56620 = CARTESIAN_POINT ( 'NONE',  ( -1.102362204724408601, -0.1870078740157480879, -0.4822834645669291653 ) ) ;
#56621 = CARTESIAN_POINT ( 'NONE',  ( 1.102362204724410155, -0.1870078740157480879, -0.4822834645669291653 ) ) ;
#56622 = ORIENTED_EDGE ( 'NONE', *, *, #7244, .T. ) ;
#56624 = CARTESIAN_POINT ( 'NONE',  ( -0.7478466213799878082, 1.968503937007873850, 0.5309055118110236338 ) ) ;
#56623 = CARTESIAN_POINT ( 'NONE',  ( 0.3458507752293908943, -0.3458507752293908943, -2.303149606299212060 ) ) ;
#56625 = CARTESIAN_POINT ( 'NONE',  ( -1.712598425196849572, 0.1660481256975885056, 0.3530559997133364547 ) ) ;
#56626 = CARTESIAN_POINT ( 'NONE',  ( -1.036745406824146176, 0.05413385826771626580, -0.4176697321401330321 ) ) ;
#56627 = CARTESIAN_POINT ( 'NONE',  ( -0.3392501089628019439, 0.1958661417322832554, -0.2637602117772160915 ) ) ;
#56628 = CARTESIAN_POINT ( 'NONE',  ( 0.05249343832021075018, 0.1283753931104746893, -0.1820866141732285504 ) ) ;
#56629 = CARTESIAN_POINT ( 'NONE',  ( 0.2867679344610366554, 0.2867679344610366554, -0.8523622047244096001 ) ) ;
#56630 = CARTESIAN_POINT ( 'NONE',  ( -0.3608923884514428360, 0.1771653543307087630, 0.09757992244046791164 ) ) ;
#56631 = CARTESIAN_POINT ( 'NONE',  ( 0.3543307086614179147, 0.1771653543307087630, 0.000000000000000000 ) ) ;
#56632 = CARTESIAN_POINT ( 'NONE',  ( 0.4396325459317590445, -0.6692913385826771977, 0.1292274648535927661 ) ) ;
#56633 = CARTESIAN_POINT ( 'NONE',  ( -0.6167979002624665030, -0.3690944881889765550, -0.3153832671262227771 ) ) ;
#56634 = CARTESIAN_POINT ( 'NONE',  ( 0.2867679344610365999, -0.2867679344610365444, -2.767716535433069946 ) ) ;
#56635 = CARTESIAN_POINT ( 'NONE',  ( 1.003937007874016185, 0.1660481256975883668, -0.3530559997133364547 ) ) ;
#56636 = CARTESIAN_POINT ( 'NONE',  ( -1.141732283464566011, 0.2952755905511811885, 0.000000000000000000 ) ) ;
#56637 = CARTESIAN_POINT ( 'NONE',  ( -0.2362204724409451284, 0.4091458600556402425, -0.7198162729658792447 ) ) ;
#56638 = CARTESIAN_POINT ( 'NONE',  ( -0.4921259842519677963, -0.5400638737290844871, 0.3530559997133364547 ) ) ;
#56639 = CARTESIAN_POINT ( 'NONE',  ( -0.4199475065616791736, -0.6046776061558807314, 0.2411417322834647770 ) ) ;
#56640 = CARTESIAN_POINT ( 'NONE',  ( 1.325459317585302665, -0.3690944881889763329, 0.3153832671262228327 ) ) ;
#56641 = CARTESIAN_POINT ( 'NONE',  ( 0.1706036745406830368, -0.004921259842519576551, 0.3153832671262227771 ) ) ;
#56642 = CARTESIAN_POINT ( 'NONE',  ( -0.08530183727034056085, -0.05778040916215560624, -0.4822834645669293319 ) ) ;
#56643 = CARTESIAN_POINT ( 'NONE',  ( -0.9842519685039360366, 0.2952755905511811885, 0.000000000000000000 ) ) ;
#56644 = CARTESIAN_POINT ( 'NONE',  ( -1.646051170424378096, 0.000000000000000000, -0.3464511005275205946 ) ) ;
#56645 = CARTESIAN_POINT ( 'NONE',  ( 1.528871391076116026, 0.1771653543307087630, 0.09757992244046791164 ) ) ;
#56646 = CARTESIAN_POINT ( 'NONE',  ( -0.2755905511811015396, -0.6692913385826771977, 8.415575281601705876E-17 ) ) ;
#56647 = CIRCLE ( 'NONE', #41882, 0.1968503937007874405 ) ;
#56648 = CARTESIAN_POINT ( 'NONE',  ( -1.141732283464566011, -0.6692913385826771977, 8.415575281601705876E-17 ) ) ;
#56649 = ORIENTED_EDGE ( 'NONE', *, *, #55727, .T. ) ;
#56650 = CARTESIAN_POINT ( 'NONE',  ( -0.1070741851644056997, 0.3996062992125984925, -1.815616797900262425 ) ) ;
#56651 = CARTESIAN_POINT ( 'NONE',  ( 1.332020997375328974, -0.05778040916215560624, -0.4822834645669293319 ) ) ;
#56652 = CARTESIAN_POINT ( 'NONE',  ( -0.8136482939632537770, -0.5023911411419708095, 0.1820866141732285504 ) ) ;
#56653 = CARTESIAN_POINT ( 'NONE',  ( -0.7283464566929126471, 0.1660481256975883668, -0.3530559997133364547 ) ) ;
#56654 = CARTESIAN_POINT ( 'NONE',  ( 1.194225721784777594, 0.05413385826771666132, 0.4176697321401328100 ) ) ;
#56655 = CARTESIAN_POINT ( 'NONE',  ( 0.9973753280839902091, -0.6046776061558807314, 0.2411417322834647770 ) ) ;
#56656 = CARTESIAN_POINT ( 'NONE',  ( 1.528871391076116026, -0.6692913385826773087, -0.1292274648535924053 ) ) ;
#56657 = CARTESIAN_POINT ( 'NONE',  ( -0.9383202099737524282, -0.08942795157527998196, 0.3641732283464567121 ) ) ;
#56658 = CARTESIAN_POINT ( 'NONE',  ( -0.3460692066303960313, 0.1998031496062989965, -0.7329396325459317518 ) ) ;
#56659 = CARTESIAN_POINT ( 'NONE',  ( -0.1070741851644056997, 0.3996062992125986035, -1.108923884514435798 ) ) ;
#56660 = CARTESIAN_POINT ( 'NONE',  ( 0.3949938075777409963, 2.418639510665530435E-17, -0.2755905511811024278 ) ) ;
#56661 = CARTESIAN_POINT ( 'NONE',  ( 0.2885979965725480323, 1.160566086728936908, 2.785141739107498182 ) ) ;
#56662 = CARTESIAN_POINT ( 'NONE',  ( 0.9645669291338591078, -0.4536011799217368745, -0.2665933059059886201 ) ) ;
#56663 = EDGE_CURVE ( 'NONE', #49469, #80363, #30117, .T. ) ;
#56664 = CARTESIAN_POINT ( 'NONE',  ( 0.7808398950131240079, -0.2845877964562159024, 0.3641732283464567677 ) ) ;
#56665 = CARTESIAN_POINT ( 'NONE',  ( 0.4724409448818904789, -0.1870078740157479769, 0.4822834645669291653 ) ) ;
#56666 = CARTESIAN_POINT ( 'NONE',  ( 1.601049868766404982, 0.2306618581243848609, 0.2411417322834645549 ) ) ;
#56667 = CARTESIAN_POINT ( 'NONE',  ( 0.1974969037888704704, 0.3420746716998660508, -1.480971128608923548 ) ) ;
#56668 = CARTESIAN_POINT ( 'NONE',  ( 0.7611548556430454138, 0.1283753931104746893, -0.1820866141732285504 ) ) ;
#56669 = CARTESIAN_POINT ( 'NONE',  ( -0.1181102362204717315, -0.6692913385826771977, 8.415575281601705876E-17 ) ) ;
#56670 = CARTESIAN_POINT ( 'NONE',  ( -1.213910761154854745, -0.6692913385826771977, 0.1292274648535927661 ) ) ;
#56671 = CARTESIAN_POINT ( 'NONE',  ( 1.345144356955381593, -0.05778040916215522460, 0.4822834645669289988 ) ) ;
#56672 = CARTESIAN_POINT ( 'NONE',  ( -0.3458507752293906723, -0.3458507752293910609, -1.791338582677165059 ) ) ;
#56673 = CARTESIAN_POINT ( 'NONE',  ( 0.000000000000000000, 1.929133858267716661, -2.362204724409448620 ) ) ;
#56674 = CARTESIAN_POINT ( 'NONE',  ( -0.05249343832020938322, -0.5023911411419708095, -0.1820866141732282451 ) ) ;
#56675 = ORIENTED_EDGE ( 'NONE', *, *, #63509, .T. ) ;
#56676 = ORIENTED_EDGE ( 'NONE', *, *, #33628, .T. ) ;
#56677 = CARTESIAN_POINT ( 'NONE',  ( -0.7808398950131225646, -0.05778040916215522460, 0.4822834645669289988 ) ) ;
#56678 = CARTESIAN_POINT ( 'NONE',  ( -0.7545931758530176614, -0.6692913385826773087, -0.1292274648535924053 ) ) ;
#56679 = CARTESIAN_POINT ( 'NONE',  ( -0.3149606299212590610, -0.1870078740157480879, -0.4822834645669291653 ) ) ;
#56680 = DIMENSIONAL_EXPONENTS ( 1.000000000000000000, 0.000000000000000000, 0.000000000000000000, 0.000000000000000000, 0.000000000000000000, 0.000000000000000000, 0.000000000000000000 ) ;
#56681 = CARTESIAN_POINT ( 'NONE',  ( 0.4724409448818904789, -0.1870078740157480879, -0.4822834645669291653 ) ) ;
#56682 = CARTESIAN_POINT ( 'NONE',  ( -0.3346456692913377662, 0.1660481256975883668, -0.3530559997133364547 ) ) ;
#56683 = CARTESIAN_POINT ( 'NONE',  ( -1.128608923884513837, 0.2306618581243847221, -0.2411417322834647770 ) ) ;
#56684 = CARTESIAN_POINT ( 'NONE',  ( -0.7283464566929126471, 0.1660481256975883668, -0.3530559997133364547 ) ) ;
#56685 = CARTESIAN_POINT ( 'NONE',  ( 0.8267716535433077274, 0.2952755905511811885, 0.000000000000000000 ) ) ;
#56686 =( BOUNDED_CURVE ( )  B_SPLINE_CURVE ( 1, ( #49515, #60908 ),
 .UNSPECIFIED., .F., .F. ) 
 B_SPLINE_CURVE_WITH_KNOTS ( ( 2, 2 ),
 ( 0.000000000000000000, 0.002000000000000001776 ),
 .UNSPECIFIED. ) 
 CURVE ( )  GEOMETRIC_REPRESENTATION_ITEM ( )  RATIONAL_B_SPLINE_CURVE ( ( 0.9875488213027530104, 0.9875488213027530104 ) ) 
 REPRESENTATION_ITEM ( '' )  );
#56687 = EDGE_CURVE ( 'NONE', #35211, #41007, #53100, .T. ) ;
#56688 = CARTESIAN_POINT ( 'NONE',  ( 0.3917322834645670104, 2.398668435337828261E-17, -1.370078740157480324 ) ) ;
#56689 = CARTESIAN_POINT ( 'NONE',  ( -0.2624671916010490880, -0.5023911411419708095, 0.1820866141732285504 ) ) ;
#56690 = ORIENTED_EDGE ( 'NONE', *, *, #43363, .F. ) ;
#56691 = CARTESIAN_POINT ( 'NONE',  ( 0.3949938075777411073, -0.1058382717557499464, -1.371391076115485719 ) ) ;
#56692 = ORIENTED_EDGE ( 'NONE', *, *, #59375, .T. ) ;
#56693 = CARTESIAN_POINT ( 'NONE',  ( -1.286089238845143479, -0.5023911411419708095, 0.1820866141732285504 ) ) ;
#56694 = CARTESIAN_POINT ( 'NONE',  ( -0.8923884514435688198, -0.6046776061558807314, 0.2411417322834647770 ) ) ;
#56695 = CARTESIAN_POINT ( 'NONE',  ( -0.9973753280839886548, 0.2306618581243848609, 0.2411417322834645549 ) ) ;
#56696 = CARTESIAN_POINT ( 'NONE',  ( -0.2925321140481930704, -0.2925321140481933480, -0.05905511811023621965 ) ) ;
#56697 = CARTESIAN_POINT ( 'NONE',  ( -0.8858267716535425107, 0.1660481256975883668, -0.3530559997133364547 ) ) ;
#56698 = CARTESIAN_POINT ( 'NONE',  ( -0.9383202099737524282, -0.05778040916215522460, 0.4822834645669289988 ) ) ;
#56699 = CARTESIAN_POINT ( 'NONE',  ( -1.614173228346455824, 0.2952755905511811885, 0.000000000000000000 ) ) ;
#56700 = DIRECTION ( 'NONE',  ( 0.000000000000000000, 0.000000000000000000, -1.000000000000000000 ) ) ;
#56701 = CARTESIAN_POINT ( 'NONE',  ( 0.6233595800524942554, -0.08942795157528024563, -0.3641732283464568787 ) ) ;
#56702 = CARTESIAN_POINT ( 'NONE',  ( 0.4849061582275022153, 1.568468489416427580, 0.4921425059946342717 ) ) ;
#56703 = CARTESIAN_POINT ( 'NONE',  ( 0.3392501089628018884, -0.1958661417322834220, 0.1253280839895012100 ) ) ;
#56704 = CARTESIAN_POINT ( 'NONE',  ( -0.1377952755905504645, 0.07958543189024085140, 0.2665933059059887866 ) ) ;
#56705 = CARTESIAN_POINT ( 'NONE',  ( -0.4658792650918627265, -0.3162353388693409650, -0.4822834645669289433 ) ) ;
#56706 = CARTESIAN_POINT ( 'NONE',  ( 1.482939632545932307, 0.05413385826771626580, -0.4176697321401330321 ) ) ;
#56707 = CARTESIAN_POINT ( 'NONE',  ( 0.01312335958005323398, -0.4281496062992127816, -0.4176697321401328100 ) ) ;
#56708 = ORIENTED_EDGE ( 'NONE', *, *, #3202, .T. ) ;
#56709 = CARTESIAN_POINT ( 'NONE',  ( 0.3996062992125986035, 0.1070741851644054776, -2.014435695538057569 ) ) ;
#56710 = DIRECTION ( 'NONE',  ( 0.000000000000000000, -1.000000000000000000, -0.000000000000000000 ) ) ;
#56711 = EDGE_LOOP ( 'NONE', ( #25615, #50242, #78786, #1330 ) ) ;
#56712 = CARTESIAN_POINT ( 'NONE',  ( -9.787531504996566615E-17, 0.3996062992125985480, -1.651574803149606474 ) ) ;
#56713 = CIRCLE ( 'NONE', #2967, 3.937007874015748143 ) ;
#56714 = CARTESIAN_POINT ( 'NONE',  ( 1.227034120734908917, -0.6692913385826771977, 0.1292274648535927661 ) ) ;
#56716 = EDGE_CURVE ( 'NONE', #74449, #78494, #68436, .T. ) ;
#56715 = CARTESIAN_POINT ( 'NONE',  ( -1.141732283464566011, -0.5511811023622047445, 6.969142054262312111E-17 ) ) ;
#56717 = CARTESIAN_POINT ( 'NONE',  ( -1.351706036745406347, 0.05413385826771626580, -0.4176697321401330321 ) ) ;
#56718 = CARTESIAN_POINT ( 'NONE',  ( -0.4724409448818899238, 0.1265901696524986686, -0.9776902887139107268 ) ) ;
#56719 = CARTESIAN_POINT ( 'NONE',  ( -0.3576100502496167843, 1.224098650525152543, 3.920795739734008301 ) ) ;
#56720 = CARTESIAN_POINT ( 'NONE',  ( -0.1958661417322834220, -0.3392501089628018884, 0.09973753280839900426 ) ) ;
#56721 = CARTESIAN_POINT ( 'NONE',  ( 1.437007874015748810, -0.5400638737290845981, -0.3530559997133363437 ) ) ;
#56722 = CARTESIAN_POINT ( 'NONE',  ( 0.5052493438320215802, 0.2952755905511811885, 0.1292274648535926551 ) ) ;
#56723 = CARTESIAN_POINT ( 'NONE',  ( 0.1902887139107617975, -0.6692913385826773087, -0.1292274648535924053 ) ) ;
#56724 = CARTESIAN_POINT ( 'NONE',  ( -1.266404199475064773, -0.08942795157528024563, -0.3641732283464568787 ) ) ;
#56725 = CARTESIAN_POINT ( 'NONE',  ( -0.4724409448818890911, -0.1870078740157479769, 0.4822834645669291653 ) ) ;
#56726 = CARTESIAN_POINT ( 'NONE',  ( 0.4091458600556404646, -0.2362204724409448231, -2.858923884514435798 ) ) ;
#56727 = CARTESIAN_POINT ( 'NONE',  ( -0.8727034120734901146, -0.05778040916215560624, -0.4822834645669293319 ) ) ;
#56728 = CARTESIAN_POINT ( 'NONE',  ( 0.3949938075777408852, 0.1058382717557500435, -2.248687664041995049 ) ) ;
#56729 = CARTESIAN_POINT ( 'NONE',  ( 1.194225721784777594, -0.3690944881889765550, -0.3153832671262227771 ) ) ;
#56730 = CARTESIAN_POINT ( 'NONE',  ( -0.2755905511811018171, 0.1771653543307087630, 0.000000000000000000 ) ) ;
#56731 = CARTESIAN_POINT ( 'NONE',  ( 1.017060367454068803, -0.2845877964562159024, 0.3641732283464567677 ) ) ;
#56732 = CARTESIAN_POINT ( 'NONE',  ( -1.653543307086613234, -0.1870078740157480879, -0.4822834645669291653 ) ) ;
#56733 = CARTESIAN_POINT ( 'NONE',  ( -1.246719160104985846, -0.3690944881889765550, -0.3153832671262227771 ) ) ;
#56734 = DIRECTION ( 'NONE',  ( 0.000000000000000000, 0.000000000000000000, 1.000000000000000000 ) ) ;
#56735 = CARTESIAN_POINT ( 'NONE',  ( 0.7480314960629927956, 0.1771653543307087630, 0.000000000000000000 ) ) ;
#56736 = CARTESIAN_POINT ( 'NONE',  ( -0.7086614173228339419, -0.1870078740157479769, 0.4822834645669291653 ) ) ;
#56737 = CARTESIAN_POINT ( 'NONE',  ( -2.170146923806674621, 1.528780496884627915, 0.4744094488188969616 ) ) ;
#56738 = CARTESIAN_POINT ( 'NONE',  ( -0.04593175853018302557, 0.1771653543307087630, 0.09757992244046791164 ) ) ;
#56739 = CARTESIAN_POINT ( 'NONE',  ( -1.679790026246718693, 0.1283753931104746893, -0.1820866141732285504 ) ) ;
#56740 = CARTESIAN_POINT ( 'NONE',  ( 0.7874015748031503170, -0.1870078740157480879, -0.4822834645669291653 ) ) ;
#56741 = CARTESIAN_POINT ( 'NONE',  ( 0.6496062992125991586, 0.1660481256975885056, 0.3530559997133364547 ) ) ;
#56742 = CARTESIAN_POINT ( 'NONE',  ( 1.384514435695538337, -0.5511811023622046335, 0.09757992244046803654 ) ) ;
#56743 = CARTESIAN_POINT ( 'NONE',  ( -0.9973753280839886548, -0.6046776061558809534, -0.2411417322834644161 ) ) ;
#56744 = CARTESIAN_POINT ( 'NONE',  ( -0.1837270341207340729, 0.1283753931104746893, -0.1820866141732285504 ) ) ;
#56745 = CARTESIAN_POINT ( 'NONE',  ( -1.646051170424378096, -0.1870078740157480046, 1.254653134982923898E-17 ) ) ;
#56746 = CARTESIAN_POINT ( 'NONE',  ( 0.3280839895013130669, -0.004921259842519576551, 0.3153832671262227771 ) ) ;
#56747 = CARTESIAN_POINT ( 'NONE',  ( -1.292650918635170010, -0.6692913385826771977, 0.1292274648535927661 ) ) ;
#56748 = CARTESIAN_POINT ( 'NONE',  ( -0.6167979002624665030, -0.4281496062992127816, -0.4176697321401328100 ) ) ;
#56749 = CARTESIAN_POINT ( 'NONE',  ( -0.3460692066303960313, 0.1998031496062989965, -0.8904199475065617264 ) ) ;
#56750 = CARTESIAN_POINT ( 'NONE',  ( -0.2867679344610365999, 0.2867679344610364889, -2.309055118110235671 ) ) ;
#56751 = CARTESIAN_POINT ( 'NONE',  ( 0.5708661417322841158, -0.4536011799217368745, -0.2665933059059886201 ) ) ;
#56752 = CARTESIAN_POINT ( 'NONE',  ( -0.1902887139107604098, 0.2952755905511810774, -0.1292274648535930714 ) ) ;
#56753 = CARTESIAN_POINT ( 'NONE',  ( -0.8530183727034112984, 0.05413385826771666132, 0.4176697321401328100 ) ) ;
#56754 = CARTESIAN_POINT ( 'NONE',  ( -0.6299212598425188991, -0.1870078740157480601, -0.3641732283464567677 ) ) ;
#56755 = CARTESIAN_POINT ( 'NONE',  ( -3.936002401691375052, 1.071382210147229452, -0.09277206283147471089 ) ) ;
#56756 = CARTESIAN_POINT ( 'NONE',  ( -0.2296587926509179312, -0.05778040916215522460, 0.4822834645669289988 ) ) ;
#56757 = CARTESIAN_POINT ( 'NONE',  ( -1.673228346456691717, 0.07958543189024071263, -0.2665933059059888421 ) ) ;
#56758 = CARTESIAN_POINT ( 'NONE',  ( 1.574803149606299746, -0.1870078740157479769, 0.4822834645669291653 ) ) ;
#56759 = CARTESIAN_POINT ( 'NONE',  ( 0.01069919276010583738, 2.739544932778246860E-15, 0.4118477457932983032 ) ) ;
#56760 = ORIENTED_EDGE ( 'NONE', *, *, #31624, .F. ) ;
#56761 = CARTESIAN_POINT ( 'NONE',  ( 0.000000000000000000, 0.000000000000000000, 1.122047244094488194 ) ) ;
#56762 = CARTESIAN_POINT ( 'NONE',  ( -1.312335958005248715, -0.6046776061558809534, -0.2411417322834644161 ) ) ;
#56763 = CIRCLE ( 'NONE', #20509, 2.559055118110236560 ) ;
#56764 = CARTESIAN_POINT ( 'NONE',  ( -0.7808398950131225646, -0.05778040916215522460, 0.4822834645669289988 ) ) ;
#56765 = CARTESIAN_POINT ( 'NONE',  ( 1.614173228346457378, 0.2952755905511811885, 0.000000000000000000 ) ) ;
#56766 = CARTESIAN_POINT ( 'NONE',  ( -0.3917322834645671215, 0.1049643490035301469, -2.007217847769029007 ) ) ;
#56767 = CARTESIAN_POINT ( 'NONE',  ( 0.2155943732411896574, 0.3272402980636398007, -1.220472440944881942 ) ) ;
#56768 = CARTESIAN_POINT ( 'NONE',  ( 0.8333333333333340365, -0.6692913385826771977, 0.1292274648535927661 ) ) ;
#56769 = CARTESIAN_POINT ( 'NONE',  ( -0.06561679790026180015, 0.05413385826771666132, 0.4176697321401328100 ) ) ;
#56770 = CARTESIAN_POINT ( 'NONE',  ( 0.3503937007874016740, 0.3242060844882008741, 0.000000000000000000 ) ) ;
#56771 = CARTESIAN_POINT ( 'NONE',  ( -0.1998031496062991630, -0.3460692066303959202, -2.662073490813648746 ) ) ;
#56772 = CARTESIAN_POINT ( 'NONE',  ( 1.069553805774278610, -0.5511811023622046335, 0.09757992244046803654 ) ) ;
#56773 = CARTESIAN_POINT ( 'NONE',  ( -0.1998031496062994683, 0.3460692066303958092, -1.115485564304461885 ) ) ;
#56774 = VERTEX_POINT ( 'NONE', #56605 ) ;
#56775 = CARTESIAN_POINT ( 'NONE',  ( 4.797336870675656522E-17, -0.3917322834645670104, -2.748031496062991685 ) ) ;
#56776 = ORIENTED_EDGE ( 'NONE', *, *, #51390, .F. ) ;
#56777 = CARTESIAN_POINT ( 'NONE',  ( 0.2821522309711292364, -0.6692913385826771977, 0.1292274648535927661 ) ) ;
#56778 = CARTESIAN_POINT ( 'NONE',  ( -0.6692913385826764205, -0.6692913385826771977, 8.415575281601705876E-17 ) ) ;
#56779 = APPLICATION_CONTEXT ( 'automotive_design' ) ;
#56780 = CARTESIAN_POINT ( 'NONE',  ( -1.397637795275589623, -0.5400638737290845981, -0.3530559997133363437 ) ) ;
#56781 = CARTESIAN_POINT ( 'NONE',  ( 0.8267716535433078384, -0.6692913385826771977, 8.415575281601705876E-17 ) ) ;
#56782 = CARTESIAN_POINT ( 'NONE',  ( 1.509186351706037543, 0.05413385826771666132, 0.4176697321401328100 ) ) ;
#56783 = FACE_OUTER_BOUND ( 'NONE', #383, .T. ) ;
#56784 = CARTESIAN_POINT ( 'NONE',  ( -0.2690288713910754526, -0.6692913385826771977, 0.1292274648535927661 ) ) ;
#56785 = CARTESIAN_POINT ( 'NONE',  ( -1.437007874015747477, 0.1660481256975883668, -0.3530559997133364547 ) ) ;
#56786 = CARTESIAN_POINT ( 'NONE',  ( -1.555118110236219930, -0.5400638737290845981, -0.3530559997133363437 ) ) ;
#56787 = CARTESIAN_POINT ( 'NONE',  ( 1.509186351706037543, 0.05413385826771666132, 0.4176697321401328100 ) ) ;
#56788 = CARTESIAN_POINT ( 'NONE',  ( -0.3917322834645670104, -7.196005306013484475E-17, 0.1259842519685039908 ) ) ;
#56789 = CARTESIAN_POINT ( 'NONE',  ( 0.7283464566929143125, 0.07958543189024085140, 0.2665933059059887866 ) ) ;
#56790 = ORIENTED_EDGE ( 'NONE', *, *, #36043, .T. ) ;
#56791 = CARTESIAN_POINT ( 'NONE',  ( -9.674558042662121740E-17, 0.3949938075777409963, -0.3149606299212598937 ) ) ;
#56792 = ORIENTED_EDGE ( 'NONE', *, *, #7741, .T. ) ;
#56793 = CARTESIAN_POINT ( 'NONE',  ( -0.1509186351706028884, -0.08942795157527998196, 0.3641732283464567121 ) ) ;
#56794 = CARTESIAN_POINT ( 'NONE',  ( 1.141392835773559211, 0.000000000000000000, 1.141392835773562764 ) ) ;
#56795 = CARTESIAN_POINT ( 'NONE',  ( 0.4461942257217855201, -0.6046776061558807314, 0.2411417322834647770 ) ) ;
#56796 = CARTESIAN_POINT ( 'NONE',  ( 0.2493438320209980519, -0.4281496062992127816, -0.4176697321401328100 ) ) ;
#56797 = CARTESIAN_POINT ( 'NONE',  ( -0.4658792650918627265, -0.05778040916215522460, 0.4822834645669289988 ) ) ;
#56798 = CARTESIAN_POINT ( 'NONE',  ( -0.3917322834645670104, -0.1049643490035307020, -1.617473384023309091 ) ) ;
#56799 = CARTESIAN_POINT ( 'NONE',  ( -1.397637795275589623, -0.5400638737290845981, -0.3530559997133363437 ) ) ;
#56800 = PRODUCT_RELATED_PRODUCT_CATEGORY ( 'part', '', ( #70817 ) ) ;
#56801 = CARTESIAN_POINT ( 'NONE',  ( -0.3392501089628017219, -0.1958661417322836718, -2.499343832020997080 ) ) ;
#56802 = CARTESIAN_POINT ( 'NONE',  ( 1.220472440944882386, -0.5511811023622047445, 6.969142054262312111E-17 ) ) ;
#56803 = CARTESIAN_POINT ( 'NONE',  ( -1.450131233595799651, 0.2952755905511810774, -0.1292274648535930714 ) ) ;
#56804 = CARTESIAN_POINT ( 'NONE',  ( 0.7939632545931766261, -0.3162353388693409650, -0.4822834645669289433 ) ) ;
#56805 = CARTESIAN_POINT ( 'NONE',  ( 1.279527559055118724, -0.5400638737290845981, -0.3530559997133363437 ) ) ;
#56806 = CARTESIAN_POINT ( 'NONE',  ( 0.3996062992125986035, 0.1070741851644054776, -0.9120734908136483021 ) ) ;
#56807 = CARTESIAN_POINT ( 'NONE',  ( -1.240157480314959759, 0.1660481256975885056, 0.3530559997133364547 ) ) ;
#56808 = CARTESIAN_POINT ( 'NONE',  ( -9.787531504996566615E-17, 0.3996062992125985480, -0.2342519685039370358 ) ) ;
#56809 = CARTESIAN_POINT ( 'NONE',  ( -0.2362204724409442680, -0.1870078740157480879, -0.4822834645669291653 ) ) ;
#56810 = CARTESIAN_POINT ( 'NONE',  ( 4.893765752498283924E-17, -0.3996062992125986035, -2.283464566929133799 ) ) ;
#56811 = CARTESIAN_POINT ( 'NONE',  ( -0.1958661417322834220, -0.3392501089628018884, -1.567585301837270295 ) ) ;
#56812 = CARTESIAN_POINT ( 'NONE',  ( 1.509186351706037543, 0.05413385826771666132, 0.4176697321401328100 ) ) ;
#56813 = CARTESIAN_POINT ( 'NONE',  ( 0.07874015748031558404, -0.1870078740157479769, 0.3641732283464567677 ) ) ;
#56814 = CARTESIAN_POINT ( 'NONE',  ( 0.8858267716535438430, -0.5400638737290845981, -0.3530559997133363437 ) ) ;
#56815 = CARTESIAN_POINT ( 'NONE',  ( -0.4724409448818899238, 0.1265901696524986686, -1.211942257217847541 ) ) ;
#56816 = CARTESIAN_POINT ( 'NONE',  ( 0.7217847769028878924, -0.004921259842519576551, 0.3153832671262227771 ) ) ;
#56817 = EDGE_CURVE ( 'NONE', #69342, #14187, #11425, .T. ) ;
#56818 = CARTESIAN_POINT ( 'NONE',  ( 0.3083989501312343062, -0.3162353388693405765, 0.4822834645669290543 ) ) ;
#56819 = CARTESIAN_POINT ( 'NONE',  ( -0.3949938075777409963, -7.255918531996591613E-17, -0.9035433070866141225 ) ) ;
#56820 = CARTESIAN_POINT ( 'NONE',  ( -0.7874015748031489847, -0.1870078740157479769, 0.4822834645669291653 ) ) ;
#56821 = CARTESIAN_POINT ( 'NONE',  ( 0.4091458600556404646, -0.2362204724409448231, -1.126640419947506633 ) ) ;
#56822 = CARTESIAN_POINT ( 'NONE',  ( 0.8727034120734912248, -0.2845877964562161244, -0.3641732283464567121 ) ) ;
#56823 = EDGE_CURVE ( 'NONE', #60349, #30126, #18152, .T. ) ;
#56824 = CARTESIAN_POINT ( 'NONE',  ( 0.09842519685039433086, 0.1012011053420777407, 0.2882089793578256898 ) ) ;
#56825 = CARTESIAN_POINT ( 'NONE',  ( -0.4658792650918627265, -0.05778040916215522460, 0.4822834645669289988 ) ) ;
#56826 = CARTESIAN_POINT ( 'NONE',  ( 0.2362204724409456558, -0.1870078740157479769, 0.3641732283464567677 ) ) ;
#56827 = CARTESIAN_POINT ( 'NONE',  ( -2.869680830158521712, 1.067671560069319403, 0.06860298820098456596 ) ) ;
#56828 = CARTESIAN_POINT ( 'NONE',  ( -0.1312335958005241554, 0.2306618581243848609, 0.2411417322834645549 ) ) ;
#56829 = CARTESIAN_POINT ( 'NONE',  ( 0.4396325459317590445, -0.5511811023622046335, 0.09757992244046803654 ) ) ;
#56830 = CARTESIAN_POINT ( 'NONE',  ( -0.3996062992125986590, 0.1070741851644051723, -1.841863517060367661 ) ) ;
#56831 = CARTESIAN_POINT ( 'NONE',  ( 0.3674540682414705883, -0.6046776061558807314, 0.2411417322834647770 ) ) ;
#56832 = CARTESIAN_POINT ( 'NONE',  ( 1.036745406824147731, -0.004921259842519576551, 0.3153832671262227771 ) ) ;
#56833 = CARTESIAN_POINT ( 'NONE',  ( 2.795275590551181910, 1.805669738366189048, 0.000000000000000000 ) ) ;
#56834 = CARTESIAN_POINT ( 'NONE',  ( -0.5905511811023615998, 0.1771653543307087630, 0.000000000000000000 ) ) ;
#56835 = CARTESIAN_POINT ( 'NONE',  ( -0.8202099737532801971, -0.5511811023622046335, 0.09757992244046803654 ) ) ;
#56836 = CARTESIAN_POINT ( 'NONE',  ( -0.3937007874015740483, -0.1870078740157479769, 0.4822834645669291653 ) ) ;
#56837 = CARTESIAN_POINT ( 'NONE',  ( 0.2099737532808405305, 0.2306618581243847221, -0.2411417322834647770 ) ) ;
#56838 = CARTESIAN_POINT ( 'NONE',  ( 0.8202099737532814183, -0.5511811023622048555, -0.09757992244046775898 ) ) ;
#56839 = FACE_OUTER_BOUND ( 'NONE', #72175, .T. ) ;
#56840 = CARTESIAN_POINT ( 'NONE',  ( 1.476377952755906220, 0.07958543189024071263, -0.2665933059059888421 ) ) ;
#56841 = ADVANCED_FACE ( 'NONE', ( #37665 ), #35639, .T. ) ;
#56842 = CARTESIAN_POINT ( 'NONE',  ( 0.7020997375328090762, -0.3162353388693405765, 0.4822834645669290543 ) ) ;
#56843 = CARTESIAN_POINT ( 'NONE',  ( 0.1938976377952755792, -0.1938976377952756069, 0.07874015748031495954 ) ) ;
#56844 = CARTESIAN_POINT ( 'NONE',  ( -0.1377952755905504645, 0.1660481256975885056, 0.3530559997133364547 ) ) ;
#56845 = CARTESIAN_POINT ( 'NONE',  ( -0.1049643490035307020, 0.3917322834645669549, -1.193569553805774452 ) ) ;
#56846 = CARTESIAN_POINT ( 'NONE',  ( 0.8333333333333340365, -0.6692913385826771977, 0.1292274648535927661 ) ) ;
#56847 = CARTESIAN_POINT ( 'NONE',  ( 0.6758530183727039509, -0.6692913385826771977, 0.1292274648535927661 ) ) ;
#56848 = CARTESIAN_POINT ( 'NONE',  ( -1.559171609364246924, 0.3937007874015747699, 0.4177787735906735578 ) ) ;
#56849 = CARTESIAN_POINT ( 'NONE',  ( 0.1837270341207357105, -0.5023911411419708095, -0.1820866141732282451 ) ) ;
#56850 = CARTESIAN_POINT ( 'NONE',  ( 1.410761154855643795, -0.05778040916215560624, -0.4822834645669293319 ) ) ;
#56851 = EDGE_CURVE ( 'NONE', #71433, #27584, #27573, .T. ) ;
#56852 = CARTESIAN_POINT ( 'NONE',  ( -0.3149606299212590610, -0.1870078740157479769, 0.3641732283464567677 ) ) ;
#56853 = CARTESIAN_POINT ( 'NONE',  ( -0.3083989501312330295, -0.3162353388693409650, -0.4822834645669289433 ) ) ;
#56854 = CARTESIAN_POINT ( 'NONE',  ( 0.5157744752572718250, 1.509207849855008998, -0.5177606540819982284 ) ) ;
#56855 = CARTESIAN_POINT ( 'NONE',  ( 0.3149606299212603933, -0.1870078740157479769, 0.4822834645669291653 ) ) ;
#56856 = CARTESIAN_POINT ( 'NONE',  ( -0.6364829396325453192, -0.05778040916215560624, -0.4822834645669293319 ) ) ;
#56857 = AXIS2_PLACEMENT_3D ( 'NONE', #60805, #23334, #67552 ) ;
#56858 = CARTESIAN_POINT ( 'NONE',  ( -0.7152230971128602510, -0.08942795157528024563, -0.3641732283464568787 ) ) ;
#56859 = CARTESIAN_POINT ( 'NONE',  ( 0.2887139107611556010, -0.6046776061558807314, 0.2411417322834647770 ) ) ;
#56860 = CARTESIAN_POINT ( 'NONE',  ( -1.056430446194224881, 0.2952755905511810774, -0.1292274648535930714 ) ) ;
#56861 = CARTESIAN_POINT ( 'NONE',  ( -0.4461942257217840213, -0.6046776061558809534, -0.2411417322834644161 ) ) ;
#56862 = EDGE_CURVE ( 'NONE', #73164, #52448, #13671, .T. ) ;
#56863 = CARTESIAN_POINT ( 'NONE',  ( -0.03443470937339728616, 0.2755905511811023723, -1.537015892239756099 ) ) ;
#56865 = CARTESIAN_POINT ( 'NONE',  ( 1.443569553805774897, 0.2306618581243848609, 0.2411417322834645549 ) ) ;
#56864 = CARTESIAN_POINT ( 'NONE',  ( -0.5944687039322197331, 1.968503937007873850, 0.4915354330708656128 ) ) ;
#56866 = CARTESIAN_POINT ( 'NONE',  ( -0.06873123812452887338, -2.191421614605370878E-15, 0.4445507791589071167 ) ) ;
#56867 = DIRECTION ( 'NONE',  ( 1.000000000000000000, 0.000000000000000000, -0.000000000000000000 ) ) ;
#56868 = FACE_OUTER_BOUND ( 'NONE', #64279, .T. ) ;
#56869 = CARTESIAN_POINT ( 'NONE',  ( -0.8202099737532801971, -0.6692913385826771977, 0.1292274648535927661 ) ) ;
#56870 =( BOUNDED_CURVE ( )  B_SPLINE_CURVE ( 1, ( #51776, #26115 ),
 .UNSPECIFIED., .F., .F. ) 
 B_SPLINE_CURVE_WITH_KNOTS ( ( 2, 2 ),
 ( 1.748223473168675632E-18, 0.001849999999999997913 ),
 .UNSPECIFIED. ) 
 CURVE ( )  GEOMETRIC_REPRESENTATION_ITEM ( )  RATIONAL_B_SPLINE_CURVE ( ( 0.9911642120908021880, 0.9911642120908021880 ) ) 
 REPRESENTATION_ITEM ( '' )  );
#56871 = CARTESIAN_POINT ( 'NONE',  ( -0.4724409448818898682, -8.678599364036362592E-17, -0.3543307086614173040 ) ) ;
#56872 = CARTESIAN_POINT ( 'NONE',  ( -9.787531504996567848E-17, 0.3996062992125986035, 0.1574803149606298913 ) ) ;
#56873 = EDGE_LOOP ( 'NONE', ( #12301, #70769, #43963, #63825, #5783, #43860, #40161, #15353 ) ) ;
#56874 = CARTESIAN_POINT ( 'NONE',  ( 0.2427821522309719648, -0.08942795157527998196, 0.3641732283464567121 ) ) ;
#56876 = CARTESIAN_POINT ( 'NONE',  ( 0.3917322834645670104, 2.398668435337828261E-17, -1.370078740157480324 ) ) ;
#56875 = VECTOR ( 'NONE', #47760, 39.37007874015748143 ) ;
#56877 = CARTESIAN_POINT ( 'NONE',  ( 0.7414698162729663755, -0.6692913385826773087, -0.1292274648535924053 ) ) ;
#56878 = CARTESIAN_POINT ( 'NONE',  ( 0.05073257145186254452, 0.3893108287682404689, -2.755905511811024944 ) ) ;
#56879 = CARTESIAN_POINT ( 'NONE',  ( -0.5631141337314348183, -4.643576453225290411E-15, -0.3627989612356168347 ) ) ;
#56880 = CARTESIAN_POINT ( 'NONE',  ( -0.6167979002624665030, -0.3690944881889765550, -0.3153832671262227771 ) ) ;
#56881 = DIRECTION ( 'NONE',  ( -3.491481338843133355E-15, -0.000000000000000000, 1.000000000000000000 ) ) ;
#56882 = CARTESIAN_POINT ( 'NONE',  ( 1.108923884514436686, -0.3162353388693409650, -0.4822834645669289433 ) ) ;
#56883 = CARTESIAN_POINT ( 'NONE',  ( 0.7939632545931766261, -0.08942795157527998196, 0.3641732283464567121 ) ) ;
#56884 = CARTESIAN_POINT ( 'NONE',  ( 0.1377952755905518800, 0.1660481256975883668, -0.3530559997133364547 ) ) ;
#56885 = CARTESIAN_POINT ( 'NONE',  ( -0.3392501089628019439, 0.1958661417322832554, -0.8936814716197357678 ) ) ;
#56886 = CARTESIAN_POINT ( 'NONE',  ( -0.5577427821522301654, -0.3162353388693405765, 0.4822834645669290543 ) ) ;
#56887 = CARTESIAN_POINT ( 'NONE',  ( -1.240157480314959759, 0.07958543189024085140, 0.2665933059059887866 ) ) ;
#56888 = CARTESIAN_POINT ( 'NONE',  ( -0.3083989501312330295, -0.05778040916215522460, 0.4822834645669289988 ) ) ;
#56889 = CARTESIAN_POINT ( 'NONE',  ( -1.604771003085130321, 1.044625174762916719, 0.1466069496707742559 ) ) ;
#56890 = DIRECTION ( 'NONE',  ( 0.000000000000000000, 0.000000000000000000, 1.000000000000000000 ) ) ;
#56891 = ORIENTED_EDGE ( 'NONE', *, *, #47083, .T. ) ;
#56892 = CARTESIAN_POINT ( 'NONE',  ( 0.3917322834645670659, -0.1049643490035303273, -1.840570496884201379 ) ) ;
#56893 = CARTESIAN_POINT ( 'NONE',  ( 0.2624671916010504757, 0.2306618581243848609, 0.2411417322834645549 ) ) ;
#56894 = EDGE_LOOP ( 'NONE', ( #21504, #24284, #35247 ) ) ;
#56895 = CARTESIAN_POINT ( 'NONE',  ( -0.1509186351706028884, -0.05778040916215522460, 0.4822834645669289988 ) ) ;
#56896 = CARTESIAN_POINT ( 'NONE',  ( -1.253280839895012377, -0.3162353388693409650, -0.4822834645669289433 ) ) ;
#56897 = CARTESIAN_POINT ( 'NONE',  ( 0.6824146981627303710, 0.2306618581243847221, -0.2411417322834647770 ) ) ;
#56898 = CARTESIAN_POINT ( 'NONE',  ( 0.006561679790026889343, -0.3162353388693409650, -0.4822834645669289433 ) ) ;
#56899 = CARTESIAN_POINT ( 'NONE',  ( 0.1958661417322836440, -0.3392501089628017219, -1.593832020997375531 ) ) ;
#56900 = CARTESIAN_POINT ( 'NONE',  ( -0.9842519685039365918, -0.6692913385826771977, 8.415575281601705876E-17 ) ) ;
#56901 = CARTESIAN_POINT ( 'NONE',  ( 0.2034120734908144990, -0.6692913385826771977, 0.1292274648535927661 ) ) ;
#56902 = CARTESIAN_POINT ( 'NONE',  ( -0.3477690288713902178, 0.2952755905511810774, -0.1292274648535930714 ) ) ;
#56903 = CARTESIAN_POINT ( 'NONE',  ( 0.3149606299212606708, -0.1870078740157480601, -0.3641732283464567677 ) ) ;
#56904 = CARTESIAN_POINT ( 'NONE',  ( -0.0003067303408297487139, 0.3990339831394625336, 7.618016766297074103E-18 ) ) ;
#56905 = CARTESIAN_POINT ( 'NONE',  ( -0.1574803149606292529, -0.1870078740157479769, 0.4822834645669291653 ) ) ;
#56906 = CARTESIAN_POINT ( 'NONE',  ( -2.094141031014932874, 1.724409448818898127, -0.4359958488159723644 ) ) ;
#56907 = CARTESIAN_POINT ( 'NONE',  ( 1.601049868766404982, 0.2306618581243848609, 0.2411417322834645549 ) ) ;
#56908 = CARTESIAN_POINT ( 'NONE',  ( -0.3917322834645669549, -0.1049643490035306603, -2.715223097112861250 ) ) ;
#56909 = ORIENTED_EDGE ( 'NONE', *, *, #50213, .T. ) ;
#56910 = ORIENTED_EDGE ( 'NONE', *, *, #34100, .T. ) ;
#56911 = CARTESIAN_POINT ( 'NONE',  ( 0.3937007874015754361, -0.1870078740157479769, 0.4822834645669291653 ) ) ;
#56912 = CARTESIAN_POINT ( 'NONE',  ( -0.05905511811023545637, -0.4536011799217368745, -0.2665933059059886201 ) ) ;
#56914 = DIRECTION ( 'NONE',  ( -0.8660254037844433705, 0.000000000000000000, 0.4999999999999920064 ) ) ;
#56913 = CARTESIAN_POINT ( 'NONE',  ( 1.253280839895013710, -0.08942795157528024563, -0.3641732283464568787 ) ) ;
#56915 = CARTESIAN_POINT ( 'NONE',  ( -9.594673741351313045E-17, 0.3917322834645670104, -1.029527559055118280 ) ) ;
#56916 = CARTESIAN_POINT ( 'NONE',  ( 0.4889872687189469880, 1.535433070866141225, 0.000000000000000000 ) ) ;
#56917 = FACE_OUTER_BOUND ( 'NONE', #39185, .T. ) ;
#56918 = EDGE_CURVE ( 'NONE', #7519, #16433, #6925, .T. ) ;
#56919 = CARTESIAN_POINT ( 'NONE',  ( -0.1998031496062991630, -0.3460692066303959202, -2.662073490813648746 ) ) ;
#56920 = CARTESIAN_POINT ( 'NONE',  ( 0.2624671916010504757, -0.6046776061558809534, -0.2411417322834644161 ) ) ;
#56921 = CARTESIAN_POINT ( 'NONE',  ( -1.128608923884513837, 0.2306618581243847221, -0.2411417322834647770 ) ) ;
#56922 = VECTOR ( 'NONE', #30256, 39.37007874015748143 ) ;
#56923 = CARTESIAN_POINT ( 'NONE',  ( -0.9776902887139098386, -0.6692913385826771977, 0.1292274648535927661 ) ) ;
#56924 = CARTESIAN_POINT ( 'NONE',  ( 0.09842519685039434474, -0.5400638737290845981, -0.3530559997133363437 ) ) ;
#56925 = CARTESIAN_POINT ( 'NONE',  ( 0.8661417322834652488, -0.1870078740157480879, -0.4822834645669291653 ) ) ;
#56926 = CARTESIAN_POINT ( 'NONE',  ( 1.318897637795276356, -0.4536011799217367080, 0.2665933059059888421 ) ) ;
#56927 = CARTESIAN_POINT ( 'NONE',  ( 1.003937007874016407, -0.4536011799217367080, 0.2665933059059888421 ) ) ;
#56928 = CARTESIAN_POINT ( 'NONE',  ( -1.062992125984250968, -0.6692913385826771977, 8.415575281601705876E-17 ) ) ;
#56929 = CARTESIAN_POINT ( 'NONE',  ( -0.3996062992125984925, -0.1070741851644056858, -0.2801837270341207553 ) ) ;
#56930 = CARTESIAN_POINT ( 'NONE',  ( 1.587926509186352586, -0.4281496062992127816, -0.4176697321401328100 ) ) ;
#56931 = CARTESIAN_POINT ( 'NONE',  ( -0.3392501089628017219, -0.1958661417322836718, -0.3595800524934382736 ) ) ;
#56933 = FACE_OUTER_BOUND ( 'NONE', #56597, .T. ) ;
#56932 = CARTESIAN_POINT ( 'NONE',  ( 1.240157480314961314, 0.1660481256975883668, -0.3530559997133364547 ) ) ;
#56934 = CARTESIAN_POINT ( 'NONE',  ( -1.686351706036744558, 0.1771653543307087075, -0.09757992244046823083 ) ) ;
#56935 = CARTESIAN_POINT ( 'NONE',  ( 0.1640419947506569498, -0.3162353388693409650, -0.4822834645669289433 ) ) ;
#56936 = CARTESIAN_POINT ( 'NONE',  ( 0.7677165354330716118, -0.4536011799217367080, 0.2665933059059888421 ) ) ;
#56937 = CARTESIAN_POINT ( 'NONE',  ( -1.456692913385826182, -0.5511811023622047445, 6.969142054262312111E-17 ) ) ;
#56938 = CARTESIAN_POINT ( 'NONE',  ( 1.122047244094488860, -0.5400638737290845981, -0.3530559997133363437 ) ) ;
#56939 = DIRECTION ( 'NONE',  ( 0.000000000000000000, 0.000000000000000000, -1.000000000000000000 ) ) ;
#56940 = CARTESIAN_POINT ( 'NONE',  ( -0.5446194225721777693, -0.2845877964562161244, -0.3641732283464567121 ) ) ;
#56941 = CARTESIAN_POINT ( 'NONE',  ( -0.7349081364829390672, 0.2306618581243847221, -0.2411417322834647770 ) ) ;
#56942 = CARTESIAN_POINT ( 'NONE',  ( 1.528871391076116026, 0.2952755905511811885, 0.1292274648535926551 ) ) ;
#56943 = CARTESIAN_POINT ( 'NONE',  ( -1.200787401574802349, 0.1660481256975883668, -0.3530559997133364547 ) ) ;
#56944 = CARTESIAN_POINT ( 'NONE',  ( 1.312335958005250269, -0.6046776061558807314, 0.2411417322834647770 ) ) ;
#56945 = CARTESIAN_POINT ( 'NONE',  ( 0.1049643490035304799, -0.3917322834645670104, -0.8694418879603171835 ) ) ;
#56946 = CARTESIAN_POINT ( 'NONE',  ( -1.259842519685038686, -0.1870078740157480601, -0.3641732283464567677 ) ) ;
#56947 = CARTESIAN_POINT ( 'NONE',  ( 0.1938976377952755792, 0.1938976377952755792, -0.3740157480314971750 ) ) ;
#56948 = CARTESIAN_POINT ( 'NONE',  ( 0.7874015748031503170, -0.1870078740157479769, 0.4822834645669291653 ) ) ;
#56949 = CARTESIAN_POINT ( 'NONE',  ( -0.1265901696524986964, -0.4724409448818899238, -2.511154855643044748 ) ) ;
#56950 = CARTESIAN_POINT ( 'NONE',  ( -1.646981627296586703, -0.3162353388693409650, -0.4822834645669289433 ) ) ;
#56951 = CARTESIAN_POINT ( 'NONE',  ( 1.660104986876641320, -0.05778040916215522460, 0.4822834645669289988 ) ) ;
#56952 = CARTESIAN_POINT ( 'NONE',  ( -1.187664041994750175, -0.08942795157528024563, -0.3641732283464568787 ) ) ;
#56953 = CARTESIAN_POINT ( 'NONE',  ( 1.515748031496063408, 0.07958543189024085140, 0.2665933059059887866 ) ) ;
#56954 = CARTESIAN_POINT ( 'NONE',  ( -0.5446194225721777693, -0.05778040916215522460, 0.4822834645669289988 ) ) ;
#56955 = CARTESIAN_POINT ( 'NONE',  ( 0.1574803149606306130, -0.1870078740157480601, -0.3641732283464567677 ) ) ;
#56956 = CARTESIAN_POINT ( 'NONE',  ( -1.548556430446193399, 0.1283753931104748280, 0.1820866141732283561 ) ) ;
#56957 = CARTESIAN_POINT ( 'NONE',  ( 1.272965879265092637, -0.004921259842519576551, 0.3153832671262227771 ) ) ;
#56958 = CARTESIAN_POINT ( 'NONE',  ( 0.8005249343832028242, -0.4281496062992127816, -0.4176697321401328100 ) ) ;
#56959 = CARTESIAN_POINT ( 'NONE',  ( 1.469816272965879911, 0.2306618581243847221, -0.2411417322834647770 ) ) ;
#56960 = CARTESIAN_POINT ( 'NONE',  ( 0.1837270341207357105, -0.5023911411419708095, -0.1820866141732282451 ) ) ;
#56961 = CARTESIAN_POINT ( 'NONE',  ( 0.2952755905511819101, 0.1660481256975883668, -0.3530559997133364547 ) ) ;
#56962 = CARTESIAN_POINT ( 'NONE',  ( 1.122047244094488860, 0.07958543189024085140, 0.2665933059059887866 ) ) ;
#56963 = ORIENTED_EDGE ( 'NONE', *, *, #28027, .T. ) ;
#56964 = CARTESIAN_POINT ( 'NONE',  ( -1.469816272965878357, 0.2306618581243848609, 0.2411417322834645549 ) ) ;
#56965 = CARTESIAN_POINT ( 'NONE',  ( -1.227034120734907141, -0.6692913385826773087, -0.1292274648535924053 ) ) ;
#56966 = CARTESIAN_POINT ( 'NONE',  ( -0.07217847769028813698, -0.3162353388693409650, -0.4822834645669289433 ) ) ;
#56967 = CARTESIAN_POINT ( 'NONE',  ( -9.787531504996567848E-17, 0.3996062992125986035, -0.4724409448818898127 ) ) ;
#56968 = CARTESIAN_POINT ( 'NONE',  ( -0.1070741851644056997, 0.3996062992125984925, -2.603018372703412631 ) ) ;
#56969 = CARTESIAN_POINT ( 'NONE',  ( 0.4593175853018379162, -0.4281496062992124485, 0.4176697321401328655 ) ) ;
#56970 = CARTESIAN_POINT ( 'NONE',  ( 1.030183727034121421, -0.2845877964562161244, -0.3641732283464567121 ) ) ;
#56971 = CARTESIAN_POINT ( 'NONE',  ( -0.2690288713910754526, -0.6692913385826771977, 0.1292274648535927661 ) ) ;
#56972 = CARTESIAN_POINT ( 'NONE',  ( 0.2624671916010504757, -0.6046776061558809534, -0.2411417322834644161 ) ) ;
#56973 = CARTESIAN_POINT ( 'NONE',  ( -0.1998031496062994683, 0.3460692066303958092, -2.375328083989501238 ) ) ;
#56974 = CARTESIAN_POINT ( 'NONE',  ( -0.3420746716998661618, 0.1974969037888702206, -1.601049868766404094 ) ) ;
#56975 = CARTESIAN_POINT ( 'NONE',  ( -0.3996062992125986035, -0.1070741851644056997, -2.880577427821522374 ) ) ;
#56976 = CARTESIAN_POINT ( 'NONE',  ( -0.5314960629921169355, 2.755905511811024056, -2.583694225513482490 ) ) ;
#56977 = VECTOR ( 'NONE', #71000, 39.37007874015748143 ) ;
#56978 = CARTESIAN_POINT ( 'NONE',  ( -0.1049643490035307020, 0.3917322834645669549, -0.6286089238845143923 ) ) ;
#56979 = CARTESIAN_POINT ( 'NONE',  ( -0.4265091863517051496, 0.1771653543307087075, -0.09757992244046823083 ) ) ;
#56980 = CARTESIAN_POINT ( 'NONE',  ( -0.7808398950131225646, -0.05778040916215522460, 0.4822834645669289988 ) ) ;
#56981 = CARTESIAN_POINT ( 'NONE',  ( 0.1058382717557500852, -0.3949938075777408852, -2.681758530183727451 ) ) ;
#56982 = CARTESIAN_POINT ( 'NONE',  ( 0.6955380577427828781, -0.4281496062992124485, 0.4176697321401328655 ) ) ;
#56983 = CARTESIAN_POINT ( 'NONE',  ( -1.463254593175852492, 0.2952755905511811885, 0.1292274648535926551 ) ) ;
#56984 = CARTESIAN_POINT ( 'NONE',  ( 0.9383202099737536495, -0.3162353388693405765, 0.4822834645669290543 ) ) ;
#56985 = CARTESIAN_POINT ( 'NONE',  ( -0.4724409448818898682, -8.678599364036362592E-17, -2.874015748031495843 ) ) ;
#56986 = CARTESIAN_POINT ( 'NONE',  ( -0.2925321140481930704, -0.2925321140481933480, -2.106299212598425452 ) ) ;
#56987 = CARTESIAN_POINT ( 'NONE',  ( 1.614173228346457378, -0.6692913385826771977, 8.415575281601705876E-17 ) ) ;
#56988 = CARTESIAN_POINT ( 'NONE',  ( 0.8923884514435701520, -0.6046776061558809534, -0.2411417322834644161 ) ) ;
#56989 = CARTESIAN_POINT ( 'NONE',  ( 0.6167979002624678353, -0.4281496062992124485, 0.4176697321401328655 ) ) ;
#56990 = CONICAL_SURFACE ( 'NONE', #15340, 3.582677165354331450, 0.5235987755982945968 ) ;
#56991 = CARTESIAN_POINT ( 'NONE',  ( 0.8530183727034126306, -0.004921259842519870586, -0.3153832671262229437 ) ) ;
#56992 = CARTESIAN_POINT ( 'NONE',  ( 1.364829396325460076, 0.2306618581243848609, 0.2411417322834645549 ) ) ;
#56993 = CARTESIAN_POINT ( 'NONE',  ( 0.1958661417322836440, -0.3392501089628017219, -0.1765091863517061210 ) ) ;
#56994 = CARTESIAN_POINT ( 'NONE',  ( -0.5314960629921346991, 2.755905511811024056, 2.503252890251014939 ) ) ;
#56995 = CARTESIAN_POINT ( 'NONE',  ( 0.9448818897637802916, -0.1870078740157480879, -0.4822834645669291653 ) ) ;
#56996 = CARTESIAN_POINT ( 'NONE',  ( 1.620734908136483465, -0.5511811023622046335, 0.09757992244046803654 ) ) ;
#56997 = CARTESIAN_POINT ( 'NONE',  ( -0.4330708661417315697, 0.2952755905511811885, 0.000000000000000000 ) ) ;
#56998 = CARTESIAN_POINT ( 'NONE',  ( -1.181102362204723644, -0.1870078740157480879, -0.4822834645669291653 ) ) ;
#56999 = CARTESIAN_POINT ( 'NONE',  ( 1.049868766404200127, -0.6046776061558809534, -0.2411417322834644161 ) ) ;
#57000 = CARTESIAN_POINT ( 'NONE',  ( -0.3917322834645670104, -7.196005306013484475E-17, -0.4389763779527560139 ) ) ;
#57001 = CARTESIAN_POINT ( 'NONE',  ( 0.1049643490035303689, 0.3917322834645670104, -1.402887139107611647 ) ) ;
#57002 =( BOUNDED_CURVE ( )  B_SPLINE_CURVE ( 2, ( #44348, #70039, #57402, #76776, #83093, #52752, #47270, #19953, #78876, #71714, #39298, #14069, #1846 ),
 .UNSPECIFIED., .F., .F. ) 
 B_SPLINE_CURVE_WITH_KNOTS ( ( 3, 2, 2, 2, 2, 2, 3 ),
 ( 0.08750000000000000833, 0.09166666666666667407, 0.09583333333333335369, 0.1000000000000000056, 0.1041666666666666713, 0.1083333333333333370, 0.1125000000000000028 ),
 .UNSPECIFIED. ) 
 CURVE ( )  GEOMETRIC_REPRESENTATION_ITEM ( )  RATIONAL_B_SPLINE_CURVE ( ( 0.9999999999999998890, 0.9659258262890684232, 1.000000000000000000, 0.9659258262890683122, 1.000000000000000000, 0.9659258262890683122, 1.000000000000000000, 0.9659258262890683122, 1.000000000000000000, 0.9659258262890683122, 1.000000000000000000, 0.9659258262890683122, 1.000000000000000000 ) ) 
 REPRESENTATION_ITEM ( '' )  );
#57003 = CARTESIAN_POINT ( 'NONE',  ( -0.1049643490035302024, -0.3917322834645671215, -2.583989501312335513 ) ) ;
#57004 = ORIENTED_EDGE ( 'NONE', *, *, #6973, .T. ) ;
#57005 = CARTESIAN_POINT ( 'NONE',  ( -0.3460692066303960868, 0.1998031496062990242, 0.1312335958005249048 ) ) ;
#57006 = VERTEX_POINT ( 'NONE', #58258 ) ;
#57007 = CARTESIAN_POINT ( 'NONE',  ( -0.05249343832020910566, 0.1539470093639523085, 0.1968503937007873850 ) ) ;
#57008 = CARTESIAN_POINT ( 'NONE',  ( 1.325459317585302665, -0.004921259842519870586, -0.3153832671262229437 ) ) ;
#57009 = CARTESIAN_POINT ( 'NONE',  ( -9.787531504996567848E-17, 0.3996062992125986035, -1.574803149606299302 ) ) ;
#57010 = CARTESIAN_POINT ( 'NONE',  ( 1.338582677165355062, -0.1870078740157479769, 0.3641732283464567677 ) ) ;
#57011 = CARTESIAN_POINT ( 'NONE',  ( 0.4091458600556403535, 0.2362204724409449896, -2.412729658792650778 ) ) ;
#57012 = CARTESIAN_POINT ( 'NONE',  ( -3.937007874015748143, 2.559055118110236560, -0.3149606299212599492 ) ) ;
#57013 = CARTESIAN_POINT ( 'NONE',  ( -0.2316604258778182934, 1.900147917493397953, 0.2109207562938686387 ) ) ;
#57014 = CARTESIAN_POINT ( 'NONE',  ( -0.3917322834645671215, 0.1049643490035301469, -0.4324146981627298159 ) ) ;
#57015 = EDGE_CURVE ( 'NONE', #59797, #70928, #62483, .T. ) ;
#57016 = CARTESIAN_POINT ( 'NONE',  ( -0.6889763779527552368, 0.07958543189024085140, 0.2665933059059887866 ) ) ;
#57017 = CARTESIAN_POINT ( 'NONE',  ( -1.666666666666665853, -0.004921259842519870586, -0.3153832671262229437 ) ) ;
#57018 = CARTESIAN_POINT ( 'NONE',  ( -1.312335958005248715, 0.2306618581243848609, 0.2411417322834645549 ) ) ;
#57019 = CARTESIAN_POINT ( 'NONE',  ( -0.06561679790026180015, -0.4281496062992127816, -0.4176697321401328100 ) ) ;
#57020 = CARTESIAN_POINT ( 'NONE',  ( 1.456692913385827515, 0.2952755905511811885, 0.000000000000000000 ) ) ;
#57021 = ORIENTED_EDGE ( 'NONE', *, *, #66513, .F. ) ;
#57022 = CARTESIAN_POINT ( 'NONE',  ( 1.581364829396326277, -0.05778040916215522460, 0.4822834645669289988 ) ) ;
#57023 = CARTESIAN_POINT ( 'NONE',  ( 1.089942661822472569, 9.906153642143428645E-17, -0.3464511005275205946 ) ) ;
#57024 = DIRECTION ( 'NONE',  ( -0.9758237301628308602, 0.000000000000000000, 0.2185590255539659466 ) ) ;
#57025 = CARTESIAN_POINT ( 'NONE',  ( -0.4724409448818899238, 0.1265901696524986686, -2.237532808398950301 ) ) ;
#57026 = CARTESIAN_POINT ( 'NONE',  ( 2.169549097624094092, 1.554815631980116741, 0.4741686481756398064 ) ) ;
#57027 = CARTESIAN_POINT ( 'NONE',  ( -0.4133858267716528645, -0.4536011799217367080, 0.2665933059059888421 ) ) ;
#57028 = CARTESIAN_POINT ( 'NONE',  ( -1.174540682414697335, -0.05778040916215522460, 0.4822834645669289988 ) ) ;
#57029 = CARTESIAN_POINT ( 'NONE',  ( 1.003937007874016407, -0.5400638737290844871, 0.3530559997133364547 ) ) ;
#57030 = ORIENTED_EDGE ( 'NONE', *, *, #29559, .F. ) ;
#57032 = FACE_OUTER_BOUND ( 'NONE', #32040, .T. ) ;
#57031 = CARTESIAN_POINT ( 'NONE',  ( 1.220472440944881942, 0.000000000000000000, -0.5309055118110238558 ) ) ;
#57033 = CARTESIAN_POINT ( 'NONE',  ( 1.410761154855643795, -0.05778040916215560624, -0.4822834645669293319 ) ) ;
#57034 = CARTESIAN_POINT ( 'NONE',  ( -1.338582677165353729, -0.1870078740157480879, -0.4822834645669291653 ) ) ;
#57035 = CARTESIAN_POINT ( 'NONE',  ( -0.3917322834645670659, 0.1049643490035301607, -0.2703218915672423450 ) ) ;
#57036 = CARTESIAN_POINT ( 'NONE',  ( -0.2821522309711278487, 0.1771653543307087630, 0.09757992244046791164 ) ) ;
#57037 = CARTESIAN_POINT ( 'NONE',  ( -0.3917322834645670104, -7.196005306013484475E-17, -0.7539370078740157410 ) ) ;
#57038 = AXIS2_PLACEMENT_3D ( 'NONE', #68454, #5296, #11208 ) ;
#57039 = CARTESIAN_POINT ( 'NONE',  ( -0.6824146981627288167, 0.1283753931104748280, 0.1820866141732283561 ) ) ;
#57040 = CARTESIAN_POINT ( 'NONE',  ( 0.3412073490813655186, 0.1283753931104748280, 0.1820866141732283561 ) ) ;
#57041 = CARTESIAN_POINT ( 'NONE',  ( 0.3149606299212603933, -0.1870078740157479769, 0.4822834645669291653 ) ) ;
#57042 = CARTESIAN_POINT ( 'NONE',  ( -0.7808398950131222316, -0.2845877964562161244, -0.3641732283464567121 ) ) ;
#57043 = CARTESIAN_POINT ( 'NONE',  ( 0.3917322834645670104, -0.1049643490035303411, -2.938320209973753538 ) ) ;
#57044 = CARTESIAN_POINT ( 'NONE',  ( 1.351706036745407458, -0.4281496062992127816, -0.4176697321401328100 ) ) ;
#57045 = CARTESIAN_POINT ( 'NONE',  ( -0.9383202099737524282, -0.3162353388693409650, -0.4822834645669289433 ) ) ;
#57046 = CARTESIAN_POINT ( 'NONE',  ( -0.4091458600556402980, -0.2362204724409451284, -1.389107611548556553 ) ) ;
#57047 = CARTESIAN_POINT ( 'NONE',  ( -0.2624671916010490880, 0.2306618581243847221, -0.2411417322834647770 ) ) ;
#57048 = CARTESIAN_POINT ( 'NONE',  ( -0.8661417322834640276, -0.1870078740157479769, 0.4822834645669291653 ) ) ;
#57049 = CARTESIAN_POINT ( 'NONE',  ( 1.167979002624672580, -0.3690944881889763329, 0.3153832671262228327 ) ) ;
#57050 = AXIS2_PLACEMENT_3D ( 'NONE', #15093, #2042, #15930 ) ;
#57051 = CARTESIAN_POINT ( 'NONE',  ( -0.2230971128608915943, -0.3690944881889765550, -0.3153832671262227771 ) ) ;
#57052 = CARTESIAN_POINT ( 'NONE',  ( -0.6824146981627291497, -0.6046776061558809534, -0.2411417322834644161 ) ) ;
#57053 = CARTESIAN_POINT ( 'NONE',  ( -1.062992125984250968, -0.6692913385826771977, 8.415575281601705876E-17 ) ) ;
#57054 = CARTESIAN_POINT ( 'NONE',  ( -0.7137454485294952855, 2.362204724409448620, 0.4917280318828573527 ) ) ;
#57055 = CARTESIAN_POINT ( 'NONE',  ( 1.456692913385827515, -0.5511811023622047445, 6.969142054262312111E-17 ) ) ;
#57056 = CARTESIAN_POINT ( 'NONE',  ( -0.1706036745406816491, 0.05413385826771626580, -0.4176697321401330321 ) ) ;
#57057 = CARTESIAN_POINT ( 'NONE',  ( -1.174540682414697335, -0.3162353388693409650, -0.4822834645669289433 ) ) ;
#57058 = ORIENTED_EDGE ( 'NONE', *, *, #50024, .T. ) ;
#57059 = CARTESIAN_POINT ( 'NONE',  ( 0.1070741851644054776, -0.3996062992125984925, -2.524278215223096478 ) ) ;
#57060 = CARTESIAN_POINT ( 'NONE',  ( 1.325459317585302665, 0.05413385826771626580, -0.4176697321401330321 ) ) ;
#57061 = CARTESIAN_POINT ( 'NONE',  ( -0.5905511811023615998, 0.1771653543307087630, 0.000000000000000000 ) ) ;
#57062 = CARTESIAN_POINT ( 'NONE',  ( 0.2925321140481932369, -0.2925321140481931814, -1.277559055118110187 ) ) ;
#57063 = CARTESIAN_POINT ( 'NONE',  ( -0.9711286089238838626, -0.6046776061558807314, 0.2411417322834647770 ) ) ;
#57064 = CARTESIAN_POINT ( 'NONE',  ( 1.312335958005250269, -0.6046776061558807314, 0.2411417322834647770 ) ) ;
#57065 = CARTESIAN_POINT ( 'NONE',  ( 1.049868766404200349, 0.2306618581243848609, 0.2411417322834645549 ) ) ;
#57066 = CARTESIAN_POINT ( 'NONE',  ( 0.4724409448818899238, -0.1265901696524985298, -0.1115485564304462274 ) ) ;
#57067 = CARTESIAN_POINT ( 'NONE',  ( -1.279527559055116948, -0.4536011799217367080, 0.2665933059059888421 ) ) ;
#57068 = CARTESIAN_POINT ( 'NONE',  ( -0.1998031496062991630, -0.3460692066303959202, -0.7723097112860892732 ) ) ;
#57069 = CARTESIAN_POINT ( 'NONE',  ( 0.3460692066303959757, -0.1998031496062991907, -1.049868766404199460 ) ) ;
#57070 = CARTESIAN_POINT ( 'NONE',  ( 0.3949938075777411073, -0.1058382717557499464, -0.4265091863517062043 ) ) ;
#57071 = CARTESIAN_POINT ( 'NONE',  ( 0.01711686753222834215, 1.062992125984252967, 2.874015748031495843 ) ) ;
#57072 = CARTESIAN_POINT ( 'NONE',  ( 1.259842519685040019, -0.1870078740157480601, -0.3641732283464567677 ) ) ;
#57073 = CARTESIAN_POINT ( 'NONE',  ( 0.7611548556430451917, -0.5023911411419708095, 0.1820866141732285504 ) ) ;
#57074 = CARTESIAN_POINT ( 'NONE',  ( 0.4330708661417329575, -0.6692913385826771977, 8.415575281601705876E-17 ) ) ;
#57075 = CARTESIAN_POINT ( 'NONE',  ( -1.519422763189357539, 0.1377952755905511861, 0.7302211324797360792 ) ) ;
#57076 = CARTESIAN_POINT ( 'NONE',  ( -0.2891555358219909388, -0.2891555358219912164, -1.238188976377952999 ) ) ;
#57077 = CARTESIAN_POINT ( 'NONE',  ( 0.9317585301837276734, -0.004921259842519870586, -0.3153832671262229437 ) ) ;
#57078 = CARTESIAN_POINT ( 'NONE',  ( -0.2165354330708654795, 0.1660481256975885056, 0.3530559997133364547 ) ) ;
#57079 = CARTESIAN_POINT ( 'NONE',  ( -1.266404199475064773, -0.05778040916215560624, -0.4822834645669293319 ) ) ;
#57080 = CARTESIAN_POINT ( 'NONE',  ( 1.023622047244095334, -0.1870078740157479769, 0.4822834645669291653 ) ) ;
#57081 = CARTESIAN_POINT ( 'NONE',  ( -0.3458507752293906723, -0.3458507752293910609, -1.476377952755905554 ) ) ;
#57082 = CARTESIAN_POINT ( 'NONE',  ( -0.7758157084527474989, 0.02791078216816064370, 0.4328096321851915285 ) ) ;
#57083 = ORIENTED_EDGE ( 'NONE', *, *, #76734, .F. ) ;
#57084 = EDGE_LOOP ( 'NONE', ( #42413, #16867, #51000, #66025 ) ) ;
#57085 = CARTESIAN_POINT ( 'NONE',  ( -0.7874015748031489847, -0.1870078740157479769, 0.4822834645669291653 ) ) ;
#57086 = CARTESIAN_POINT ( 'NONE',  ( -0.6233595800524928121, -0.3162353388693409650, -0.4822834645669289433 ) ) ;
#57088 = CARTESIAN_POINT ( 'NONE',  ( -0.6036745406824141069, -0.6046776061558809534, -0.2411417322834644161 ) ) ;
#57087 = CARTESIAN_POINT ( 'NONE',  ( -0.9776902887139098386, 0.1771653543307087075, -0.09757992244046823083 ) ) ;
#57089 = CARTESIAN_POINT ( 'NONE',  ( 0.2493438320209980519, 0.05413385826771666132, 0.4176697321401328100 ) ) ;
#57090 = CARTESIAN_POINT ( 'NONE',  ( -0.5577427821522301654, -0.3162353388693405765, 0.4822834645669290543 ) ) ;
#57091 = CARTESIAN_POINT ( 'NONE',  ( -1.404199475065615932, -0.4281496062992127816, -0.4176697321401328100 ) ) ;
#57092 = CARTESIAN_POINT ( 'NONE',  ( -0.7808398950131225646, -0.05778040916215522460, 0.4822834645669289988 ) ) ;
#57093 = CARTESIAN_POINT ( 'NONE',  ( 0.7808398950131240079, -0.3162353388693405765, 0.4822834645669290543 ) ) ;
#57094 = EDGE_CURVE ( 'NONE', #19150, #55865, #21025, .T. ) ;
#57095 = CARTESIAN_POINT ( 'NONE',  ( -0.3917322834645669549, -0.1049643490035306603, -1.455380577427821676 ) ) ;
#57096 = CARTESIAN_POINT ( 'NONE',  ( -0.8923884514435688198, -0.5023911411419708095, 0.1820866141732285504 ) ) ;
#57097 = ORIENTED_EDGE ( 'NONE', *, *, #17054, .T. ) ;
#57098 = CARTESIAN_POINT ( 'NONE',  ( 0.1058382717557499880, 0.3949938075777411073, -1.253280839895013488 ) ) ;
#57099 = VERTEX_POINT ( 'NONE', #33850 ) ;
#57100 = CARTESIAN_POINT ( 'NONE',  ( -1.312335958005248715, -0.5023911411419708095, -0.1820866141732282451 ) ) ;
#57101 = CARTESIAN_POINT ( 'NONE',  ( -0.8858267716535425107, -0.5400638737290844871, 0.3530559997133364547 ) ) ;
#57102 = CARTESIAN_POINT ( 'NONE',  ( -0.6758530183727028406, 0.2952755905511811885, 0.1292274648535926551 ) ) ;
#57103 = CARTESIAN_POINT ( 'NONE',  ( 0.3996062992125986590, -0.1070741851644053111, -0.2690288713910760632 ) ) ;
#57104 = CARTESIAN_POINT ( 'NONE',  ( -0.9711286089238838626, -0.6046776061558807314, 0.2411417322834647770 ) ) ;
#57105 = CARTESIAN_POINT ( 'NONE',  ( -1.332020997375327642, -0.3162353388693409650, -0.4822834645669289433 ) ) ;
#57106 = CARTESIAN_POINT ( 'NONE',  ( 2.530077726415320249, 2.729661064330337616, -0.5314960629921260393 ) ) ;
#57107 = CARTESIAN_POINT ( 'NONE',  ( -1.666666666666665853, 0.05413385826771626580, -0.4176697321401330321 ) ) ;
#57108 = CIRCLE ( 'NONE', #23486, 0.2165354330708659791 ) ;
#57109 = CARTESIAN_POINT ( 'NONE',  ( 0.3477690288713918276, -0.5511811023622048555, -0.09757992244046775898 ) ) ;
#57110 = CARTESIAN_POINT ( 'NONE',  ( 3.250800423740332512, 2.742781085175769018, 0.5314960629921260393 ) ) ;
#57111 = CARTESIAN_POINT ( 'NONE',  ( -9.594673741351313045E-17, 0.3917322834645670104, 0.07283464566929125084 ) ) ;
#57112 = CARTESIAN_POINT ( 'NONE',  ( 0.1574803149606306130, -0.1870078740157479769, 0.3641732283464567677 ) ) ;
#57113 = CARTESIAN_POINT ( 'NONE',  ( -0.3805774278215216522, 0.05413385826771666132, 0.4176697321401328100 ) ) ;
#57114 = CARTESIAN_POINT ( 'NONE',  ( 1.181102362204724976, -0.1870078740157480879, -0.4822834645669291653 ) ) ;
#57115 = CARTESIAN_POINT ( 'NONE',  ( -0.2887139107611542133, -0.6046776061558809534, -0.2411417322834644161 ) ) ;
#57116 = ORIENTED_EDGE ( 'NONE', *, *, #81979, .F. ) ;
#57117 = CARTESIAN_POINT ( 'NONE',  ( -0.8070866141732276899, 0.1012011053420775880, -0.2882089793578256898 ) ) ;
#57118 = ORIENTED_EDGE ( 'NONE', *, *, #59835, .T. ) ;
#57119 = CARTESIAN_POINT ( 'NONE',  ( -0.3996062992125985480, -7.340648628747423112E-17, -1.375984251968503713 ) ) ;
#57120 = CARTESIAN_POINT ( 'NONE',  ( -0.7611548556430438595, -0.6046776061558809534, -0.2411417322834644161 ) ) ;
#57121 = CARTESIAN_POINT ( 'NONE',  ( 1.502624671916010790, -0.3162353388693409650, -0.4822834645669289433 ) ) ;
#57122 = CARTESIAN_POINT ( 'NONE',  ( -1.095800524934382292, -0.08942795157527998196, 0.3641732283464567121 ) ) ;
#57123 = CARTESIAN_POINT ( 'NONE',  ( -1.437007874015747477, -0.5400638737290844871, 0.3530559997133364547 ) ) ;
#57124 = CARTESIAN_POINT ( 'NONE',  ( -0.4091458600556402980, -0.2362204724409451284, -0.8398950131233595684 ) ) ;
#57125 = LINE ( 'NONE', #56313, #7575 ) ;
#57126 = CARTESIAN_POINT ( 'NONE',  ( 0.3392501089628018884, -0.1958661417322834220, 0.06036745406824151755 ) ) ;
#57127 = CARTESIAN_POINT ( 'NONE',  ( 1.108923884514436686, -0.3162353388693409650, -0.4822834645669289433 ) ) ;
#57128 = CARTESIAN_POINT ( 'NONE',  ( 0.3392501089628018329, 0.1958661417322835607, -1.948162729658792891 ) ) ;
#57129 = CARTESIAN_POINT ( 'NONE',  ( 0.2493438320209980519, 0.05413385826771666132, 0.4176697321401328100 ) ) ;
#57130 = CARTESIAN_POINT ( 'NONE',  ( -1.115485564304461219, -0.004921259842519870586, -0.3153832671262229437 ) ) ;
#57131 = CARTESIAN_POINT ( 'NONE',  ( -0.1771653543307080136, -0.5400638737290844871, 0.3530559997133364547 ) ) ;
#57132 = CARTESIAN_POINT ( 'NONE',  ( -0.4724409448818895907, -0.1265901696524993070, -2.642388451443570041 ) ) ;
#57133 = CARTESIAN_POINT ( 'NONE',  ( -0.6758530183727028406, -0.6692913385826773087, -0.1292274648535924053 ) ) ;
#57134 = CARTESIAN_POINT ( 'NONE',  ( -0.9580052493438311334, -0.4281496062992124485, 0.4176697321401328655 ) ) ;
#57135 = CARTESIAN_POINT ( 'NONE',  ( 0.3949938075777409408, -0.1058382717557499186, -2.393044619422572072 ) ) ;
#57136 = CARTESIAN_POINT ( 'NONE',  ( 0.7480314960629927956, -0.5511811023622047445, 6.969142054262312111E-17 ) ) ;
#57137 = CARTESIAN_POINT ( 'NONE',  ( -0.2821522309711278487, 0.1771653543307087630, 0.09757992244046791164 ) ) ;
#57138 = CARTESIAN_POINT ( 'NONE',  ( 0.6889763779527566800, -0.4536011799217367080, 0.2665933059059888421 ) ) ;
#57139 = CARTESIAN_POINT ( 'NONE',  ( -1.535433070866141225, 0.2952755905511811885, 0.000000000000000000 ) ) ;
#57140 = CARTESIAN_POINT ( 'NONE',  ( 1.535433070866142335, -0.6692913385826771977, 8.415575281601705876E-17 ) ) ;
#57141 = CARTESIAN_POINT ( 'NONE',  ( 0.4790026246719168435, -0.2845877964562161244, -0.3641732283464567121 ) ) ;
#57142 = CARTESIAN_POINT ( 'NONE',  ( -0.6627296587926501115, 0.2952755905511810774, -0.1292274648535930714 ) ) ;
#57143 = CARTESIAN_POINT ( 'NONE',  ( 1.450131233595801428, 0.2952755905511811885, 0.1292274648535926551 ) ) ;
#57144 = CARTESIAN_POINT ( 'NONE',  ( -2.153151837758440212, 1.453715418023200145, 0.4672341690643352363 ) ) ;
#57145 = CARTESIAN_POINT ( 'NONE',  ( -0.1509186351706028884, -0.2845877964562161244, -0.3641732283464567121 ) ) ;
#57146 = CARTESIAN_POINT ( 'NONE',  ( 0.03280839895013198948, 0.2952755905511811885, 0.1292274648535926551 ) ) ;
#57147 = CARTESIAN_POINT ( 'NONE',  ( 0.5052493438320218022, -0.6692913385826773087, -0.1292274648535924053 ) ) ;
#57148 = DIRECTION ( 'NONE',  ( 0.000000000000000000, 0.000000000000000000, -1.000000000000000000 ) ) ;
#57149 = CARTESIAN_POINT ( 'NONE',  ( 1.443569553805774897, 0.1283753931104748280, 0.1820866141732283561 ) ) ;
#57150 = CARTESIAN_POINT ( 'NONE',  ( 0.1312335958005255154, -0.5023911411419708095, 0.1820866141732285504 ) ) ;
#57151 = CARTESIAN_POINT ( 'NONE',  ( -1.384514435695537005, 0.2952755905511811885, 0.1292274648535926551 ) ) ;
#57152 = CARTESIAN_POINT ( 'NONE',  ( -0.5446194225721777693, -0.08942795157527998196, 0.3641732283464567121 ) ) ;
#57153 = CARTESIAN_POINT ( 'NONE',  ( 1.035555078613326518, 5.982513598207969926E-16, 0.3627989612356145033 ) ) ;
#57154 = CARTESIAN_POINT ( 'NONE',  ( -0.9514435695538050464, -0.3162353388693405765, 0.4822834645669290543 ) ) ;
#57155 = CARTESIAN_POINT ( 'NONE',  ( -0.6036745406824141069, -0.6046776061558809534, -0.2411417322834644161 ) ) ;
#57156 = CARTESIAN_POINT ( 'NONE',  ( 4.893765752498283308E-17, -0.3996062992125985480, -0.7854330708661416693 ) ) ;
#57157 = CARTESIAN_POINT ( 'NONE',  ( 0.3392501089628018329, 0.1958661417322835607, -2.420603674540682260 ) ) ;
#57158 = CARTESIAN_POINT ( 'NONE',  ( 0.7086614173228352742, -0.1870078740157480601, -0.3641732283464567677 ) ) ;
#57159 = CARTESIAN_POINT ( 'NONE',  ( -0.5577427821522301654, -0.3162353388693405765, 0.4822834645669290543 ) ) ;
#57160 = CONICAL_SURFACE ( 'NONE', #67957, 3.228346456692913424, 0.7853981633974500554 ) ;
#57161 = CARTESIAN_POINT ( 'NONE',  ( -0.6824146981627288167, 0.2306618581243848609, 0.2411417322834645549 ) ) ;
#57162 = CARTESIAN_POINT ( 'NONE',  ( -0.6955380577427815458, -0.004921259842519576551, 0.3153832671262227771 ) ) ;
#57163 = DIRECTION ( 'NONE',  ( -0.000000000000000000, 1.000000000000000000, -0.000000000000000000 ) ) ;
#57164 = CARTESIAN_POINT ( 'NONE',  ( -0.2624671916010490880, -0.6046776061558807314, 0.2411417322834647770 ) ) ;
#57165 = DIRECTION ( 'NONE',  ( 1.000000000000000000, 3.096699300667737957E-16, -1.692413147294446216E-16 ) ) ;
#57166 = CARTESIAN_POINT ( 'NONE',  ( 1.391076115485564868, -0.6046776061558807314, 0.2411417322834647770 ) ) ;
#57167 = CARTESIAN_POINT ( 'NONE',  ( -0.1265901696524986964, -0.4724409448818899238, -0.7020997375328084100 ) ) ;
#57168 = CARTESIAN_POINT ( 'NONE',  ( -0.2867679344610365444, -0.2867679344610367664, -2.260518003445880719 ) ) ;
#57169 = ORIENTED_EDGE ( 'NONE', *, *, #34817, .F. ) ;
#57170 = CARTESIAN_POINT ( 'NONE',  ( 0.1771653543307086798, 0.000000000000000000, 0.000000000000000000 ) ) ;
#57171 = CARTESIAN_POINT ( 'NONE',  ( -1.286089238845143479, -0.6046776061558807314, 0.2411417322834647770 ) ) ;
#57172 = CARTESIAN_POINT ( 'NONE',  ( -0.7939632545931754048, -0.3162353388693405765, 0.4822834645669290543 ) ) ;
#57173 = CARTESIAN_POINT ( 'NONE',  ( 1.463254593175853824, 0.2952755905511810774, -0.1292274648535930714 ) ) ;
#57174 = CARTESIAN_POINT ( 'NONE',  ( 0.2867679344610365999, -0.2867679344610365444, -1.915354330708661124 ) ) ;
#57175 = DIRECTION ( 'NONE',  ( 0.000000000000000000, 0.000000000000000000, -1.000000000000000000 ) ) ;
#57176 = CARTESIAN_POINT ( 'NONE',  ( 1.148293963254593875, -0.6692913385826771977, 0.1292274648535927661 ) ) ;
#57177 = CARTESIAN_POINT ( 'NONE',  ( 0.05249343832021075018, -0.6046776061558807314, 0.2411417322834647770 ) ) ;
#57178 = DIRECTION ( 'NONE',  ( 0.000000000000000000, 1.000000000000000000, 0.000000000000000000 ) ) ;
#57179 = CARTESIAN_POINT ( 'NONE',  ( 0.1938976377952755792, 0.1938976377952755792, 0.1574803149606299191 ) ) ;
#57180 = CARTESIAN_POINT ( 'NONE',  ( 1.194225721784777594, -0.3690944881889765550, -0.3153832671262227771 ) ) ;
#57181 = CARTESIAN_POINT ( 'NONE',  ( 0.2925321140481932369, -0.2925321140481932369, -1.515748031496062742 ) ) ;
#57182 = ORIENTED_EDGE ( 'NONE', *, *, #10455, .F. ) ;
#57183 = CARTESIAN_POINT ( 'NONE',  ( -0.3917322834645670659, -7.196005306013484475E-17, 0.1213717603336463974 ) ) ;
#57184 = ORIENTED_EDGE ( 'NONE', *, *, #24269, .T. ) ;
#57185 = CARTESIAN_POINT ( 'NONE',  ( 0.4790026246719167324, -0.05778040916215522460, 0.4822834645669289988 ) ) ;
#57186 = CARTESIAN_POINT ( 'NONE',  ( -0.8792650918635160906, 0.05413385826771626580, -0.4176697321401330321 ) ) ;
#57187 = CARTESIAN_POINT ( 'NONE',  ( -1.345144356955379816, -0.3162353388693405765, 0.4822834645669290543 ) ) ;
#57188 = CARTESIAN_POINT ( 'NONE',  ( 0.6758530183727039509, -0.6692913385826771977, 0.1292274648535927661 ) ) ;
#57189 = CARTESIAN_POINT ( 'NONE',  ( 1.660104986876641320, -0.05778040916215522460, 0.4822834645669289988 ) ) ;
#57190 = CARTESIAN_POINT ( 'NONE',  ( 1.528871391076116026, -0.6692913385826773087, -0.1292274648535924053 ) ) ;
#57191 = CARTESIAN_POINT ( 'NONE',  ( -0.2821522309711278487, -0.6692913385826773087, -0.1292274648535924053 ) ) ;
#57192 = CARTESIAN_POINT ( 'NONE',  ( -1.108923884514435132, -0.05778040916215560624, -0.4822834645669293319 ) ) ;
#57193 = CARTESIAN_POINT ( 'NONE',  ( 1.561679790026247350, -0.4281496062992124485, 0.4176697321401328655 ) ) ;
#57194 = CARTESIAN_POINT ( 'NONE',  ( 1.496062992125985147, -0.1870078740157479769, 0.4822834645669291653 ) ) ;
#57195 = CARTESIAN_POINT ( 'NONE',  ( -0.1049643490035307020, 0.3917322834645669549, -0.3136482939632545541 ) ) ;
#57196 = CARTESIAN_POINT ( 'NONE',  ( 1.017060367454068803, -0.2845877964562159024, 0.3641732283464567677 ) ) ;
#57197 = ORIENTED_EDGE ( 'NONE', *, *, #67875, .T. ) ;
#57198 = CARTESIAN_POINT ( 'NONE',  ( 0.1974969037888706369, -0.3420746716998659953, -0.2493438320209974690 ) ) ;
#57199 = ORIENTED_EDGE ( 'NONE', *, *, #23584, .F. ) ;
#57200 = CARTESIAN_POINT ( 'NONE',  ( 0.05905511811023681640, 0.07958543189024071263, -0.2665933059059888421 ) ) ;
#57201 = CIRCLE ( 'NONE', #37092, 2.598425196850393970 ) ;
#57202 = CARTESIAN_POINT ( 'NONE',  ( -0.4724409448818898682, -8.678599364036362592E-17, -2.716535433070865757 ) ) ;
#57203 = CARTESIAN_POINT ( 'NONE',  ( 0.1443569553805781891, -0.4281496062992124485, 0.4176697321401328655 ) ) ;
#57204 = CARTESIAN_POINT ( 'NONE',  ( 0.3280839895013130669, 0.05413385826771666132, 0.4176697321401328100 ) ) ;
#57205 = CARTESIAN_POINT ( 'NONE',  ( -0.6824146981627291497, -0.6046776061558809534, -0.2411417322834644161 ) ) ;
#57206 = CARTESIAN_POINT ( 'NONE',  ( 0.1049643490035303967, 0.3917322834645670659, -1.564979945703099062 ) ) ;
#57207 = CARTESIAN_POINT ( 'NONE',  ( -1.325459317585300889, 0.05413385826771666132, 0.4176697321401328100 ) ) ;
#57208 = CARTESIAN_POINT ( 'NONE',  ( -0.1049643490035307020, 0.3917322834645669549, -2.453412073490813139 ) ) ;
#57209 = CARTESIAN_POINT ( 'NONE',  ( 1.391076115485564868, -0.5023911411419708095, 0.1820866141732285504 ) ) ;
#57210 = CARTESIAN_POINT ( 'NONE',  ( 0.8202099737532814183, -0.6692913385826773087, -0.1292274648535924053 ) ) ;
#57211 = CARTESIAN_POINT ( 'NONE',  ( 0.6036745406824154392, 0.2306618581243847221, -0.2411417322834647770 ) ) ;
#57212 = CARTESIAN_POINT ( 'NONE',  ( 0.3460692066303959757, -0.1998031496062991907, -0.7349081364829396223 ) ) ;
#57213 = CARTESIAN_POINT ( 'NONE',  ( -1.437007874015747477, -0.5400638737290844871, 0.3530559997133364547 ) ) ;
#57214 = CARTESIAN_POINT ( 'NONE',  ( -0.1998031496062994405, 0.3460692066303957537, -0.4048556430446194621 ) ) ;
#57215 = CARTESIAN_POINT ( 'NONE',  ( -0.1070741851644051862, -0.3996062992125986590, -0.1489501312335958227 ) ) ;
#57216 = CARTESIAN_POINT ( 'NONE',  ( -0.2099737532808391705, -0.6046776061558809534, -0.2411417322834644161 ) ) ;
#57217 = CARTESIAN_POINT ( 'NONE',  ( -0.3460692066303960868, 0.1998031496062990242, -2.545931758530183497 ) ) ;
#57218 = CARTESIAN_POINT ( 'NONE',  ( -0.2867679344610365999, 0.2867679344610364889, -1.836614173228346747 ) ) ;
#57219 = CARTESIAN_POINT ( 'NONE',  ( 1.141732283464567566, 0.2952755905511811885, 0.000000000000000000 ) ) ;
#57220 = AXIS2_PLACEMENT_3D ( 'NONE', #54861, #74658, #37159 ) ;
#57221 = CARTESIAN_POINT ( 'NONE',  ( 1.305774278215223960, -0.6692913385826771977, 0.1292274648535927661 ) ) ;
#57222 = CARTESIAN_POINT ( 'NONE',  ( 0.1312335958005257930, 0.1283753931104746893, -0.1820866141732285504 ) ) ;
#57223 = CARTESIAN_POINT ( 'NONE',  ( 0.8005249343832027131, 0.05413385826771666132, 0.4176697321401328100 ) ) ;
#57224 = CARTESIAN_POINT ( 'NONE',  ( -1.157146581871515012E-16, 0.4724409448818898682, -1.336614173228346303 ) ) ;
#57225 = CARTESIAN_POINT ( 'NONE',  ( 0.3215223097112867578, -0.2845877964562161244, -0.3641732283464567121 ) ) ;
#57226 = CARTESIAN_POINT ( 'NONE',  ( 0.2165354330708668673, 0.1660481256975883668, -0.3530559997133364547 ) ) ;
#57227 = CARTESIAN_POINT ( 'NONE',  ( -0.1058382717557503072, 0.3949938075777408852, -0.8707349081364829102 ) ) ;
#57228 = CARTESIAN_POINT ( 'NONE',  ( -1.332020997375327642, -0.3162353388693409650, -0.4822834645669289433 ) ) ;
#57229 = CARTESIAN_POINT ( 'NONE',  ( 0.9776902887139113929, 0.1771653543307087630, 0.09757992244046791164 ) ) ;
#57231 = EDGE_CURVE ( 'NONE', #82979, #50773, #36982, .T. ) ;
#57230 = CARTESIAN_POINT ( 'NONE',  ( -0.2427821522309703550, -0.05778040916215560624, -0.4822834645669293319 ) ) ;
#57232 = CARTESIAN_POINT ( 'NONE',  ( 0.03937007874015833325, -0.5511811023622047445, 6.969142054262312111E-17 ) ) ;
#57233 = DIRECTION ( 'NONE',  ( 0.000000000000000000, 0.000000000000000000, 1.000000000000000000 ) ) ;
#57234 = CARTESIAN_POINT ( 'NONE',  ( -0.2624671916010490880, 0.2306618581243847221, -0.2411417322834647770 ) ) ;
#57235 = CARTESIAN_POINT ( 'NONE',  ( 0.2362204724409456558, -0.1870078740157480601, -0.3641732283464567677 ) ) ;
#57236 = CARTESIAN_POINT ( 'NONE',  ( 4.893765752498283308E-17, -0.3996062992125985480, -2.202755905511811108 ) ) ;
#57237 = CARTESIAN_POINT ( 'NONE',  ( 0.06561679790026316017, -0.4281496062992124485, 0.4176697321401328655 ) ) ;
#57238 = EDGE_CURVE ( 'NONE', #66126, #74865, #38909, .T. ) ;
#57239 = CARTESIAN_POINT ( 'NONE',  ( 1.043307086614173818, 0.07958543189024085140, 0.2665933059059887866 ) ) ;
#57240 = CARTESIAN_POINT ( 'NONE',  ( -0.1694133573824160299, -1.310289619585134409E-15, -0.3627985898453504054 ) ) ;
#57241 = CARTESIAN_POINT ( 'NONE',  ( -0.2755905511811018171, 0.1771653543307087630, 0.000000000000000000 ) ) ;
#57242 = CARTESIAN_POINT ( 'NONE',  ( -0.8005249343832013809, -0.3690944881889763329, 0.3153832671262228327 ) ) ;
#57243 = CARTESIAN_POINT ( 'NONE',  ( -0.3477690288713902178, 0.2952755905511810774, -0.1292274648535930714 ) ) ;
#57244 = CARTESIAN_POINT ( 'NONE',  ( 0.06561679790026316017, 0.05413385826771626580, -0.4176697321401330321 ) ) ;
#57245 = CARTESIAN_POINT ( 'NONE',  ( 1.089238845144357759, -0.004921259842519870586, -0.3153832671262229437 ) ) ;
#57246 = CARTESIAN_POINT ( 'NONE',  ( 0.3245613508421869020, 1.191052126719460036, -1.074140734518187701 ) ) ;
#57247 = CARTESIAN_POINT ( 'NONE',  ( 1.574803149606299746, -0.1870078740157479769, 0.3641732283464567677 ) ) ;
#57248 = CARTESIAN_POINT ( 'NONE',  ( 0.7611548556430454138, 0.2306618581243847221, -0.2411417322834647770 ) ) ;
#57249 = EDGE_CURVE ( 'NONE', #49969, #66560, #62153, .T. ) ;
#57250 = CARTESIAN_POINT ( 'NONE',  ( 0.1181161979004412693, 1.077624259009876573, -1.863928217990339364 ) ) ;
#57251 = CARTESIAN_POINT ( 'NONE',  ( -0.1706036745406816491, -0.4281496062992124485, 0.4176697321401328655 ) ) ;
#57252 = CONICAL_SURFACE ( 'NONE', #21004, 0.1978346456692914035, 0.8726646259971700959 ) ;
#57253 = CARTESIAN_POINT ( 'NONE',  ( -0.2867679344610364334, -0.2867679344610367109, -0.9311023622047245318 ) ) ;
#57255 = CARTESIAN_POINT ( 'NONE',  ( 1.056430446194226658, 0.2952755905511811885, 0.1292274648535926551 ) ) ;
#57254 = AXIS2_PLACEMENT_3D ( 'NONE', #67650, #34834, #16312 ) ;
#57256 = AXIS2_PLACEMENT_3D ( 'NONE', #42301, #15839, #61251 ) ;
#57257 = CARTESIAN_POINT ( 'NONE',  ( 0.6561679790026253567, -0.6046776061558809534, -0.2411417322834644161 ) ) ;
#57258 = EDGE_CURVE ( 'NONE', #45100, #38768, #80568, .T. ) ;
#57259 = CARTESIAN_POINT ( 'NONE',  ( -1.614173228346456712, 2.362204724409448620, -0.1372047244094478091 ) ) ;
#57260 = CARTESIAN_POINT ( 'NONE',  ( 0.3805774278215230400, -0.3690944881889763329, 0.3153832671262228327 ) ) ;
#57261 = CARTESIAN_POINT ( 'NONE',  ( 1.135170603674541256, -0.6692913385826773087, -0.1292274648535924053 ) ) ;
#57262 = CARTESIAN_POINT ( 'NONE',  ( -0.2165354330708654795, -0.4536011799217368745, -0.2665933059059886201 ) ) ;
#57263 = CARTESIAN_POINT ( 'NONE',  ( -0.5314960629921250401, 0.1660481256975885056, 0.3530559997133364547 ) ) ;
#57264 = CARTESIAN_POINT ( 'NONE',  ( 0.8398950131233602345, 0.2306618581243847221, -0.2411417322834647770 ) ) ;
#57265 = CARTESIAN_POINT ( 'NONE',  ( 0.2624671916010504757, -0.6046776061558809534, -0.2411417322834644161 ) ) ;
#57266 =( REPRESENTATION_RELATIONSHIP ('NONE','NONE', #79348, #27201 ) REPRESENTATION_RELATIONSHIP_WITH_TRANSFORMATION ( #41421 )SHAPE_REPRESENTATION_RELATIONSHIP( ) );
#57267 = CARTESIAN_POINT ( 'NONE',  ( -0.9776902887139098386, 0.2952755905511810774, -0.1292274648535930714 ) ) ;
#57268 = CARTESIAN_POINT ( 'NONE',  ( -0.8923884514435688198, 0.1283753931104746893, -0.1820866141732285504 ) ) ;
#57269 = CARTESIAN_POINT ( 'NONE',  ( 0.4330708661417329575, -0.6692913385826771977, 8.415575281601705876E-17 ) ) ;
#57270 = CARTESIAN_POINT ( 'NONE',  ( -1.318897637795274802, -0.5400638737290845981, -0.3530559997133363437 ) ) ;
#57271 = CARTESIAN_POINT ( 'NONE',  ( -0.2296587926509179312, -0.05778040916215522460, 0.4822834645669289988 ) ) ;
#57272 = CARTESIAN_POINT ( 'NONE',  ( 0.6299212598425235621, 2.165354330708662012, -0.9285414500055688691 ) ) ;
#57274 = CARTESIAN_POINT ( 'NONE',  ( 1.200787401574803681, -0.5400638737290845981, -0.3530559997133363437 ) ) ;
#57273 = DIRECTION ( 'NONE',  ( 0.000000000000000000, -1.000000000000000000, 0.000000000000000000 ) ) ;
#57275 = CARTESIAN_POINT ( 'NONE',  ( 1.272965879265092637, -0.4281496062992127816, -0.4176697321401328100 ) ) ;
#57276 = CARTESIAN_POINT ( 'NONE',  ( 4.797336870675656522E-17, -0.3917322834645670104, -2.118110236220472675 ) ) ;
#57278 = CIRCLE ( 'NONE', #41218, 0.1771653543307085410 ) ;
#57277 = CARTESIAN_POINT ( 'NONE',  ( -1.476377952755905110, 0.1660481256975885056, 0.3530559997133364547 ) ) ;
#57279 = CARTESIAN_POINT ( 'NONE',  ( -1.036745406824146176, 0.05413385826771626580, -0.4176697321401330321 ) ) ;
#57280 = CARTESIAN_POINT ( 'NONE',  ( -0.4724409448818895907, -0.1265901696524993070, -0.2034120734908136108 ) ) ;
#57281 = CARTESIAN_POINT ( 'NONE',  ( -0.3420746716998659953, -0.1974969037888706647, -2.729658792650918819 ) ) ;
#57282 = ORIENTED_EDGE ( 'NONE', *, *, #64580, .F. ) ;
#57283 = CARTESIAN_POINT ( 'NONE',  ( 0.09842519685039434474, 0.07958543189024085140, 0.2665933059059887866 ) ) ;
#57284 = CARTESIAN_POINT ( 'NONE',  ( 0.1958661417322834775, 0.3392501089628018884, -1.396325459317585338 ) ) ;
#57285 = CARTESIAN_POINT ( 'NONE',  ( 0.5380577427821529035, 0.05413385826771626580, -0.4176697321401330321 ) ) ;
#57286 = CARTESIAN_POINT ( 'NONE',  ( -0.1938976377952756902, 0.1938976377952756069, 0.09542247959850373717 ) ) ;
#57287 = CARTESIAN_POINT ( 'NONE',  ( 0.000000000000000000, -1.268531780058464091E-17, -0.1937007874015748143 ) ) ;
#57288 = CARTESIAN_POINT ( 'NONE',  ( -0.6627296587926501115, 0.1771653543307087075, -0.09757992244046823083 ) ) ;
#57289 = CARTESIAN_POINT ( 'NONE',  ( 1.010498687664042716, -0.4281496062992124485, 0.4176697321401328655 ) ) ;
#57290 = CARTESIAN_POINT ( 'NONE',  ( 1.056430446194226436, -0.5511811023622048555, -0.09757992244046775898 ) ) ;
#57291 = CARTESIAN_POINT ( 'NONE',  ( -0.05249343832020911260, 0.2306618581243848609, 0.2411417322834645549 ) ) ;
#57292 = CARTESIAN_POINT ( 'NONE',  ( 0.3917322834645669549, 2.398668435337827645E-17, -0.6705843587588433685 ) ) ;
#57293 = CARTESIAN_POINT ( 'NONE',  ( -0.5774278215223089816, -0.6046776061558807314, 0.2411417322834647770 ) ) ;
#57294 = CARTESIAN_POINT ( 'NONE',  ( -1.535433070866141225, 0.1771653543307087630, 0.000000000000000000 ) ) ;
#57295 = CARTESIAN_POINT ( 'NONE',  ( -0.3149606299212590610, -0.1870078740157479769, 0.4822834645669291653 ) ) ;
#57296 = CARTESIAN_POINT ( 'NONE',  ( 1.568241469816273659, -0.05778040916215560624, -0.4822834645669293319 ) ) ;
#57297 = CARTESIAN_POINT ( 'NONE',  ( 0.6399301791983058596, -1.374501131054255944E-15, 0.4445507791589066726 ) ) ;
#57298 = ORIENTED_EDGE ( 'NONE', *, *, #68594, .T. ) ;
#57299 = CARTESIAN_POINT ( 'NONE',  ( 0.1958661417322836718, -0.3392501089628017219, -2.135846087435382401 ) ) ;
#57300 = CARTESIAN_POINT ( 'NONE',  ( 0.5446194225721792126, -0.3162353388693405765, 0.4822834645669290543 ) ) ;
#57301 = ORIENTED_EDGE ( 'NONE', *, *, #25913, .F. ) ;
#57302 = CARTESIAN_POINT ( 'NONE',  ( -0.8267716535433065062, -0.6692913385826771977, 8.415575281601705876E-17 ) ) ;
#57303 = CARTESIAN_POINT ( 'NONE',  ( -1.259842519685038686, -0.1870078740157480879, -0.4822834645669291653 ) ) ;
#57304 = CARTESIAN_POINT ( 'NONE',  ( 0.4921259842519691285, 0.1660481256975885056, 0.3530559997133364547 ) ) ;
#57305 = CARTESIAN_POINT ( 'NONE',  ( -0.1509186351706028884, -0.3162353388693409650, -0.4822834645669289433 ) ) ;
#57306 = CARTESIAN_POINT ( 'NONE',  ( 0.2867679344610365999, -0.2867679344610365444, -1.285433070866141669 ) ) ;
#57307 = CARTESIAN_POINT ( 'NONE',  ( -0.6430446194225716283, -0.4281496062992124485, 0.4176697321401328655 ) ) ;
#57308 = CARTESIAN_POINT ( 'NONE',  ( -0.03937007874015669567, 0.2952755905511811885, 0.000000000000000000 ) ) ;
#57309 = CARTESIAN_POINT ( 'NONE',  ( -0.7480314960629914633, -0.6692913385826771977, 8.415575281601705876E-17 ) ) ;
#57310 = CARTESIAN_POINT ( 'NONE',  ( -0.2690288713910754526, -0.5511811023622046335, 0.09757992244046803654 ) ) ;
#57311 = CARTESIAN_POINT ( 'NONE',  ( -2.362204724409448620, 1.724409448818897461, -2.474278114140802984E-14 ) ) ;
#57312 = CARTESIAN_POINT ( 'NONE',  ( 0.006561679790026889343, -0.05778040916215522460, 0.4822834645669289988 ) ) ;
#57313 = DIRECTION ( 'NONE',  ( 0.000000000000000000, 1.000000000000000000, 0.000000000000000000 ) ) ;
#57314 = EDGE_CURVE ( 'NONE', #24482, #25219, #60232, .T. ) ;
#57315 = CARTESIAN_POINT ( 'NONE',  ( 1.154855643044620184, 0.2306618581243847221, -0.2411417322834647770 ) ) ;
#57316 = CARTESIAN_POINT ( 'NONE',  ( -0.2867679344610364334, -0.2867679344610367109, -2.885826771653543066 ) ) ;
#57317 = EDGE_LOOP ( 'NONE', ( #2048, #26810, #43215, #34866, #29075, #21377 ) ) ;
#57318 = ORIENTED_EDGE ( 'NONE', *, *, #36633, .T. ) ;
#57319 = AXIS2_PLACEMENT_3D ( 'NONE', #13174, #32935, #51856 ) ;
#57320 = CARTESIAN_POINT ( 'NONE',  ( 0.2952755905511819101, 0.1660481256975883668, -0.3530559997133364547 ) ) ;
#57321 = CARTESIAN_POINT ( 'NONE',  ( 0.2427821522309716595, -0.2845877964562161244, -0.3641732283464567121 ) ) ;
#57322 = VECTOR ( 'NONE', #52921, 39.37007874015748143 ) ;
#57323 = AXIS2_PLACEMENT_3D ( 'NONE', #68412, #10344, #11163 ) ;
#57325 = FACE_OUTER_BOUND ( 'NONE', #34687, .T. ) ;
#57324 = CARTESIAN_POINT ( 'NONE',  ( 1.410761154855643795, -0.08942795157528024563, -0.3641732283464568787 ) ) ;
#57326 = CARTESIAN_POINT ( 'NONE',  ( 0.1049643490035303689, 0.3917322834645670104, -1.180446194225722056 ) ) ;
#57327 = CARTESIAN_POINT ( 'NONE',  ( 0.4724409448818896462, 0.1265901696524990294, -0.2014435695538057958 ) ) ;
#57328 = CARTESIAN_POINT ( 'NONE',  ( 1.463254593175853824, -0.5511811023622046335, 0.09757992244046803654 ) ) ;
#57329 = CARTESIAN_POINT ( 'NONE',  ( 1.601049868766404982, 0.2306618581243848609, 0.2411417322834645549 ) ) ;
#57330 = CARTESIAN_POINT ( 'NONE',  ( 4.893765752498283308E-17, -0.3996062992125985480, -2.675196850393700920 ) ) ;
#57331 = CARTESIAN_POINT ( 'NONE',  ( 0.5446194225721792126, -0.05778040916215560624, -0.4822834645669293319 ) ) ;
#57332 = CARTESIAN_POINT ( 'NONE',  ( -1.154855643044618851, 0.2306618581243848609, 0.2411417322834645549 ) ) ;
#57333 = CARTESIAN_POINT ( 'NONE',  ( -1.003937007874015297, -0.5400638737290845981, -0.3530559997133363437 ) ) ;
#57334 = CARTESIAN_POINT ( 'NONE',  ( 0.4133858267716541968, -0.5400638737290845981, -0.3530559997133363437 ) ) ;
#57335 = CARTESIAN_POINT ( 'NONE',  ( 0.8398950131233602345, 0.2306618581243847221, -0.2411417322834647770 ) ) ;
#57336 = CARTESIAN_POINT ( 'NONE',  ( 1.351706036745407680, -0.004921259842519576551, 0.3153832671262227771 ) ) ;
#57337 = CARTESIAN_POINT ( 'NONE',  ( 0.7742782152230979209, -0.004921259842519870586, -0.3153832671262229437 ) ) ;
#57338 = CARTESIAN_POINT ( 'NONE',  ( -0.9055118110236215490, -0.6692913385826771977, 8.415575281601705876E-17 ) ) ;
#57339 = B_SPLINE_CURVE_WITH_KNOTS ( 'NONE', 3,
 ( #10367, #61699, #62520, #81898, #9940, #61275, #68841 ),
 .UNSPECIFIED., .F., .F.,
 ( 4, 3, 4 ),
 ( 3.469446951953614189E-17, 0.001246232571205268744, 0.002492492258783276290 ),
 .UNSPECIFIED. ) ;
#57340 = CARTESIAN_POINT ( 'NONE',  ( -0.1998031496062991630, -0.3460692066303959202, -0.2998687664041995160 ) ) ;
#57341 = CARTESIAN_POINT ( 'NONE',  ( -1.587926509186350810, -0.004921259842519870586, -0.3153832671262229437 ) ) ;
#57342 = CARTESIAN_POINT ( 'NONE',  ( -0.1958661417322834220, -0.3392501089628018884, -0.2152230971128608339 ) ) ;
#57344 = CARTESIAN_POINT ( 'NONE',  ( -0.2239781325220785713, 1.118900601684390761, 1.901750336123934737 ) ) ;
#57343 = CARTESIAN_POINT ( 'NONE',  ( 0.7283464566929143125, 0.1660481256975885056, 0.3530559997133364547 ) ) ;
#57345 = CARTESIAN_POINT ( 'NONE',  ( -1.404199475065615932, -0.004921259842519576551, 0.3153832671262227771 ) ) ;
#57346 = CARTESIAN_POINT ( 'NONE',  ( -0.07217847769028787330, -0.05778040916215522460, 0.4822834645669289988 ) ) ;
#57347 = CARTESIAN_POINT ( 'NONE',  ( 0.8267716535433077274, 0.1771653543307087630, 0.000000000000000000 ) ) ;
#57348 = CARTESIAN_POINT ( 'NONE',  ( 0.9973753280839902091, -0.6046776061558807314, 0.2411417322834647770 ) ) ;
#57349 = DIRECTION ( 'NONE',  ( -0.000000000000000000, -1.000000000000000000, -0.000000000000000000 ) ) ;
#57350 = CARTESIAN_POINT ( 'NONE',  ( -0.6102362204724400829, 0.07958543189024085140, 0.2665933059059887866 ) ) ;
#57351 = CARTESIAN_POINT ( 'NONE',  ( -0.4396325459317579898, 0.2952755905511811885, 0.1292274648535926551 ) ) ;
#57352 = CARTESIAN_POINT ( 'NONE',  ( -1.627296587926508442, 0.1283753931104748280, 0.1820866141732283561 ) ) ;
#57353 = CARTESIAN_POINT ( 'NONE',  ( -0.9514435695538050464, -0.3162353388693405765, 0.4822834645669290543 ) ) ;
#57354 = CARTESIAN_POINT ( 'NONE',  ( 1.062992125984252745, 0.2952755905511811885, 0.000000000000000000 ) ) ;
#57355 = CARTESIAN_POINT ( 'NONE',  ( -0.1049643490035307158, 0.3917322834645670104, -0.7907017304800020296 ) ) ;
#57356 = CARTESIAN_POINT ( 'NONE',  ( -1.482939632545930975, -0.004921259842519576551, 0.3153832671262227771 ) ) ;
#57357 = EDGE_CURVE ( 'NONE', #46955, #79849, #56186, .T. ) ;
#57358 = CARTESIAN_POINT ( 'NONE',  ( 1.038214557251247117, 1.325842827038092420, 0.4257573143050834008 ) ) ;
#57359 = CARTESIAN_POINT ( 'NONE',  ( 1.056430446194226436, -0.6692913385826773087, -0.1292274648535924053 ) ) ;
#57360 = CARTESIAN_POINT ( 'NONE',  ( -0.1265901696524993347, 0.4724409448818895907, -2.445538057742782101 ) ) ;
#57361 = PLANE ( 'NONE',  #41427 ) ;
#57362 = CARTESIAN_POINT ( 'NONE',  ( 1.679790026246720025, 0.2306618581243848609, 0.2411417322834645549 ) ) ;
#57363 = CARTESIAN_POINT ( 'NONE',  ( -0.8398950131233589023, -0.5023911411419708095, -0.1820866141732282451 ) ) ;
#57364 = B_SPLINE_CURVE_WITH_KNOTS ( 'NONE', 3,
 ( #1881, #71750, #58692, #14524 ),
 .UNSPECIFIED., .F., .F.,
 ( 4, 4 ),
 ( 1.027584591209733963E-14, 0.001730108991789992097 ),
 .UNSPECIFIED. ) ;
#57366 = CARTESIAN_POINT ( 'NONE',  ( 1.594488188976378673, -0.4536011799217368745, -0.2665933059059886201 ) ) ;
#57365 =( BOUNDED_SURFACE ( )  B_SPLINE_SURFACE ( 1, 2, ( 
 ( #20332, #14863, #71680, #8543, #14032, #59872, #7715, #33383, #34209, #13609, #20754, #59046, #64945, #46404, #72098, #72925, #40938, #14456, #33794, #53551, #27472, #66617, #8955, #34629, #60293, #2643, #7285, #75006, #68280, #11017, #42579, #36674, #4688, #81321, #49305, #60702, #74177, #35869, #15696, #41353, #67034, #22818, #55610, #4284, #16938, #54799, #16523, #3051, #61535, #29946, #30361, #9366, #35037, #28717, #16104, #22411, #23634, #3880, #61114, #36272, #3466, #54380, #62350, #79674, #23223, #17353, #42981, #80090, #55202, #48067, #80910, #73770, #61943, #41749, #67444, #48893, #21991, #29132, #9777, #47652, #73348, #68676, #74594, #29539, #35449, #10615, #80502, #48475, #42168, #67863, #10200, #69902, #76639, #64422, #12669, #25691, #12256, #57255, #56029, #38746, #24046, #30778, #31181, #45040, #37091, #56439, #82142, #24457, #5111, #62777, #50123, #70314, #37913, #82956, #44619, #75822, #18164, #38329, #18569, #18970, #25274, #43796, #31597, #64003, #6344, #63590, #44212, #69501, #32016, #37503, #24862, #56846, #50942, #63178, #57676, #11436, #11850, #51352, #38, #77055, #19388, #5925, #5516, #70740, #82544, #50530, #13093, #81737, #6757, #49717, #75413, #76235, #17757, #43387, #69088, #32851, #72416, #58520, #64842, #1712, #66518, #39585, #885, #15176, #32429, #21477, #27367, #65699, #79160, #8029, #72826, #40833, #65274, #7612, #26952, #46305, #53028, #58092, #14765, #2124, #71999, #33692, #457, #26113, #51774, #7180, #33284, #47135, #13501, #26543, #52196, #77900, #20231, #39157, #45879, #46724, #14354, #59353, #21065, #71577, #13928, #40421, #78321, #78741, #66102, #58945, #8438, #34108, #59769, #40012, #20652, #1303, #27791, #52615, #53452, #77478, #19814, #45463, #71161, #47553, #34943, #61845, #10100, #10518, #2544, #41658, #67349, #36172, #29849, #41253, #9272, #16840, #9682, #74077, #29444, #4186, #55512, #73245, #3781, #81220, #80812, #23536, #55103, #49205, #17255, #74907, #42883, #15594, #3366, #48378, #28202, #53861, #79573, #35353, #68177, #42474, #23127, #61015, #29030, #66940, #16423, #8850, #34529, #21889, #60606, #2955, #28620, #54278, #60193, #67764, #54699, #80407, #42069, #22719, #79994, #22308, #47969, #73670, #16012, #35764, #48795, #61432, #74493, #82859, #36576, #18876, #11758, #56752, #37413, #50030, #25180, #4591, #62255, #69812, #63085, #82047, #83269, #30262, #55926, #81641, #82452, #36995, #76548, #24767, #31085, #75727, #23950, #5016, #18067, #12161, #43701, #57578, #5827, #75312, #49618, #50435, #30685, #11336, #68987, #24360, #17659, #43290, #62675, #44525, #70213, #12569, #25592, #31916, #38227, #63904, #5423, #69405, #6240, #51255, #37817, #76137, #68578, #63493, #18478, #56346, #44120, #31500, #76957, #57159, #19285, #50848, #10919, #7081, #32752, #78221, #52930, #20554, #65597, #22103, #26014, #77801, #46206, #65173, #44936, #19707, #357, #64323, #80204, #77375, #47763, #57993, #58419, #27269, #64743, #51672, #39910, #3165, #70633, #41462, #52513, #35149, #33591, #7509, #15812, #73461, #79787, #45365, #67146, #71900, #1204, #26854, #71061, #26440, #13405, #39060, #778, #12990, #9476, #58846, #52092, #20133, #60813, #28829, #45781, #71480, #54493, #13827, #14251, #7930, #38645, #6659, #39486, #59256, #32331, #1613, #33178, #68793, #62890, #30889, #24164, #75532, #3580, #17053, #62061, #41866, #67560, #9893, #49010, #81852, #30483, #43097, #81027, #42694, #29247, #4400, #56149, #56557, #35563, #61227, #54911, #42277, #48594, #49833, #30067, #3993, #62472, #29657, #80617, #5226, #22521, #49426, #17872, #69206, #22929, #81438, #74291, #23753, #16636, #4807, #67974, #10317, #75121, #48183, #55319, #35982, #73880, #16219, #11554, #17466, #55730, #37211, #11138, #61652, #23340, #74708, #68391, #10730, #36387, #36797, #43506, #38858, #51893, #12788, #155, #82257, #64960, #50243, #56964, #57377, #71274, #63294, #82662, #24976, #50649, #31300, #5633, #76352, #13212, #64127, #25808, #70861, #18683, #44327, #64539, #44735, #45157, #51469, #70019, #57789, #6876, #32545, #38444, #70431, #12371, #58209, #63705 ),
 ( #32967, #38030, #576, #11963, #6045, #26229, #31717, #83072, #77171, #39275, #24576, #77598, #6462, #13623, #19932, #32132, #45581, #7297, #75939, #25392, #18280, #19503, #43921, #69618, #51056, #76756, #19087, #37619, #59058, #9378, #8967, #72527, #65808, #78439, #53974, #34223, #8141, #27484, #8555, #53142, #47664, #78017, #22004, #15707, #79687, #73359, #21586, #33396, #33806, #72938, #26657, #34641, #1824, #46835, #78854, #40120, #15290, #20345, #52310, #59884, #21180, #72110, #41364, #45997, #71693, #14045, #14877, #27069, #66629, #40537, #66216, #59471, #39701, #20766, #2238, #27903, #1413, #52728, #67045, #58634, #53563, #60306, #1002, #65393, #79272, #7727, #47249, #46417, #40950, #14468, #2655, #28314, #69098, #42179, #3476, #17767, #35048, #24058, #29958, #68291, #81747, #10627, #75425, #43399, #67873, #10211, #29551, #48905, #55623, #60713, #75018, #4699, #74606, #36283, #3062, #28730, #54391, #9789, #35879, #49727, #16116, #35460, #61125, #29143, #67455, #41762, #54809, #80513, #81332, #80102, #22421, #30372, #42591, #48078, #23646, #80921, #56039, #62361, #42992, #22828, #17364, #61956, #16949, #4295, #48487, #16534, #74188, #61547, #3891, #73780, #68687, #49317, #55214, #23236, #11029, #36686, #44223, #63602, #44630, #5938, #469, #30788, #58103, #51786, #6769, #26125, #57687, #69512, #18580, #25703, #62787, #45051, #37925, #82967, #31608, #76246, #51363, #56451, #5121, #12682, #57269, #24874, #77490, #82154, #24469, #50136, #25285, #63189, #19400, #50953, #76650, #69913, #75834, #12267, #38340, #19825, #45475, #11446, #32027, #18175, #43808, #18982, #56859, #37514, #11861, #50542, #5529, #31193, #82556, #70752, #13103, #38757, #37102, #70326, #64434, #32441, #64015, #6356, #49, #77067, #72429, #8042, #71172, #14779, #27381, #64854, #39170, #77912, #2556, #46737, #53873, #7192, #898, #33297, #58957, #21079, #79172, #40434, #8450, #47148, #52208, #20665, #66115, #33705, #13513, #45892, #26555, #32864, #21901, #20243, #72838, #71589, #1315, #53464, #59366, #14367, #52629, #27804, #58532, #13941, #34121, #40024, #26964, #28214, #39598, #65287, #7625, #1724, #78334, #21489, #53042, #78754, #46318, #72011, #65712, #59782, #60206, #34540, #79588, #2136, #15188, #40845, #66531, #8862, #73683, #47983, #3379, #66952, #2968, #41266, #55524, #23549, #81233, #36588, #10931, #49217, #74923, #67776, #48390, #17267, #42896, #48807, #10115, #47565, #74506, #3793, #9284, #15606, #54291, #62266, #23138, #30275, #34955, #60618, #9695, #35365, #80824, #68590, #16853, #68191, #4603, #28634, #80419, #42488, #35776, #73258, #22320, #80007, #16023, #81653, #41670, #55938, #67361, #61030, #29862, #29042, #54713, #10530, #22731, #74089, #16436, #55115, #42081, #36185, #61446, #29457, #61857, #4198, #24372, #6253, #82870, #63508, #5839, #82058, #5436, #5028, #50043, #75738, #58006, #57592, #37831, #31096, #43714, #19300, #25194, #56764, #76149, #57172, #18489, #13003, #43301, #70648, #64336, #44951, #38659, #70228, #18079, #82463, #38241, #75324, #83282, #50447, #50860, #31513, #17670, #68998, #30696, #6673, #76560, #32345, #11350, #37008, #69416, #11770, #18888, #31930, #44537, #12582, #25605, #56360, #24779, #63917, #44132, #23964, #37424, #62686, #63097, #49630, #69824, #51268, #12173, #76970, #66016, #20145, #7094, #78655, #40744, #26026, #79075, #7942, #72739, #72331, #46218, #53365, #27701, #8352, #793, #34020, #59267, #39922, #65612, #58431, #65186, #64755, #26452, #52106, #34438, #59680, #14264, #7522, #45794, #21391, #1624, #33191, #52527, #33604, #78233, #15086, #19720, #47047, #66428, #8763, #371, #46635, #77814, #58859, #14679, #51686, #2036, #26866, #71914, #20567, #1217, #40335, #45378, #77388, #27281, #52941, #13840, #71075, #13417, #39074, #32764, #20976, #71492, #39498, #73989, #22631, #41571, #15503, #35262, #3692, #49116, #23451, #74821, #80725, #66850, #41161, #48292, #22218, #2866, #60517, #15924, #79483, #9183, #53770, #68086, #36088, #10431, #17166, #42800, #61759, #4097, #80316, #60927, #29765, #55427, #61339, #16336, #60104, #81135 ) ),
 .UNSPECIFIED., .F., .F., .F. ) 
 B_SPLINE_SURFACE_WITH_KNOTS ( ( 2, 2 ),
 ( 3, 2, 2, 2, 2, 2, 2, 2, 2, 2, 2, 2, 2, 2, 2, 2, 2, 2, 2, 2, 2, 2, 2, 2, 2, 2, 2, 2, 2, 2, 2, 2, 2, 2, 2, 2, 2, 2, 2, 2, 2, 2, 2, 2, 2, 2, 2, 2, 2, 2, 2, 2, 2, 2, 2, 2, 2, 2, 2, 2, 2, 2, 2, 2, 2, 2, 2, 2, 2, 2, 2, 2, 2, 2, 2, 2, 2, 2, 2, 2, 2, 2, 2, 2, 2, 2, 2, 2, 2, 2, 2, 2, 2, 2, 2, 2, 2, 2, 2, 2, 2, 2, 2, 2, 2, 2, 2, 2, 2, 2, 2, 2, 2, 2, 2, 2, 2, 2, 2, 2, 2, 2, 2, 2, 2, 2, 2, 2, 2, 2, 2, 2, 2, 2, 2, 2, 2, 2, 2, 2, 2, 2, 2, 2, 2, 2, 2, 2, 2, 2, 2, 2, 2, 2, 2, 2, 2, 2, 2, 2, 2, 2, 2, 2, 2, 2, 2, 2, 2, 2, 2, 2, 2, 2, 2, 2, 2, 2, 2, 2, 2, 2, 2, 2, 2, 2, 2, 2, 2, 2, 2, 2, 2, 2, 2, 2, 2, 2, 2, 2, 2, 2, 2, 2, 2, 2, 2, 2, 2, 2, 2, 2, 2, 2, 2, 2, 2, 2, 2, 2, 2, 2, 2, 2, 2, 2, 2, 2, 2, 2, 2, 2, 2, 2, 2, 2, 2, 2, 2, 2, 2, 2, 2, 2, 2, 2, 2, 2, 2, 2, 2, 2, 2, 2, 2, 3 ),
 ( 0.000000000000000000, 1.000000000000000000 ),
 ( 0.000000000000000000, 0.003787878787878787984, 0.007575757575757575968, 0.01136363636363636395, 0.01515151515151515194, 0.01893939393939393992, 0.02272727272727272790, 0.02651515151515151589, 0.03030303030303030387, 0.03409090909090908839, 0.03787878787878787984, 0.04166666666666666435, 0.04545454545454545581, 0.04924242424242424032, 0.05303030303030303177, 0.05681818181818181629, 0.06060606060606060774, 0.06439393939393939226, 0.06818181818181817677, 0.07196969696969697516, 0.07575757575757575968, 0.07954545454545454419, 0.08333333333333332871, 0.08712121212121212710, 0.09090909090909091161, 0.09469696969696969613, 0.09848484848484848064, 0.1022727272727272790, 0.1060606060606060635, 0.1098484848484848481, 0.1136363636363636326, 0.1174242424242424310, 0.1212121212121212155, 0.1250000000000000000, 0.1287878787878787845, 0.1325757575757575690, 0.1363636363636363535, 0.1401515151515151381, 0.1439393939393939503, 0.1477272727272727348, 0.1515151515151515194, 0.1553030303030303039, 0.1590909090909090884, 0.1628787878787878729, 0.1666666666666666574, 0.1704545454545454419, 0.1742424242424242542, 0.1780303030303030387, 0.1818181818181818232, 0.1856060606060606077, 0.1893939393939393923, 0.1931818181818181768, 0.1969696969696969613, 0.2007575757575757458, 0.2045454545454545581, 0.2083333333333333426, 0.2121212121212121271, 0.2159090909090909116, 0.2196969696969696961, 0.2234848484848484806, 0.2272727272727272652, 0.2310606060606060497, 0.2348484848484848619, 0.2386363636363636465, 0.2424242424242424310, 0.2462121212121212155, 0.2500000000000000000, 0.2537878787878787845, 0.2575757575757575690, 0.2613636363636363535, 0.2651515151515151381, 0.2689393939393939226, 0.2727272727272727071, 0.2765151515151514916, 0.2803030303030302761, 0.2840909090909091161, 0.2878787878787879007, 0.2916666666666666852, 0.2954545454545454697, 0.2992424242424242542, 0.3030303030303030387, 0.3068181818181818232, 0.3106060606060606077, 0.3143939393939393923, 0.3181818181818181768, 0.3219696969696969613, 0.3257575757575757458, 0.3295454545454545303, 0.3333333333333333148, 0.3371212121212120993, 0.3409090909090908839, 0.3446969696969697239, 0.3484848484848485084, 0.3522727272727272929, 0.3560606060606060774, 0.3598484848484848619, 0.3636363636363636465, 0.3674242424242424310, 0.3712121212121212155, 0.3750000000000000000, 0.3787878787878787845, 0.3825757575757575690, 0.3863636363636363535, 0.3901515151515151381, 0.3939393939393939226, 0.3977272727272727071, 0.4015151515151514916, 0.4053030303030302761, 0.4090909090909091161, 0.4128787878787879007, 0.4166666666666666852, 0.4204545454545454697, 0.4242424242424242542, 0.4280303030303030387, 0.4318181818181818232, 0.4356060606060606077, 0.4393939393939393923, 0.4431818181818181768, 0.4469696969696969613, 0.4507575757575757458, 0.4545454545454545303, 0.4583333333333333148, 0.4621212121212120993, 0.4659090909090908839, 0.4696969696969697239, 0.4734848484848485084, 0.4772727272727272929, 0.4810606060606060774, 0.4848484848484848619, 0.4886363636363636465, 0.4924242424242424310, 0.4962121212121212155, 0.5000000000000000000, 0.5037878787878787845, 0.5075757575757575690, 0.5113636363636363535, 0.5151515151515151381, 0.5189393939393939226, 0.5227272727272727071, 0.5265151515151514916, 0.5303030303030302761, 0.5340909090909090606, 0.5378787878787878451, 0.5416666666666666297, 0.5454545454545454142, 0.5492424242424241987, 0.5530303030303029832, 0.5568181818181817677, 0.5606060606060605522, 0.5643939393939394478, 0.5681818181818182323, 0.5719696969696970168, 0.5757575757575758013, 0.5795454545454545858, 0.5833333333333333703, 0.5871212121212121549, 0.5909090909090909394, 0.5946969696969697239, 0.5984848484848485084, 0.6022727272727272929, 0.6060606060606060774, 0.6098484848484848619, 0.6136363636363636465, 0.6174242424242424310, 0.6212121212121212155, 0.6250000000000000000, 0.6287878787878787845, 0.6325757575757575690, 0.6363636363636363535, 0.6401515151515151381, 0.6439393939393939226, 0.6477272727272727071, 0.6515151515151514916, 0.6553030303030302761, 0.6590909090909090606, 0.6628787878787878451, 0.6666666666666666297, 0.6704545454545454142, 0.6742424242424241987, 0.6780303030303029832, 0.6818181818181817677, 0.6856060606060605522, 0.6893939393939394478, 0.6931818181818182323, 0.6969696969696970168, 0.7007575757575758013, 0.7045454545454545858, 0.7083333333333333703, 0.7121212121212121549, 0.7159090909090909394, 0.7196969696969697239, 0.7234848484848485084, 0.7272727272727272929, 0.7310606060606060774, 0.7348484848484848619, 0.7386363636363636465, 0.7424242424242424310, 0.7462121212121212155, 0.7500000000000000000, 0.7537878787878787845, 0.7575757575757575690, 0.7613636363636363535, 0.7651515151515151381, 0.7689393939393939226, 0.7727272727272727071, 0.7765151515151514916, 0.7803030303030302761, 0.7840909090909090606, 0.7878787878787878451, 0.7916666666666666297, 0.7954545454545454142, 0.7992424242424241987, 0.8030303030303029832, 0.8068181818181817677, 0.8106060606060605522, 0.8143939393939394478, 0.8181818181818182323, 0.8219696969696970168, 0.8257575757575758013, 0.8295454545454545858, 0.8333333333333333703, 0.8371212121212121549, 0.8409090909090909394, 0.8446969696969697239, 0.8484848484848485084, 0.8522727272727272929, 0.8560606060606060774, 0.8598484848484848619, 0.8636363636363636465, 0.8674242424242424310, 0.8712121212121212155, 0.8750000000000000000, 0.8787878787878787845, 0.8825757575757575690, 0.8863636363636363535, 0.8901515151515151381, 0.8939393939393939226, 0.8977272727272727071, 0.9015151515151514916, 0.9053030303030302761, 0.9090909090909090606, 0.9128787878787878451, 0.9166666666666666297, 0.9204545454545454142, 0.9242424242424241987, 0.9280303030303029832, 0.9318181818181817677, 0.9356060606060605522, 0.9393939393939394478, 0.9431818181818182323, 0.9469696969696970168, 0.9507575757575758013, 0.9545454545454545858, 0.9583333333333333703, 0.9621212121212121549, 0.9659090909090909394 ),
 .UNSPECIFIED. ) 
 GEOMETRIC_REPRESENTATION_ITEM ( )  RATIONAL_B_SPLINE_SURFACE ( (
 ( 1.000000000000000000, 0.9659258262890683122, 1.000000000000000000, 0.9659258262890683122, 1.000000000000000000, 0.9659258262890683122, 1.000000000000000000, 0.9659258262890683122, 1.000000000000000000, 0.9659258262890683122, 1.000000000000000000, 0.9659258262890683122, 1.000000000000000000, 0.9659258262890683122, 1.000000000000000000, 0.9659258262890683122, 1.000000000000000000, 0.9659258262890683122, 1.000000000000000000, 0.9659258262890683122, 1.000000000000000000, 0.9659258262890683122, 1.000000000000000000, 0.9659258262890683122, 1.000000000000000000, 0.9659258262890683122, 1.000000000000000000, 0.9659258262890683122, 1.000000000000000000, 0.9659258262890683122, 1.000000000000000000, 0.9659258262890683122, 1.000000000000000000, 0.9659258262890683122, 1.000000000000000000, 0.9659258262890683122, 1.000000000000000000, 0.9659258262890683122, 1.000000000000000000, 0.9659258262890683122, 1.000000000000000000, 0.9659258262890683122, 1.000000000000000000, 0.9659258262890683122, 1.000000000000000000, 0.9659258262890683122, 1.000000000000000000, 0.9659258262890683122, 1.000000000000000000, 0.9659258262890683122, 1.000000000000000000, 0.9659258262890683122, 1.000000000000000000, 0.9659258262890683122, 1.000000000000000000, 0.9659258262890683122, 1.000000000000000000, 0.9659258262890683122, 1.000000000000000000, 0.9659258262890683122, 1.000000000000000000, 0.9659258262890683122, 1.000000000000000000, 0.9659258262890683122, 1.000000000000000000, 0.9659258262890683122, 1.000000000000000000, 0.9659258262890683122, 1.000000000000000000, 0.9659258262890683122, 1.000000000000000000, 0.9659258262890683122, 1.000000000000000000, 0.9659258262890683122, 1.000000000000000000, 0.9659258262890683122, 1.000000000000000000, 0.9659258262890683122, 1.000000000000000000, 0.9659258262890683122, 1.000000000000000000, 0.9659258262890683122, 1.000000000000000000, 0.9659258262890683122, 1.000000000000000000, 0.9659258262890683122, 1.000000000000000000, 0.9659258262890683122, 1.000000000000000000, 0.9659258262890683122, 1.000000000000000000, 0.9659258262890683122, 1.000000000000000000, 0.9659258262890683122, 1.000000000000000000, 0.9659258262890683122, 1.000000000000000000, 0.9659258262890683122, 1.000000000000000000, 0.9659258262890683122, 1.000000000000000000, 0.9659258262890683122, 1.000000000000000000, 0.9659258262890683122, 1.000000000000000000, 0.9659258262890683122, 1.000000000000000000, 0.9659258262890683122, 1.000000000000000000, 0.9659258262890683122, 1.000000000000000000, 0.9659258262890683122, 1.000000000000000000, 0.9659258262890683122, 1.000000000000000000, 0.9659258262890683122, 1.000000000000000000, 0.9659258262890683122, 1.000000000000000000, 0.9659258262890683122, 1.000000000000000000, 0.9659258262890683122, 1.000000000000000000, 0.9659258262890683122, 1.000000000000000000, 0.9659258262890683122, 1.000000000000000000, 0.9659258262890683122, 1.000000000000000000, 0.9659258262890683122, 1.000000000000000000, 0.9659258262890683122, 1.000000000000000000, 0.9659258262890683122, 1.000000000000000000, 0.9659258262890683122, 1.000000000000000000, 0.9659258262890683122, 1.000000000000000000, 0.9659258262890683122, 1.000000000000000000, 0.9659258262890683122, 1.000000000000000000, 0.9659258262890683122, 1.000000000000000000, 0.9659258262890683122, 1.000000000000000000, 0.9659258262890683122, 1.000000000000000000, 0.9659258262890683122, 1.000000000000000000, 0.9659258262890683122, 1.000000000000000000, 0.9659258262890683122, 1.000000000000000000, 0.9659258262890683122, 1.000000000000000000, 0.9659258262890683122, 1.000000000000000000, 0.9659258262890683122, 1.000000000000000000, 0.9659258262890683122, 1.000000000000000000, 0.9659258262890683122, 1.000000000000000000, 0.9659258262890683122, 1.000000000000000000, 0.9659258262890683122, 1.000000000000000000, 0.9659258262890683122, 1.000000000000000000, 0.9659258262890683122, 1.000000000000000000, 0.9659258262890683122, 1.000000000000000000, 0.9659258262890683122, 1.000000000000000000, 0.9659258262890683122, 1.000000000000000000, 0.9659258262890683122, 1.000000000000000000, 0.9659258262890683122, 1.000000000000000000, 0.9659258262890683122, 1.000000000000000000, 0.9659258262890683122, 1.000000000000000000, 0.9659258262890683122, 1.000000000000000000, 0.9659258262890683122, 1.000000000000000000, 0.9659258262890683122, 1.000000000000000000, 0.9659258262890683122, 1.000000000000000000, 0.9659258262890683122, 1.000000000000000000, 0.9659258262890683122, 1.000000000000000000, 0.9659258262890683122, 1.000000000000000000, 0.9659258262890683122, 1.000000000000000000, 0.9659258262890683122, 1.000000000000000000, 0.9659258262890683122, 1.000000000000000000, 0.9659258262890683122, 1.000000000000000000, 0.9659258262890683122, 1.000000000000000000, 0.9659258262890683122, 1.000000000000000000, 0.9659258262890683122, 1.000000000000000000, 0.9659258262890683122, 1.000000000000000000, 0.9659258262890683122, 1.000000000000000000, 0.9659258262890683122, 1.000000000000000000, 0.9659258262890683122, 1.000000000000000000, 0.9659258262890683122, 1.000000000000000000, 0.9659258262890683122, 1.000000000000000000, 0.9659258262890683122, 1.000000000000000000, 0.9659258262890683122, 1.000000000000000000, 0.9659258262890683122, 1.000000000000000000, 0.9659258262890683122, 1.000000000000000000, 0.9659258262890683122, 1.000000000000000000, 0.9659258262890683122, 1.000000000000000000, 0.9659258262890683122, 1.000000000000000000, 0.9659258262890683122, 1.000000000000000000, 0.9659258262890683122, 1.000000000000000000, 0.9659258262890683122, 1.000000000000000000, 0.9659258262890683122, 1.000000000000000000, 0.9659258262890683122, 1.000000000000000000, 0.9659258262890683122, 1.000000000000000000, 0.9659258262890683122, 1.000000000000000000, 0.9659258262890683122, 1.000000000000000000, 0.9659258262890683122, 1.000000000000000000, 0.9659258262890683122, 1.000000000000000000, 0.9659258262890683122, 1.000000000000000000, 0.9659258262890683122, 1.000000000000000000, 0.9659258262890683122, 1.000000000000000000, 0.9659258262890683122, 1.000000000000000000, 0.9659258262890683122, 1.000000000000000000, 0.9659258262890683122, 1.000000000000000000, 0.9659258262890683122, 1.000000000000000000, 0.9659258262890683122, 1.000000000000000000, 0.9659258262890683122, 1.000000000000000000, 0.9659258262890683122, 1.000000000000000000, 0.9659258262890683122, 1.000000000000000000, 0.9659258262890683122, 1.000000000000000000, 0.9659258262890683122, 1.000000000000000000, 0.9659258262890683122, 1.000000000000000000, 0.9659258262890683122, 1.000000000000000000, 0.9659258262890683122, 1.000000000000000000, 0.9659258262890683122, 1.000000000000000000, 0.9659258262890683122, 1.000000000000000000, 0.9659258262890683122, 1.000000000000000000, 0.9659258262890683122, 1.000000000000000000, 0.9659258262890683122, 1.000000000000000000, 0.9659258262890683122, 1.000000000000000000, 0.9659258262890683122, 1.000000000000000000, 0.9659258262890683122, 1.000000000000000000, 0.9659258262890683122, 1.000000000000000000, 0.9659258262890683122, 1.000000000000000000, 0.9659258262890683122, 1.000000000000000000, 0.9659258262890683122, 1.000000000000000000, 0.9659258262890683122, 1.000000000000000000, 0.9659258262890683122, 1.000000000000000000, 0.9659258262890683122, 1.000000000000000000, 0.9659258262890683122, 1.000000000000000000, 0.9659258262890683122, 1.000000000000000000, 0.9659258262890683122, 1.000000000000000000, 0.9659258262890683122, 1.000000000000000000, 0.9659258262890683122, 1.000000000000000000, 0.9659258262890683122, 1.000000000000000000, 0.9659258262890683122, 1.000000000000000000, 0.9659258262890683122, 1.000000000000000000, 0.9659258262890683122, 1.000000000000000000, 0.9659258262890683122, 1.000000000000000000, 0.9659258262890683122, 1.000000000000000000, 0.9659258262890683122, 1.000000000000000000, 0.9659258262890683122, 1.000000000000000000, 0.9659258262890683122, 1.000000000000000000, 0.9659258262890683122, 1.000000000000000000, 0.9659258262890683122, 1.000000000000000000, 0.9659258262890683122, 1.000000000000000000, 0.9659258262890683122, 1.000000000000000000, 0.9659258262890683122, 1.000000000000000000, 0.9659258262890683122, 1.000000000000000000, 0.9659258262890683122, 1.000000000000000000, 0.9659258262890683122, 1.000000000000000000, 0.9659258262890683122, 1.000000000000000000, 0.9659258262890683122, 1.000000000000000000, 0.9659258262890683122, 1.000000000000000000, 0.9659258262890683122, 1.000000000000000000, 0.9659258262890683122, 1.000000000000000000, 0.9659258262890683122, 1.000000000000000000, 0.9659258262890683122, 1.000000000000000000, 0.9659258262890683122, 1.000000000000000000, 0.9659258262890683122, 1.000000000000000000, 0.9659258262890683122, 1.000000000000000000, 0.9659258262890683122, 1.000000000000000000, 0.9659258262890683122, 1.000000000000000000, 0.9659258262890683122, 1.000000000000000000, 0.9659258262890683122, 1.000000000000000000, 0.9659258262890683122, 1.000000000000000000, 0.9659258262890683122, 1.000000000000000000, 0.9659258262890683122, 1.000000000000000000, 0.9659258262890683122, 1.000000000000000000, 0.9659258262890683122, 1.000000000000000000, 0.9659258262890683122, 1.000000000000000000, 0.9659258262890683122, 1.000000000000000000, 0.9659258262890683122, 1.000000000000000000, 0.9659258262890683122, 1.000000000000000000, 0.9659258262890683122, 1.000000000000000000, 0.9659258262890683122, 1.000000000000000000, 0.9659258262890683122, 1.000000000000000000, 0.9659258262890683122, 1.000000000000000000, 0.9659258262890683122, 1.000000000000000000, 0.9659258262890683122, 1.000000000000000000, 0.9659258262890683122, 1.000000000000000000, 0.9659258262890683122, 1.000000000000000000, 0.9659258262890683122, 1.000000000000000000, 0.9659258262890683122, 1.000000000000000000, 0.9659258262890683122, 1.000000000000000000, 0.9659258262890683122, 1.000000000000000000, 0.9659258262890683122, 1.000000000000000000, 0.9659258262890683122, 1.000000000000000000, 0.9659258262890683122, 1.000000000000000000, 0.9659258262890683122, 1.000000000000000000, 0.9659258262890683122, 1.000000000000000000, 0.9659258262890683122, 1.000000000000000000, 0.9659258262890683122, 1.000000000000000000, 0.9659258262890683122, 1.000000000000000000, 0.9659258262890683122, 1.000000000000000000, 0.9659258262890683122, 1.000000000000000000, 0.9659258262890683122, 1.000000000000000000, 0.9659258262890683122, 1.000000000000000000, 0.9659258262890683122, 1.000000000000000000, 0.9659258262890683122, 1.000000000000000000, 0.9659258262890683122, 1.000000000000000000, 0.9659258262890683122, 1.000000000000000000, 0.9659258262890683122, 1.000000000000000000, 0.9659258262890683122, 1.000000000000000000, 0.9659258262890683122, 1.000000000000000000, 0.9659258262890683122, 1.000000000000000000, 0.9659258262890683122, 1.000000000000000000, 0.9659258262890683122, 1.000000000000000000, 0.9659258262890683122, 1.000000000000000000, 0.9659258262890683122, 1.000000000000000000, 0.9659258262890683122, 1.000000000000000000, 0.9659258262890683122, 1.000000000000000000, 0.9659258262890683122, 1.000000000000000000, 0.9659258262890683122, 1.000000000000000000, 0.9659258262890683122, 1.000000000000000000, 0.9659258262890683122, 1.000000000000000000, 0.9659258262890683122, 1.000000000000000000, 0.9659258262890683122, 1.000000000000000000, 0.9659258262890683122, 1.000000000000000000, 0.9659258262890683122, 1.000000000000000000, 0.9659258262890683122, 1.000000000000000000, 0.9659258262890683122, 1.000000000000000000, 0.9659258262890683122, 1.000000000000000000),
 ( 1.000000000000000000, 0.9659258262890683122, 1.000000000000000000, 0.9659258262890683122, 1.000000000000000000, 0.9659258262890683122, 1.000000000000000000, 0.9659258262890683122, 1.000000000000000000, 0.9659258262890683122, 1.000000000000000000, 0.9659258262890683122, 1.000000000000000000, 0.9659258262890683122, 1.000000000000000000, 0.9659258262890683122, 1.000000000000000000, 0.9659258262890683122, 1.000000000000000000, 0.9659258262890683122, 1.000000000000000000, 0.9659258262890683122, 1.000000000000000000, 0.9659258262890683122, 1.000000000000000000, 0.9659258262890683122, 1.000000000000000000, 0.9659258262890683122, 1.000000000000000000, 0.9659258262890683122, 1.000000000000000000, 0.9659258262890683122, 1.000000000000000000, 0.9659258262890683122, 1.000000000000000000, 0.9659258262890683122, 1.000000000000000000, 0.9659258262890683122, 1.000000000000000000, 0.9659258262890683122, 1.000000000000000000, 0.9659258262890683122, 1.000000000000000000, 0.9659258262890683122, 1.000000000000000000, 0.9659258262890683122, 1.000000000000000000, 0.9659258262890683122, 1.000000000000000000, 0.9659258262890683122, 1.000000000000000000, 0.9659258262890683122, 1.000000000000000000, 0.9659258262890683122, 1.000000000000000000, 0.9659258262890683122, 1.000000000000000000, 0.9659258262890683122, 1.000000000000000000, 0.9659258262890683122, 1.000000000000000000, 0.9659258262890683122, 1.000000000000000000, 0.9659258262890683122, 1.000000000000000000, 0.9659258262890683122, 1.000000000000000000, 0.9659258262890683122, 1.000000000000000000, 0.9659258262890683122, 1.000000000000000000, 0.9659258262890683122, 1.000000000000000000, 0.9659258262890683122, 1.000000000000000000, 0.9659258262890683122, 1.000000000000000000, 0.9659258262890683122, 1.000000000000000000, 0.9659258262890683122, 1.000000000000000000, 0.9659258262890683122, 1.000000000000000000, 0.9659258262890683122, 1.000000000000000000, 0.9659258262890683122, 1.000000000000000000, 0.9659258262890683122, 1.000000000000000000, 0.9659258262890683122, 1.000000000000000000, 0.9659258262890683122, 1.000000000000000000, 0.9659258262890683122, 1.000000000000000000, 0.9659258262890683122, 1.000000000000000000, 0.9659258262890683122, 1.000000000000000000, 0.9659258262890683122, 1.000000000000000000, 0.9659258262890683122, 1.000000000000000000, 0.9659258262890683122, 1.000000000000000000, 0.9659258262890683122, 1.000000000000000000, 0.9659258262890683122, 1.000000000000000000, 0.9659258262890683122, 1.000000000000000000, 0.9659258262890683122, 1.000000000000000000, 0.9659258262890683122, 1.000000000000000000, 0.9659258262890683122, 1.000000000000000000, 0.9659258262890683122, 1.000000000000000000, 0.9659258262890683122, 1.000000000000000000, 0.9659258262890683122, 1.000000000000000000, 0.9659258262890683122, 1.000000000000000000, 0.9659258262890683122, 1.000000000000000000, 0.9659258262890683122, 1.000000000000000000, 0.9659258262890683122, 1.000000000000000000, 0.9659258262890683122, 1.000000000000000000, 0.9659258262890683122, 1.000000000000000000, 0.9659258262890683122, 1.000000000000000000, 0.9659258262890683122, 1.000000000000000000, 0.9659258262890683122, 1.000000000000000000, 0.9659258262890683122, 1.000000000000000000, 0.9659258262890683122, 1.000000000000000000, 0.9659258262890683122, 1.000000000000000000, 0.9659258262890683122, 1.000000000000000000, 0.9659258262890683122, 1.000000000000000000, 0.9659258262890683122, 1.000000000000000000, 0.9659258262890683122, 1.000000000000000000, 0.9659258262890683122, 1.000000000000000000, 0.9659258262890683122, 1.000000000000000000, 0.9659258262890683122, 1.000000000000000000, 0.9659258262890683122, 1.000000000000000000, 0.9659258262890683122, 1.000000000000000000, 0.9659258262890683122, 1.000000000000000000, 0.9659258262890683122, 1.000000000000000000, 0.9659258262890683122, 1.000000000000000000, 0.9659258262890683122, 1.000000000000000000, 0.9659258262890683122, 1.000000000000000000, 0.9659258262890683122, 1.000000000000000000, 0.9659258262890683122, 1.000000000000000000, 0.9659258262890683122, 1.000000000000000000, 0.9659258262890683122, 1.000000000000000000, 0.9659258262890683122, 1.000000000000000000, 0.9659258262890683122, 1.000000000000000000, 0.9659258262890683122, 1.000000000000000000, 0.9659258262890683122, 1.000000000000000000, 0.9659258262890683122, 1.000000000000000000, 0.9659258262890683122, 1.000000000000000000, 0.9659258262890683122, 1.000000000000000000, 0.9659258262890683122, 1.000000000000000000, 0.9659258262890683122, 1.000000000000000000, 0.9659258262890683122, 1.000000000000000000, 0.9659258262890683122, 1.000000000000000000, 0.9659258262890683122, 1.000000000000000000, 0.9659258262890683122, 1.000000000000000000, 0.9659258262890683122, 1.000000000000000000, 0.9659258262890683122, 1.000000000000000000, 0.9659258262890683122, 1.000000000000000000, 0.9659258262890683122, 1.000000000000000000, 0.9659258262890683122, 1.000000000000000000, 0.9659258262890683122, 1.000000000000000000, 0.9659258262890683122, 1.000000000000000000, 0.9659258262890683122, 1.000000000000000000, 0.9659258262890683122, 1.000000000000000000, 0.9659258262890683122, 1.000000000000000000, 0.9659258262890683122, 1.000000000000000000, 0.9659258262890683122, 1.000000000000000000, 0.9659258262890683122, 1.000000000000000000, 0.9659258262890683122, 1.000000000000000000, 0.9659258262890683122, 1.000000000000000000, 0.9659258262890683122, 1.000000000000000000, 0.9659258262890683122, 1.000000000000000000, 0.9659258262890683122, 1.000000000000000000, 0.9659258262890683122, 1.000000000000000000, 0.9659258262890683122, 1.000000000000000000, 0.9659258262890683122, 1.000000000000000000, 0.9659258262890683122, 1.000000000000000000, 0.9659258262890683122, 1.000000000000000000, 0.9659258262890683122, 1.000000000000000000, 0.9659258262890683122, 1.000000000000000000, 0.9659258262890683122, 1.000000000000000000, 0.9659258262890683122, 1.000000000000000000, 0.9659258262890683122, 1.000000000000000000, 0.9659258262890683122, 1.000000000000000000, 0.9659258262890683122, 1.000000000000000000, 0.9659258262890683122, 1.000000000000000000, 0.9659258262890683122, 1.000000000000000000, 0.9659258262890683122, 1.000000000000000000, 0.9659258262890683122, 1.000000000000000000, 0.9659258262890683122, 1.000000000000000000, 0.9659258262890683122, 1.000000000000000000, 0.9659258262890683122, 1.000000000000000000, 0.9659258262890683122, 1.000000000000000000, 0.9659258262890683122, 1.000000000000000000, 0.9659258262890683122, 1.000000000000000000, 0.9659258262890683122, 1.000000000000000000, 0.9659258262890683122, 1.000000000000000000, 0.9659258262890683122, 1.000000000000000000, 0.9659258262890683122, 1.000000000000000000, 0.9659258262890683122, 1.000000000000000000, 0.9659258262890683122, 1.000000000000000000, 0.9659258262890683122, 1.000000000000000000, 0.9659258262890683122, 1.000000000000000000, 0.9659258262890683122, 1.000000000000000000, 0.9659258262890683122, 1.000000000000000000, 0.9659258262890683122, 1.000000000000000000, 0.9659258262890683122, 1.000000000000000000, 0.9659258262890683122, 1.000000000000000000, 0.9659258262890683122, 1.000000000000000000, 0.9659258262890683122, 1.000000000000000000, 0.9659258262890683122, 1.000000000000000000, 0.9659258262890683122, 1.000000000000000000, 0.9659258262890683122, 1.000000000000000000, 0.9659258262890683122, 1.000000000000000000, 0.9659258262890683122, 1.000000000000000000, 0.9659258262890683122, 1.000000000000000000, 0.9659258262890683122, 1.000000000000000000, 0.9659258262890683122, 1.000000000000000000, 0.9659258262890683122, 1.000000000000000000, 0.9659258262890683122, 1.000000000000000000, 0.9659258262890683122, 1.000000000000000000, 0.9659258262890683122, 1.000000000000000000, 0.9659258262890683122, 1.000000000000000000, 0.9659258262890683122, 1.000000000000000000, 0.9659258262890683122, 1.000000000000000000, 0.9659258262890683122, 1.000000000000000000, 0.9659258262890683122, 1.000000000000000000, 0.9659258262890683122, 1.000000000000000000, 0.9659258262890683122, 1.000000000000000000, 0.9659258262890683122, 1.000000000000000000, 0.9659258262890683122, 1.000000000000000000, 0.9659258262890683122, 1.000000000000000000, 0.9659258262890683122, 1.000000000000000000, 0.9659258262890683122, 1.000000000000000000, 0.9659258262890683122, 1.000000000000000000, 0.9659258262890683122, 1.000000000000000000, 0.9659258262890683122, 1.000000000000000000, 0.9659258262890683122, 1.000000000000000000, 0.9659258262890683122, 1.000000000000000000, 0.9659258262890683122, 1.000000000000000000, 0.9659258262890683122, 1.000000000000000000, 0.9659258262890683122, 1.000000000000000000, 0.9659258262890683122, 1.000000000000000000, 0.9659258262890683122, 1.000000000000000000, 0.9659258262890683122, 1.000000000000000000, 0.9659258262890683122, 1.000000000000000000, 0.9659258262890683122, 1.000000000000000000, 0.9659258262890683122, 1.000000000000000000, 0.9659258262890683122, 1.000000000000000000, 0.9659258262890683122, 1.000000000000000000, 0.9659258262890683122, 1.000000000000000000, 0.9659258262890683122, 1.000000000000000000, 0.9659258262890683122, 1.000000000000000000, 0.9659258262890683122, 1.000000000000000000, 0.9659258262890683122, 1.000000000000000000, 0.9659258262890683122, 1.000000000000000000, 0.9659258262890683122, 1.000000000000000000, 0.9659258262890683122, 1.000000000000000000, 0.9659258262890683122, 1.000000000000000000, 0.9659258262890683122, 1.000000000000000000, 0.9659258262890683122, 1.000000000000000000, 0.9659258262890683122, 1.000000000000000000, 0.9659258262890683122, 1.000000000000000000, 0.9659258262890683122, 1.000000000000000000, 0.9659258262890683122, 1.000000000000000000, 0.9659258262890683122, 1.000000000000000000, 0.9659258262890683122, 1.000000000000000000, 0.9659258262890683122, 1.000000000000000000, 0.9659258262890683122, 1.000000000000000000, 0.9659258262890683122, 1.000000000000000000, 0.9659258262890683122, 1.000000000000000000, 0.9659258262890683122, 1.000000000000000000, 0.9659258262890683122, 1.000000000000000000, 0.9659258262890683122, 1.000000000000000000, 0.9659258262890683122, 1.000000000000000000, 0.9659258262890683122, 1.000000000000000000, 0.9659258262890683122, 1.000000000000000000, 0.9659258262890683122, 1.000000000000000000, 0.9659258262890683122, 1.000000000000000000, 0.9659258262890683122, 1.000000000000000000, 0.9659258262890683122, 1.000000000000000000, 0.9659258262890683122, 1.000000000000000000, 0.9659258262890683122, 1.000000000000000000, 0.9659258262890683122, 1.000000000000000000, 0.9659258262890683122, 1.000000000000000000, 0.9659258262890683122, 1.000000000000000000, 0.9659258262890683122, 1.000000000000000000, 0.9659258262890683122, 1.000000000000000000, 0.9659258262890683122, 1.000000000000000000, 0.9659258262890683122, 1.000000000000000000, 0.9659258262890683122, 1.000000000000000000, 0.9659258262890683122, 1.000000000000000000, 0.9659258262890683122, 1.000000000000000000, 0.9659258262890683122, 1.000000000000000000, 0.9659258262890683122, 1.000000000000000000, 0.9659258262890683122, 1.000000000000000000, 0.9659258262890683122, 1.000000000000000000, 0.9659258262890683122, 1.000000000000000000, 0.9659258262890683122, 1.000000000000000000, 0.9659258262890683122, 1.000000000000000000, 0.9659258262890683122, 1.000000000000000000, 0.9659258262890683122, 1.000000000000000000, 0.9659258262890683122, 1.000000000000000000, 0.9659258262890683122, 1.000000000000000000, 0.9659258262890683122, 1.000000000000000000, 0.9659258262890683122, 1.000000000000000000) ) ) 
 REPRESENTATION_ITEM ( '' )  SURFACE ( )  );
#57367 = CARTESIAN_POINT ( 'NONE',  ( -0.1902887139107604098, 0.2952755905511810774, -0.1292274648535930714 ) ) ;
#57368 = CARTESIAN_POINT ( 'NONE',  ( -0.3608923884514428360, 0.1771653543307087630, 0.09757992244046791164 ) ) ;
#57369 = CARTESIAN_POINT ( 'NONE',  ( -1.620734908136482577, -0.5511811023622048555, -0.09757992244046775898 ) ) ;
#57370 = CARTESIAN_POINT ( 'NONE',  ( 0.8267716535433077274, 0.1771653543307087630, 0.000000000000000000 ) ) ;
#57371 = CARTESIAN_POINT ( 'NONE',  ( 0.9711286089238851948, -0.6046776061558809534, -0.2411417322834644161 ) ) ;
#57372 = CARTESIAN_POINT ( 'NONE',  ( 1.482939632545932307, 0.05413385826771626580, -0.4176697321401330321 ) ) ;
#57373 = CARTESIAN_POINT ( 'NONE',  ( -0.09186351706036663400, -0.3690944881889763329, 0.3153832671262228327 ) ) ;
#57374 = CARTESIAN_POINT ( 'NONE',  ( 0.3477690288713918276, -0.6692913385826773087, -0.1292274648535924053 ) ) ;
#57375 = CARTESIAN_POINT ( 'NONE',  ( 0.4658792650918640033, -0.2845877964562159024, 0.3641732283464567677 ) ) ;
#57377 = CARTESIAN_POINT ( 'NONE',  ( -1.476377952755905110, 0.1660481256975885056, 0.3530559997133364547 ) ) ;
#57376 = AXIS2_PLACEMENT_3D ( 'NONE', #14672, #58852, #34012 ) ;
#57378 = CARTESIAN_POINT ( 'NONE',  ( -1.194225721784776262, -0.4281496062992124485, 0.4176697321401328655 ) ) ;
#57379 = CARTESIAN_POINT ( 'NONE',  ( -0.4790026246719154557, -0.3162353388693405765, 0.4822834645669290543 ) ) ;
#57380 = VECTOR ( 'NONE', #2523, 39.37007874015748143 ) ;
#57381 = CARTESIAN_POINT ( 'NONE',  ( -0.1070741851644051862, -0.3996062992125986590, -0.2296587926509186528 ) ) ;
#57382 = CARTESIAN_POINT ( 'NONE',  ( 4.893765752498283308E-17, -0.3996062992125985480, -2.832677165354331006 ) ) ;
#57383 = CARTESIAN_POINT ( 'NONE',  ( 0.2887139107611556010, -0.6046776061558807314, 0.2411417322834647770 ) ) ;
#57384 = CARTESIAN_POINT ( 'NONE',  ( 1.043307086614173818, -0.4536011799217368745, -0.2665933059059886201 ) ) ;
#57385 = AXIS2_PLACEMENT_3D ( 'NONE', #72057, #33343, #6818 ) ;
#57386 = AXIS2_PLACEMENT_3D ( 'NONE', #24317, #56710, #68536 ) ;
#57387 = CARTESIAN_POINT ( 'NONE',  ( -0.5183727034120726440, 0.2952755905511811885, 0.1292274648535926551 ) ) ;
#57388 = CARTESIAN_POINT ( 'NONE',  ( 0.2296587926509192634, -0.05778040916215560624, -0.4822834645669293319 ) ) ;
#57389 = EDGE_CURVE ( 'NONE', #9709, #45259, #38316, .T. ) ;
#57390 = CARTESIAN_POINT ( 'NONE',  ( 0.1070741851644054915, -0.3996062992125986035, -2.290026246719159442 ) ) ;
#57391 = CARTESIAN_POINT ( 'NONE',  ( -0.1974969037888706647, 0.3420746716998658843, -1.430446194225722056 ) ) ;
#57392 = CARTESIAN_POINT ( 'NONE',  ( -0.1070741851644051862, -0.3996062992125987146, -2.749343832020996636 ) ) ;
#57393 = CARTESIAN_POINT ( 'NONE',  ( -1.854472803289052507, 2.716535433070866645, -0.5314960629921260393 ) ) ;
#57394 = CARTESIAN_POINT ( 'NONE',  ( 0.1049643490035303689, 0.3917322834645670104, -1.087926509186351476 ) ) ;
#57395 = EDGE_CURVE ( 'NONE', #69205, #37133, #57108, .T. ) ;
#57396 = CARTESIAN_POINT ( 'NONE',  ( -0.4855643044619415427, -0.3690944881889763329, 0.3153832671262228327 ) ) ;
#57397 = CARTESIAN_POINT ( 'NONE',  ( -1.266404199475064773, -0.3162353388693405765, 0.4822834645669290543 ) ) ;
#57398 = CARTESIAN_POINT ( 'NONE',  ( 0.3420746716998660508, -0.1974969037888704149, -2.701443569553805713 ) ) ;
#57399 = CARTESIAN_POINT ( 'NONE',  ( 0.9908136482939640111, -0.6692913385826771977, 0.1292274648535927661 ) ) ;
#57400 = CARTESIAN_POINT ( 'NONE',  ( 1.397637795275591177, -0.5400638737290844871, 0.3530559997133364547 ) ) ;
#57401 = CARTESIAN_POINT ( 'NONE',  ( 0.7020997375328090762, -0.05778040916215560624, -0.4822834645669293319 ) ) ;
#57402 = CARTESIAN_POINT ( 'NONE',  ( 0.4091458600556403535, 0.2362204724409449896, -0.05052493438320210251 ) ) ;
#57403 = CARTESIAN_POINT ( 'NONE',  ( 0.1070741851644054915, -0.3996062992125986035, -2.290026246719159442 ) ) ;
#57404 = CARTESIAN_POINT ( 'NONE',  ( 1.686351706036745890, 0.2952755905511811885, 0.1292274648535926551 ) ) ;
#57405 = CARTESIAN_POINT ( 'NONE',  ( 0.6102362204724416372, -0.5400638737290844871, 0.3530559997133364547 ) ) ;
#57406 = CARTESIAN_POINT ( 'NONE',  ( 0.6889763779527563470, 0.1660481256975883668, -0.3530559997133364547 ) ) ;
#57407 = CARTESIAN_POINT ( 'NONE',  ( 0.6561679790026253567, 0.1283753931104748280, 0.1820866141732283561 ) ) ;
#57408 = CARTESIAN_POINT ( 'NONE',  ( 1.194225721784777594, 0.05413385826771666132, 0.4176697321401328100 ) ) ;
#57409 = CARTESIAN_POINT ( 'NONE',  ( -0.3392501089628019995, 0.1958661417322832277, 0.04658792650918625738 ) ) ;
#57410 = CARTESIAN_POINT ( 'NONE',  ( 0.3280839895013130669, 0.05413385826771666132, 0.4176697321401328100 ) ) ;
#57411 = CARTESIAN_POINT ( 'NONE',  ( 1.259842519685040019, -0.1870078740157480879, -0.4822834645669291653 ) ) ;
#57412 = CARTESIAN_POINT ( 'NONE',  ( 0.2821522309711292364, 0.2952755905511810774, -0.1292274648535930714 ) ) ;
#57413 = CARTESIAN_POINT ( 'NONE',  ( 1.666666666666667185, -0.004921259842519576551, 0.3153832671262227771 ) ) ;
#57414 = CARTESIAN_POINT ( 'NONE',  ( -0.9383202099737524282, -0.05778040916215522460, 0.4822834645669289988 ) ) ;
#57415 = CARTESIAN_POINT ( 'NONE',  ( -1.115485564304461219, -0.4281496062992124485, 0.4176697321401328655 ) ) ;
#57416 = CARTESIAN_POINT ( 'NONE',  ( 1.377952755905512472, -0.6692913385826771977, 8.415575281601705876E-17 ) ) ;
#57417 = CARTESIAN_POINT ( 'NONE',  ( 0.1958661417322834775, 0.3392501089628018884, -0.7014435695538058235 ) ) ;
#57418 = CARTESIAN_POINT ( 'NONE',  ( -0.3392501089628019995, 0.1958661417322832277, -1.593175853018372612 ) ) ;
#57419 = CARTESIAN_POINT ( 'NONE',  ( 0.3917322834645669549, 0.1049643490035304660, -2.636482939632545985 ) ) ;
#57420 = EDGE_LOOP ( 'NONE', ( #45703, #70679, #74868, #1535 ) ) ;
#57421 = CARTESIAN_POINT ( 'NONE',  ( -0.3460692066303958092, -0.1998031496062994683, 0.1049868766404199322 ) ) ;
#57422 = VERTEX_POINT ( 'NONE', #15759 ) ;
#57423 = CARTESIAN_POINT ( 'NONE',  ( 1.541994750656168645, 0.2952755905511810774, -0.1292274648535930714 ) ) ;
#57424 = CARTESIAN_POINT ( 'NONE',  ( 1.286089238845145033, 0.1283753931104748280, 0.1820866141732283561 ) ) ;
#57425 = CARTESIAN_POINT ( 'NONE',  ( -0.3996062992125987146, 0.1070741851644051862, -1.607611548556430403 ) ) ;
#57426 = CARTESIAN_POINT ( 'NONE',  ( 1.299212598425197429, -0.5511811023622047445, 6.969142054262312111E-17 ) ) ;
#57427 = CARTESIAN_POINT ( 'NONE',  ( 0.2362204724409449064, 0.4091458600556404646, -2.425853018372703396 ) ) ;
#57428 = DIRECTION ( 'NONE',  ( -1.000000000000000000, -0.000000000000000000, -0.000000000000000000 ) ) ;
#57429 = CARTESIAN_POINT ( 'NONE',  ( -0.2766439779403090937, 1.847060205936300159, 0.1468512772251157894 ) ) ;
#57430 = CARTESIAN_POINT ( 'NONE',  ( -0.1049643490035302024, -0.3917322834645671215, -0.9442257217847768169 ) ) ;
#57431 = CARTESIAN_POINT ( 'NONE',  ( -0.6299212598425188991, -0.1870078740157480601, -0.3641732283464567677 ) ) ;
#57432 = CARTESIAN_POINT ( 'NONE',  ( -1.601049868766403650, -0.5023911411419708095, 0.1820866141732285504 ) ) ;
#57433 = CARTESIAN_POINT ( 'NONE',  ( -1.338582677165353729, -0.1870078740157479769, 0.4822834645669291653 ) ) ;
#57434 = CARTESIAN_POINT ( 'NONE',  ( 0.2690288713910767848, -0.6692913385826773087, -0.1292274648535924053 ) ) ;
#57435 = CARTESIAN_POINT ( 'NONE',  ( 1.437007874015748810, 0.1660481256975885056, 0.3530559997133364547 ) ) ;
#57436 = VERTEX_POINT ( 'NONE', #79316 ) ;
#57437 = DIRECTION ( 'NONE',  ( 0.000000000000000000, -0.6853444168423467042, 0.7282190812544145908 ) ) ;
#57438 =( CONVERSION_BASED_UNIT ( 'INCH', #4873 ) LENGTH_UNIT ( ) NAMED_UNIT ( #63153 ) );
#57439 = CARTESIAN_POINT ( 'NONE',  ( -0.1265901696524986964, -0.4724409448818899238, -1.961942257217847763 ) ) ;
#57440 = CARTESIAN_POINT ( 'NONE',  ( 0.4102808022082901629, 1.299212598425196985, -1.736178228450289573 ) ) ;
#57441 = CARTESIAN_POINT ( 'NONE',  ( -0.6496062992125976043, 0.07958543189024071263, -0.2665933059059888421 ) ) ;
#57442 = CARTESIAN_POINT ( 'NONE',  ( -1.213910761154854745, -0.6692913385826771977, 0.1292274648535927661 ) ) ;
#57443 = CARTESIAN_POINT ( 'NONE',  ( 1.108923884514436686, -0.3162353388693409650, -0.4822834645669289433 ) ) ;
#57444 = AXIS2_PLACEMENT_3D ( 'NONE', #50562, #43827, #69116 ) ;
#57445 = VERTEX_POINT ( 'NONE', #1870 ) ;
#57447 = DIRECTION ( 'NONE',  ( 0.000000000000000000, 0.000000000000000000, -1.000000000000000000 ) ) ;
#57446 = CARTESIAN_POINT ( 'NONE',  ( -1.868118647894634776, 2.729653158204613739, -0.5314960629921260393 ) ) ;
#57448 = CARTESIAN_POINT ( 'NONE',  ( 1.200787401574803681, 0.1660481256975885056, 0.3530559997133364547 ) ) ;
#57449 = CARTESIAN_POINT ( 'NONE',  ( -1.430446194225721390, -0.4281496062992124485, 0.4176697321401328655 ) ) ;
#57450 = CARTESIAN_POINT ( 'NONE',  ( 0.1049643490035304522, -0.3917322834645668994, -0.6377759598087122672 ) ) ;
#57451 = CARTESIAN_POINT ( 'NONE',  ( -0.2887139107611542133, 0.1283753931104748280, 0.1820866141732283561 ) ) ;
#57452 = CARTESIAN_POINT ( 'NONE',  ( -0.1958661417322836718, 0.3392501089628017219, -0.7276902887139108378 ) ) ;
#57453 = CARTESIAN_POINT ( 'NONE',  ( -0.4790026246719152336, -0.08942795157528024563, -0.3641732283464568787 ) ) ;
#57454 = CARTESIAN_POINT ( 'NONE',  ( 0.03937007874015806264, 0.1771653543307087630, 0.000000000000000000 ) ) ;
#57455 = CARTESIAN_POINT ( 'NONE',  ( -0.006561679790025524116, -0.3162353388693405765, 0.4822834645669290543 ) ) ;
#57456 = CARTESIAN_POINT ( 'NONE',  ( -0.8464566929133852113, 0.07958543189024085140, 0.2665933059059887866 ) ) ;
#57457 = CARTESIAN_POINT ( 'NONE',  ( -0.1049643490035302024, -0.3917322834645671215, -2.898950131233595684 ) ) ;
#57458 = CARTESIAN_POINT ( 'NONE',  ( 1.279527559055118724, 0.1660481256975885056, 0.3530559997133364547 ) ) ;
#57459 = CARTESIAN_POINT ( 'NONE',  ( -1.594488188976377119, 0.1660481256975883668, -0.3530559997133364547 ) ) ;
#57460 = CARTESIAN_POINT ( 'NONE',  ( 5.785732909357575061E-17, -0.4724409448818898682, -1.100393700787401619 ) ) ;
#57461 = CARTESIAN_POINT ( 'NONE',  ( -0.3608923884514428360, -0.6692913385826773087, -0.1292274648535924053 ) ) ;
#57462 = CARTESIAN_POINT ( 'NONE',  ( -1.003937007874014853, 0.1660481256975885056, 0.3530559997133364547 ) ) ;
#57463 = CARTESIAN_POINT ( 'NONE',  ( 1.082677165354331228, 0.07958543189024071263, -0.2665933059059888421 ) ) ;
#57464 = CARTESIAN_POINT ( 'NONE',  ( -0.1377952755905504645, 0.07958543189024085140, 0.2665933059059887866 ) ) ;
#57465 = CARTESIAN_POINT ( 'NONE',  ( -0.7808398950131225646, -0.05778040916215522460, 0.4822834645669289988 ) ) ;
#57466 = CARTESIAN_POINT ( 'NONE',  ( -1.030183727034119867, -0.3162353388693405765, 0.4822834645669290543 ) ) ;
#57467 = FACE_OUTER_BOUND ( 'NONE', #4081, .T. ) ;
#57468 = CARTESIAN_POINT ( 'NONE',  ( 1.299212598425197429, -0.5511811023622047445, 6.969142054262312111E-17 ) ) ;
#57469 = CARTESIAN_POINT ( 'NONE',  ( -0.2624671916010490880, -0.6046776061558807314, 0.2411417322834647770 ) ) ;
#57470 = CARTESIAN_POINT ( 'NONE',  ( -1.482939632545930975, -0.4281496062992127816, -0.4176697321401328100 ) ) ;
#57471 = VERTEX_POINT ( 'NONE', #3114 ) ;
#57472 = CARTESIAN_POINT ( 'NONE',  ( -0.3996062992125985480, -7.340648628747423112E-17, -2.320866141732283783 ) ) ;
#57473 = CARTESIAN_POINT ( 'NONE',  ( -0.9514435695538050464, -0.08942795157528024563, -0.3641732283464568787 ) ) ;
#57474 = CARTESIAN_POINT ( 'NONE',  ( 0.7545931758530188826, -0.6692913385826771977, 0.1292274648535927661 ) ) ;
#57475 = CARTESIAN_POINT ( 'NONE',  ( -0.9580052493438311334, -0.3690944881889763329, 0.3153832671262228327 ) ) ;
#57476 = CARTESIAN_POINT ( 'NONE',  ( -0.1998031496062994405, 0.3460692066303957537, -1.349737532808399143 ) ) ;
#57477 = CARTESIAN_POINT ( 'NONE',  ( -0.8727034120734901146, -0.05778040916215560624, -0.4822834645669293319 ) ) ;
#57478 = CARTESIAN_POINT ( 'NONE',  ( 0.8923884514435703741, 0.2306618581243848609, 0.2411417322834645549 ) ) ;
#57479 = CARTESIAN_POINT ( 'NONE',  ( 1.056430446194226658, 0.2952755905511811885, 0.1292274648535926551 ) ) ;
#57480 = CARTESIAN_POINT ( 'NONE',  ( 0.4531182788721078158, 1.771653543307086354, 0.5309055118110234117 ) ) ;
#57481 = CARTESIAN_POINT ( 'NONE',  ( -1.528871391076114250, 0.1771653543307087075, -0.09757992244046823083 ) ) ;
#57483 = ADVANCED_FACE ( 'NONE', ( #48542, #22051 ), #66260, .T. ) ;
#57482 = CARTESIAN_POINT ( 'NONE',  ( -0.3996062992125984925, -0.1070741851644056719, -0.5951443569553805935 ) ) ;
#57484 = CARTESIAN_POINT ( 'NONE',  ( 0.3996062992125986035, 0.1070741851644054776, -0.7545931758530182165 ) ) ;
#57485 = CARTESIAN_POINT ( 'NONE',  ( -0.1974969037888706647, 0.3420746716998658843, -0.1706036745406825095 ) ) ;
#57486 = CARTESIAN_POINT ( 'NONE',  ( 0.3961676841499099377, 1.274902735363087736, -1.382762819646744523 ) ) ;
#57487 = CARTESIAN_POINT ( 'NONE',  ( 1.194225721784777594, -0.004921259842519576551, 0.3153832671262227771 ) ) ;
#57488 = CARTESIAN_POINT ( 'NONE',  ( 0.6102362204724416372, -0.4536011799217367080, 0.2665933059059888421 ) ) ;
#57489 = CARTESIAN_POINT ( 'NONE',  ( 0.06561679790026316017, 0.05413385826771626580, -0.4176697321401330321 ) ) ;
#57490 = CARTESIAN_POINT ( 'NONE',  ( 1.587926509186352142, 0.05413385826771666132, 0.4176697321401328100 ) ) ;
#57491 = CARTESIAN_POINT ( 'NONE',  ( -0.3949938075777411073, 0.1058382717557497660, -1.369422572178477848 ) ) ;
#57492 = CARTESIAN_POINT ( 'NONE',  ( 0.5118110236220480003, -0.5511811023622047445, 6.969142054262312111E-17 ) ) ;
#57493 =( BOUNDED_SURFACE ( )  B_SPLINE_SURFACE ( 1, 2, ( 
 ( #54758, #74136, #80464, #22368, #80049, #13663, #48436, #66160, #54339, #67822, #48027, #73305, #10159, #51933, #35825, #61491, #3839, #66575, #39316, #60663, #21534, #35410, #77638, #19970, #45621, #47194, #66995, #34997, #71315, #72885, #53921, #79633, #3011, #8500, #3425, #15234, #40894, #21951, #41309, #28678, #73727, #16066, #41712, #67405, #9739, #61074, #68633, #4646, #30738, #49675, #4240, #68238, #17713, #5069, #29904, #49263, #55568, #18528, #82504, #16897, #74965, #69864, #30317, #56805, #76191, #81276, #56401, #23592, #74552, #61899, #75779, #62309, #24413, #43341, #42536, #55985, #29499, #50083, #80869, #44171, #55158, #63547, #24820, #24007, #18120, #10573, #50487, #75365, #12215, #69042, #11392, #37873, #17311, #23181, #48851, #36632, #31138, #62731, #43753, #5476, #36230, #37049, #42939, #10973, #81696, #82099, #69459, #11809, #37464, #63137, #63959, #5881, #70693, #71532, #25646, #12624, #838, #1259, #45833, #39113, #71114, #19344, #6296, #413, #44994, #64795, #13457, #19765, #51309, #64377, #76598, #20607, #13046, #13880, #33237, #7134, #44577, #39967, #39539, #45418, #38699, #32807, #58899, #58474, #26496, #52566, #78275, #52148, #70270, #77854, #20183, #31971, #31554, #38283, #77012, #65227, #7565, #46259, #50898, #6714, #32383, #57632, #26907, #71954, #28936, #14307, #57211, #58047, #26069, #82912, #25233, #18928, #77430, #51728, #53813, #34060, #73623, #47089, #41206, #66057, #2078, #40375, #54649, #35305, #52983, #27743, #22672, #40785, #9635, #28982, #8394, #66894, #59723, #27323, #14722, #28573, #15129, #60559, #79526, #78696, #66470, #65654, #2909, #33647, #80359, #7983, #16374, #60967, #60147, #54230, #21019, #3318, #2499, #48331, #21841, #47505, #74028, #53408, #59309, #1666, #72779, #67301, #15547, #79947, #41612, #46680, #28158, #72373, #79116, #8805, #9224, #21434, #22260, #34481, #73197, #34897, #47918, #15965, #24314, #61799, #48746, #36951, #37369, #82000, #75270, #23909, #55465, #16791, #36534, #81175, #17613, #49574, #55881, #4139, #17207, #29397, #56707, #23492, #49984, #69359, #43244, #80764, #76090, #75682, #81592, #49158, #68942, #11713, #11292, #62628, #5378, #55056, #63040, #4972, #30638, #62210, #82406, #42021, #31039, #24725, #50393, #74864, #23078, #56303, #74445, #18023, #67715, #10051, #35714, #36126, #43657, #61384, #3733, #42428, #42840, #68533, #68128, #10473, #29804, #10873, #4548, #30218, #57115, #25545, #20086, #25133, #63858, #732, #26390, #65124, #63446, #6195, #76908, #82809, #52048, #39011, #50803, #1157, #77753, #76504, #51212, #45736, #71432, #12113, #6613, #37771, #32284, #70169, #13779, #83224, #18833, #44478, #57944, #77328, #12522, #38183, #31873, #7459, #39436, #5782, #57533, #58799, #19238, #33129, #26808, #44889, #19657, #70588, #31452, #12942, #64695, #38600, #13358, #311, #64278, #25965, #18434, #7034, #69769, #52466, #44076, #51623, #45319, #71014, #32704, #58370, #47823, #72682, #73524, #34380, #8709, #15873, #20921, #71855, #22164, #1979, #79847, #28059, #15449, #54132, #59209, #15030, #41521, #78597, #27642, #53716, #33547, #9131, #67206, #53304, #52885, #78174, #59624, #60462, #14621, #1570, #73097, #9539, #34802, #79423, #60045, #8294, #46576, #40686, #33962, #21743, #2401, #47408, #40275, #79017, #65552, #35209, #21336, #2812, #60871, #41108, #27224, #28889, #28471, #66796, #46988, #3224, #20505, #46159, #14205, #39861, #66372, #72273, #7883, #65958, #49483, #54967, #80264, #36856, #81494, #4868, #5283, #55788, #23810, #74350, #4459, #68849, #35622, #62530, #17113, #17520, #75176, #61285, #80674, #16694, #43152, #3637, #30124, #11197, #24218, #30541, #29305, #42334, #56205, #81906, #49889, #22580, #75590, #68443, #22987, #42748, #10783, #4048, #29713, #17929, #43565, #69266, #11613, #37273, #16280, #62948, #41926, #54549, #36443, #48241, #74764, #73937, #67619, #9949, #48653, #68032, #10377, #36034, #62116, #61708, #55376, #81082, #23399, #49066, #25035, #44791, #12844, #39330, #31354, #6100, #70072, #70487, #19985, #64596, #65016, #75996, #50298, #69675, #38085, #32603, #5685 ),
 ( #18338, #63350, #77228, #63759, #25865, #38503, #43978, #31774, #30945, #51525, #82312, #77652, #56612, #24632, #26286, #25448, #19557, #12018, #630, #51113, #51947, #64185, #6519, #45635, #57020, #37673, #58266, #57435, #71330, #32189, #45216, #6932, #82715, #76810, #13678, #50708, #76407, #18738, #70917, #44380, #57845, #13266, #12427, #38916, #83128, #19141, #212, #72991, #2707, #33019, #15344, #21229, #65448, #53195, #46884, #40173, #65857, #9024, #28367, #66689, #59938, #34277, #52364, #54029, #78070, #60360, #72578, #2294, #27538, #47719, #7351, #79741, #22057, #73417, #20816, #20401, #14925, #71747, #41006, #15766, #41418, #58689, #1464, #40585, #66267, #1054, #7780, #8190, #46471, #8606, #26708, #34697, #46053, #14100, #39752, #33448, #14520, #59108, #27120, #1878, #52784, #78493, #78908, #72165, #33857, #27954, #53613, #79321, #21641, #59521, #47301, #23708, #4762, #22886, #36749, #30438, #24119, #68749, #62016, #48966, #61183, #28786, #54448, #74248, #80576, #75489, #56103, #17829, #17010, #35939, #48138, #61608, #81807, #54870, #36342, #29204, #74666, #49788, #55685, #42650, #67102, #80160, #43053, #41821, #42236, #9433, #73835, #16591, #75075, #49379, #10687, #17422, #35102, #68347, #4353, #3537, #30021, #81392, #16175, #11092, #29612, #62425, #60769, #67512, #9849, #48550, #35520, #3120, #22477, #67930, #10271, #3951, #55272, #80983, #23296, #69574, #44692, #18236, #5183, #75896, #6420, #76311, #38403, #57334, #30847, #18642, #43463, #64083, #11511, #6835, #69160, #77558, #38819, #37988, #32089, #82214, #13169, #63664, #64497, #83028, #25351, #32505, #11922, #37167, #70821, #50604, #45114, #76712, #57750, #19464, #24533, #6004, #58168, #43876, #44286, #19045, #50199, #112, #537, #69976, #37577, #62847, #24934, #25767, #63250, #5589, #51428, #26190, #77131, #70389, #51013, #56924, #31256, #31673, #82618, #12744, #51851, #56512, #12330, #78396, #7258, #34605, #33357, #59847, #47211, #21143, #58595, #53938, #53527, #33767, #27027, #1784, #72901, #59429, #46798, #15252, #40083, #20306, #79235, #27444, #14838, #45956, #45539, #26618, #65352, #2199, #27867, #66593, #64920, #7690, #20728, #964, #21550, #40498, #52271, #2620, #40912, #77976, #52688, #8928, #60270, #13581, #8102, #39235, #53105, #71653, #28276, #1375, #14005, #39662, #78814, #72489, #66178, #46379, #8516, #19891, #34183, #71237, #32930, #65770, #59020, #72072, #14431, #74570, #80067, #21967, #3028, #41727, #61917, #4259, #42957, #41331, #67421, #54776, #60679, #29922, #16915, #28694, #62325, #55585, #35015, #29105, #81297, #49280, #73323, #67838, #15669, #10177, #48045, #23611, #61091, #54356, #22385, #35842, #55177, #73746, #16082, #9754, #68651, #74983, #67011, #35426, #36650, #80479, #17328, #10989, #3442, #80886, #22792, #9344, #48452, #42553, #74152, #68256, #61510, #16499, #42143, #79650, #10591, #47628, #5802, #3856, #31472, #29516, #23199, #36248, #48870, #26826, #51641, #52484, #13376, #71032, #78192, #83241, #50821, #1175, #64295, #58818, #7054, #77771, #33149, #38200, #77346, #20523, #57550, #6629, #32722, #12542, #71449, #46175, #32301, #31890, #57134, #38617, #39455, #76927, #63875, #52064, #71871, #13797, #58389, #39029, #70605, #25563, #19677, #12960, #750, #64713, #26411, #19255, #57962, #44497, #14221, #329, #65142, #39881, #20103, #6214, #7902, #7479, #45753, #51229, #65568, #82831, #25983, #44907, #25153, #45336, #76523, #18851, #70188, #28488, #28902, #73543, #66813, #15464, #47005, #8311, #28074, #72699, #9146, #41122, #47422, #79033, #8724, #20937, #48254, #15046, #15886, #60888, #34818, #72291, #67635, #67222, #73113, #40702, #60476, #3238, #2827, #54148, #54565, #53732, #33978, #9554, #79862, #22179, #59639, #59225, #40293, #21352, #41535, #35224, #80280, #78613, #66386, #34395, #14637, #22593, #47837, #65974, #16296, #73950, #1995, #60063, #41939, #33563, #27241, #21759, #52900, #1586, #27658, #46595, #2417, #53324, #79440, #81506, #68861, #10393, #29726, #68046, #82325, #62961, #80688, #55388, #50311, #68457, #37286, #56625, #36049, #11210, #61722 ) ),
 .UNSPECIFIED., .F., .F., .F. ) 
 B_SPLINE_SURFACE_WITH_KNOTS ( ( 2, 2 ),
 ( 3, 2, 2, 2, 2, 2, 2, 2, 2, 2, 2, 2, 2, 2, 2, 2, 2, 2, 2, 2, 2, 2, 2, 2, 2, 2, 2, 2, 2, 2, 2, 2, 2, 2, 2, 2, 2, 2, 2, 2, 2, 2, 2, 2, 2, 2, 2, 2, 2, 2, 2, 2, 2, 2, 2, 2, 2, 2, 2, 2, 2, 2, 2, 2, 2, 2, 2, 2, 2, 2, 2, 2, 2, 2, 2, 2, 2, 2, 2, 2, 2, 2, 2, 2, 2, 2, 2, 2, 2, 2, 2, 2, 2, 2, 2, 2, 2, 2, 2, 2, 2, 2, 2, 2, 2, 2, 2, 2, 2, 2, 2, 2, 2, 2, 2, 2, 2, 2, 2, 2, 2, 2, 2, 2, 2, 2, 2, 2, 2, 2, 2, 2, 2, 2, 2, 2, 2, 2, 2, 2, 2, 2, 2, 2, 2, 2, 2, 2, 2, 2, 2, 2, 2, 2, 2, 2, 2, 2, 2, 2, 2, 2, 2, 2, 2, 2, 2, 2, 2, 2, 2, 2, 2, 2, 2, 2, 2, 2, 2, 2, 2, 2, 2, 2, 2, 2, 2, 2, 2, 2, 2, 2, 2, 2, 2, 2, 2, 2, 2, 2, 2, 2, 2, 2, 2, 2, 2, 2, 2, 2, 2, 2, 2, 2, 2, 2, 2, 2, 2, 2, 2, 2, 2, 2, 2, 2, 2, 2, 2, 2, 2, 2, 2, 2, 2, 2, 2, 2, 2, 2, 2, 2, 2, 2, 2, 2, 2, 2, 2, 2, 2, 2, 2, 2, 2, 3 ),
 ( 0.000000000000000000, 1.000000000000000000 ),
 ( 0.000000000000000000, 0.003787878787878787984, 0.007575757575757575968, 0.01136363636363636395, 0.01515151515151515194, 0.01893939393939393992, 0.02272727272727272790, 0.02651515151515151589, 0.03030303030303030387, 0.03409090909090908839, 0.03787878787878787984, 0.04166666666666666435, 0.04545454545454545581, 0.04924242424242424032, 0.05303030303030303177, 0.05681818181818181629, 0.06060606060606060774, 0.06439393939393939226, 0.06818181818181817677, 0.07196969696969697516, 0.07575757575757575968, 0.07954545454545454419, 0.08333333333333332871, 0.08712121212121212710, 0.09090909090909091161, 0.09469696969696969613, 0.09848484848484848064, 0.1022727272727272790, 0.1060606060606060635, 0.1098484848484848481, 0.1136363636363636326, 0.1174242424242424310, 0.1212121212121212155, 0.1250000000000000000, 0.1287878787878787845, 0.1325757575757575690, 0.1363636363636363535, 0.1401515151515151381, 0.1439393939393939503, 0.1477272727272727348, 0.1515151515151515194, 0.1553030303030303039, 0.1590909090909090884, 0.1628787878787878729, 0.1666666666666666574, 0.1704545454545454419, 0.1742424242424242542, 0.1780303030303030387, 0.1818181818181818232, 0.1856060606060606077, 0.1893939393939393923, 0.1931818181818181768, 0.1969696969696969613, 0.2007575757575757458, 0.2045454545454545581, 0.2083333333333333426, 0.2121212121212121271, 0.2159090909090909116, 0.2196969696969696961, 0.2234848484848484806, 0.2272727272727272652, 0.2310606060606060497, 0.2348484848484848619, 0.2386363636363636465, 0.2424242424242424310, 0.2462121212121212155, 0.2500000000000000000, 0.2537878787878787845, 0.2575757575757575690, 0.2613636363636363535, 0.2651515151515151381, 0.2689393939393939226, 0.2727272727272727071, 0.2765151515151514916, 0.2803030303030302761, 0.2840909090909091161, 0.2878787878787879007, 0.2916666666666666852, 0.2954545454545454697, 0.2992424242424242542, 0.3030303030303030387, 0.3068181818181818232, 0.3106060606060606077, 0.3143939393939393923, 0.3181818181818181768, 0.3219696969696969613, 0.3257575757575757458, 0.3295454545454545303, 0.3333333333333333148, 0.3371212121212120993, 0.3409090909090908839, 0.3446969696969697239, 0.3484848484848485084, 0.3522727272727272929, 0.3560606060606060774, 0.3598484848484848619, 0.3636363636363636465, 0.3674242424242424310, 0.3712121212121212155, 0.3750000000000000000, 0.3787878787878787845, 0.3825757575757575690, 0.3863636363636363535, 0.3901515151515151381, 0.3939393939393939226, 0.3977272727272727071, 0.4015151515151514916, 0.4053030303030302761, 0.4090909090909091161, 0.4128787878787879007, 0.4166666666666666852, 0.4204545454545454697, 0.4242424242424242542, 0.4280303030303030387, 0.4318181818181818232, 0.4356060606060606077, 0.4393939393939393923, 0.4431818181818181768, 0.4469696969696969613, 0.4507575757575757458, 0.4545454545454545303, 0.4583333333333333148, 0.4621212121212120993, 0.4659090909090908839, 0.4696969696969697239, 0.4734848484848485084, 0.4772727272727272929, 0.4810606060606060774, 0.4848484848484848619, 0.4886363636363636465, 0.4924242424242424310, 0.4962121212121212155, 0.5000000000000000000, 0.5037878787878787845, 0.5075757575757575690, 0.5113636363636363535, 0.5151515151515151381, 0.5189393939393939226, 0.5227272727272727071, 0.5265151515151514916, 0.5303030303030302761, 0.5340909090909090606, 0.5378787878787878451, 0.5416666666666666297, 0.5454545454545454142, 0.5492424242424241987, 0.5530303030303029832, 0.5568181818181817677, 0.5606060606060605522, 0.5643939393939394478, 0.5681818181818182323, 0.5719696969696970168, 0.5757575757575758013, 0.5795454545454545858, 0.5833333333333333703, 0.5871212121212121549, 0.5909090909090909394, 0.5946969696969697239, 0.5984848484848485084, 0.6022727272727272929, 0.6060606060606060774, 0.6098484848484848619, 0.6136363636363636465, 0.6174242424242424310, 0.6212121212121212155, 0.6250000000000000000, 0.6287878787878787845, 0.6325757575757575690, 0.6363636363636363535, 0.6401515151515151381, 0.6439393939393939226, 0.6477272727272727071, 0.6515151515151514916, 0.6553030303030302761, 0.6590909090909090606, 0.6628787878787878451, 0.6666666666666666297, 0.6704545454545454142, 0.6742424242424241987, 0.6780303030303029832, 0.6818181818181817677, 0.6856060606060605522, 0.6893939393939394478, 0.6931818181818182323, 0.6969696969696970168, 0.7007575757575758013, 0.7045454545454545858, 0.7083333333333333703, 0.7121212121212121549, 0.7159090909090909394, 0.7196969696969697239, 0.7234848484848485084, 0.7272727272727272929, 0.7310606060606060774, 0.7348484848484848619, 0.7386363636363636465, 0.7424242424242424310, 0.7462121212121212155, 0.7500000000000000000, 0.7537878787878787845, 0.7575757575757575690, 0.7613636363636363535, 0.7651515151515151381, 0.7689393939393939226, 0.7727272727272727071, 0.7765151515151514916, 0.7803030303030302761, 0.7840909090909090606, 0.7878787878787878451, 0.7916666666666666297, 0.7954545454545454142, 0.7992424242424241987, 0.8030303030303029832, 0.8068181818181817677, 0.8106060606060605522, 0.8143939393939394478, 0.8181818181818182323, 0.8219696969696970168, 0.8257575757575758013, 0.8295454545454545858, 0.8333333333333333703, 0.8371212121212121549, 0.8409090909090909394, 0.8446969696969697239, 0.8484848484848485084, 0.8522727272727272929, 0.8560606060606060774, 0.8598484848484848619, 0.8636363636363636465, 0.8674242424242424310, 0.8712121212121212155, 0.8750000000000000000, 0.8787878787878787845, 0.8825757575757575690, 0.8863636363636363535, 0.8901515151515151381, 0.8939393939393939226, 0.8977272727272727071, 0.9015151515151514916, 0.9053030303030302761, 0.9090909090909090606, 0.9128787878787878451, 0.9166666666666666297, 0.9204545454545454142, 0.9242424242424241987, 0.9280303030303029832, 0.9318181818181817677, 0.9356060606060605522, 0.9393939393939394478, 0.9431818181818182323, 0.9469696969696970168, 0.9507575757575758013, 0.9545454545454545858, 0.9583333333333333703, 0.9621212121212121549, 0.9659090909090909394 ),
 .UNSPECIFIED. ) 
 GEOMETRIC_REPRESENTATION_ITEM ( )  RATIONAL_B_SPLINE_SURFACE ( (
 ( 1.000000000000000000, 0.9659258262890683122, 1.000000000000000000, 0.9659258262890683122, 1.000000000000000000, 0.9659258262890683122, 1.000000000000000000, 0.9659258262890683122, 1.000000000000000000, 0.9659258262890683122, 1.000000000000000000, 0.9659258262890683122, 1.000000000000000000, 0.9659258262890683122, 1.000000000000000000, 0.9659258262890683122, 1.000000000000000000, 0.9659258262890683122, 1.000000000000000000, 0.9659258262890683122, 1.000000000000000000, 0.9659258262890683122, 1.000000000000000000, 0.9659258262890683122, 1.000000000000000000, 0.9659258262890683122, 1.000000000000000000, 0.9659258262890683122, 1.000000000000000000, 0.9659258262890683122, 1.000000000000000000, 0.9659258262890683122, 1.000000000000000000, 0.9659258262890683122, 1.000000000000000000, 0.9659258262890683122, 1.000000000000000000, 0.9659258262890683122, 1.000000000000000000, 0.9659258262890683122, 1.000000000000000000, 0.9659258262890683122, 1.000000000000000000, 0.9659258262890683122, 1.000000000000000000, 0.9659258262890683122, 1.000000000000000000, 0.9659258262890683122, 1.000000000000000000, 0.9659258262890683122, 1.000000000000000000, 0.9659258262890683122, 1.000000000000000000, 0.9659258262890683122, 1.000000000000000000, 0.9659258262890683122, 1.000000000000000000, 0.9659258262890683122, 1.000000000000000000, 0.9659258262890683122, 1.000000000000000000, 0.9659258262890683122, 1.000000000000000000, 0.9659258262890683122, 1.000000000000000000, 0.9659258262890683122, 1.000000000000000000, 0.9659258262890683122, 1.000000000000000000, 0.9659258262890683122, 1.000000000000000000, 0.9659258262890683122, 1.000000000000000000, 0.9659258262890683122, 1.000000000000000000, 0.9659258262890683122, 1.000000000000000000, 0.9659258262890683122, 1.000000000000000000, 0.9659258262890683122, 1.000000000000000000, 0.9659258262890683122, 1.000000000000000000, 0.9659258262890683122, 1.000000000000000000, 0.9659258262890683122, 1.000000000000000000, 0.9659258262890683122, 1.000000000000000000, 0.9659258262890683122, 1.000000000000000000, 0.9659258262890683122, 1.000000000000000000, 0.9659258262890683122, 1.000000000000000000, 0.9659258262890683122, 1.000000000000000000, 0.9659258262890683122, 1.000000000000000000, 0.9659258262890683122, 1.000000000000000000, 0.9659258262890683122, 1.000000000000000000, 0.9659258262890683122, 1.000000000000000000, 0.9659258262890683122, 1.000000000000000000, 0.9659258262890683122, 1.000000000000000000, 0.9659258262890683122, 1.000000000000000000, 0.9659258262890683122, 1.000000000000000000, 0.9659258262890683122, 1.000000000000000000, 0.9659258262890683122, 1.000000000000000000, 0.9659258262890683122, 1.000000000000000000, 0.9659258262890683122, 1.000000000000000000, 0.9659258262890683122, 1.000000000000000000, 0.9659258262890683122, 1.000000000000000000, 0.9659258262890683122, 1.000000000000000000, 0.9659258262890683122, 1.000000000000000000, 0.9659258262890683122, 1.000000000000000000, 0.9659258262890683122, 1.000000000000000000, 0.9659258262890683122, 1.000000000000000000, 0.9659258262890683122, 1.000000000000000000, 0.9659258262890683122, 1.000000000000000000, 0.9659258262890683122, 1.000000000000000000, 0.9659258262890683122, 1.000000000000000000, 0.9659258262890683122, 1.000000000000000000, 0.9659258262890683122, 1.000000000000000000, 0.9659258262890683122, 1.000000000000000000, 0.9659258262890683122, 1.000000000000000000, 0.9659258262890683122, 1.000000000000000000, 0.9659258262890683122, 1.000000000000000000, 0.9659258262890683122, 1.000000000000000000, 0.9659258262890683122, 1.000000000000000000, 0.9659258262890683122, 1.000000000000000000, 0.9659258262890683122, 1.000000000000000000, 0.9659258262890683122, 1.000000000000000000, 0.9659258262890683122, 1.000000000000000000, 0.9659258262890683122, 1.000000000000000000, 0.9659258262890683122, 1.000000000000000000, 0.9659258262890683122, 1.000000000000000000, 0.9659258262890683122, 1.000000000000000000, 0.9659258262890683122, 1.000000000000000000, 0.9659258262890683122, 1.000000000000000000, 0.9659258262890683122, 1.000000000000000000, 0.9659258262890683122, 1.000000000000000000, 0.9659258262890683122, 1.000000000000000000, 0.9659258262890683122, 1.000000000000000000, 0.9659258262890683122, 1.000000000000000000, 0.9659258262890683122, 1.000000000000000000, 0.9659258262890683122, 1.000000000000000000, 0.9659258262890683122, 1.000000000000000000, 0.9659258262890683122, 1.000000000000000000, 0.9659258262890683122, 1.000000000000000000, 0.9659258262890683122, 1.000000000000000000, 0.9659258262890683122, 1.000000000000000000, 0.9659258262890683122, 1.000000000000000000, 0.9659258262890683122, 1.000000000000000000, 0.9659258262890683122, 1.000000000000000000, 0.9659258262890683122, 1.000000000000000000, 0.9659258262890683122, 1.000000000000000000, 0.9659258262890683122, 1.000000000000000000, 0.9659258262890683122, 1.000000000000000000, 0.9659258262890683122, 1.000000000000000000, 0.9659258262890683122, 1.000000000000000000, 0.9659258262890683122, 1.000000000000000000, 0.9659258262890683122, 1.000000000000000000, 0.9659258262890683122, 1.000000000000000000, 0.9659258262890683122, 1.000000000000000000, 0.9659258262890683122, 1.000000000000000000, 0.9659258262890683122, 1.000000000000000000, 0.9659258262890683122, 1.000000000000000000, 0.9659258262890683122, 1.000000000000000000, 0.9659258262890683122, 1.000000000000000000, 0.9659258262890683122, 1.000000000000000000, 0.9659258262890683122, 1.000000000000000000, 0.9659258262890683122, 1.000000000000000000, 0.9659258262890683122, 1.000000000000000000, 0.9659258262890683122, 1.000000000000000000, 0.9659258262890683122, 1.000000000000000000, 0.9659258262890683122, 1.000000000000000000, 0.9659258262890683122, 1.000000000000000000, 0.9659258262890683122, 1.000000000000000000, 0.9659258262890683122, 1.000000000000000000, 0.9659258262890683122, 1.000000000000000000, 0.9659258262890683122, 1.000000000000000000, 0.9659258262890683122, 1.000000000000000000, 0.9659258262890683122, 1.000000000000000000, 0.9659258262890683122, 1.000000000000000000, 0.9659258262890683122, 1.000000000000000000, 0.9659258262890683122, 1.000000000000000000, 0.9659258262890683122, 1.000000000000000000, 0.9659258262890683122, 1.000000000000000000, 0.9659258262890683122, 1.000000000000000000, 0.9659258262890683122, 1.000000000000000000, 0.9659258262890683122, 1.000000000000000000, 0.9659258262890683122, 1.000000000000000000, 0.9659258262890683122, 1.000000000000000000, 0.9659258262890683122, 1.000000000000000000, 0.9659258262890683122, 1.000000000000000000, 0.9659258262890683122, 1.000000000000000000, 0.9659258262890683122, 1.000000000000000000, 0.9659258262890683122, 1.000000000000000000, 0.9659258262890683122, 1.000000000000000000, 0.9659258262890683122, 1.000000000000000000, 0.9659258262890683122, 1.000000000000000000, 0.9659258262890683122, 1.000000000000000000, 0.9659258262890683122, 1.000000000000000000, 0.9659258262890683122, 1.000000000000000000, 0.9659258262890683122, 1.000000000000000000, 0.9659258262890683122, 1.000000000000000000, 0.9659258262890683122, 1.000000000000000000, 0.9659258262890683122, 1.000000000000000000, 0.9659258262890683122, 1.000000000000000000, 0.9659258262890683122, 1.000000000000000000, 0.9659258262890683122, 1.000000000000000000, 0.9659258262890683122, 1.000000000000000000, 0.9659258262890683122, 1.000000000000000000, 0.9659258262890683122, 1.000000000000000000, 0.9659258262890683122, 1.000000000000000000, 0.9659258262890683122, 1.000000000000000000, 0.9659258262890683122, 1.000000000000000000, 0.9659258262890683122, 1.000000000000000000, 0.9659258262890683122, 1.000000000000000000, 0.9659258262890683122, 1.000000000000000000, 0.9659258262890683122, 1.000000000000000000, 0.9659258262890683122, 1.000000000000000000, 0.9659258262890683122, 1.000000000000000000, 0.9659258262890683122, 1.000000000000000000, 0.9659258262890683122, 1.000000000000000000, 0.9659258262890683122, 1.000000000000000000, 0.9659258262890683122, 1.000000000000000000, 0.9659258262890683122, 1.000000000000000000, 0.9659258262890683122, 1.000000000000000000, 0.9659258262890683122, 1.000000000000000000, 0.9659258262890683122, 1.000000000000000000, 0.9659258262890683122, 1.000000000000000000, 0.9659258262890683122, 1.000000000000000000, 0.9659258262890683122, 1.000000000000000000, 0.9659258262890683122, 1.000000000000000000, 0.9659258262890683122, 1.000000000000000000, 0.9659258262890683122, 1.000000000000000000, 0.9659258262890683122, 1.000000000000000000, 0.9659258262890683122, 1.000000000000000000, 0.9659258262890683122, 1.000000000000000000, 0.9659258262890683122, 1.000000000000000000, 0.9659258262890683122, 1.000000000000000000, 0.9659258262890683122, 1.000000000000000000, 0.9659258262890683122, 1.000000000000000000, 0.9659258262890683122, 1.000000000000000000, 0.9659258262890683122, 1.000000000000000000, 0.9659258262890683122, 1.000000000000000000, 0.9659258262890683122, 1.000000000000000000, 0.9659258262890683122, 1.000000000000000000, 0.9659258262890683122, 1.000000000000000000, 0.9659258262890683122, 1.000000000000000000, 0.9659258262890683122, 1.000000000000000000, 0.9659258262890683122, 1.000000000000000000, 0.9659258262890683122, 1.000000000000000000, 0.9659258262890683122, 1.000000000000000000, 0.9659258262890683122, 1.000000000000000000, 0.9659258262890683122, 1.000000000000000000, 0.9659258262890683122, 1.000000000000000000, 0.9659258262890683122, 1.000000000000000000, 0.9659258262890683122, 1.000000000000000000, 0.9659258262890683122, 1.000000000000000000, 0.9659258262890683122, 1.000000000000000000, 0.9659258262890683122, 1.000000000000000000, 0.9659258262890683122, 1.000000000000000000, 0.9659258262890683122, 1.000000000000000000, 0.9659258262890683122, 1.000000000000000000, 0.9659258262890683122, 1.000000000000000000, 0.9659258262890683122, 1.000000000000000000, 0.9659258262890683122, 1.000000000000000000, 0.9659258262890683122, 1.000000000000000000, 0.9659258262890683122, 1.000000000000000000, 0.9659258262890683122, 1.000000000000000000, 0.9659258262890683122, 1.000000000000000000, 0.9659258262890683122, 1.000000000000000000, 0.9659258262890683122, 1.000000000000000000, 0.9659258262890683122, 1.000000000000000000, 0.9659258262890683122, 1.000000000000000000, 0.9659258262890683122, 1.000000000000000000, 0.9659258262890683122, 1.000000000000000000, 0.9659258262890683122, 1.000000000000000000, 0.9659258262890683122, 1.000000000000000000, 0.9659258262890683122, 1.000000000000000000, 0.9659258262890683122, 1.000000000000000000, 0.9659258262890683122, 1.000000000000000000, 0.9659258262890683122, 1.000000000000000000, 0.9659258262890683122, 1.000000000000000000, 0.9659258262890683122, 1.000000000000000000, 0.9659258262890683122, 1.000000000000000000, 0.9659258262890683122, 1.000000000000000000, 0.9659258262890683122, 1.000000000000000000, 0.9659258262890683122, 1.000000000000000000, 0.9659258262890683122, 1.000000000000000000, 0.9659258262890683122, 1.000000000000000000, 0.9659258262890683122, 1.000000000000000000, 0.9659258262890683122, 1.000000000000000000, 0.9659258262890683122, 1.000000000000000000, 0.9659258262890683122, 1.000000000000000000, 0.9659258262890683122, 1.000000000000000000, 0.9659258262890683122, 1.000000000000000000, 0.9659258262890683122, 1.000000000000000000, 0.9659258262890683122, 1.000000000000000000, 0.9659258262890683122, 1.000000000000000000, 0.9659258262890683122, 1.000000000000000000, 0.9659258262890683122, 1.000000000000000000, 0.9659258262890683122, 1.000000000000000000),
 ( 1.000000000000000000, 0.9659258262890683122, 1.000000000000000000, 0.9659258262890683122, 1.000000000000000000, 0.9659258262890683122, 1.000000000000000000, 0.9659258262890683122, 1.000000000000000000, 0.9659258262890683122, 1.000000000000000000, 0.9659258262890683122, 1.000000000000000000, 0.9659258262890683122, 1.000000000000000000, 0.9659258262890683122, 1.000000000000000000, 0.9659258262890683122, 1.000000000000000000, 0.9659258262890683122, 1.000000000000000000, 0.9659258262890683122, 1.000000000000000000, 0.9659258262890683122, 1.000000000000000000, 0.9659258262890683122, 1.000000000000000000, 0.9659258262890683122, 1.000000000000000000, 0.9659258262890683122, 1.000000000000000000, 0.9659258262890683122, 1.000000000000000000, 0.9659258262890683122, 1.000000000000000000, 0.9659258262890683122, 1.000000000000000000, 0.9659258262890683122, 1.000000000000000000, 0.9659258262890683122, 1.000000000000000000, 0.9659258262890683122, 1.000000000000000000, 0.9659258262890683122, 1.000000000000000000, 0.9659258262890683122, 1.000000000000000000, 0.9659258262890683122, 1.000000000000000000, 0.9659258262890683122, 1.000000000000000000, 0.9659258262890683122, 1.000000000000000000, 0.9659258262890683122, 1.000000000000000000, 0.9659258262890683122, 1.000000000000000000, 0.9659258262890683122, 1.000000000000000000, 0.9659258262890683122, 1.000000000000000000, 0.9659258262890683122, 1.000000000000000000, 0.9659258262890683122, 1.000000000000000000, 0.9659258262890683122, 1.000000000000000000, 0.9659258262890683122, 1.000000000000000000, 0.9659258262890683122, 1.000000000000000000, 0.9659258262890683122, 1.000000000000000000, 0.9659258262890683122, 1.000000000000000000, 0.9659258262890683122, 1.000000000000000000, 0.9659258262890683122, 1.000000000000000000, 0.9659258262890683122, 1.000000000000000000, 0.9659258262890683122, 1.000000000000000000, 0.9659258262890683122, 1.000000000000000000, 0.9659258262890683122, 1.000000000000000000, 0.9659258262890683122, 1.000000000000000000, 0.9659258262890683122, 1.000000000000000000, 0.9659258262890683122, 1.000000000000000000, 0.9659258262890683122, 1.000000000000000000, 0.9659258262890683122, 1.000000000000000000, 0.9659258262890683122, 1.000000000000000000, 0.9659258262890683122, 1.000000000000000000, 0.9659258262890683122, 1.000000000000000000, 0.9659258262890683122, 1.000000000000000000, 0.9659258262890683122, 1.000000000000000000, 0.9659258262890683122, 1.000000000000000000, 0.9659258262890683122, 1.000000000000000000, 0.9659258262890683122, 1.000000000000000000, 0.9659258262890683122, 1.000000000000000000, 0.9659258262890683122, 1.000000000000000000, 0.9659258262890683122, 1.000000000000000000, 0.9659258262890683122, 1.000000000000000000, 0.9659258262890683122, 1.000000000000000000, 0.9659258262890683122, 1.000000000000000000, 0.9659258262890683122, 1.000000000000000000, 0.9659258262890683122, 1.000000000000000000, 0.9659258262890683122, 1.000000000000000000, 0.9659258262890683122, 1.000000000000000000, 0.9659258262890683122, 1.000000000000000000, 0.9659258262890683122, 1.000000000000000000, 0.9659258262890683122, 1.000000000000000000, 0.9659258262890683122, 1.000000000000000000, 0.9659258262890683122, 1.000000000000000000, 0.9659258262890683122, 1.000000000000000000, 0.9659258262890683122, 1.000000000000000000, 0.9659258262890683122, 1.000000000000000000, 0.9659258262890683122, 1.000000000000000000, 0.9659258262890683122, 1.000000000000000000, 0.9659258262890683122, 1.000000000000000000, 0.9659258262890683122, 1.000000000000000000, 0.9659258262890683122, 1.000000000000000000, 0.9659258262890683122, 1.000000000000000000, 0.9659258262890683122, 1.000000000000000000, 0.9659258262890683122, 1.000000000000000000, 0.9659258262890683122, 1.000000000000000000, 0.9659258262890683122, 1.000000000000000000, 0.9659258262890683122, 1.000000000000000000, 0.9659258262890683122, 1.000000000000000000, 0.9659258262890683122, 1.000000000000000000, 0.9659258262890683122, 1.000000000000000000, 0.9659258262890683122, 1.000000000000000000, 0.9659258262890683122, 1.000000000000000000, 0.9659258262890683122, 1.000000000000000000, 0.9659258262890683122, 1.000000000000000000, 0.9659258262890683122, 1.000000000000000000, 0.9659258262890683122, 1.000000000000000000, 0.9659258262890683122, 1.000000000000000000, 0.9659258262890683122, 1.000000000000000000, 0.9659258262890683122, 1.000000000000000000, 0.9659258262890683122, 1.000000000000000000, 0.9659258262890683122, 1.000000000000000000, 0.9659258262890683122, 1.000000000000000000, 0.9659258262890683122, 1.000000000000000000, 0.9659258262890683122, 1.000000000000000000, 0.9659258262890683122, 1.000000000000000000, 0.9659258262890683122, 1.000000000000000000, 0.9659258262890683122, 1.000000000000000000, 0.9659258262890683122, 1.000000000000000000, 0.9659258262890683122, 1.000000000000000000, 0.9659258262890683122, 1.000000000000000000, 0.9659258262890683122, 1.000000000000000000, 0.9659258262890683122, 1.000000000000000000, 0.9659258262890683122, 1.000000000000000000, 0.9659258262890683122, 1.000000000000000000, 0.9659258262890683122, 1.000000000000000000, 0.9659258262890683122, 1.000000000000000000, 0.9659258262890683122, 1.000000000000000000, 0.9659258262890683122, 1.000000000000000000, 0.9659258262890683122, 1.000000000000000000, 0.9659258262890683122, 1.000000000000000000, 0.9659258262890683122, 1.000000000000000000, 0.9659258262890683122, 1.000000000000000000, 0.9659258262890683122, 1.000000000000000000, 0.9659258262890683122, 1.000000000000000000, 0.9659258262890683122, 1.000000000000000000, 0.9659258262890683122, 1.000000000000000000, 0.9659258262890683122, 1.000000000000000000, 0.9659258262890683122, 1.000000000000000000, 0.9659258262890683122, 1.000000000000000000, 0.9659258262890683122, 1.000000000000000000, 0.9659258262890683122, 1.000000000000000000, 0.9659258262890683122, 1.000000000000000000, 0.9659258262890683122, 1.000000000000000000, 0.9659258262890683122, 1.000000000000000000, 0.9659258262890683122, 1.000000000000000000, 0.9659258262890683122, 1.000000000000000000, 0.9659258262890683122, 1.000000000000000000, 0.9659258262890683122, 1.000000000000000000, 0.9659258262890683122, 1.000000000000000000, 0.9659258262890683122, 1.000000000000000000, 0.9659258262890683122, 1.000000000000000000, 0.9659258262890683122, 1.000000000000000000, 0.9659258262890683122, 1.000000000000000000, 0.9659258262890683122, 1.000000000000000000, 0.9659258262890683122, 1.000000000000000000, 0.9659258262890683122, 1.000000000000000000, 0.9659258262890683122, 1.000000000000000000, 0.9659258262890683122, 1.000000000000000000, 0.9659258262890683122, 1.000000000000000000, 0.9659258262890683122, 1.000000000000000000, 0.9659258262890683122, 1.000000000000000000, 0.9659258262890683122, 1.000000000000000000, 0.9659258262890683122, 1.000000000000000000, 0.9659258262890683122, 1.000000000000000000, 0.9659258262890683122, 1.000000000000000000, 0.9659258262890683122, 1.000000000000000000, 0.9659258262890683122, 1.000000000000000000, 0.9659258262890683122, 1.000000000000000000, 0.9659258262890683122, 1.000000000000000000, 0.9659258262890683122, 1.000000000000000000, 0.9659258262890683122, 1.000000000000000000, 0.9659258262890683122, 1.000000000000000000, 0.9659258262890683122, 1.000000000000000000, 0.9659258262890683122, 1.000000000000000000, 0.9659258262890683122, 1.000000000000000000, 0.9659258262890683122, 1.000000000000000000, 0.9659258262890683122, 1.000000000000000000, 0.9659258262890683122, 1.000000000000000000, 0.9659258262890683122, 1.000000000000000000, 0.9659258262890683122, 1.000000000000000000, 0.9659258262890683122, 1.000000000000000000, 0.9659258262890683122, 1.000000000000000000, 0.9659258262890683122, 1.000000000000000000, 0.9659258262890683122, 1.000000000000000000, 0.9659258262890683122, 1.000000000000000000, 0.9659258262890683122, 1.000000000000000000, 0.9659258262890683122, 1.000000000000000000, 0.9659258262890683122, 1.000000000000000000, 0.9659258262890683122, 1.000000000000000000, 0.9659258262890683122, 1.000000000000000000, 0.9659258262890683122, 1.000000000000000000, 0.9659258262890683122, 1.000000000000000000, 0.9659258262890683122, 1.000000000000000000, 0.9659258262890683122, 1.000000000000000000, 0.9659258262890683122, 1.000000000000000000, 0.9659258262890683122, 1.000000000000000000, 0.9659258262890683122, 1.000000000000000000, 0.9659258262890683122, 1.000000000000000000, 0.9659258262890683122, 1.000000000000000000, 0.9659258262890683122, 1.000000000000000000, 0.9659258262890683122, 1.000000000000000000, 0.9659258262890683122, 1.000000000000000000, 0.9659258262890683122, 1.000000000000000000, 0.9659258262890683122, 1.000000000000000000, 0.9659258262890683122, 1.000000000000000000, 0.9659258262890683122, 1.000000000000000000, 0.9659258262890683122, 1.000000000000000000, 0.9659258262890683122, 1.000000000000000000, 0.9659258262890683122, 1.000000000000000000, 0.9659258262890683122, 1.000000000000000000, 0.9659258262890683122, 1.000000000000000000, 0.9659258262890683122, 1.000000000000000000, 0.9659258262890683122, 1.000000000000000000, 0.9659258262890683122, 1.000000000000000000, 0.9659258262890683122, 1.000000000000000000, 0.9659258262890683122, 1.000000000000000000, 0.9659258262890683122, 1.000000000000000000, 0.9659258262890683122, 1.000000000000000000, 0.9659258262890683122, 1.000000000000000000, 0.9659258262890683122, 1.000000000000000000, 0.9659258262890683122, 1.000000000000000000, 0.9659258262890683122, 1.000000000000000000, 0.9659258262890683122, 1.000000000000000000, 0.9659258262890683122, 1.000000000000000000, 0.9659258262890683122, 1.000000000000000000, 0.9659258262890683122, 1.000000000000000000, 0.9659258262890683122, 1.000000000000000000, 0.9659258262890683122, 1.000000000000000000, 0.9659258262890683122, 1.000000000000000000, 0.9659258262890683122, 1.000000000000000000, 0.9659258262890683122, 1.000000000000000000, 0.9659258262890683122, 1.000000000000000000, 0.9659258262890683122, 1.000000000000000000, 0.9659258262890683122, 1.000000000000000000, 0.9659258262890683122, 1.000000000000000000, 0.9659258262890683122, 1.000000000000000000, 0.9659258262890683122, 1.000000000000000000, 0.9659258262890683122, 1.000000000000000000, 0.9659258262890683122, 1.000000000000000000, 0.9659258262890683122, 1.000000000000000000, 0.9659258262890683122, 1.000000000000000000, 0.9659258262890683122, 1.000000000000000000, 0.9659258262890683122, 1.000000000000000000, 0.9659258262890683122, 1.000000000000000000, 0.9659258262890683122, 1.000000000000000000, 0.9659258262890683122, 1.000000000000000000, 0.9659258262890683122, 1.000000000000000000, 0.9659258262890683122, 1.000000000000000000, 0.9659258262890683122, 1.000000000000000000, 0.9659258262890683122, 1.000000000000000000, 0.9659258262890683122, 1.000000000000000000, 0.9659258262890683122, 1.000000000000000000, 0.9659258262890683122, 1.000000000000000000, 0.9659258262890683122, 1.000000000000000000, 0.9659258262890683122, 1.000000000000000000, 0.9659258262890683122, 1.000000000000000000, 0.9659258262890683122, 1.000000000000000000, 0.9659258262890683122, 1.000000000000000000, 0.9659258262890683122, 1.000000000000000000, 0.9659258262890683122, 1.000000000000000000, 0.9659258262890683122, 1.000000000000000000, 0.9659258262890683122, 1.000000000000000000, 0.9659258262890683122, 1.000000000000000000, 0.9659258262890683122, 1.000000000000000000, 0.9659258262890683122, 1.000000000000000000, 0.9659258262890683122, 1.000000000000000000, 0.9659258262890683122, 1.000000000000000000) ) ) 
 REPRESENTATION_ITEM ( '' )  SURFACE ( )  );
#57494 = CARTESIAN_POINT ( 'NONE',  ( -0.8530183727034112984, 0.05413385826771666132, 0.4176697321401328100 ) ) ;
#57495 = CARTESIAN_POINT ( 'NONE',  ( -1.069553805774277722, -0.6692913385826773087, -0.1292274648535924053 ) ) ;
#57496 = CARTESIAN_POINT ( 'NONE',  ( 0.7349081364829403995, 0.2306618581243848609, 0.2411417322834645549 ) ) ;
#57497 = CARTESIAN_POINT ( 'NONE',  ( 0.4724409448818897572, -0.1265901696524988906, -1.686351706036745446 ) ) ;
#57498 = AXIS2_PLACEMENT_3D ( 'NONE', #53455, #8032, #72829 ) ;
#57499 = CARTESIAN_POINT ( 'NONE',  ( 0.4724409448818898682, 0.000000000000000000, -2.755905511811024056 ) ) ;
#57500 = VERTEX_POINT ( 'NONE', #80154 ) ;
#57501 = ORIENTED_EDGE ( 'NONE', *, *, #1376, .T. ) ;
#57502 = CARTESIAN_POINT ( 'NONE',  ( -1.279527559055116948, -0.5400638737290844871, 0.3530559997133364547 ) ) ;
#57503 = CARTESIAN_POINT ( 'NONE',  ( -0.8070866141732276899, 0.1660481256975883668, -0.3530559997133364547 ) ) ;
#57505 = CARTESIAN_POINT ( 'NONE',  ( -0.7742782152230962556, -0.4281496062992127816, -0.4176697321401328100 ) ) ;
#57504 = CARTESIAN_POINT ( 'NONE',  ( -0.9908136482939626788, 0.1771653543307087630, 0.09757992244046791164 ) ) ;
#57506 = CARTESIAN_POINT ( 'NONE',  ( -0.3917322834645668994, -0.1049643490035306742, -2.173209030674854159 ) ) ;
#57507 = CARTESIAN_POINT ( 'NONE',  ( 0.1829408352246091884, -0.2319625946588664833, 0.1465682319128800981 ) ) ;
#57508 = CARTESIAN_POINT ( 'NONE',  ( 1.660104986876641320, -0.05778040916215522460, 0.4822834645669289988 ) ) ;
#57509 = CARTESIAN_POINT ( 'NONE',  ( 1.509186351706037543, -0.4281496062992127816, -0.4176697321401328100 ) ) ;
#57510 = CARTESIAN_POINT ( 'NONE',  ( -0.6364829396325453192, -0.3162353388693405765, 0.4822834645669290543 ) ) ;
#57511 = CARTESIAN_POINT ( 'NONE',  ( 0.5314960629921264834, 0.1660481256975883668, -0.3530559997133364547 ) ) ;
#57512 = CARTESIAN_POINT ( 'NONE',  ( -0.6758530183727028406, 0.2952755905511811885, 0.1292274648535926551 ) ) ;
#57513 = CARTESIAN_POINT ( 'NONE',  ( -0.1049643490035307020, 0.3917322834645669549, -1.573490813648293907 ) ) ;
#57514 = CARTESIAN_POINT ( 'NONE',  ( -0.6824146981627288167, 0.1283753931104748280, 0.1820866141732283561 ) ) ;
#57515 = VERTEX_POINT ( 'NONE', #2288 ) ;
#57516 = CARTESIAN_POINT ( 'NONE',  ( 0.2891555358219910499, 0.2891555358219910499, -2.027559055118110631 ) ) ;
#57517 = ORIENTED_EDGE ( 'NONE', *, *, #63069, .F. ) ;
#57518 = CARTESIAN_POINT ( 'NONE',  ( -1.496062992125983815, -0.1870078740157480601, -0.3641732283464567677 ) ) ;
#57519 = CARTESIAN_POINT ( 'NONE',  ( -1.266404199475064773, -0.05778040916215560624, -0.4822834645669293319 ) ) ;
#57520 = CARTESIAN_POINT ( 'NONE',  ( -0.9317585301837263412, -0.4281496062992127816, -0.4176697321401328100 ) ) ;
#57521 = CARTESIAN_POINT ( 'NONE',  ( -0.1998031496062991907, -0.3460692066303959757, -0.06561679790026248016 ) ) ;
#57522 = CARTESIAN_POINT ( 'NONE',  ( -1.213910761154854745, 0.2952755905511810774, -0.1292274648535930714 ) ) ;
#57523 = CARTESIAN_POINT ( 'NONE',  ( -1.128608923884513837, -0.6046776061558807314, 0.2411417322834647770 ) ) ;
#57525 = CARTESIAN_POINT ( 'NONE',  ( -1.561679790026246017, -0.4281496062992127816, -0.4176697321401328100 ) ) ;
#57524 = B_SPLINE_CURVE_WITH_KNOTS ( 'NONE', 3,
 ( #12710, #56069, #76678, #23674 ),
 .UNSPECIFIED., .F., .F.,
 ( 4, 4 ),
 ( 0.02802642476679309200, 0.02831579184770149915 ),
 .UNSPECIFIED. ) ;
#57526 = CARTESIAN_POINT ( 'NONE',  ( -0.7989874411535504706, 0.02791078216816347476, -0.4328096321851898631 ) ) ;
#57527 = CARTESIAN_POINT ( 'NONE',  ( 0.3280839895013130669, -0.3690944881889765550, -0.3153832671262227771 ) ) ;
#57528 = CARTESIAN_POINT ( 'NONE',  ( 3.237502114873379799, 2.729657712569140582, 0.5314960629921260393 ) ) ;
#57529 = CARTESIAN_POINT ( 'NONE',  ( -0.3917322834645670104, -7.196005306013484475E-17, -0.2814960629921260393 ) ) ;
#57530 = CARTESIAN_POINT ( 'NONE',  ( -0.2559055118110230564, 0.07958543189024071263, -0.2665933059059888421 ) ) ;
#57531 = CARTESIAN_POINT ( 'NONE',  ( -0.8661417322834640276, -0.1870078740157479769, 0.4822834645669291653 ) ) ;
#57532 = CARTESIAN_POINT ( 'NONE',  ( 1.568241469816273437, -0.3162353388693405765, 0.4822834645669290543 ) ) ;
#57533 = CARTESIAN_POINT ( 'NONE',  ( -0.5380577427821514602, 0.05413385826771666132, 0.4176697321401328100 ) ) ;
#57534 = DIRECTION ( 'NONE',  ( 0.000000000000000000, -1.000000000000000000, -0.000000000000000000 ) ) ;
#57535 = EDGE_LOOP ( 'NONE', ( #18629, #65867, #57501, #6823 ) ) ;
#57536 = CARTESIAN_POINT ( 'NONE',  ( -0.3996062992125985480, -7.340648628747423112E-17, -2.163385826771653697 ) ) ;
#57537 = CARTESIAN_POINT ( 'NONE',  ( -0.6430446194225712953, 0.05413385826771626580, -0.4176697321401330321 ) ) ;
#57538 = CARTESIAN_POINT ( 'NONE',  ( 1.332020997375328974, -0.05778040916215560624, -0.4822834645669293319 ) ) ;
#57539 = CARTESIAN_POINT ( 'NONE',  ( -0.9776902887139098386, -0.5511811023622046335, 0.09757992244046803654 ) ) ;
#57540 = CARTESIAN_POINT ( 'NONE',  ( -1.450131233595799651, -0.6692913385826771977, 0.1292274648535927661 ) ) ;
#57541 = CARTESIAN_POINT ( 'NONE',  ( 0.2362204724409451007, -0.4091458600556402980, -0.7217847769028871152 ) ) ;
#57542 = CARTESIAN_POINT ( 'NONE',  ( 1.923693779251858693, 1.143166703770561732, 0.2643333500026358585 ) ) ;
#57543 = CARTESIAN_POINT ( 'NONE',  ( -0.3392501089628019995, 0.1958661417322832277, 0.1391076115485564701 ) ) ;
#57544 = CARTESIAN_POINT ( 'NONE',  ( -0.3917322834645669549, -0.1049643490035306603, -2.020341207349081181 ) ) ;
#57545 = CARTESIAN_POINT ( 'NONE',  ( -0.03280839895013062252, 0.2952755905511810774, -0.1292274648535930714 ) ) ;
#57546 = CARTESIAN_POINT ( 'NONE',  ( -1.213910761154854745, -0.5511811023622046335, 0.09757992244046803654 ) ) ;
#57547 = CARTESIAN_POINT ( 'NONE',  ( -0.7545931758530177724, 0.2952755905511811885, 0.1292274648535926551 ) ) ;
#57548 = CARTESIAN_POINT ( 'NONE',  ( -0.1265901696524986964, -0.4724409448818899238, -2.826115485564304475 ) ) ;
#57549 = CARTESIAN_POINT ( 'NONE',  ( -0.7020997375328076329, -0.3162353388693409650, -0.4822834645669289433 ) ) ;
#57550 = CARTESIAN_POINT ( 'NONE',  ( -0.9055118110236215490, 0.2952755905511811885, 0.000000000000000000 ) ) ;
#57551 = CARTESIAN_POINT ( 'NONE',  ( 0.1509186351706042484, -0.3162353388693405765, 0.4822834645669290543 ) ) ;
#57552 = CARTESIAN_POINT ( 'NONE',  ( 0.2891555358219910499, 0.2891555358219910499, -2.104330708661417138 ) ) ;
#57553 = CARTESIAN_POINT ( 'NONE',  ( 0.8595800524934390507, -0.08942795157528024563, -0.3641732283464568787 ) ) ;
#57554 = CARTESIAN_POINT ( 'NONE',  ( -0.7808398950131225646, -0.08942795157527998196, 0.3641732283464567121 ) ) ;
#57555 = CARTESIAN_POINT ( 'NONE',  ( 0.8792650918635177559, -0.004921259842519576551, 0.3153832671262227771 ) ) ;
#57556 = CARTESIAN_POINT ( 'NONE',  ( -1.660104986876639543, -0.05778040916215560624, -0.4822834645669293319 ) ) ;
#57557 = CARTESIAN_POINT ( 'NONE',  ( 1.279527559055118724, 0.1660481256975885056, 0.3530559997133364547 ) ) ;
#57558 = CARTESIAN_POINT ( 'NONE',  ( 0.4265091863517067594, 0.1771653543307087630, 0.09757992244046791164 ) ) ;
#57559 = CARTESIAN_POINT ( 'NONE',  ( -9.594673741351313045E-17, 0.3917322834645670104, -1.566929133858267820 ) ) ;
#57560 = CARTESIAN_POINT ( 'NONE',  ( -0.9186351706036736120, -0.6046776061558809534, -0.2411417322834644161 ) ) ;
#57561 = CARTESIAN_POINT ( 'NONE',  ( 1.122047244094488860, 0.1660481256975885056, 0.3530559997133364547 ) ) ;
#57562 = FACE_OUTER_BOUND ( 'NONE', #28954, .T. ) ;
#57563 = CARTESIAN_POINT ( 'NONE',  ( -0.07217847769028787330, -0.08942795157527998196, 0.3641732283464567121 ) ) ;
#57564 = CARTESIAN_POINT ( 'NONE',  ( -0.4052866537519759782, 0.02791078216816347476, -0.4328096321851898631 ) ) ;
#57565 = CARTESIAN_POINT ( 'NONE',  ( 0.3674540682414705883, -0.6046776061558807314, 0.2411417322834647770 ) ) ;
#57566 = CARTESIAN_POINT ( 'NONE',  ( 0.2319625946588665111, 0.1829408352246091884, 0.1465682319128801259 ) ) ;
#57567 = CARTESIAN_POINT ( 'NONE',  ( 0.8989501312335963501, -0.5511811023622048555, -0.09757992244046775898 ) ) ;
#57568 = CARTESIAN_POINT ( 'NONE',  ( 0.3149606299212603933, -0.1870078740157479769, 0.3641732283464567677 ) ) ;
#57569 = CARTESIAN_POINT ( 'NONE',  ( -0.07874015748031421014, -0.1870078740157479769, 0.4822834645669291653 ) ) ;
#57570 = CARTESIAN_POINT ( 'NONE',  ( -1.194225721784776262, 0.05413385826771626580, -0.4176697321401330321 ) ) ;
#57571 = CARTESIAN_POINT ( 'NONE',  ( -0.7349081364829387342, -0.5023911411419708095, 0.1820866141732285504 ) ) ;
#57572 = CARTESIAN_POINT ( 'NONE',  ( 2.795275590551181466, 1.062992125984252079, -2.156651478620225655E-16 ) ) ;
#57573 = CARTESIAN_POINT ( 'NONE',  ( -0.4461942257217840213, -0.6046776061558809534, -0.2411417322834644161 ) ) ;
#57574 = CARTESIAN_POINT ( 'NONE',  ( -0.1070741851644056997, 0.3996062992125984925, -1.343175853018372834 ) ) ;
#57575 = EDGE_CURVE ( 'NONE', #37133, #17817, #67906, .T. ) ;
#57576 = CARTESIAN_POINT ( 'NONE',  ( -0.1958661417322834220, -0.3392501089628018884, -2.354986876640420057 ) ) ;
#57577 = CARTESIAN_POINT ( 'NONE',  ( 0.03937007874015806264, 0.1771653543307087630, 0.000000000000000000 ) ) ;
#57578 = CARTESIAN_POINT ( 'NONE',  ( -0.3477690288713902178, 0.2952755905511810774, -0.1292274648535930714 ) ) ;
#57579 = CARTESIAN_POINT ( 'NONE',  ( -1.181102362204723644, -0.1870078740157479769, 0.4822834645669291653 ) ) ;
#57580 = CARTESIAN_POINT ( 'NONE',  ( -1.043307086614172041, -0.4536011799217367080, 0.2665933059059888421 ) ) ;
#57581 = DIRECTION ( 'NONE',  ( -1.953992523340275511E-14, -1.460819769243627131E-15, -1.000000000000000000 ) ) ;
#57582 = CARTESIAN_POINT ( 'NONE',  ( -0.3215223097112853146, -0.05778040916215560624, -0.4822834645669293319 ) ) ;
#57583 = CARTESIAN_POINT ( 'NONE',  ( -0.9776902887139098386, 0.1771653543307087075, -0.09757992244046823083 ) ) ;
#57584 = CARTESIAN_POINT ( 'NONE',  ( -1.391076115485563758, 0.1283753931104748280, 0.1820866141732283561 ) ) ;
#57585 = CARTESIAN_POINT ( 'NONE',  ( 1.253280839895013710, -0.3162353388693405765, 0.4822834645669290543 ) ) ;
#57586 = FACE_OUTER_BOUND ( 'NONE', #78504, .T. ) ;
#57587 = EDGE_CURVE ( 'NONE', #69925, #81066, #39691, .T. ) ;
#57588 = CARTESIAN_POINT ( 'NONE',  ( 4.797336870675656522E-17, -0.3917322834645670659, -1.965242412894699919 ) ) ;
#57589 = ORIENTED_EDGE ( 'NONE', *, *, #66351, .T. ) ;
#57590 = CARTESIAN_POINT ( 'NONE',  ( -0.2238009295390064879, -2.294479370626195693E-15, 0.3464511005275217603 ) ) ;
#57591 = CARTESIAN_POINT ( 'NONE',  ( -1.509186351706035767, 0.05413385826771626580, -0.4176697321401330321 ) ) ;
#57592 = CARTESIAN_POINT ( 'NONE',  ( -0.7414698162729651543, 0.2952755905511810774, -0.1292274648535930714 ) ) ;
#57593 = CARTESIAN_POINT ( 'NONE',  ( -1.496062992125983815, -0.1870078740157479769, 0.4822834645669291653 ) ) ;
#57594 = CARTESIAN_POINT ( 'NONE',  ( -0.3392501089628019995, 0.1958661417322832277, -2.000656167979002920 ) ) ;
#57595 = CARTESIAN_POINT ( 'NONE',  ( 0.05870088567680617486, 0.3874523867751286099, -1.220472440944882164 ) ) ;
#57596 = CARTESIAN_POINT ( 'NONE',  ( 1.115485564304462551, -0.4281496062992127816, -0.4176697321401328100 ) ) ;
#57597 = CARTESIAN_POINT ( 'NONE',  ( -0.03280839895013062252, 0.2952755905511810774, -0.1292274648535930714 ) ) ;
#57598 = DIRECTION ( 'NONE',  ( 0.000000000000000000, 0.000000000000000000, 1.000000000000000000 ) ) ;
#57599 = CARTESIAN_POINT ( 'NONE',  ( -0.7426113562967729953, 2.199547029020892275, -0.5309055118110235227 ) ) ;
#57600 = CARTESIAN_POINT ( 'NONE',  ( 1.108923884514436242, -0.08942795157527998196, 0.3641732283464567121 ) ) ;
#57601 = CARTESIAN_POINT ( 'NONE',  ( 0.2925321140481932369, 0.2925321140481932369, -1.240157480314960647 ) ) ;
#57602 = EDGE_LOOP ( 'NONE', ( #5266, #56288, #21918, #7104 ) ) ;
#57603 = CARTESIAN_POINT ( 'NONE',  ( -0.3392501089628019995, 0.1958661417322832277, -2.853018372703412187 ) ) ;
#57604 = ORIENTED_EDGE ( 'NONE', *, *, #65161, .F. ) ;
#57605 = CARTESIAN_POINT ( 'NONE',  ( -0.01312335958005186876, -0.4281496062992124485, 0.4176697321401328655 ) ) ;
#57606 = CARTESIAN_POINT ( 'NONE',  ( -0.6889763779527552368, -0.5400638737290845981, -0.3530559997133363437 ) ) ;
#57607 = CARTESIAN_POINT ( 'NONE',  ( -1.318897637795274802, 0.1660481256975885056, 0.3530559997133364547 ) ) ;
#57608 = CARTESIAN_POINT ( 'NONE',  ( 0.4986876640419954376, -0.6046776061558809534, -0.2411417322834644161 ) ) ;
#57609 = CARTESIAN_POINT ( 'NONE',  ( 1.673228346456693494, 0.1660481256975885056, 0.3530559997133364547 ) ) ;
#57610 = CARTESIAN_POINT ( 'NONE',  ( 1.581364829396326277, -0.05778040916215522460, 0.4822834645669289988 ) ) ;
#57611 = CARTESIAN_POINT ( 'NONE',  ( -0.5446194225721777693, -0.05778040916215522460, 0.4822834645669289988 ) ) ;
#57612 = CARTESIAN_POINT ( 'NONE',  ( 0.6430446194225728496, 0.05413385826771666132, 0.4176697321401328100 ) ) ;
#57613 = CARTESIAN_POINT ( 'NONE',  ( -1.627296587926508442, 0.2306618581243848609, 0.2411417322834645549 ) ) ;
#57614 = CARTESIAN_POINT ( 'NONE',  ( 1.286089238845145033, 0.2306618581243848609, 0.2411417322834645549 ) ) ;
#57615 = CARTESIAN_POINT ( 'NONE',  ( 0.3811282389481255306, 1.253478596003493095, -2.704694874393154702 ) ) ;
#57616 = CARTESIAN_POINT ( 'NONE',  ( -0.1246719160104980823, 0.2952755905511811885, 0.1292274648535926551 ) ) ;
#57617 = CARTESIAN_POINT ( 'NONE',  ( 0.3917322834645669549, 0.1049643490035304660, -0.2742782152230970327 ) ) ;
#57618 = CARTESIAN_POINT ( 'NONE',  ( 0.3543307086614181922, -0.5511811023622047445, 6.969142054262312111E-17 ) ) ;
#57619 = ORIENTED_EDGE ( 'NONE', *, *, #8988, .F. ) ;
#57620 = CARTESIAN_POINT ( 'NONE',  ( 0.3949938075777409963, 2.418639510665530435E-17, -0.4330708661417323468 ) ) ;
#57621 = ORIENTED_EDGE ( 'NONE', *, *, #45382, .T. ) ;
#57622 = CARTESIAN_POINT ( 'NONE',  ( -0.1968503937007867743, -0.5511811023622047445, 6.969142054262312111E-17 ) ) ;
#57623 = CARTESIAN_POINT ( 'NONE',  ( 2.873110008490984857, 1.063968899401425583, -0.03484477857462457695 ) ) ;
#57624 = CARTESIAN_POINT ( 'NONE',  ( -0.05905511811023545637, -0.5400638737290845981, -0.3530559997133363437 ) ) ;
#57625 = CARTESIAN_POINT ( 'NONE',  ( -0.1509186351706028884, -0.05778040916215522460, 0.4822834645669289988 ) ) ;
#57626 = CARTESIAN_POINT ( 'NONE',  ( -0.4330708661417315697, 0.2952755905511811885, 0.000000000000000000 ) ) ;
#57627 = CARTESIAN_POINT ( 'NONE',  ( -0.3392501089628017219, -0.1958661417322836995, -1.624035063813334956 ) ) ;
#57628 = CARTESIAN_POINT ( 'NONE',  ( -1.161417322834644716, 0.1660481256975885056, 0.3530559997133364547 ) ) ;
#57629 = CARTESIAN_POINT ( 'NONE',  ( -0.2867679344610364334, -0.2867679344610367109, -2.663385826771653253 ) ) ;
#57630 = CARTESIAN_POINT ( 'NONE',  ( 0.7020997375328090762, -0.08942795157528024563, -0.3641732283464568787 ) ) ;
#57631 = CARTESIAN_POINT ( 'NONE',  ( 1.062992125984252745, 0.2952755905511811885, 0.000000000000000000 ) ) ;
#57632 = CARTESIAN_POINT ( 'NONE',  ( 0.6364829396325465405, -0.3162353388693409650, -0.4822834645669289433 ) ) ;
#57633 = CARTESIAN_POINT ( 'NONE',  ( 0.3460692066303959757, -0.1998031496062991907, -1.049868766404199460 ) ) ;
#57634 = CARTESIAN_POINT ( 'NONE',  ( -1.397637795275589623, 0.1660481256975885056, 0.3530559997133364547 ) ) ;
#57635 = CARTESIAN_POINT ( 'NONE',  ( -0.1070741851644056997, 0.3996062992125984925, -0.8707349081364830212 ) ) ;
#57636 = CARTESIAN_POINT ( 'NONE',  ( -9.787531504996566615E-17, 0.3996062992125985480, -0.2342519685039370358 ) ) ;
#57637 = CARTESIAN_POINT ( 'NONE',  ( -0.3346456692913377662, -0.5400638737290844871, 0.3530559997133364547 ) ) ;
#57638 = CARTESIAN_POINT ( 'NONE',  ( 4.893765752498283924E-17, -0.3996062992125986035, -2.913385826771653697 ) ) ;
#57639 = CARTESIAN_POINT ( 'NONE',  ( -0.1049643490035302024, -0.3917322834645671215, -1.889107611548556109 ) ) ;
#57640 = CARTESIAN_POINT ( 'NONE',  ( -1.384514435695537005, -0.5511811023622048555, -0.09757992244046775898 ) ) ;
#57641 = CARTESIAN_POINT ( 'NONE',  ( 1.358267716535433323, -0.5400638737290845981, -0.3530559997133363437 ) ) ;
#57642 = CARTESIAN_POINT ( 'NONE',  ( 1.423884514435696413, -0.3162353388693409650, -0.4822834645669289433 ) ) ;
#57643 = CARTESIAN_POINT ( 'NONE',  ( 0.1377952755905518800, 0.07958543189024071263, -0.2665933059059888421 ) ) ;
#57644 = CARTESIAN_POINT ( 'NONE',  ( 1.062992125984252745, -0.6692913385826771977, 8.415575281601705876E-17 ) ) ;
#57645 = CARTESIAN_POINT ( 'NONE',  ( 0.3458507752293908943, -0.3458507752293908943, -1.592519685039370358 ) ) ;
#57646 = CARTESIAN_POINT ( 'NONE',  ( 0.1837270341207357105, -0.5023911411419708095, -0.1820866141732282451 ) ) ;
#57647 = CARTESIAN_POINT ( 'NONE',  ( 0.5708661417322841158, -0.5400638737290845981, -0.3530559997133363437 ) ) ;
#57648 = CARTESIAN_POINT ( 'NONE',  ( -0.1974969037888704149, -0.3420746716998661063, -1.087270341207349000 ) ) ;
#57649 = ADVANCED_FACE ( 'NONE', ( #9841 ), #46374, .F. ) ;
#57650 = CARTESIAN_POINT ( 'NONE',  ( -1.056430446194224881, 0.2952755905511810774, -0.1292274648535930714 ) ) ;
#57651 = CARTESIAN_POINT ( 'NONE',  ( 0.5511811023622054106, -0.1870078740157480601, -0.3641732283464567677 ) ) ;
#57652 = FACE_OUTER_BOUND ( 'NONE', #37274, .T. ) ;
#57653 = CARTESIAN_POINT ( 'NONE',  ( -0.4724409448818890911, -0.1870078740157479769, 0.4822834645669291653 ) ) ;
#57654 = CARTESIAN_POINT ( 'NONE',  ( -0.1837270341207340729, 0.1283753931104746893, -0.1820866141732285504 ) ) ;
#57655 = CARTESIAN_POINT ( 'NONE',  ( 3.184294706754630777, 2.755905511811024056, 0.5314960629921260393 ) ) ;
#57656 = CARTESIAN_POINT ( 'NONE',  ( -0.1968503937007867743, -0.6692913385826771977, 8.415575281601705876E-17 ) ) ;
#57657 = CARTESIAN_POINT ( 'NONE',  ( 0.4986876640419954376, 0.1283753931104748280, 0.1820866141732283561 ) ) ;
#57658 = CARTESIAN_POINT ( 'NONE',  ( 0.2925321140481932369, -0.2925321140481931814, -2.222440944881889813 ) ) ;
#57659 = CARTESIAN_POINT ( 'NONE',  ( -0.01968503937007793844, 0.1660481256975883668, -0.3530559997133364547 ) ) ;
#57660 = CARTESIAN_POINT ( 'NONE',  ( -0.3917322834645669549, -7.196005306013483243E-17, -1.851686720963567456 ) ) ;
#57661 = CARTESIAN_POINT ( 'NONE',  ( 1.167979002624672580, -0.3690944881889763329, 0.3153832671262228327 ) ) ;
#57662 = CARTESIAN_POINT ( 'NONE',  ( -0.1689764809739026374, 5.625543525484885637E-15, -0.3791475997938201781 ) ) ;
#57663 = AXIS2_PLACEMENT_3D ( 'NONE', #30210, #69352, #11284 ) ;
#57664 = CARTESIAN_POINT ( 'NONE',  ( -0.7414698162729651543, 0.1771653543307087075, -0.09757992244046823083 ) ) ;
#57665 = CARTESIAN_POINT ( 'NONE',  ( -0.7742782152230965886, -0.004921259842519576551, 0.3153832671262227771 ) ) ;
#57666 = CARTESIAN_POINT ( 'NONE',  ( -0.8464566929133852113, 0.1660481256975885056, 0.3530559997133364547 ) ) ;
#57667 = CARTESIAN_POINT ( 'NONE',  ( -0.2952755905511804668, 0.1660481256975885056, 0.3530559997133364547 ) ) ;
#57668 = CARTESIAN_POINT ( 'NONE',  ( 0.4527559055118117182, 0.07958543189024071263, -0.2665933059059888421 ) ) ;
#57669 = CARTESIAN_POINT ( 'NONE',  ( -0.2489951994332677276, 0.1588014424199898911, 5.622579823899913620 ) ) ;
#57670 = CARTESIAN_POINT ( 'NONE',  ( 1.358267716535433323, -0.4536011799217368745, -0.2665933059059886201 ) ) ;
#57671 = CARTESIAN_POINT ( 'NONE',  ( 0.7086614173228353852, -0.1870078740157479769, 0.4822834645669291653 ) ) ;
#57672 = CARTESIAN_POINT ( 'NONE',  ( 0.1998031496062994128, -0.3460692066303957537, -0.01115485564304462100 ) ) ;
#57673 = CARTESIAN_POINT ( 'NONE',  ( -0.3543307086614165824, -0.6692913385826771977, 8.415575281601705876E-17 ) ) ;
#57674 = CARTESIAN_POINT ( 'NONE',  ( 0.2867679344610365999, -0.2867679344610365444, -0.9704724409448820532 ) ) ;
#57675 = CARTESIAN_POINT ( 'NONE',  ( -1.692913385826770645, 0.2952755905511811885, 0.000000000000000000 ) ) ;
#57676 = CARTESIAN_POINT ( 'NONE',  ( 0.8136482939632553313, -0.6046776061558809534, -0.2411417322834644161 ) ) ;
#57677 = CARTESIAN_POINT ( 'NONE',  ( 0.3608923884514443348, -0.6692913385826771977, 0.1292274648535927661 ) ) ;
#57678 = CARTESIAN_POINT ( 'NONE',  ( -0.4705807874741004815, 1.475249678874074322, -3.908783329518705330 ) ) ;
#57679 = CARTESIAN_POINT ( 'NONE',  ( 0.2952755905511819101, 0.07958543189024071263, -0.2665933059059888421 ) ) ;
#57680 = CARTESIAN_POINT ( 'NONE',  ( 1.272965879265092637, -0.4281496062992127816, -0.4176697321401328100 ) ) ;
#57681 = CARTESIAN_POINT ( 'NONE',  ( -0.4855643044619415427, -0.3690944881889763329, 0.3153832671262228327 ) ) ;
#57682 = CARTESIAN_POINT ( 'NONE',  ( -0.6824146981627288167, 0.2306618581243848609, 0.2411417322834645549 ) ) ;
#57683 = DIRECTION ( 'NONE',  ( 1.000000000000000000, -0.000000000000000000, -0.000000000000000000 ) ) ;
#57684 = CARTESIAN_POINT ( 'NONE',  ( 0.05905511811023681640, 0.1660481256975883668, -0.3530559997133364547 ) ) ;
#57685 = CARTESIAN_POINT ( 'NONE',  ( -0.8530183727034112984, 0.05413385826771666132, 0.4176697321401328100 ) ) ;
#57686 = CARTESIAN_POINT ( 'NONE',  ( -0.8333333333333323711, -0.5511811023622048555, -0.09757992244046775898 ) ) ;
#57687 = CARTESIAN_POINT ( 'NONE',  ( 0.5249343832021003964, 0.2306618581243847221, -0.2411417322834647770 ) ) ;
#57688 = CARTESIAN_POINT ( 'NONE',  ( -1.122047244094487306, -0.5400638737290844871, 0.3530559997133364547 ) ) ;
#57689 = CARTESIAN_POINT ( 'NONE',  ( -0.1902887139107604098, 0.2952755905511810774, -0.1292274648535930714 ) ) ;
#57690 = FILL_AREA_STYLE_COLOUR ( '', #28125 ) ;
#57692 = CARTESIAN_POINT ( 'NONE',  ( 1.299212598425197429, 0.2952755905511811885, 0.000000000000000000 ) ) ;
#57691 = DIRECTION ( 'NONE',  ( 0.000000000000000000, 1.000000000000000000, 0.000000000000000000 ) ) ;
#57693 = CARTESIAN_POINT ( 'NONE',  ( 1.292650918635171564, -0.6692913385826773087, -0.1292274648535924053 ) ) ;
#57694 = CARTESIAN_POINT ( 'NONE',  ( 4.797336870675656522E-17, -0.3917322834645670104, -2.590551181102362044 ) ) ;
#57695 = CARTESIAN_POINT ( 'NONE',  ( -1.482939632545930975, 0.05413385826771666132, 0.4176697321401328100 ) ) ;
#57696 = CARTESIAN_POINT ( 'NONE',  ( -0.6955380577427815458, -0.4281496062992127816, -0.4176697321401328100 ) ) ;
#57697 = CARTESIAN_POINT ( 'NONE',  ( -0.3458507752293906723, -0.3458507752293910609, -0.3740157480314960092 ) ) ;
#57698 = CARTESIAN_POINT ( 'NONE',  ( -0.3996062992125986035, -7.340648628747425578E-17, -0.03937007874015750059 ) ) ;
#57699 = ORIENTED_EDGE ( 'NONE', *, *, #67786, .T. ) ;
#57700 = CARTESIAN_POINT ( 'NONE',  ( 0.09186351706036827158, -0.004921259842519576551, 0.3153832671262227771 ) ) ;
#57701 = CARTESIAN_POINT ( 'NONE',  ( -0.1049643490035307020, 0.3917322834645669549, -1.730971128608923992 ) ) ;
#57702 = CARTESIAN_POINT ( 'NONE',  ( 0.3083989501312343062, -0.3162353388693405765, 0.4822834645669290543 ) ) ;
#57703 = CARTESIAN_POINT ( 'NONE',  ( -0.4724409448818895907, -0.1265901696524993070, -2.880577427821522374 ) ) ;
#57704 = FACE_OUTER_BOUND ( 'NONE', #61594, .T. ) ;
#57705 = CARTESIAN_POINT ( 'NONE',  ( -0.4068241469816264999, -0.3690944881889763329, 0.3153832671262228327 ) ) ;
#57706 = CARTESIAN_POINT ( 'NONE',  ( 0.3740157480314966754, 0.1660481256975883391, -0.3530559997133364547 ) ) ;
#57707 = CARTESIAN_POINT ( 'NONE',  ( 1.259842519685040019, -0.1870078740157480879, -0.4822834645669291653 ) ) ;
#57708 = EDGE_CURVE ( 'NONE', #15414, #75751, #44963, .T. ) ;
#57709 = CARTESIAN_POINT ( 'NONE',  ( 0.7349081364829402885, -0.5023911411419708095, -0.1820866141732282451 ) ) ;
#57710 = CARTESIAN_POINT ( 'NONE',  ( 0.1706036745406830368, -0.4281496062992127816, -0.4176697321401328100 ) ) ;
#57711 = CARTESIAN_POINT ( 'NONE',  ( 0.1049643490035303689, 0.3917322834645668994, -0.8608730726696044444 ) ) ;
#57712 = CARTESIAN_POINT ( 'NONE',  ( -1.030183727034119867, -0.3162353388693405765, 0.4822834645669290543 ) ) ;
#57713 = CARTESIAN_POINT ( 'NONE',  ( -1.272965879265091305, -0.3690944881889763329, 0.3153832671262228327 ) ) ;
#57714 = CARTESIAN_POINT ( 'NONE',  ( -0.5314960629921254842, -0.5400638737290845981, -0.3530559997133363437 ) ) ;
#57715 = DIRECTION ( 'NONE',  ( 1.000000000000000000, -0.000000000000000000, -0.000000000000000000 ) ) ;
#57716 = FACE_OUTER_BOUND ( 'NONE', #28126, .T. ) ;
#57717 = ORIENTED_EDGE ( 'NONE', *, *, #35281, .T. ) ;
#57718 = CARTESIAN_POINT ( 'NONE',  ( 0.3917322834645670659, 2.398668435337828261E-17, -1.847132176674227688 ) ) ;
#57719 = CARTESIAN_POINT ( 'NONE',  ( 0.3083989501312343062, -0.05778040916215560624, -0.4822834645669293319 ) ) ;
#57720 = ORIENTED_EDGE ( 'NONE', *, *, #36884, .T. ) ;
#57721 = CARTESIAN_POINT ( 'NONE',  ( -0.6036745406824141069, 0.2306618581243848609, 0.2411417322834645549 ) ) ;
#57722 = CARTESIAN_POINT ( 'NONE',  ( 1.318897637795276356, 0.1660481256975883668, -0.3530559997133364547 ) ) ;
#57723 = CARTESIAN_POINT ( 'NONE',  ( 1.312335958005249825, 0.2306618581243847221, -0.2411417322834647770 ) ) ;
#57724 = CARTESIAN_POINT ( 'NONE',  ( 0.4855643044619428750, 0.05413385826771666132, 0.4176697321401328100 ) ) ;
#57725 = CARTESIAN_POINT ( 'NONE',  ( 0.2099737532808405305, -0.6046776061558807314, 0.2411417322834647770 ) ) ;
#57726 = CARTESIAN_POINT ( 'NONE',  ( -0.3917322834645669549, -0.1049643490035306603, -1.390419947506561504 ) ) ;
#57727 = CARTESIAN_POINT ( 'NONE',  ( -0.8858267716535425107, 0.1660481256975883668, -0.3530559997133364547 ) ) ;
#57728 = CARTESIAN_POINT ( 'NONE',  ( -0.1181102362204717315, -0.6692913385826771977, 8.415575281601705876E-17 ) ) ;
#57729 = CARTESIAN_POINT ( 'NONE',  ( -0.2099737532808391705, 0.1283753931104748280, 0.1820866141732283561 ) ) ;
#57730 = CARTESIAN_POINT ( 'NONE',  ( -0.2814587350932031828, -0.08983405572796258898, 5.548838678696989213 ) ) ;
#57731 = CARTESIAN_POINT ( 'NONE',  ( -0.07874015748031421014, -0.1870078740157480879, -0.4822834645669291653 ) ) ;
#57732 = CARTESIAN_POINT ( 'NONE',  ( -1.313877454013331780, 0.2755905511811023723, 0.7983292792091805090 ) ) ;
#57733 = CARTESIAN_POINT ( 'NONE',  ( 1.082677165354331228, -0.5400638737290844871, 0.3530559997133364547 ) ) ;
#57734 = CARTESIAN_POINT ( 'NONE',  ( 0.5052493438320215802, 0.2066929133858267931, 0.1054918080437490802 ) ) ;
#57735 = ORIENTED_EDGE ( 'NONE', *, *, #50179, .T. ) ;
#57736 = EDGE_CURVE ( 'NONE', #36842, #58460, #9427, .T. ) ;
#57737 = ORIENTED_EDGE ( 'NONE', *, *, #57803, .F. ) ;
#57738 = CARTESIAN_POINT ( 'NONE',  ( 0.4790026246719168435, -0.3162353388693409650, -0.4822834645669289433 ) ) ;
#57739 = CARTESIAN_POINT ( 'NONE',  ( -0.1837270341207343505, -0.5023911411419708095, 0.1820866141732285504 ) ) ;
#57741 = CARTESIAN_POINT ( 'NONE',  ( 0.3996062992125986035, 2.446882876249141962E-17, -1.220472440944881942 ) ) ;
#57740 = CARTESIAN_POINT ( 'NONE',  ( 1.594488188976378673, -0.4536011799217368745, -0.2665933059059886201 ) ) ;
#57742 = CARTESIAN_POINT ( 'NONE',  ( -0.1049643490035307020, 0.3917322834645669549, -1.193569553805774452 ) ) ;
#57743 = CARTESIAN_POINT ( 'NONE',  ( 0.1265901696524989462, 0.4724409448818897572, -0.3851706036745406458 ) ) ;
#57744 = CARTESIAN_POINT ( 'NONE',  ( 1.417322834645670104, -0.1870078740157480601, -0.3641732283464567677 ) ) ;
#57745 = CARTESIAN_POINT ( 'NONE',  ( 1.528871391076116026, -0.6692913385826773087, -0.1292274648535924053 ) ) ;
#57746 = CARTESIAN_POINT ( 'NONE',  ( -0.2891555358219911054, 0.2891555358219909388, 0.2185039370078739884 ) ) ;
#57747 = CARTESIAN_POINT ( 'NONE',  ( -0.1312335958005241554, 0.2306618581243848609, 0.2411417322834645549 ) ) ;
#57748 = CARTESIAN_POINT ( 'NONE',  ( -1.213910761154854745, -0.6692913385826771977, 0.1292274648535927661 ) ) ;
#57749 = CARTESIAN_POINT ( 'NONE',  ( -1.102362204724408601, -0.1870078740157479769, 0.4822834645669291653 ) ) ;
#57750 = CARTESIAN_POINT ( 'NONE',  ( 0.2493438320209980519, -0.4281496062992127816, -0.4176697321401328100 ) ) ;
#57751 = CARTESIAN_POINT ( 'NONE',  ( 0.3949938075777409963, 2.418639510665530743E-17, 0.1200787401574803376 ) ) ;
#57752 = CARTESIAN_POINT ( 'NONE',  ( 1.646981627296588035, -0.3162353388693405765, 0.4822834645669290543 ) ) ;
#57753 = CARTESIAN_POINT ( 'NONE',  ( 1.062992125984252745, -0.6692913385826771977, 8.415575281601705876E-17 ) ) ;
#57754 = CARTESIAN_POINT ( 'NONE',  ( 0.7611548556430454138, 0.1283753931104746893, -0.1820866141732285504 ) ) ;
#57755 = CARTESIAN_POINT ( 'NONE',  ( 0.3030237754406461814, 1.228860182587816929, 0.07866021050574804885 ) ) ;
#57756 = CARTESIAN_POINT ( 'NONE',  ( 0.9908136482939640111, -0.5511811023622046335, 0.09757992244046803654 ) ) ;
#57757 = CARTESIAN_POINT ( 'NONE',  ( -1.141732283464566011, 0.2952755905511811885, 0.000000000000000000 ) ) ;
#57758 = CARTESIAN_POINT ( 'NONE',  ( -0.3460692066303957537, -0.1998031496062994405, -0.9166666666666666297 ) ) ;
#57759 = CARTESIAN_POINT ( 'NONE',  ( 1.167979002624672580, -0.4281496062992124485, 0.4176697321401328655 ) ) ;
#57760 = CARTESIAN_POINT ( 'NONE',  ( 0.1958661417322834775, 0.3392501089628018884, -0.2939632545931757934 ) ) ;
#57762 = CARTESIAN_POINT ( 'NONE',  ( -0.4744094488189047332, 1.528796061338912882, 2.170146923806633765 ) ) ;
#57761 = CARTESIAN_POINT ( 'NONE',  ( 0.6430446194225729606, -0.4281496062992127816, -0.4176697321401328100 ) ) ;
#57763 = CARTESIAN_POINT ( 'NONE',  ( -1.620734908136482577, -0.5511811023622048555, -0.09757992244046775898 ) ) ;
#57764 = CARTESIAN_POINT ( 'NONE',  ( 0.05905511811023709395, -0.5400638737290844871, 0.3530559997133364547 ) ) ;
#57765 = CARTESIAN_POINT ( 'NONE',  ( 0.3083989501312343062, -0.2845877964562159024, 0.3641732283464567677 ) ) ;
#57766 = CARTESIAN_POINT ( 'NONE',  ( 0.8661417322834653598, -0.1870078740157479769, 0.4822834645669291653 ) ) ;
#57767 = CARTESIAN_POINT ( 'NONE',  ( -0.4417590601942997797, 1.710972922415816555, 2.103514684735031892 ) ) ;
#57768 = CARTESIAN_POINT ( 'NONE',  ( -0.7217847769028863381, -0.004921259842519870586, -0.3153832671262229437 ) ) ;
#57769 = CARTESIAN_POINT ( 'NONE',  ( -0.7874015748031489847, -0.1870078740157479769, 0.4822834645669291653 ) ) ;
#57770 = CARTESIAN_POINT ( 'NONE',  ( 1.620734908136483465, -0.6692913385826771977, 0.1292274648535927661 ) ) ;
#57771 = CARTESIAN_POINT ( 'NONE',  ( -0.9842519685039365918, -0.6692913385826771977, 8.415575281601705876E-17 ) ) ;
#57772 = CARTESIAN_POINT ( 'NONE',  ( 0.9055118110236227702, 0.2952755905511811885, 0.000000000000000000 ) ) ;
#57773 = CARTESIAN_POINT ( 'NONE',  ( -1.404199475065615932, -0.3690944881889765550, -0.3153832671262227771 ) ) ;
#57774 = CARTESIAN_POINT ( 'NONE',  ( 1.063938142021821021, 1.224083459767688176, 0.3565564186812866243 ) ) ;
#57775 = CARTESIAN_POINT ( 'NONE',  ( 0.8333333333333340365, 0.2952755905511810774, -0.1292274648535930714 ) ) ;
#57776 = CARTESIAN_POINT ( 'NONE',  ( 0.2362204724409449064, 0.4091458600556404646, -2.583333333333333481 ) ) ;
#57777 = CARTESIAN_POINT ( 'NONE',  ( -1.482939632545930975, -0.4281496062992127816, -0.4176697321401328100 ) ) ;
#57778 = CARTESIAN_POINT ( 'NONE',  ( -1.351706036745406347, -0.3690944881889763329, 0.3153832671262228327 ) ) ;
#57779 = CARTESIAN_POINT ( 'NONE',  ( -1.227034120734907585, 0.1771653543307087630, 0.09757992244046791164 ) ) ;
#57780 = CARTESIAN_POINT ( 'NONE',  ( 1.522309711286089939, 0.1283753931104748280, 0.1820866141732283561 ) ) ;
#57781 = CARTESIAN_POINT ( 'NONE',  ( -0.3215223097112853146, -0.05778040916215560624, -0.4822834645669293319 ) ) ;
#57782 = CARTESIAN_POINT ( 'NONE',  ( -0.3805774278215216522, -0.004921259842519576551, 0.3153832671262227771 ) ) ;
#57783 = CARTESIAN_POINT ( 'NONE',  ( -1.633858267716534529, -0.4536011799217368745, -0.2665933059059886201 ) ) ;
#57784 = CARTESIAN_POINT ( 'NONE',  ( 0.8005249343832027131, -0.004921259842519576551, 0.3153832671262227771 ) ) ;
#57785 = CARTESIAN_POINT ( 'NONE',  ( 0.3805774278215230400, -0.4281496062992124485, 0.4176697321401328655 ) ) ;
#57786 = CARTESIAN_POINT ( 'NONE',  ( 1.614173228346457378, 0.2952755905511811885, 0.000000000000000000 ) ) ;
#57787 = CARTESIAN_POINT ( 'NONE',  ( 0.6036745406824154392, 0.2306618581243847221, -0.2411417322834647770 ) ) ;
#57788 = CARTESIAN_POINT ( 'NONE',  ( 0.4790026246719167324, -0.08942795157527998196, 0.3641732283464567121 ) ) ;
#57789 = CARTESIAN_POINT ( 'NONE',  ( -1.607611548556429737, 0.2952755905511810774, -0.1292274648535930714 ) ) ;
#57790 = CARTESIAN_POINT ( 'NONE',  ( -1.240157480314959759, -0.5400638737290845981, -0.3530559997133363437 ) ) ;
#57791 = CARTESIAN_POINT ( 'NONE',  ( -0.3149606299212590610, -0.1870078740157479769, 0.4822834645669291653 ) ) ;
#57792 = CARTESIAN_POINT ( 'NONE',  ( -0.3996062992125986035, -7.340648628747425578E-17, -0.1968503937007874405 ) ) ;
#57793 = CARTESIAN_POINT ( 'NONE',  ( -0.2925321140481930149, -0.2925321140481933480, -2.498031496062992574 ) ) ;
#57794 = CARTESIAN_POINT ( 'NONE',  ( 0.5052493438320215802, 0.2952755905511811885, 0.1292274648535926551 ) ) ;
#57795 = CARTESIAN_POINT ( 'NONE',  ( 1.194225721784777594, -0.3690944881889765550, -0.3153832671262227771 ) ) ;
#57796 = CARTESIAN_POINT ( 'NONE',  ( -0.5052493438320203589, 0.2952755905511810774, -0.1292274648535930714 ) ) ;
#57797 = CARTESIAN_POINT ( 'NONE',  ( 0.2755905511811031494, -0.6692913385826771977, 8.415575281601705876E-17 ) ) ;
#57798 = CARTESIAN_POINT ( 'NONE',  ( -0.3996062992125987146, 0.1070741851644051862, -2.080052493438320216 ) ) ;
#57799 = CARTESIAN_POINT ( 'NONE',  ( 0.1058382717557499880, 0.3949938075777411073, -2.040682414698163250 ) ) ;
#57800 = CARTESIAN_POINT ( 'NONE',  ( -0.2867679344610365999, 0.2867679344610364889, -0.4842519685039369248 ) ) ;
#57801 = DIRECTION ( 'NONE',  ( 0.000000000000000000, 0.000000000000000000, -1.000000000000000000 ) ) ;
#57802 = CARTESIAN_POINT ( 'NONE',  ( -0.2867679344610364334, -0.2867679344610367109, -0.9960629921259841479 ) ) ;
#57803 = EDGE_CURVE ( 'NONE', #35701, #21301, #43650, .T. ) ;
#57804 = CARTESIAN_POINT ( 'NONE',  ( -0.8202099737532801971, -0.5511811023622046335, 0.09757992244046803654 ) ) ;
#57805 = CARTESIAN_POINT ( 'NONE',  ( -1.187664041994750175, -0.05778040916215560624, -0.4822834645669293319 ) ) ;
#57806 = CARTESIAN_POINT ( 'NONE',  ( -0.1974969037888704149, -0.3420746716998661063, -2.662073490813648746 ) ) ;
#57807 = CARTESIAN_POINT ( 'NONE',  ( 0.5314960629921267055, -0.5400638737290844871, 0.3530559997133364547 ) ) ;
#57808 = CARTESIAN_POINT ( 'NONE',  ( 1.463254593175853824, 0.2952755905511810774, -0.1292274648535930714 ) ) ;
#57809 = CARTESIAN_POINT ( 'NONE',  ( 0.8267716535433077274, 0.2952755905511811885, 0.000000000000000000 ) ) ;
#57810 = CARTESIAN_POINT ( 'NONE',  ( 0.1265901696524990294, -0.4724409448818896462, -2.762467191601049255 ) ) ;
#57811 = CARTESIAN_POINT ( 'NONE',  ( 0.3460692066303959202, 0.1998031496062993295, -2.178477690288713742 ) ) ;
#57812 = CARTESIAN_POINT ( 'NONE',  ( 0.1958661417322834775, 0.3392501089628018884, -0.6135363761492932388 ) ) ;
#57813 = CARTESIAN_POINT ( 'NONE',  ( 1.568241469816273659, -0.05778040916215560624, -0.4822834645669293319 ) ) ;
#57814 = CARTESIAN_POINT ( 'NONE',  ( 0.6561679790026253567, 0.2306618581243848609, 0.2411417322834645549 ) ) ;
#57815 = CARTESIAN_POINT ( 'NONE',  ( 0.04593175853018440641, 0.2952755905511810774, -0.1292274648535930714 ) ) ;
#57816 = CARTESIAN_POINT ( 'NONE',  ( 0.7217847769028878924, -0.3690944881889765550, -0.3153832671262227771 ) ) ;
#57817 = CARTESIAN_POINT ( 'NONE',  ( 1.437007874015748810, -0.5400638737290845981, -0.3530559997133363437 ) ) ;
#57818 = CARTESIAN_POINT ( 'NONE',  ( 4.797336870675656522E-17, -0.3917322834645670104, -0.3208661417322835607 ) ) ;
#57819 = CARTESIAN_POINT ( 'NONE',  ( 0.6496062992125991586, 0.1660481256975885056, 0.3530559997133364547 ) ) ;
#57820 = CARTESIAN_POINT ( 'NONE',  ( 1.194225721784777594, 0.05413385826771666132, 0.4176697321401328100 ) ) ;
#57821 = CARTESIAN_POINT ( 'NONE',  ( 0.1902887139107617975, -0.6692913385826773087, -0.1292274648535924053 ) ) ;
#57822 = CARTESIAN_POINT ( 'NONE',  ( 1.062992125984252745, 0.1771653543307087630, 0.000000000000000000 ) ) ;
#57823 = CARTESIAN_POINT ( 'NONE',  ( -0.7283464566929126471, 0.1660481256975883668, -0.3530559997133364547 ) ) ;
#57824 = CARTESIAN_POINT ( 'NONE',  ( -0.9251968503937002541, 0.1660481256975885056, 0.3530559997133364547 ) ) ;
#57825 = CARTESIAN_POINT ( 'NONE',  ( 1.095800524934383846, -0.3162353388693405765, 0.4822834645669290543 ) ) ;
#57826 = CARTESIAN_POINT ( 'NONE',  ( -0.3917322834645671215, 0.1049643490035301469, -0.7473753280839893209 ) ) ;
#57827 = CARTESIAN_POINT ( 'NONE',  ( -0.3917322834645670104, -7.196005306013484475E-17, -1.448818897637795367 ) ) ;
#57828 = CARTESIAN_POINT ( 'NONE',  ( 4.797336870675656522E-17, -0.3917322834645670104, -2.590551181102362044 ) ) ;
#57829 = ORIENTED_EDGE ( 'NONE', *, *, #71814, .F. ) ;
#57830 = CARTESIAN_POINT ( 'NONE',  ( 0.1070741851644053527, 0.3996062992125986590, -0.1509186351706036655 ) ) ;
#57831 = ORIENTED_EDGE ( 'NONE', *, *, #27922, .T. ) ;
#57832 = DIRECTION ( 'NONE',  ( -0.000000000000000000, -1.000000000000000000, -0.000000000000000000 ) ) ;
#57833 = CARTESIAN_POINT ( 'NONE',  ( 0.8727034120734912248, -0.2845877964562161244, -0.3641732283464567121 ) ) ;
#57834 = CARTESIAN_POINT ( 'NONE',  ( 0.1070741851644054915, -0.3996062992125986035, -1.345144356955380704 ) ) ;
#57835 = CARTESIAN_POINT ( 'NONE',  ( 1.430446194225722500, -0.3690944881889765550, -0.3153832671262227771 ) ) ;
#57836 = DIRECTION ( 'NONE',  ( 0.7071067811865524577, 0.000000000000000000, 0.7071067811865425767 ) ) ;
#57837 = CARTESIAN_POINT ( 'NONE',  ( -0.3813326747118357951, 1.253753238304356810, 2.704466544682207374 ) ) ;
#57838 = CARTESIAN_POINT ( 'NONE',  ( -2.154527559055114061, 0.03937007874015747977, -0.4677827689125148014 ) ) ;
#57839 = CARTESIAN_POINT ( 'NONE',  ( -0.1049643490035307020, 0.3917322834645669549, -1.036089238845144589 ) ) ;
#57840 = CARTESIAN_POINT ( 'NONE',  ( -0.9580052493438311334, -0.004921259842519870586, -0.3153832671262229437 ) ) ;
#57841 = CARTESIAN_POINT ( 'NONE',  ( -1.581364829396324945, -0.2845877964562159024, 0.3641732283464567677 ) ) ;
#57842 = ADVANCED_FACE ( 'NONE', ( #66683 ), #54023, .T. ) ;
#57843 = CARTESIAN_POINT ( 'NONE',  ( -1.437007874015747477, 0.1660481256975883668, -0.3530559997133364547 ) ) ;
#57844 = CARTESIAN_POINT ( 'NONE',  ( -0.05905511811023545637, -0.5400638737290845981, -0.3530559997133363437 ) ) ;
#57845 = CARTESIAN_POINT ( 'NONE',  ( 1.351706036745407458, -0.4281496062992127816, -0.4176697321401328100 ) ) ;
#57846 = VERTEX_POINT ( 'NONE', #62010 ) ;
#57847 = AXIS2_PLACEMENT_3D ( 'NONE', #43652, #63035, #18429 ) ;
#57848 = CARTESIAN_POINT ( 'NONE',  ( -1.114781747626346187, -2.609869883881465018E-15, -0.3464511005275220379 ) ) ;
#57849 = CARTESIAN_POINT ( 'NONE',  ( -0.3458507752293909498, 0.3458507752293907833, -2.066929133858267154 ) ) ;
#57850 = DIRECTION ( 'NONE',  ( 0.000000000000000000, -1.000000000000000000, 0.000000000000000000 ) ) ;
#57851 = CARTESIAN_POINT ( 'NONE',  ( 0.2017716535433070613, 0.2017716535433070613, -0.3937007874015748254 ) ) ;
#57852 = CARTESIAN_POINT ( 'NONE',  ( -1.030183727034119867, -0.2845877964562159024, 0.3641732283464567677 ) ) ;
#57853 = CARTESIAN_POINT ( 'NONE',  ( -1.299212598425196097, 0.2952755905511811885, 0.000000000000000000 ) ) ;
#57854 = CARTESIAN_POINT ( 'NONE',  ( 0.7545931758530189937, 0.2952755905511810774, -0.1292274648535930714 ) ) ;
#57855 = VERTEX_POINT ( 'NONE', #56506 ) ;
#57857 = CARTESIAN_POINT ( 'NONE',  ( 0.4677827689124922084, 0.03937007874015747977, -2.154527559055118946 ) ) ;
#57856 = CARTESIAN_POINT ( 'NONE',  ( -0.4724409448818896462, -0.1265901696524993070, -2.484908136482939955 ) ) ;
#57858 = ADVANCED_FACE ( 'NONE', ( #17004 ), #10680, .F. ) ;
#57859 = CARTESIAN_POINT ( 'NONE',  ( 1.148293963254593875, -0.6692913385826771977, 0.1292274648535927661 ) ) ;
#57860 = CARTESIAN_POINT ( 'NONE',  ( -1.227034120734907585, 0.2952755905511811885, 0.1292274648535926551 ) ) ;
#57861 = CARTESIAN_POINT ( 'NONE',  ( 0.2867679344610365999, 0.2867679344610365999, -0.6902693981289222958 ) ) ;
#57862 = CARTESIAN_POINT ( 'NONE',  ( -0.5708661417322828946, 0.07958543189024071263, -0.2665933059059888421 ) ) ;
#57863 = CARTESIAN_POINT ( 'NONE',  ( -0.1049643490035301885, -0.3917322834645671215, -0.9442257217847769279 ) ) ;
#57864 = EDGE_CURVE ( 'NONE', #78494, #37713, #78281, .T. ) ;
#57865 = CARTESIAN_POINT ( 'NONE',  ( -0.3215223097112853146, -0.08942795157528024563, -0.3641732283464568787 ) ) ;
#57866 = CARTESIAN_POINT ( 'NONE',  ( -0.06561679790026180015, -0.3690944881889765550, -0.3153832671262227771 ) ) ;
#57867 = VECTOR ( 'NONE', #70231, 39.37007874015748143 ) ;
#57868 = CARTESIAN_POINT ( 'NONE',  ( 0.2690288713910767848, -0.6692913385826773087, -0.1292274648535924053 ) ) ;
#57869 = CARTESIAN_POINT ( 'NONE',  ( -0.9448818897637790704, -0.1870078740157480601, -0.3641732283464567677 ) ) ;
#57870 = CARTESIAN_POINT ( 'NONE',  ( -0.3917322834645670104, -7.196005306013484475E-17, -2.866141732283464361 ) ) ;
#57871 = CARTESIAN_POINT ( 'NONE',  ( 1.325459317585302665, 0.05413385826771626580, -0.4176697321401330321 ) ) ;
#57872 = CARTESIAN_POINT ( 'NONE',  ( -1.430446194225720724, 0.05413385826771626580, -0.4176697321401330321 ) ) ;
#57873 = CARTESIAN_POINT ( 'NONE',  ( 0.1265901696524990294, -0.4724409448818896462, -1.264435695538057569 ) ) ;
#57874 = CARTESIAN_POINT ( 'NONE',  ( -0.2165354330708654795, -0.5400638737290845981, -0.3530559997133363437 ) ) ;
#57875 = CARTESIAN_POINT ( 'NONE',  ( -0.8727034120734901146, -0.3162353388693405765, 0.4822834645669290543 ) ) ;
#57876 = CARTESIAN_POINT ( 'NONE',  ( 0.9580052493438327987, -0.3690944881889765550, -0.3153832671262227771 ) ) ;
#57877 = CARTESIAN_POINT ( 'NONE',  ( -0.2559055118110230564, 0.07958543189024071263, -0.2665933059059888421 ) ) ;
#57878 = CARTESIAN_POINT ( 'NONE',  ( -0.7611548556430438595, 0.2306618581243848609, 0.2411417322834645549 ) ) ;
#57879 = CARTESIAN_POINT ( 'NONE',  ( 1.594488188976378673, -0.5400638737290845981, -0.3530559997133363437 ) ) ;
#57880 = DIRECTION ( 'NONE',  ( 0.000000000000000000, -1.000000000000000000, -0.000000000000000000 ) ) ;
#57881 = CARTESIAN_POINT ( 'NONE',  ( 1.220472440944882608, 0.1771653543307087630, 0.000000000000000000 ) ) ;
#57882 = CARTESIAN_POINT ( 'NONE',  ( -0.4265091863517051496, -0.6692913385826771977, 0.1292274648535927661 ) ) ;
#57883 = CARTESIAN_POINT ( 'NONE',  ( -1.568241469816272105, -0.05778040916215522460, 0.4822834645669289988 ) ) ;
#57884 = VERTEX_POINT ( 'NONE', #62418 ) ;
#57885 = EDGE_CURVE ( 'NONE', #24806, #72153, #65197, .T. ) ;
#57886 = CARTESIAN_POINT ( 'NONE',  ( -0.1070741851644056997, 0.3996062992125984925, -2.445538057742782101 ) ) ;
#57887 = CARTESIAN_POINT ( 'NONE',  ( -0.8923884514435688198, -0.5023911411419708095, 0.1820866141732285504 ) ) ;
#57888 = CARTESIAN_POINT ( 'NONE',  ( 0.9186351706036751663, -0.6046776061558807314, 0.2411417322834647770 ) ) ;
#57889 = CARTESIAN_POINT ( 'NONE',  ( -1.227034120734907585, 0.1771653543307087630, 0.09757992244046791164 ) ) ;
#57890 = CARTESIAN_POINT ( 'NONE',  ( -0.3996062992125986590, 0.1070741851644051723, -1.211942257217847541 ) ) ;
#57891 = CARTESIAN_POINT ( 'NONE',  ( -0.8923884514435688198, 0.2306618581243847221, -0.2411417322834647770 ) ) ;
#57892 = CARTESIAN_POINT ( 'NONE',  ( 0.7152230971128616943, -0.05778040916215522460, 0.4822834645669289988 ) ) ;
#57893 = CARTESIAN_POINT ( 'NONE',  ( 0.5905511811023629321, 0.2952755905511811885, 0.000000000000000000 ) ) ;
#57894 = CARTESIAN_POINT ( 'NONE',  ( 1.535433070866142335, -0.6692913385826771977, 8.415575281601705876E-17 ) ) ;
#57895 = CARTESIAN_POINT ( 'NONE',  ( -1.594488188976377563, -0.4536011799217367080, 0.2665933059059888421 ) ) ;
#57896 = CARTESIAN_POINT ( 'NONE',  ( -0.3996062992125986035, 0.1070741851644051584, -0.7395013123359578389 ) ) ;
#57898 = ADVANCED_FACE ( 'NONE', ( #80977 ), #17108, .T. ) ;
#57897 = CARTESIAN_POINT ( 'NONE',  ( -0.2925321140481930704, -0.2925321140481933480, -0.8464566929133857665 ) ) ;
#57899 = CARTESIAN_POINT ( 'NONE',  ( -9.674558042662121740E-17, 0.3949938075777409963, -0.1574803149606300023 ) ) ;
#57900 = CARTESIAN_POINT ( 'NONE',  ( 0.4670403427555926967, 1.622209144264177283, 2.571698080334799297 ) ) ;
#57901 = CARTESIAN_POINT ( 'NONE',  ( 1.220472440944882608, 0.1771653543307087630, 0.000000000000000000 ) ) ;
#57902 = CARTESIAN_POINT ( 'NONE',  ( 0.3937007874015754361, -0.1870078740157480601, -0.3641732283464567677 ) ) ;
#57903 = AXIS2_PLACEMENT_3D ( 'NONE', #41515, #16688, #80668 ) ;
#57904 = CARTESIAN_POINT ( 'NONE',  ( 0.2690288713910767848, -0.6692913385826773087, -0.1292274648535924053 ) ) ;
#57905 = CARTESIAN_POINT ( 'NONE',  ( 1.167979002624672580, 0.05413385826771626580, -0.4176697321401330321 ) ) ;
#57906 = CARTESIAN_POINT ( 'NONE',  ( -0.3949938075777408852, -0.1058382717557502933, -1.382545931758530688 ) ) ;
#57907 = CARTESIAN_POINT ( 'NONE',  ( 0.4724409448818904789, -0.1870078740157480601, -0.3641732283464567677 ) ) ;
#57908 = EDGE_CURVE ( 'NONE', #16375, #43096, #36073, .T. ) ;
#57909 = CARTESIAN_POINT ( 'NONE',  ( -0.7414698162729651543, -0.6692913385826771977, 0.1292274648535927661 ) ) ;
#57910 = CARTESIAN_POINT ( 'NONE',  ( -1.437007874015747477, 0.1660481256975883668, -0.3530559997133364547 ) ) ;
#57911 = CARTESIAN_POINT ( 'NONE',  ( 0.7677165354330716118, 0.1660481256975883668, -0.3530559997133364547 ) ) ;
#57912 = CARTESIAN_POINT ( 'NONE',  ( -0.4724409448818895907, -0.1265901696524993070, -1.620734908136482799 ) ) ;
#57913 = LINE ( 'NONE', #57499, #38470 ) ;
#57914 = EDGE_LOOP ( 'NONE', ( #18418, #73624, #46751 ) ) ;
#57915 = ORIENTED_EDGE ( 'NONE', *, *, #66595, .F. ) ;
#57916 = CARTESIAN_POINT ( 'NONE',  ( -1.286089238845143479, -0.6046776061558807314, 0.2411417322834647770 ) ) ;
#57917 = CARTESIAN_POINT ( 'NONE',  ( -0.7217847769028863381, -0.4281496062992124485, 0.4176697321401328655 ) ) ;
#57919 = CARTESIAN_POINT ( 'NONE',  ( -0.6496062992125976043, 0.1660481256975883668, -0.3530559997133364547 ) ) ;
#57918 = CARTESIAN_POINT ( 'NONE',  ( -0.9514435695538050464, -0.08942795157528024563, -0.3641732283464568787 ) ) ;
#57920 = CARTESIAN_POINT ( 'NONE',  ( 0.3917322834645668994, 0.1049643490035304522, -1.779508243273278945 ) ) ;
#57921 = CARTESIAN_POINT ( 'NONE',  ( -0.1998031496062991630, -0.3460692066303959202, -2.819553805774277944 ) ) ;
#57922 = CARTESIAN_POINT ( 'NONE',  ( -1.496062992125983815, -0.1870078740157479769, 0.3641732283464567677 ) ) ;
#57923 = CARTESIAN_POINT ( 'NONE',  ( -1.404199475065615932, 0.05413385826771666132, 0.4176697321401328100 ) ) ;
#57924 = CARTESIAN_POINT ( 'NONE',  ( 0.5052493438320215802, 0.2952755905511811885, 0.1292274648535926551 ) ) ;
#57925 = CARTESIAN_POINT ( 'NONE',  ( -0.6561679790026240244, 0.2306618581243847221, -0.2411417322834647770 ) ) ;
#57926 = CARTESIAN_POINT ( 'NONE',  ( 0.1049643490035303689, 0.3917322834645670104, -1.560367454068241511 ) ) ;
#57927 = CARTESIAN_POINT ( 'NONE',  ( -0.6955380577427815458, -0.004921259842519576551, 0.3153832671262227771 ) ) ;
#57928 = VERTEX_POINT ( 'NONE', #39834 ) ;
#57929 = CARTESIAN_POINT ( 'NONE',  ( 0.2891555358219910499, -0.2891555358219909944, -1.988188976377952777 ) ) ;
#57930 = ORIENTED_EDGE ( 'NONE', *, *, #22777, .T. ) ;
#57931 = CARTESIAN_POINT ( 'NONE',  ( -1.509186351706035767, -0.004921259842519870586, -0.3153832671262229437 ) ) ;
#57932 = CARTESIAN_POINT ( 'NONE',  ( -1.279527559055116948, 0.1660481256975883668, -0.3530559997133364547 ) ) ;
#57933 = CARTESIAN_POINT ( 'NONE',  ( -0.9448818897637790704, -0.1870078740157480879, -0.4822834645669291653 ) ) ;
#57934 = CARTESIAN_POINT ( 'NONE',  ( 0.1070741851644053527, 0.3996062992125986590, -0.3083989501312335846 ) ) ;
#57935 = CARTESIAN_POINT ( 'NONE',  ( -1.062992125984250968, 0.2952755905511811885, 0.000000000000000000 ) ) ;
#57936 = CARTESIAN_POINT ( 'NONE',  ( -1.384514435695537005, 0.2952755905511811885, 0.1292274648535926551 ) ) ;
#57937 = DIRECTION ( 'NONE',  ( -1.000000000000000000, 0.000000000000000000, -0.000000000000000000 ) ) ;
#57938 = CARTESIAN_POINT ( 'NONE',  ( 0.4461942257217856311, 0.1283753931104746893, -0.1820866141732285504 ) ) ;
#57939 = CARTESIAN_POINT ( 'NONE',  ( -0.005429349025308751603, 1.062992125984252745, -1.442783214386379020 ) ) ;
#57940 = CARTESIAN_POINT ( 'NONE',  ( 0.3392501089628018329, 0.1958661417322835607, -0.5308398950131234528 ) ) ;
#57941 = CARTESIAN_POINT ( 'NONE',  ( -0.3674540682414692561, -0.5023911411419708095, -0.1820866141732282451 ) ) ;
#57942 = CARTESIAN_POINT ( 'NONE',  ( -0.8792650918635160906, -0.4281496062992124485, 0.4176697321401328655 ) ) ;
#57943 = CARTESIAN_POINT ( 'NONE',  ( 1.292650918635171564, 0.2952755905511811885, 0.1292274648535926551 ) ) ;
#57944 = CARTESIAN_POINT ( 'NONE',  ( -0.4855643044619415427, 0.05413385826771626580, -0.4176697321401330321 ) ) ;
#57945 = VERTEX_POINT ( 'NONE', #77302 ) ;
#57946 = ORIENTED_EDGE ( 'NONE', *, *, #19828, .F. ) ;
#57947 = CARTESIAN_POINT ( 'NONE',  ( 0.1070741851644054776, -0.3996062992125984925, -2.051837270341206665 ) ) ;
#57948 = CARTESIAN_POINT ( 'NONE',  ( -0.8923884514435688198, -0.6046776061558807314, 0.2411417322834647770 ) ) ;
#57949 = CARTESIAN_POINT ( 'NONE',  ( 1.437007874015748810, 0.1660481256975885056, 0.3530559997133364547 ) ) ;
#57950 = CARTESIAN_POINT ( 'NONE',  ( -1.174540682414697335, -0.2845877964562161244, -0.3641732283464567121 ) ) ;
#57951 = CARTESIAN_POINT ( 'NONE',  ( -1.259842519685038686, -0.1870078740157479769, 0.4822834645669291653 ) ) ;
#57952 = CARTESIAN_POINT ( 'NONE',  ( -0.2362204724409451284, 0.4091458600556402425, -0.6430446194225721834 ) ) ;
#57953 = CARTESIAN_POINT ( 'NONE',  ( -2.170146923806675954, 1.554943921348594049, 0.4744094488188970171 ) ) ;
#57954 = CARTESIAN_POINT ( 'NONE',  ( 0.1049643490035304938, -0.3917322834645669549, -0.3923884514435695414 ) ) ;
#57955 = CARTESIAN_POINT ( 'NONE',  ( 0.000000000000000000, 0.000000000000000000, 0.000000000000000000 ) ) ;
#57956 = CARTESIAN_POINT ( 'NONE',  ( 0.2230971128608932319, -0.4281496062992124485, 0.4176697321401328655 ) ) ;
#57957 = CARTESIAN_POINT ( 'NONE',  ( -1.082677165354329896, -0.4536011799217368745, -0.2665933059059886201 ) ) ;
#57958 = CARTESIAN_POINT ( 'NONE',  ( -0.6167979002624665030, 0.05413385826771666132, 0.4176697321401328100 ) ) ;
#57959 = CARTESIAN_POINT ( 'NONE',  ( -0.2362204724409447953, -0.4091458600556404646, -2.819553805774277944 ) ) ;
#57960 = CARTESIAN_POINT ( 'NONE',  ( -1.371391076115484831, 0.2952755905511810774, -0.1292274648535930714 ) ) ;
#57961 = EDGE_CURVE ( 'NONE', #9709, #77311, #70562, .T. ) ;
#57962 = CARTESIAN_POINT ( 'NONE',  ( -1.076115485564303809, 0.2306618581243848609, 0.2411417322834645549 ) ) ;
#57963 = CARTESIAN_POINT ( 'NONE',  ( 0.07874015748031558404, -0.1870078740157480879, -0.4822834645669291653 ) ) ;
#57964 = CARTESIAN_POINT ( 'NONE',  ( 0.3420746716998660508, 0.1974969037888705814, -2.727690288713910949 ) ) ;
#57965 = CARTESIAN_POINT ( 'NONE',  ( 1.023622047244095112, -0.1870078740157480601, -0.3641732283464567677 ) ) ;
#57966 = CARTESIAN_POINT ( 'NONE',  ( -0.7480314960629914633, 0.1771653543307087630, 0.000000000000000000 ) ) ;
#57967 = CARTESIAN_POINT ( 'NONE',  ( -0.08704787641669393949, 1.071034085402255309, -1.469981051961803287 ) ) ;
#57968 = CARTESIAN_POINT ( 'NONE',  ( 0.8858267716535438430, 0.07958543189024085140, 0.2665933059059887866 ) ) ;
#57969 = CARTESIAN_POINT ( 'NONE',  ( 1.528871391076116026, -0.5511811023622048555, -0.09757992244046775898 ) ) ;
#57970 = AXIS2_PLACEMENT_3D ( 'NONE', #59516, #14095, #39747 ) ;
#57971 = CARTESIAN_POINT ( 'NONE',  ( 1.325459317585302665, 0.05413385826771626580, -0.4176697321401330321 ) ) ;
#57972 = UNCERTAINTY_MEASURE_WITH_UNIT (LENGTH_MEASURE( 1.000000000000000082E-05 ), #38360, 'distance_accuracy_value', 'NONE');
#57973 = CARTESIAN_POINT ( 'NONE',  ( -0.006561679790025524116, -0.08942795157528024563, -0.3641732283464568787 ) ) ;
#57974 = CARTESIAN_POINT ( 'NONE',  ( -0.2867679344610364334, -0.2867679344610367109, -1.468503937007874294 ) ) ;
#57975 = CARTESIAN_POINT ( 'NONE',  ( -1.017060367454067249, -0.05778040916215522460, 0.4822834645669289988 ) ) ;
#57976 = CARTESIAN_POINT ( 'NONE',  ( 1.384514435695538337, -0.6692913385826771977, 0.1292274648535927661 ) ) ;
#57977 = DIRECTION ( 'NONE',  ( -5.372046893347524115E-15, 0.000000000000000000, 1.000000000000000000 ) ) ;
#57978 = CARTESIAN_POINT ( 'NONE',  ( -0.5446194225721777693, -0.08942795157527998196, 0.3641732283464567121 ) ) ;
#57979 = DIRECTION ( 'NONE',  ( 0.000000000000000000, 0.000000000000000000, -1.000000000000000000 ) ) ;
#57980 = CARTESIAN_POINT ( 'NONE',  ( 0.1246719160104994284, 0.2952755905511810774, -0.1292274648535930714 ) ) ;
#57981 = CARTESIAN_POINT ( 'NONE',  ( -1.033875059083676717, 1.724409448818897905, -0.4359958488159722534 ) ) ;
#57982 = CARTESIAN_POINT ( 'NONE',  ( 0.9973753280839902091, 0.1283753931104746893, -0.1820866141732285504 ) ) ;
#57983 = CARTESIAN_POINT ( 'NONE',  ( 0.2230971128608929543, -0.004921259842519870586, -0.3153832671262229437 ) ) ;
#57984 = CARTESIAN_POINT ( 'NONE',  ( 0.3083989501312343062, -0.05778040916215560624, -0.4822834645669293319 ) ) ;
#57985 = CARTESIAN_POINT ( 'NONE',  ( -1.259842519685038686, -0.1870078740157479769, 0.4822834645669291653 ) ) ;
#57986 = CARTESIAN_POINT ( 'NONE',  ( -0.7677165354330699465, -0.4536011799217368745, -0.2665933059059886201 ) ) ;
#57987 = CARTESIAN_POINT ( 'NONE',  ( 0.000000000000000000, 0.000000000000000000, 0.1574803149606299191 ) ) ;
#57988 = CARTESIAN_POINT ( 'NONE',  ( -0.8202099737532799750, 0.2952755905511810774, -0.1292274648535930714 ) ) ;
#57989 = CARTESIAN_POINT ( 'NONE',  ( -0.3996062992125985480, -7.340648628747423112E-17, -1.061023622047243986 ) ) ;
#57990 =( BOUNDED_CURVE ( )  B_SPLINE_CURVE ( 2, ( #49076, #74777, #17128, #42760, #55798, #36868, #62544, #4882, #30556, #56222, #51537, #76820, #13688 ),
 .UNSPECIFIED., .F., .F. ) 
 B_SPLINE_CURVE_WITH_KNOTS ( ( 3, 2, 2, 2, 2, 2, 3 ),
 ( 0.6853969023887781509, 0.6856060606060606633, 0.6893939393939394478, 0.6931818181818182323, 0.6969696969696970168, 0.7007575757575758013, 0.7009667339748582027 ),
 .UNSPECIFIED. ) 
 CURVE ( )  GEOMETRIC_REPRESENTATION_ITEM ( )  RATIONAL_B_SPLINE_CURVE ( ( 0.9964447847208419695, 0.9981185001348091834, 1.000000000000000000, 0.9659258262890683122, 1.000000000000000000, 0.9659258262890683122, 1.000000000000000000, 0.9659258262890683122, 1.000000000000000000, 0.9659258262890683122, 1.000000000000000000, 0.9981185001348101826, 0.9964447847208438569 ) ) 
 REPRESENTATION_ITEM ( '' )  );
#57991 = CARTESIAN_POINT ( 'NONE',  ( -0.3392501089628019995, 0.1958661417322832277, -2.473097112860892288 ) ) ;
#57992 = CARTESIAN_POINT ( 'NONE',  ( 0.2690288713910767848, -0.5511811023622048555, -0.09757992244046775898 ) ) ;
#57993 = CARTESIAN_POINT ( 'NONE',  ( -0.7020997375328074108, -0.05778040916215522460, 0.4822834645669289988 ) ) ;
#57994 = CARTESIAN_POINT ( 'NONE',  ( -1.200787401574802349, -0.5400638737290844871, 0.3530559997133364547 ) ) ;
#57995 = CARTESIAN_POINT ( 'NONE',  ( -1.397637795275589623, -0.4536011799217368745, -0.2665933059059886201 ) ) ;
#57996 = CARTESIAN_POINT ( 'NONE',  ( 1.555118110236221041, 0.1660481256975883668, -0.3530559997133364547 ) ) ;
#57997 = CARTESIAN_POINT ( 'NONE',  ( -0.3083989501312330295, -0.3162353388693409650, -0.4822834645669289433 ) ) ;
#57998 = CARTESIAN_POINT ( 'NONE',  ( -0.7152230971128602510, -0.2845877964562159024, 0.3641732283464567677 ) ) ;
#57999 = CARTESIAN_POINT ( 'NONE',  ( -1.614173228346456268, -0.5511811023622047445, 6.969142054262312111E-17 ) ) ;
#58000 = CARTESIAN_POINT ( 'NONE',  ( 1.351706036745407458, -0.4281496062992127816, -0.4176697321401328100 ) ) ;
#58001 = CARTESIAN_POINT ( 'NONE',  ( -0.3460692066303960868, 0.1998031496062990242, 0.1312335958005249048 ) ) ;
#58002 = CARTESIAN_POINT ( 'NONE',  ( 0.3917322834645670659, -0.1049643490035303273, -1.998050811844831243 ) ) ;
#58003 = ORIENTED_EDGE ( 'NONE', *, *, #5997, .F. ) ;
#58004 = DIRECTION ( 'NONE',  ( -8.881784197001252323E-16, 0.000000000000000000, 1.000000000000000000 ) ) ;
#58005 = CARTESIAN_POINT ( 'NONE',  ( 1.437007874015748810, 0.07958543189024085140, 0.2665933059059887866 ) ) ;
#58006 = CARTESIAN_POINT ( 'NONE',  ( -0.7349081364829390672, 0.2306618581243847221, -0.2411417322834647770 ) ) ;
#58007 = CARTESIAN_POINT ( 'NONE',  ( -1.581364829396324945, -0.05778040916215560624, -0.4822834645669293319 ) ) ;
#58008 = CARTESIAN_POINT ( 'NONE',  ( -0.3392501089628017219, -0.1958661417322836718, -2.184383202099737797 ) ) ;
#58009 = CARTESIAN_POINT ( 'NONE',  ( 1.653543307086614789, -0.1870078740157479769, 0.3641732283464567677 ) ) ;
#58010 = CARTESIAN_POINT ( 'NONE',  ( 0.6299212598425204535, -0.1870078740157480879, -0.4822834645669291653 ) ) ;
#58011 = CARTESIAN_POINT ( 'NONE',  ( 0.2165354330708668673, -0.5400638737290844871, 0.3530559997133364547 ) ) ;
#58012 = DIRECTION ( 'NONE',  ( 1.000000000000000000, 0.000000000000000000, 0.000000000000000000 ) ) ;
#58013 = CARTESIAN_POINT ( 'NONE',  ( -0.7426113562972000981, 2.401574803149605586, 0.5309055118110236338 ) ) ;
#58014 = CARTESIAN_POINT ( 'NONE',  ( 0.8530183727034126306, -0.004921259842519870586, -0.3153832671262229437 ) ) ;
#58015 = CARTESIAN_POINT ( 'NONE',  ( 0.2925321140481932369, 0.2925321140481932369, -1.397637795275590067 ) ) ;
#58016 = ORIENTED_EDGE ( 'NONE', *, *, #25337, .F. ) ;
#58017 = CARTESIAN_POINT ( 'NONE',  ( -0.3917322834645671215, 0.1049643490035301469, -2.859580052493438274 ) ) ;
#58018 = ORIENTED_EDGE ( 'NONE', *, *, #21915, .T. ) ;
#58019 = CARTESIAN_POINT ( 'NONE',  ( -0.1443569553805768291, 0.05413385826771666132, 0.4176697321401328100 ) ) ;
#58020 = PRODUCT_DEFINITION_SHAPE ( 'NONE', 'NONE',  #38279 ) ;
#58021 = CARTESIAN_POINT ( 'NONE',  ( -1.522309711286088607, -0.6046776061558807314, 0.2411417322834647770 ) ) ;
#58022 = CARTESIAN_POINT ( 'NONE',  ( 0.6627296587926517768, -0.6692913385826773087, -0.1292274648535924053 ) ) ;
#58023 = CARTESIAN_POINT ( 'NONE',  ( 1.089238845144357759, 0.05413385826771626580, -0.4176697321401330321 ) ) ;
#58024 = CARTESIAN_POINT ( 'NONE',  ( 1.463254593175853824, 0.2952755905511810774, -0.1292274648535930714 ) ) ;
#58025 = CARTESIAN_POINT ( 'NONE',  ( -0.3215223097112853146, -0.05778040916215560624, -0.4822834645669293319 ) ) ;
#58026 = CARTESIAN_POINT ( 'NONE',  ( -0.07217847769028813698, -0.3162353388693409650, -0.4822834645669289433 ) ) ;
#58027 = CARTESIAN_POINT ( 'NONE',  ( 1.522309711286089939, -0.6046776061558809534, -0.2411417322834644161 ) ) ;
#58028 = AXIS2_PLACEMENT_3D ( 'NONE', #56456, #70756, #51367 ) ;
#58029 = CARTESIAN_POINT ( 'NONE',  ( 1.489501312335958172, -0.05778040916215560624, -0.4822834645669293319 ) ) ;
#58030 = CARTESIAN_POINT ( 'NONE',  ( 1.673228346456693494, 0.1660481256975885056, 0.3530559997133364547 ) ) ;
#58031 = CARTESIAN_POINT ( 'NONE',  ( -0.3018372703412066094, 0.05413385826771666132, 0.4176697321401328100 ) ) ;
#58032 = CARTESIAN_POINT ( 'NONE',  ( 0.1958661417322836440, -0.3392501089628017219, -0.2414698162729658204 ) ) ;
#58033 = CARTESIAN_POINT ( 'NONE',  ( 0.6036745406824154392, 0.1283753931104746893, -0.1820866141732285504 ) ) ;
#58034 = EDGE_LOOP ( 'NONE', ( #17916, #51151, #74936, #57197 ) ) ;
#58035 = CARTESIAN_POINT ( 'NONE',  ( 4.837279021331060870E-17, -0.3949938075777409963, -0.5511811023622048555 ) ) ;
#58036 = ORIENTED_EDGE ( 'NONE', *, *, #12851, .T. ) ;
#58037 = CARTESIAN_POINT ( 'NONE',  ( -0.5446194225721777693, -0.2845877964562161244, -0.3641732283464567121 ) ) ;
#58038 = CARTESIAN_POINT ( 'NONE',  ( 2.610350574616482788, 1.379859446982311777, -0.4477348144951681652 ) ) ;
#58039 = CARTESIAN_POINT ( 'NONE',  ( 0.1640419947506569498, -0.05778040916215522460, 0.4822834645669289988 ) ) ;
#58040 = CARTESIAN_POINT ( 'NONE',  ( -0.1706036745406816491, -0.4281496062992124485, 0.4176697321401328655 ) ) ;
#58041 = CARTESIAN_POINT ( 'NONE',  ( -0.8792650918635160906, 0.05413385826771626580, -0.4176697321401330321 ) ) ;
#58042 = CARTESIAN_POINT ( 'NONE',  ( 0.3917322834645670659, -0.1049643490035303273, -1.525609866962941430 ) ) ;
#58043 = CARTESIAN_POINT ( 'NONE',  ( -1.318897637795274802, 0.1660481256975885056, 0.3530559997133364547 ) ) ;
#58044 = CARTESIAN_POINT ( 'NONE',  ( -1.614173228346456712, 1.543375672658095610, -0.1372047244094478091 ) ) ;
#58045 = CARTESIAN_POINT ( 'NONE',  ( 0.9186351706036751663, -0.5023911411419708095, 0.1820866141732285504 ) ) ;
#58046 = CARTESIAN_POINT ( 'NONE',  ( 0.3346456692913393205, -0.5400638737290845981, -0.3530559997133363437 ) ) ;
#58047 = CARTESIAN_POINT ( 'NONE',  ( 0.5971128608923891301, 0.2952755905511810774, -0.1292274648535930714 ) ) ;
#58048 = CARTESIAN_POINT ( 'NONE',  ( 4.893765752498283924E-17, -0.3996062992125986035, -1.181102362204724310 ) ) ;
#58049 = CARTESIAN_POINT ( 'NONE',  ( 0.3260583142159772518, 2.726622551019859153E-15, 0.3954974714151457960 ) ) ;
#58050 = CARTESIAN_POINT ( 'NONE',  ( -0.3996062992125985480, -7.340648628747423112E-17, -0.5885826771653542844 ) ) ;
#58051 = CARTESIAN_POINT ( 'NONE',  ( 4.893765752498283308E-17, -0.3996062992125985480, -0.1555118110236220763 ) ) ;
#58052 = CARTESIAN_POINT ( 'NONE',  ( -0.3083989501312330295, -0.05778040916215522460, 0.4822834645669289988 ) ) ;
#58053 = CARTESIAN_POINT ( 'NONE',  ( 0.3996062992125986035, 2.446882876249141962E-17, -2.637795275590551380 ) ) ;
#58054 = CARTESIAN_POINT ( 'NONE',  ( -0.1958661417322836718, 0.3392501089628017219, -2.145013123359580387 ) ) ;
#58055 = CARTESIAN_POINT ( 'NONE',  ( -1.325459317585300889, -0.004921259842519576551, 0.3153832671262227771 ) ) ;
#58056 = CARTESIAN_POINT ( 'NONE',  ( 1.325459317585302665, 0.05413385826771626580, -0.4176697321401330321 ) ) ;
#58057 = CARTESIAN_POINT ( 'NONE',  ( 1.233595800524935227, 0.2306618581243847221, -0.2411417322834647770 ) ) ;
#58058 = CARTESIAN_POINT ( 'NONE',  ( 0.3280839895013130669, -0.3690944881889765550, -0.3153832671262227771 ) ) ;
#58059 = CARTESIAN_POINT ( 'NONE',  ( 0.6692913385826777528, 0.2952755905511811885, 0.000000000000000000 ) ) ;
#58060 = CARTESIAN_POINT ( 'NONE',  ( -0.1265901696524986964, -0.4724409448818899238, -1.566272965879265344 ) ) ;
#58061 = CARTESIAN_POINT ( 'NONE',  ( 0.3149606299212606708, -0.1870078740157480601, -0.3641732283464567677 ) ) ;
#58062 = CARTESIAN_POINT ( 'NONE',  ( 0.1574803149606306130, -0.1870078740157479769, 0.4822834645669291653 ) ) ;
#58063 = CARTESIAN_POINT ( 'NONE',  ( 4.837279021331061486E-17, -0.3949938075777409963, -1.257874015748031260 ) ) ;
#58064 = CARTESIAN_POINT ( 'NONE',  ( -1.010498687664041384, -0.4281496062992127816, -0.4176697321401328100 ) ) ;
#58065 = CARTESIAN_POINT ( 'NONE',  ( 0.7152230971128614723, -0.2845877964562161244, -0.3641732283464567121 ) ) ;
#58066 = DIRECTION ( 'NONE',  ( 0.000000000000000000, -1.000000000000000000, 0.000000000000000000 ) ) ;
#58067 = CARTESIAN_POINT ( 'NONE',  ( -0.5511811023622041894, -0.1870078740157480879, -0.4822834645669291653 ) ) ;
#58068 = B_SPLINE_CURVE_WITH_KNOTS ( 'NONE', 3,
 ( #65802, #46829, #20760, #46410 ),
 .UNSPECIFIED., .F., .F.,
 ( 4, 4 ),
 ( 0.1177794994733336598, 0.1192034014685218191 ),
 .UNSPECIFIED. ) ;
#58069 = CARTESIAN_POINT ( 'NONE',  ( -0.4986876640419939388, 0.1283753931104746893, -0.1820866141732285504 ) ) ;
#58070 = CARTESIAN_POINT ( 'NONE',  ( 0.000000000000000000, 0.000000000000000000, 0.000000000000000000 ) ) ;
#58071 = CARTESIAN_POINT ( 'NONE',  ( -0.1837270341207343505, -0.6046776061558807314, 0.2411417322834647770 ) ) ;
#58072 = CARTESIAN_POINT ( 'NONE',  ( -0.2755905511811015396, -0.6692913385826771977, 8.415575281601705876E-17 ) ) ;
#58073 = CARTESIAN_POINT ( 'NONE',  ( 0.5314960629921264834, 0.07958543189024071263, -0.2665933059059888421 ) ) ;
#58074 = CARTESIAN_POINT ( 'NONE',  ( 0.1998031496062992463, 0.3460692066303959202, -2.268372703412073754 ) ) ;
#58075 = CARTESIAN_POINT ( 'NONE',  ( -0.1115485564304453947, -0.6692913385826771977, 0.1292274648535927661 ) ) ;
#58076 = CARTESIAN_POINT ( 'NONE',  ( -0.1049643490035301746, -0.3917322834645670659, -1.569534489992439497 ) ) ;
#58077 = CARTESIAN_POINT ( 'NONE',  ( 0.8727034120734913358, -0.08942795157527998196, 0.3641732283464567121 ) ) ;
#58078 = CARTESIAN_POINT ( 'NONE',  ( 1.305774278215223960, 0.2952755905511810774, -0.1292274648535930714 ) ) ;
#58079 = CARTESIAN_POINT ( 'NONE',  ( -1.003937007874015297, -0.4536011799217368745, -0.2665933059059886201 ) ) ;
#58080 = CARTESIAN_POINT ( 'NONE',  ( -0.8333333333333323711, -0.5511811023622048555, -0.09757992244046775898 ) ) ;
#58081 = CARTESIAN_POINT ( 'NONE',  ( -0.8661417322834640276, -0.1870078740157479769, 0.4822834645669291653 ) ) ;
#58082 = CARTESIAN_POINT ( 'NONE',  ( -0.1902887139107604098, -0.6692913385826771977, 0.1292274648535927661 ) ) ;
#58083 = CARTESIAN_POINT ( 'NONE',  ( 0.6167979002624679463, -0.004921259842519870586, -0.3153832671262229437 ) ) ;
#58084 = CARTESIAN_POINT ( 'NONE',  ( 0.2362204724409449064, 0.4091458600556404646, -2.349081364829396446 ) ) ;
#58085 = CARTESIAN_POINT ( 'NONE',  ( 1.122047244094488860, 0.07958543189024085140, 0.2665933059059887866 ) ) ;
#58086 = AXIS2_PLACEMENT_3D ( 'NONE', #14371, #39174, #45479 ) ;
#58087 = CARTESIAN_POINT ( 'NONE',  ( 0.8530183727034128527, -0.4281496062992124485, 0.4176697321401328655 ) ) ;
#58088 = CARTESIAN_POINT ( 'NONE',  ( -0.3460692066303960313, 0.1998031496062989965, 0.05446194225721784354 ) ) ;
#58089 = CARTESIAN_POINT ( 'NONE',  ( -0.2165354330708654795, -0.5400638737290845981, -0.3530559997133363437 ) ) ;
#58090 = CARTESIAN_POINT ( 'NONE',  ( -0.3917322834645669549, -0.1049643490035306603, -1.232939632545931863 ) ) ;
#58091 = CARTESIAN_POINT ( 'NONE',  ( -1.712598425196849572, 0.1660481256975885056, 0.3530559997133364547 ) ) ;
#58092 = CARTESIAN_POINT ( 'NONE',  ( 0.5314960629921267055, -0.5400638737290844871, 0.3530559997133364547 ) ) ;
#58093 = CARTESIAN_POINT ( 'NONE',  ( 0.3083989501312343062, -0.05778040916215560624, -0.4822834645669293319 ) ) ;
#58094 = CARTESIAN_POINT ( 'NONE',  ( 0.000000000000000000, 0.000000000000000000, 6.062992125984251857 ) ) ;
#58095 = CARTESIAN_POINT ( 'NONE',  ( 0.5577427821522316087, -0.08942795157527998196, 0.3641732283464567121 ) ) ;
#58096 = CARTESIAN_POINT ( 'NONE',  ( 0.9645669291338591078, -0.5400638737290845981, -0.3530559997133363437 ) ) ;
#58097 = CARTESIAN_POINT ( 'NONE',  ( -0.1968503937007867743, -0.5511811023622047445, 6.969142054262312111E-17 ) ) ;
#58098 = CARTESIAN_POINT ( 'NONE',  ( -0.6627296587926501115, 0.2952755905511810774, -0.1292274648535930714 ) ) ;
#58099 = CARTESIAN_POINT ( 'NONE',  ( 0.8561328129276796206, 8.471767977567108961E-16, -0.4445507791589058955 ) ) ;
#58100 = CARTESIAN_POINT ( 'NONE',  ( -0.2034120734908131112, -0.6692913385826773087, -0.1292274648535924053 ) ) ;
#58101 = CARTESIAN_POINT ( 'NONE',  ( -1.417322834645668772, -0.1870078740157480879, -0.4822834645669291653 ) ) ;
#58102 = CARTESIAN_POINT ( 'NONE',  ( -0.7480314960629914633, 0.1771653543307087630, 0.000000000000000000 ) ) ;
#58103 = CARTESIAN_POINT ( 'NONE',  ( 0.5511811023622054106, -0.1870078740157480879, -0.4822834645669291653 ) ) ;
#58104 = CARTESIAN_POINT ( 'NONE',  ( -1.358267716535432434, 0.1660481256975883668, -0.3530559997133364547 ) ) ;
#58105 = CARTESIAN_POINT ( 'NONE',  ( -0.5118110236220466680, 0.2952755905511811885, 0.000000000000000000 ) ) ;
#58106 = CARTESIAN_POINT ( 'NONE',  ( 0.4741708390789288186, 1.554782515222133954, -2.169554433241255520 ) ) ;
#58108 = CARTESIAN_POINT ( 'NONE',  ( 1.509186351706037543, -0.4281496062992127816, -0.4176697321401328100 ) ) ;
#58107 = DIRECTION ( 'NONE',  ( 0.000000000000000000, -1.000000000000000000, 0.000000000000000000 ) ) ;
#58109 = CARTESIAN_POINT ( 'NONE',  ( 1.489501312335958172, -0.3162353388693405765, 0.4822834645669290543 ) ) ;
#58110 = CARTESIAN_POINT ( 'NONE',  ( 0.2867679344610366554, -0.2867679344610365444, -2.452755905511810663 ) ) ;
#58111 = CARTESIAN_POINT ( 'NONE',  ( -0.03443470937339725840, 0.2755905511811023723, -1.320480459168889897 ) ) ;
#58112 = CARTESIAN_POINT ( 'NONE',  ( -1.286089238845143479, -0.6046776061558807314, 0.2411417322834647770 ) ) ;
#58113 = CARTESIAN_POINT ( 'NONE',  ( 0.3458507752293908943, 0.3458507752293908943, -0.7677165354330709457 ) ) ;
#58114 = CARTESIAN_POINT ( 'NONE',  ( -0.3996062992125987146, 0.1070741851644051862, 0.1246719160104986790 ) ) ;
#58115 = ORIENTED_EDGE ( 'NONE', *, *, #9984, .F. ) ;
#58116 = CARTESIAN_POINT ( 'NONE',  ( 0.04593175853018440641, -0.5511811023622046335, 0.09757992244046803654 ) ) ;
#58117 = CARTESIAN_POINT ( 'NONE',  ( 0.1049643490035303689, 0.3917322834645670104, -1.717847769028871596 ) ) ;
#58118 = ORIENTED_EDGE ( 'NONE', *, *, #12124, .F. ) ;
#58119 = CARTESIAN_POINT ( 'NONE',  ( 0.09842519685039434474, -0.5400638737290845981, -0.3530559997133363437 ) ) ;
#58120 = CARTESIAN_POINT ( 'NONE',  ( 0.4002624671916016896, -0.3162353388693409650, -0.4822834645669289433 ) ) ;
#58121 = CARTESIAN_POINT ( 'NONE',  ( 0.4091458600556404646, -0.2362204724409448231, -2.782152230971128848 ) ) ;
#58122 = FACE_OUTER_BOUND ( 'NONE', #21845, .T. ) ;
#58123 = CARTESIAN_POINT ( 'NONE',  ( -0.2755905511811015396, -0.5511811023622047445, 6.969142054262312111E-17 ) ) ;
#58124 = CARTESIAN_POINT ( 'NONE',  ( 0.3249695492770460770, 1.223219560026271499E-15, 0.4445507791589056734 ) ) ;
#58125 = CARTESIAN_POINT ( 'NONE',  ( 0.9120734908136490793, 0.2952755905511810774, -0.1292274648535930714 ) ) ;
#58126 = CARTESIAN_POINT ( 'NONE',  ( 0.8989501312335963501, -0.5511811023622048555, -0.09757992244046775898 ) ) ;
#58127 = CARTESIAN_POINT ( 'NONE',  ( -0.6233595800524928121, -0.3162353388693409650, -0.4822834645669289433 ) ) ;
#58128 = CARTESIAN_POINT ( 'NONE',  ( -0.2867679344610364334, -0.2867679344610368219, -1.241450500491126707 ) ) ;
#58129 = CARTESIAN_POINT ( 'NONE',  ( -0.9055118110236215490, -0.6692913385826771977, 8.415575281601705876E-17 ) ) ;
#58130 = CARTESIAN_POINT ( 'NONE',  ( -1.286089238845143479, -0.5023911411419708095, 0.1820866141732285504 ) ) ;
#58131 = CARTESIAN_POINT ( 'NONE',  ( -1.023622047244094002, -0.1870078740157480879, -0.4822834645669291653 ) ) ;
#58132 = CARTESIAN_POINT ( 'NONE',  ( 1.496062992125985147, -0.1870078740157479769, 0.4822834645669291653 ) ) ;
#58133 = CARTESIAN_POINT ( 'NONE',  ( -0.4314295484911011003, 1.339559522712173267, -2.086640540083727124 ) ) ;
#58134 = ORIENTED_EDGE ( 'NONE', *, *, #57357, .F. ) ;
#58135 = CARTESIAN_POINT ( 'NONE',  ( -0.2867679344610365444, -0.2867679344610367664, -2.575478633367141779 ) ) ;
#58136 = CARTESIAN_POINT ( 'NONE',  ( 0.1181102362204730916, 0.2952755905511811885, 0.000000000000000000 ) ) ;
#58137 = ORIENTED_EDGE ( 'NONE', *, *, #31097, .T. ) ;
#58138 = CARTESIAN_POINT ( 'NONE',  ( -0.9580052493438311334, -0.4281496062992124485, 0.4176697321401328655 ) ) ;
#58139 = CARTESIAN_POINT ( 'NONE',  ( 1.581364829396326277, -0.05778040916215522460, 0.4822834645669289988 ) ) ;
#58140 = CARTESIAN_POINT ( 'NONE',  ( 1.102362204724410155, -0.1870078740157479769, 0.4822834645669291653 ) ) ;
#58141 = CARTESIAN_POINT ( 'NONE',  ( 0.06561679790026316017, 0.05413385826771626580, -0.4176697321401330321 ) ) ;
#58142 = CIRCLE ( 'NONE', #21878, 0.5118110236220472231 ) ;
#58143 = CARTESIAN_POINT ( 'NONE',  ( 0.06561679790026316017, -0.4281496062992124485, 0.4176697321401328655 ) ) ;
#58144 = CARTESIAN_POINT ( 'NONE',  ( -0.1049643490035302024, -0.3917322834645671215, -1.731627296587926468 ) ) ;
#58145 = CARTESIAN_POINT ( 'NONE',  ( -1.200787401574802349, 0.1660481256975883668, -0.3530559997133364547 ) ) ;
#58146 = CARTESIAN_POINT ( 'NONE',  ( -0.01968503937007793844, 0.1660481256975883668, -0.3530559997133364547 ) ) ;
#58147 = CARTESIAN_POINT ( 'NONE',  ( -0.2427821522309703550, -0.2845877964562159024, 0.3641732283464567677 ) ) ;
#58148 = CARTESIAN_POINT ( 'NONE',  ( 1.620734908136483465, -0.6692913385826771977, 0.1292274648535927661 ) ) ;
#58149 = CARTESIAN_POINT ( 'NONE',  ( 1.463254593175853824, -0.6692913385826771977, 0.1292274648535927661 ) ) ;
#58150 = CARTESIAN_POINT ( 'NONE',  ( -0.5971128608923877978, 0.2952755905511811885, 0.1292274648535926551 ) ) ;
#58151 = CARTESIAN_POINT ( 'NONE',  ( 0.2489931967792015644, 0.004960608223780119466, 0.3437734562760182411 ) ) ;
#58152 = CARTESIAN_POINT ( 'NONE',  ( 1.122047244094488860, 0.1660481256975885056, 0.3530559997133364547 ) ) ;
#58153 = CARTESIAN_POINT ( 'NONE',  ( -0.5314960629921325896, 2.755905511811024056, 1.895394334970790018 ) ) ;
#58154 = VERTEX_POINT ( 'NONE', #64669 ) ;
#58155 = EDGE_CURVE ( 'NONE', #12714, #82375, #26361, .T. ) ;
#58156 = ORIENTED_EDGE ( 'NONE', *, *, #36314, .T. ) ;
#58157 = CARTESIAN_POINT ( 'NONE',  ( 0.1377952755905518800, 0.1660481256975883668, -0.3530559997133364547 ) ) ;
#58158 = CARTESIAN_POINT ( 'NONE',  ( -0.4527559055118102749, 0.07958543189024085140, 0.2665933059059887866 ) ) ;
#58160 = CARTESIAN_POINT ( 'NONE',  ( 0.3458507752293908943, -0.3458507752293908943, -0.4133858267716534196 ) ) ;
#58159 = CARTESIAN_POINT ( 'NONE',  ( 1.476377952755906442, -0.4536011799217367080, 0.2665933059059888421 ) ) ;
#58161 = CARTESIAN_POINT ( 'NONE',  ( -0.2362204724409451284, 0.4091458600556402425, -0.4048556430446194621 ) ) ;
#58162 = CARTESIAN_POINT ( 'NONE',  ( 1.594488188976378673, -0.4536011799217368745, -0.2665933059059886201 ) ) ;
#58163 = CARTESIAN_POINT ( 'NONE',  ( 1.607611548556431069, 0.2952755905511811885, 0.1292274648535926551 ) ) ;
#58164 = CARTESIAN_POINT ( 'NONE',  ( -0.1058382717557503072, 0.3949938075777408852, 0.2316272965879264401 ) ) ;
#58165 = CARTESIAN_POINT ( 'NONE',  ( -0.02624671916010428221, -0.6046776061558807314, 0.2411417322834647770 ) ) ;
#58166 = CARTESIAN_POINT ( 'NONE',  ( 0.000000000000000000, 2.559055118110236560, 0.000000000000000000 ) ) ;
#58167 = CARTESIAN_POINT ( 'NONE',  ( -1.410761154855642463, -0.05778040916215522460, 0.4822834645669289988 ) ) ;
#58168 = CARTESIAN_POINT ( 'NONE',  ( 0.2230971128608929543, 0.05413385826771626580, -0.4176697321401330321 ) ) ;
#58169 = CARTESIAN_POINT ( 'NONE',  ( 0.3420746716998660508, -0.1974969037888704149, 0.1332020997375328031 ) ) ;
#58170 = CARTESIAN_POINT ( 'NONE',  ( 1.679790026246720025, 0.2306618581243848609, 0.2411417322834645549 ) ) ;
#58171 = CARTESIAN_POINT ( 'NONE',  ( 1.056430446194226436, -0.6692913385826773087, -0.1292274648535924053 ) ) ;
#58172 = CARTESIAN_POINT ( 'NONE',  ( 1.003937007874016407, -0.4536011799217367080, 0.2665933059059888421 ) ) ;
#58173 = CARTESIAN_POINT ( 'NONE',  ( 0.8464566929133864326, 0.1012011053420775880, -0.2882089793578257453 ) ) ;
#58174 = CARTESIAN_POINT ( 'NONE',  ( 0.9251968503937015864, 0.07958543189024071263, -0.2665933059059888421 ) ) ;
#58175 = CARTESIAN_POINT ( 'NONE',  ( -1.279527559055116948, 0.1660481256975883668, -0.3530559997133364547 ) ) ;
#58176 = CARTESIAN_POINT ( 'NONE',  ( -0.3460692066303957537, -0.1998031496062994405, -0.7591863517060367661 ) ) ;
#58177 = CARTESIAN_POINT ( 'NONE',  ( 1.377952755905512472, 0.2952755905511811885, 0.000000000000000000 ) ) ;
#58178 = CARTESIAN_POINT ( 'NONE',  ( -0.1049643490035307020, 0.3917322834645669549, -0.7860892388451442558 ) ) ;
#58180 = DIRECTION ( 'NONE',  ( 0.000000000000000000, 0.000000000000000000, -1.000000000000000000 ) ) ;
#58179 = CARTESIAN_POINT ( 'NONE',  ( 0.8464566929133866546, -0.5400638737290844871, 0.3530559997133364547 ) ) ;
#58181 = CYLINDRICAL_SURFACE ( 'NONE', #52318, 0.2952755905511810774 ) ;
#58182 = CARTESIAN_POINT ( 'NONE',  ( 0.3543307086614179147, 0.1771653543307087630, 0.000000000000000000 ) ) ;
#58183 = CARTESIAN_POINT ( 'NONE',  ( 0.7086614173228353852, -0.1870078740157479769, 0.4822834645669291653 ) ) ;
#58184 = CARTESIAN_POINT ( 'NONE',  ( -0.2726377952755906220, 0.1133856558944467546, 0.1574803149606299191 ) ) ;
#58185 = CARTESIAN_POINT ( 'NONE',  ( -1.062992125984250968, 0.1771653543307087630, 0.000000000000000000 ) ) ;
#58186 = CARTESIAN_POINT ( 'NONE',  ( -1.213910761154854745, 0.2952755905511810774, -0.1292274648535930714 ) ) ;
#58187 = AXIS2_PLACEMENT_3D ( 'NONE', #39791, #41042, #34736 ) ;
#58188 = CARTESIAN_POINT ( 'NONE',  ( 1.509186351706037543, 0.05413385826771666132, 0.4176697321401328100 ) ) ;
#58189 = EDGE_CURVE ( 'NONE', #54098, #81558, #32028, .T. ) ;
#58190 = CARTESIAN_POINT ( 'NONE',  ( -1.036745406824146176, 0.05413385826771626580, -0.4176697321401330321 ) ) ;
#58191 = CARTESIAN_POINT ( 'NONE',  ( 0.7611548556430454138, 0.2306618581243847221, -0.2411417322834647770 ) ) ;
#58192 = CARTESIAN_POINT ( 'NONE',  ( -1.332020997375327642, -0.08942795157527998196, 0.3641732283464567121 ) ) ;
#58193 = CARTESIAN_POINT ( 'NONE',  ( 1.968503937007874072, 2.169649841009086334E-17, 5.524802951929911998 ) ) ;
#58194 = CARTESIAN_POINT ( 'NONE',  ( 1.062992125984252745, -0.6692913385826771977, 8.415575281601705876E-17 ) ) ;
#58195 = CARTESIAN_POINT ( 'NONE',  ( -0.3458507752293906723, -0.3458507752293910609, -2.655511811023622215 ) ) ;
#58196 = DIRECTION ( 'NONE',  ( 0.000000000000000000, -0.000000000000000000, 1.000000000000000000 ) ) ;
#58197 = CARTESIAN_POINT ( 'NONE',  ( 1.213910761154856299, 0.2952755905511811885, 0.1292274648535926551 ) ) ;
#58198 = CARTESIAN_POINT ( 'NONE',  ( -0.9973753280839886548, -0.5023911411419708095, -0.1820866141732282451 ) ) ;
#58199 = CARTESIAN_POINT ( 'NONE',  ( 1.679790026246720025, 0.1283753931104748280, 0.1820866141732283561 ) ) ;
#58200 = CARTESIAN_POINT ( 'NONE',  ( -1.233595800524933894, -0.5023911411419708095, -0.1820866141732282451 ) ) ;
#58201 = CARTESIAN_POINT ( 'NONE',  ( -0.5052493438320203589, 0.1771653543307087075, -0.09757992244046823083 ) ) ;
#58202 = CARTESIAN_POINT ( 'NONE',  ( -1.699475065616797398, 0.1771653543307087630, 0.09757992244046791164 ) ) ;
#58203 = CARTESIAN_POINT ( 'NONE',  ( 0.7677165354330716118, -0.4536011799217367080, 0.2665933059059888421 ) ) ;
#58204 = VECTOR ( 'NONE', #59779, 39.37007874015748143 ) ;
#58205 = CARTESIAN_POINT ( 'NONE',  ( 0.3346456692913393205, -0.5400638737290845981, -0.3530559997133363437 ) ) ;
#58206 = CARTESIAN_POINT ( 'NONE',  ( 1.345144356955381593, -0.3162353388693409650, -0.4822834645669289433 ) ) ;
#58207 = CARTESIAN_POINT ( 'NONE',  ( -0.1509186351706028884, -0.3162353388693409650, -0.4822834645669289433 ) ) ;
#58208 = CARTESIAN_POINT ( 'NONE',  ( 0.7349081364829402885, -0.5023911411419708095, -0.1820866141732282451 ) ) ;
#58209 = CARTESIAN_POINT ( 'NONE',  ( -1.646981627296586703, -0.05778040916215522460, 0.4822834645669289988 ) ) ;
#58210 = EDGE_CURVE ( 'NONE', #66560, #29487, #59776, .T. ) ;
#58211 = CARTESIAN_POINT ( 'NONE',  ( -1.443569553805773564, 0.2306618581243847221, -0.2411417322834647770 ) ) ;
#58212 = CARTESIAN_POINT ( 'NONE',  ( -0.7020997375328076329, -0.3162353388693409650, -0.4822834645669289433 ) ) ;
#58213 = CARTESIAN_POINT ( 'NONE',  ( -0.3996062992125985480, -0.1070741851644057135, -0.2034120734908136663 ) ) ;
#58214 = CARTESIAN_POINT ( 'NONE',  ( 0.4724409448818898682, 2.892866454678787531E-17, -1.139763779527559029 ) ) ;
#58215 = CARTESIAN_POINT ( 'NONE',  ( 0.2099737532808405305, 0.2306618581243847221, -0.2411417322834647770 ) ) ;
#58216 = CARTESIAN_POINT ( 'NONE',  ( -0.2493438320209966919, -0.4281496062992124485, 0.4176697321401328655 ) ) ;
#58217 = CARTESIAN_POINT ( 'NONE',  ( 0.2559055118110243332, -0.5400638737290845981, -0.3530559997133363437 ) ) ;
#58218 = CARTESIAN_POINT ( 'NONE',  ( 4.893765752498283924E-17, -0.3996062992125986035, -2.598425196850393970 ) ) ;
#58219 = CARTESIAN_POINT ( 'NONE',  ( -0.3949938075777411628, 0.1058382717557497937, -2.080052493438320216 ) ) ;
#58220 = CARTESIAN_POINT ( 'NONE',  ( 0.1958661417322834775, 0.3392501089628018884, -0.6089238845144356871 ) ) ;
#58221 = DIRECTION ( 'NONE',  ( -0.000000000000000000, -1.000000000000000000, -0.000000000000000000 ) ) ;
#58222 = CARTESIAN_POINT ( 'NONE',  ( -0.3917322834645670104, -7.196005306013484475E-17, -0.8188976377952754682 ) ) ;
#58223 = CARTESIAN_POINT ( 'NONE',  ( -0.7414698162729651543, 0.1771653543307087075, -0.09757992244046823083 ) ) ;
#58224 = CARTESIAN_POINT ( 'NONE',  ( 0.3917322834645670104, 2.398668435337828261E-17, -1.055118110236220375 ) ) ;
#58225 = CARTESIAN_POINT ( 'NONE',  ( -1.089238845144356427, 0.05413385826771666132, 0.4176697321401328100 ) ) ;
#58226 = CARTESIAN_POINT ( 'NONE',  ( 0.3420746716998660508, -0.1974969037888704149, -2.858923884514436242 ) ) ;
#58227 = CARTESIAN_POINT ( 'NONE',  ( 0.5839895013123367340, 0.2952755905511811885, 0.1292274648535926551 ) ) ;
#58228 = CARTESIAN_POINT ( 'NONE',  ( 0.08530183727034192087, -0.2845877964562161244, -0.3641732283464567121 ) ) ;
#58229 = CARTESIAN_POINT ( 'NONE',  ( 1.194225721784777594, -0.4281496062992127816, -0.4176697321401328100 ) ) ;
#58230 = CARTESIAN_POINT ( 'NONE',  ( 0.3871391076115492380, -0.05778040916215560624, -0.4822834645669293319 ) ) ;
#58231 = CARTESIAN_POINT ( 'NONE',  ( 0.4724409448818897572, -0.1265901696524988906, -2.788713910761154047 ) ) ;
#58232 = CARTESIAN_POINT ( 'NONE',  ( -0.2925321140481932924, 0.2925321140481931814, -2.539370078740157410 ) ) ;
#58233 = CARTESIAN_POINT ( 'NONE',  ( -0.3917322834645670659, -7.196005306013484475E-17, -1.295951074312022833 ) ) ;
#58234 = CARTESIAN_POINT ( 'NONE',  ( 1.207349081364829990, 0.2306618581243848609, 0.2411417322834645549 ) ) ;
#58235 = CARTESIAN_POINT ( 'NONE',  ( 0.6299212598425204535, -0.1870078740157479769, 0.4822834645669291653 ) ) ;
#58236 = CARTESIAN_POINT ( 'NONE',  ( 0.05249343832021075018, 0.2306618581243847221, -0.2411417322834647770 ) ) ;
#58237 = CARTESIAN_POINT ( 'NONE',  ( 0.9120734908136489683, -0.5511811023622046335, 0.09757992244046803654 ) ) ;
#58238 = B_SPLINE_CURVE_WITH_KNOTS ( 'NONE', 3,
 ( #18292, #43937, #6058, #82674, #32145, #17478, #11151, #49439 ),
 .UNSPECIFIED., .F., .F.,
 ( 4, 2, 2, 4 ),
 ( 0.000000000000000000, 0.002428646466414857708, 0.003642969699622285694, 0.004857292932829714548 ),
 .UNSPECIFIED. ) ;
#58239 = CARTESIAN_POINT ( 'NONE',  ( 1.358267716535433323, 0.1660481256975885056, 0.3530559997133364547 ) ) ;
#58240 = CARTESIAN_POINT ( 'NONE',  ( -0.2867679344610365999, 0.2867679344610364889, -0.1043307086614174151 ) ) ;
#58241 = CARTESIAN_POINT ( 'NONE',  ( 0.2362204724409456558, -0.1870078740157480879, -0.4822834645669291653 ) ) ;
#58242 = CARTESIAN_POINT ( 'NONE',  ( 1.240157480314961314, 0.1660481256975883668, -0.3530559997133364547 ) ) ;
#58243 = CARTESIAN_POINT ( 'NONE',  ( 0.5577427821522316087, -0.05778040916215522460, 0.4822834645669289988 ) ) ;
#58244 = AXIS2_PLACEMENT_3D ( 'NONE', #39480, #33172, #78215 ) ;
#58245 = CARTESIAN_POINT ( 'NONE',  ( 1.207349081364829990, 0.1283753931104748280, 0.1820866141732283561 ) ) ;
#58246 = CARTESIAN_POINT ( 'NONE',  ( -1.010498687664041384, -0.4281496062992127816, -0.4176697321401328100 ) ) ;
#58247 = CARTESIAN_POINT ( 'NONE',  ( -0.8661417322834640276, -0.1870078740157480879, -0.4822834645669291653 ) ) ;
#58248 = CARTESIAN_POINT ( 'NONE',  ( 1.069553805774278610, -0.6692913385826771977, 0.1292274648535927661 ) ) ;
#58249 = CARTESIAN_POINT ( 'NONE',  ( -0.1308238996047441649, -0.3698506310986687806, -1.929133858267718660 ) ) ;
#58250 = CARTESIAN_POINT ( 'NONE',  ( -0.1049643490035302024, -0.3917322834645671215, -1.954068241469816503 ) ) ;
#58251 = CARTESIAN_POINT ( 'NONE',  ( -0.3392501089628017219, -0.1958661417322836718, -2.879265091863516979 ) ) ;
#58252 = EDGE_LOOP ( 'NONE', ( #38512, #37526, #13546, #41406, #68943 ) ) ;
#58253 = CARTESIAN_POINT ( 'NONE',  ( 0.3460692066303959757, -0.1998031496062991907, -0.1049868766404199599 ) ) ;
#58254 = ORIENTED_EDGE ( 'NONE', *, *, #40513, .T. ) ;
#58255 = CARTESIAN_POINT ( 'NONE',  ( 1.469816272965879911, -0.6046776061558807314, 0.2411417322834647770 ) ) ;
#58256 = CARTESIAN_POINT ( 'NONE',  ( 0.8464566929133865436, 0.07958543189024071263, -0.2665933059059888421 ) ) ;
#58257 = CARTESIAN_POINT ( 'NONE',  ( -0.7749820319012115100, 0.000000000000000000, 0.3464511005275205946 ) ) ;
#58258 = CARTESIAN_POINT ( 'NONE',  ( 3.821484228344193657, 2.755905511811024056, 0.5314960629921260393 ) ) ;
#58259 = CARTESIAN_POINT ( 'NONE',  ( 0.3959418824714268648, 0.02190130575838933683, -1.929133858267716661 ) ) ;
#58260 = CARTESIAN_POINT ( 'NONE',  ( 0.2867679344610365999, -0.2867679344610365444, -0.6555118110236222151 ) ) ;
#58261 = CIRCLE ( 'NONE', #12558, 3.307086614173228689 ) ;
#58262 = CARTESIAN_POINT ( 'NONE',  ( -1.246719160104985846, -0.3690944881889765550, -0.3153832671262227771 ) ) ;
#58263 = CARTESIAN_POINT ( 'NONE',  ( -1.450131233595799651, -0.5511811023622046335, 0.09757992244046803654 ) ) ;
#58264 = CARTESIAN_POINT ( 'NONE',  ( -1.299212598425196097, 0.2952755905511811885, 0.000000000000000000 ) ) ;
#58265 = CARTESIAN_POINT ( 'NONE',  ( -0.1181102362204717315, 0.2952755905511811885, 0.000000000000000000 ) ) ;
#58266 = CARTESIAN_POINT ( 'NONE',  ( 1.443569553805774897, 0.2306618581243848609, 0.2411417322834645549 ) ) ;
#58267 = ORIENTED_EDGE ( 'NONE', *, *, #72340, .T. ) ;
#58268 = CARTESIAN_POINT ( 'NONE',  ( 0.3495983942378627085, 0.3045330818767438275, -0.01888973282054023581 ) ) ;
#58269 = CARTESIAN_POINT ( 'NONE',  ( 7.456690011882651348, 3.916330350904249968, 5.973313079581529017 ) ) ;
#58270 = FACE_OUTER_BOUND ( 'NONE', #26466, .T. ) ;
#58271 = CARTESIAN_POINT ( 'NONE',  ( -1.614173228346457378, 1.881821177735609085, -0.1372047244094477536 ) ) ;
#58272 = CARTESIAN_POINT ( 'NONE',  ( -1.056430446194224881, -0.5511811023622046335, 0.09757992244046803654 ) ) ;
#58273 = CARTESIAN_POINT ( 'NONE',  ( -1.404199475065615932, -0.4281496062992127816, -0.4176697321401328100 ) ) ;
#58274 = CARTESIAN_POINT ( 'NONE',  ( 0.5314960629921267055, -0.5400638737290844871, 0.3530559997133364547 ) ) ;
#58275 = ORIENTED_EDGE ( 'NONE', *, *, #58647, .T. ) ;
#58277 = DIRECTION ( 'NONE',  ( 0.000000000000000000, -1.000000000000000000, 0.000000000000000000 ) ) ;
#58276 = CARTESIAN_POINT ( 'NONE',  ( -0.03443470937339728616, 1.062992125984252079, -1.537015892239756099 ) ) ;
#58278 = CARTESIAN_POINT ( 'NONE',  ( 1.246719160104987623, 0.05413385826771626580, -0.4176697321401330321 ) ) ;
#58279 = CARTESIAN_POINT ( 'NONE',  ( -1.587926509186350810, -0.4281496062992124485, 0.4176697321401328655 ) ) ;
#58280 = CARTESIAN_POINT ( 'NONE',  ( -0.3392501089628018329, -0.1958661417322836440, -0.6049675608585809439 ) ) ;
#58281 = CARTESIAN_POINT ( 'NONE',  ( -0.2559055118110230564, 0.07958543189024071263, -0.2665933059059888421 ) ) ;
#58282 = CARTESIAN_POINT ( 'NONE',  ( -1.443569553805773564, 0.1283753931104746893, -0.1820866141732285504 ) ) ;
#58283 = CARTESIAN_POINT ( 'NONE',  ( 0.5611900217179910388, 1.223219560026271499E-15, 0.4445507791589056734 ) ) ;
#58284 = CARTESIAN_POINT ( 'NONE',  ( -0.5446194225721777693, -0.08942795157527998196, 0.3641732283464567121 ) ) ;
#58285 = CARTESIAN_POINT ( 'NONE',  ( 0.2099737532808405305, 0.1283753931104746893, -0.1820866141732285504 ) ) ;
#58286 = ADVANCED_FACE ( 'NONE', ( #26780 ), #34311, .F. ) ;
#58287 = CARTESIAN_POINT ( 'NONE',  ( 0.3083989501312343062, -0.3162353388693405765, 0.4822834645669290543 ) ) ;
#58288 = CARTESIAN_POINT ( 'NONE',  ( -1.154855643044618851, 0.1283753931104748280, 0.1820866141732283561 ) ) ;
#58289 = CARTESIAN_POINT ( 'NONE',  ( 0.3917322834645670104, 2.398668435337828261E-17, -2.629921259842519898 ) ) ;
#58290 = CARTESIAN_POINT ( 'NONE',  ( 0.6955380577427828781, 0.05413385826771626580, -0.4176697321401330321 ) ) ;
#58291 = ADVANCED_FACE ( 'NONE', ( #14176 ), #11483, .T. ) ;
#58292 = CARTESIAN_POINT ( 'NONE',  ( -1.522309711286088607, -0.6046776061558807314, 0.2411417322834647770 ) ) ;
#58293 = CARTESIAN_POINT ( 'NONE',  ( -0.4091458600556405756, 0.2362204724409446288, -1.205380577427821454 ) ) ;
#58294 = CARTESIAN_POINT ( 'NONE',  ( -0.3674540682414692561, -0.6046776061558809534, -0.2411417322834644161 ) ) ;
#58295 = CARTESIAN_POINT ( 'NONE',  ( 0.1706036745406830368, -0.004921259842519576551, 0.3153832671262227771 ) ) ;
#58296 = CARTESIAN_POINT ( 'NONE',  ( -0.8858267716535425107, -0.5400638737290844871, 0.3530559997133364547 ) ) ;
#58297 = CARTESIAN_POINT ( 'NONE',  ( 0.8005249343832028242, -0.3690944881889765550, -0.3153832671262227771 ) ) ;
#58298 = CARTESIAN_POINT ( 'NONE',  ( -0.1246719160104980823, 0.1771653543307087630, 0.09757992244046791164 ) ) ;
#58299 = CARTESIAN_POINT ( 'NONE',  ( -0.6430446194225716283, -0.4281496062992124485, 0.4176697321401328655 ) ) ;
#58300 = CARTESIAN_POINT ( 'NONE',  ( -1.489501312335957062, -0.05778040916215522460, 0.4822834645669289988 ) ) ;
#58301 = CARTESIAN_POINT ( 'NONE',  ( -0.7535225988626923499, 2.401574803149606474, 0.4915354330708645025 ) ) ;
#58302 = CARTESIAN_POINT ( 'NONE',  ( 1.292650918635171564, -0.5511811023622048555, -0.09757992244046775898 ) ) ;
#58303 = AXIS2_PLACEMENT_3D ( 'NONE', #11600, #24619, #75984 ) ;
#58304 = CARTESIAN_POINT ( 'NONE',  ( -1.587926509186350810, 0.05413385826771626580, -0.4176697321401330321 ) ) ;
#58305 = CARTESIAN_POINT ( 'NONE',  ( -1.397637795275589623, 0.1660481256975885056, 0.3530559997133364547 ) ) ;
#58306 = ORIENTED_EDGE ( 'NONE', *, *, #33733, .F. ) ;
#58307 = CARTESIAN_POINT ( 'NONE',  ( 0.3460692066303958092, 0.1998031496062993018, -2.570209973753280863 ) ) ;
#58308 = EDGE_CURVE ( 'NONE', #74503, #57928, #40248, .T. ) ;
#58309 = CARTESIAN_POINT ( 'NONE',  ( -0.8530183727034112984, -0.004921259842519576551, 0.3153832671262227771 ) ) ;
#58310 = CARTESIAN_POINT ( 'NONE',  ( 0.6299212598425204535, -0.1870078740157479769, 0.4822834645669291653 ) ) ;
#58311 = CARTESIAN_POINT ( 'NONE',  ( -1.108923884514435132, -0.2845877964562159024, 0.3641732283464567677 ) ) ;
#58312 = CARTESIAN_POINT ( 'NONE',  ( 0.3996062992125985480, 2.446882876249141654E-17, -1.927165354330708791 ) ) ;
#58313 = CARTESIAN_POINT ( 'NONE',  ( -1.174540682414697335, -0.3162353388693409650, -0.4822834645669289433 ) ) ;
#58314 = CARTESIAN_POINT ( 'NONE',  ( 1.062992125984252745, 0.2952755905511811885, 0.000000000000000000 ) ) ;
#58315 = CARTESIAN_POINT ( 'NONE',  ( 0.5839895013123367340, 0.2952755905511811885, 0.1292274648535926551 ) ) ;
#58316 = EDGE_CURVE ( 'NONE', #25219, #41276, #55801, .T. ) ;
#58317 = CARTESIAN_POINT ( 'NONE',  ( 0.4724409448818898682, 2.892866454678787531E-17, -0.1181102362204724532 ) ) ;
#58318 = CARTESIAN_POINT ( 'NONE',  ( -1.312335958005248715, -0.5023911411419708095, -0.1820866141732282451 ) ) ;
#58319 = CARTESIAN_POINT ( 'NONE',  ( 0.1998031496062992463, 0.3460692066303959202, -1.166010498687663821 ) ) ;
#58320 = CARTESIAN_POINT ( 'NONE',  ( 0.1070741851644054915, -0.3996062992125986035, -0.8727034120734907807 ) ) ;
#58321 = AXIS2_PLACEMENT_3D ( 'NONE', #10216, #29556, #67050 ) ;
#58322 = CARTESIAN_POINT ( 'NONE',  ( 0.3420746716998660508, -0.1974969037888703871, -0.5774278215223097588 ) ) ;
#58323 = CARTESIAN_POINT ( 'NONE',  ( 0.4889872687189469325, 1.535433070866141225, -0.4915354330708656683 ) ) ;
#58324 = CARTESIAN_POINT ( 'NONE',  ( 0.8923884514435703741, 0.1283753931104748280, 0.1820866141732283561 ) ) ;
#58325 = CARTESIAN_POINT ( 'NONE',  ( 0.2821522309711292364, -0.5511811023622046335, 0.09757992244046803654 ) ) ;
#58326 = CARTESIAN_POINT ( 'NONE',  ( -0.006561679790025524116, -0.3162353388693405765, 0.4822834645669290543 ) ) ;
#58327 = CARTESIAN_POINT ( 'NONE',  ( 1.489501312335958172, -0.05778040916215560624, -0.4822834645669293319 ) ) ;
#58328 = CARTESIAN_POINT ( 'NONE',  ( 0.2891555358219910499, 0.2891555358219910499, -1.789370078740157632 ) ) ;
#58329 = CARTESIAN_POINT ( 'NONE',  ( 0.2755905511811031494, 0.1771653543307087630, 0.000000000000000000 ) ) ;
#58330 = CARTESIAN_POINT ( 'NONE',  ( -0.8661417322834640276, -0.1870078740157479769, 0.4822834645669291653 ) ) ;
#58331 = CARTESIAN_POINT ( 'NONE',  ( -1.128608923884513837, 0.2306618581243847221, -0.2411417322834647770 ) ) ;
#58332 = CARTESIAN_POINT ( 'NONE',  ( 0.7611548556430454138, 0.2306618581243847221, -0.2411417322834647770 ) ) ;
#58333 = CARTESIAN_POINT ( 'NONE',  ( -0.2362204724409451284, 0.4091458600556402425, -1.745406824146981561 ) ) ;
#58334 = CARTESIAN_POINT ( 'NONE',  ( -0.7611548556430438595, 0.2306618581243848609, 0.2411417322834645549 ) ) ;
#58335 = VERTEX_POINT ( 'NONE', #2374 ) ;
#58336 = EDGE_LOOP ( 'NONE', ( #53072, #5349, #21402, #13957 ) ) ;
#58337 = CARTESIAN_POINT ( 'NONE',  ( -1.351706036745406347, 0.05413385826771626580, -0.4176697321401330321 ) ) ;
#58338 = CARTESIAN_POINT ( 'NONE',  ( -0.6496062992125976043, 0.1660481256975883668, -0.3530559997133364547 ) ) ;
#58340 = CARTESIAN_POINT ( 'NONE',  ( -0.6102362204724400829, -0.5400638737290845981, -0.3530559997133363437 ) ) ;
#58339 = CARTESIAN_POINT ( 'NONE',  ( -0.7283464566929126471, -0.4536011799217367080, 0.2665933059059888421 ) ) ;
#58341 = CARTESIAN_POINT ( 'NONE',  ( -0.2867679344610364334, -0.2867679344610368219, -2.028852075294276691 ) ) ;
#58343 = ADVANCED_FACE ( 'NONE', ( #41899 ), #37002, .F. ) ;
#58342 = CARTESIAN_POINT ( 'NONE',  ( 4.893765752498283308E-17, -0.3996062992125985480, -2.832677165354331006 ) ) ;
#58344 = CARTESIAN_POINT ( 'NONE',  ( 1.666666666666667185, 0.05413385826771666132, 0.4176697321401328100 ) ) ;
#58345 = CARTESIAN_POINT ( 'NONE',  ( -1.056430446194224881, 0.2952755905511810774, -0.1292274648535930714 ) ) ;
#58346 = CARTESIAN_POINT ( 'NONE',  ( 0.1771653543307093182, 0.1660481256975885056, 0.3530559997133364547 ) ) ;
#58347 = CARTESIAN_POINT ( 'NONE',  ( -0.8202099737532799750, 0.2952755905511810774, -0.1292274648535930714 ) ) ;
#58348 = CARTESIAN_POINT ( 'NONE',  ( 0.8136482939632553313, 0.2306618581243848609, 0.2411417322834645549 ) ) ;
#58349 = CARTESIAN_POINT ( 'NONE',  ( -0.2867679344610364334, -0.2867679344610367109, -1.468503937007874294 ) ) ;
#58350 = CARTESIAN_POINT ( 'NONE',  ( -0.6299212598425188991, -0.1870078740157480601, -0.3641732283464567677 ) ) ;
#58351 = ORIENTED_EDGE ( 'NONE', *, *, #8767, .T. ) ;
#58352 = CARTESIAN_POINT ( 'NONE',  ( 0.3949938075777411073, -0.1058382717557499464, -1.686351706036745668 ) ) ;
#58353 = ORIENTED_EDGE ( 'NONE', *, *, #61206, .T. ) ;
#58354 = CARTESIAN_POINT ( 'NONE',  ( -1.220472440944881054, 0.8346805926620878280, 0.5309055118110237448 ) ) ;
#58355 = CARTESIAN_POINT ( 'NONE',  ( -1.069553805774277722, 0.2952755905511811885, 0.1292274648535926551 ) ) ;
#58356 = CARTESIAN_POINT ( 'NONE',  ( -1.371391076115484609, -0.6692913385826771977, 0.1292274648535927661 ) ) ;
#58357 = CARTESIAN_POINT ( 'NONE',  ( -0.3996062992125987146, 0.1070741851644051862, -0.1902887139107611314 ) ) ;
#58358 = CARTESIAN_POINT ( 'NONE',  ( -1.279527559055116948, -0.5400638737290844871, 0.3530559997133364547 ) ) ;
#58359 = CARTESIAN_POINT ( 'NONE',  ( -1.220472440944881054, 0.2952755905511811885, 0.000000000000000000 ) ) ;
#58360 = CARTESIAN_POINT ( 'NONE',  ( -1.240157480314959759, -0.5400638737290845981, -0.3530559997133363437 ) ) ;
#58361 = PRESENTATION_STYLE_ASSIGNMENT (( #53297 ) ) ;
#58362 = CARTESIAN_POINT ( 'NONE',  ( 0.000000000000000000, 2.185078740157480937, 0.4527559055118110520 ) ) ;
#58363 = CARTESIAN_POINT ( 'NONE',  ( -0.01968503937007793844, 0.07958543189024071263, -0.2665933059059888421 ) ) ;
#58364 = DIRECTION ( 'NONE',  ( 0.000000000000000000, 0.000000000000000000, 1.000000000000000000 ) ) ;
#58365 = CARTESIAN_POINT ( 'NONE',  ( 4.797336870675656522E-17, -0.3917322834645670104, -0.1633858267716536417 ) ) ;
#58366 = CARTESIAN_POINT ( 'NONE',  ( -0.4068241469816267775, -0.004921259842519870586, -0.3153832671262229437 ) ) ;
#58367 = VECTOR ( 'NONE', #12855, 39.37007874015748143 ) ;
#58368 = CARTESIAN_POINT ( 'NONE',  ( -0.8267716535433065062, 0.2952755905511811885, 0.000000000000000000 ) ) ;
#58369 = CARTESIAN_POINT ( 'NONE',  ( 1.233595800524935227, -0.6046776061558807314, 0.2411417322834647770 ) ) ;
#58370 = CARTESIAN_POINT ( 'NONE',  ( -0.7020997375328074108, -0.05778040916215522460, 0.4822834645669289988 ) ) ;
#58371 = VERTEX_POINT ( 'NONE', #9103 ) ;
#58372 = ORIENTED_EDGE ( 'NONE', *, *, #80532, .T. ) ;
#58373 = CARTESIAN_POINT ( 'NONE',  ( 0.1070741851644054776, -0.3996062992125984925, -2.209317585301837195 ) ) ;
#58374 = CARTESIAN_POINT ( 'NONE',  ( -0.8530183727034112984, 0.05413385826771666132, 0.4176697321401328100 ) ) ;
#58375 = CARTESIAN_POINT ( 'NONE',  ( 1.318897637795276356, 0.1660481256975883668, -0.3530559997133364547 ) ) ;
#58376 = CARTESIAN_POINT ( 'NONE',  ( -1.587926509186350810, -0.3690944881889763329, 0.3153832671262228327 ) ) ;
#58377 = CARTESIAN_POINT ( 'NONE',  ( -1.305774278215222184, -0.6692913385826773087, -0.1292274648535924053 ) ) ;
#58378 = CARTESIAN_POINT ( 'NONE',  ( -0.4724409448818895907, -0.1265901696524993070, -0.8333333333333332593 ) ) ;
#58379 = EDGE_CURVE ( 'NONE', #34463, #4617, #19513, .T. ) ;
#58380 = CARTESIAN_POINT ( 'NONE',  ( 0.000000000000000000, 0.000000000000000000, 0.000000000000000000 ) ) ;
#58381 = CARTESIAN_POINT ( 'NONE',  ( 0.3392501089628018884, -0.1958661417322834220, -0.2545931758530183275 ) ) ;
#58382 = CARTESIAN_POINT ( 'NONE',  ( -0.1958661417322836718, 0.3392501089628017219, -1.987532808398950079 ) ) ;
#58383 = CARTESIAN_POINT ( 'NONE',  ( -0.3674540682414689785, 0.2306618581243848609, 0.2411417322834645549 ) ) ;
#58384 = CARTESIAN_POINT ( 'NONE',  ( -1.476377952755905110, 0.07958543189024085140, 0.2665933059059887866 ) ) ;
#58385 = CARTESIAN_POINT ( 'NONE',  ( -0.8727034120734901146, -0.05778040916215560624, -0.4822834645669293319 ) ) ;
#58386 = CARTESIAN_POINT ( 'NONE',  ( 0.1265901696524990294, -0.4724409448818896462, -2.839238845144356649 ) ) ;
#58388 = CARTESIAN_POINT ( 'NONE',  ( -0.1968503937007867743, 0.2952755905511811885, 0.000000000000000000 ) ) ;
#58387 = CARTESIAN_POINT ( 'NONE',  ( -1.102362204724408601, -0.1870078740157479769, 0.4822834645669291653 ) ) ;
#58389 = CARTESIAN_POINT ( 'NONE',  ( -1.010498687664041384, -0.4281496062992127816, -0.4176697321401328100 ) ) ;
#58390 = CARTESIAN_POINT ( 'NONE',  ( -0.3805774278215216522, -0.4281496062992127816, -0.4176697321401328100 ) ) ;
#58391 = AXIS2_PLACEMENT_3D ( 'NONE', #82995, #63218, #5150 ) ;
#58392 = CARTESIAN_POINT ( 'NONE',  ( -0.2891555358219911054, 0.2891555358219909388, -2.773622047244094446 ) ) ;
#58393 = CARTESIAN_POINT ( 'NONE',  ( 1.036745406824147508, -0.3690944881889765550, -0.3153832671262227771 ) ) ;
#58394 = CARTESIAN_POINT ( 'NONE',  ( 0.1049643490035304799, -0.3917322834645669549, -0.1699475065616798675 ) ) ;
#58395 = CARTESIAN_POINT ( 'NONE',  ( 0.9580052493438327987, -0.3690944881889765550, -0.3153832671262227771 ) ) ;
#58396 = CARTESIAN_POINT ( 'NONE',  ( 1.279527559055118724, 0.07958543189024085140, 0.2665933059059887866 ) ) ;
#58397 = CARTESIAN_POINT ( 'NONE',  ( 1.397637795275591177, -0.5400638737290844871, 0.3530559997133364547 ) ) ;
#58398 = CARTESIAN_POINT ( 'NONE',  ( 0.2427821522309719648, -0.08942795157527998196, 0.3641732283464567121 ) ) ;
#58399 = CARTESIAN_POINT ( 'NONE',  ( 0.3392501089628018884, -0.1958661417322834220, -1.514435695538058013 ) ) ;
#58400 = CARTESIAN_POINT ( 'NONE',  ( -1.062992125984250968, -0.6692913385826771977, 8.415575281601705876E-17 ) ) ;
#58401 = CARTESIAN_POINT ( 'NONE',  ( 1.141732283464567566, 0.2952755905511811885, 0.000000000000000000 ) ) ;
#58402 = EDGE_CURVE ( 'NONE', #68129, #27226, #22063, .T. ) ;
#58403 = CARTESIAN_POINT ( 'NONE',  ( 5.785732909357575061E-17, -0.4724409448818898682, 0.1594488188976377896 ) ) ;
#58404 = CARTESIAN_POINT ( 'NONE',  ( -0.6496062992125976043, 0.07958543189024071263, -0.2665933059059888421 ) ) ;
#58405 = FACE_OUTER_BOUND ( 'NONE', #20049, .T. ) ;
#58406 = CARTESIAN_POINT ( 'NONE',  ( 0.2952755905511819101, 0.1660481256975883668, -0.3530559997133364547 ) ) ;
#58407 = CARTESIAN_POINT ( 'NONE',  ( 0.3149606299212183158, 2.165354330708661568, 3.937007874015792552 ) ) ;
#58408 = CARTESIAN_POINT ( 'NONE',  ( 0.8136482939632553313, 0.1283753931104748280, 0.1820866141732283561 ) ) ;
#58409 = CARTESIAN_POINT ( 'NONE',  ( 0.3346456692913390985, 0.07958543189024085140, 0.2665933059059887866 ) ) ;
#58410 = CARTESIAN_POINT ( 'NONE',  ( -0.4002624671916004129, -0.3162353388693405765, 0.4822834645669290543 ) ) ;
#58411 = CARTESIAN_POINT ( 'NONE',  ( -1.404199475065615932, 0.05413385826771666132, 0.4176697321401328100 ) ) ;
#58412 = CARTESIAN_POINT ( 'NONE',  ( -0.6496062992125976043, 0.07958543189024071263, -0.2665933059059888421 ) ) ;
#58413 = DIRECTION ( 'NONE',  ( 0.000000000000000000, 0.000000000000000000, 1.000000000000000000 ) ) ;
#58414 = CARTESIAN_POINT ( 'NONE',  ( 0.5511811023622055217, -0.1870078740157479769, 0.4822834645669291653 ) ) ;
#58415 = CARTESIAN_POINT ( 'NONE',  ( -1.030183727034119867, -0.3162353388693405765, 0.4822834645669290543 ) ) ;
#58416 = CARTESIAN_POINT ( 'NONE',  ( 0.2925321140481932369, 0.2925321140481932369, -1.159448818897637734 ) ) ;
#58417 = CARTESIAN_POINT ( 'NONE',  ( 0.3392501089628018884, -0.1958661417322834220, -2.709317585301837195 ) ) ;
#58418 = CARTESIAN_POINT ( 'NONE',  ( 0.3740157480314966754, 0.07958543189024071263, -0.2665933059059888421 ) ) ;
#58419 = CARTESIAN_POINT ( 'NONE',  ( -0.7086614173228339419, -0.1870078740157479769, 0.4822834645669291653 ) ) ;
#58420 = CARTESIAN_POINT ( 'NONE',  ( -1.253280839895012377, -0.3162353388693409650, -0.4822834645669289433 ) ) ;
#58421 = CARTESIAN_POINT ( 'NONE',  ( -1.430446194225720724, -0.004921259842519870586, -0.3153832671262229437 ) ) ;
#58422 = DIRECTION ( 'NONE',  ( 0.000000000000000000, 0.000000000000000000, 1.000000000000000000 ) ) ;
#58423 = CARTESIAN_POINT ( 'NONE',  ( -1.082677165354329896, -0.4536011799217368745, -0.2665933059059886201 ) ) ;
#58424 = CARTESIAN_POINT ( 'NONE',  ( -1.528871391076114250, 0.1771653543307087075, -0.09757992244046823083 ) ) ;
#58425 = CARTESIAN_POINT ( 'NONE',  ( 1.108923884514436242, -0.05778040916215522460, 0.4822834645669289988 ) ) ;
#58426 = CARTESIAN_POINT ( 'NONE',  ( -0.1998031496062994683, 0.3460692066303958092, 0.1443569553805774119 ) ) ;
#58427 = CARTESIAN_POINT ( 'NONE',  ( -0.2867679344610367109, 0.2867679344610365444, -2.378628239666354283 ) ) ;
#58428 = ORIENTED_EDGE ( 'NONE', *, *, #72187, .T. ) ;
#58429 = CARTESIAN_POINT ( 'NONE',  ( 0.5411721830064198935, 8.471767977567108961E-16, -0.4445507791589058955 ) ) ;
#58430 = CARTESIAN_POINT ( 'NONE',  ( -1.686351706036744558, 0.2952755905511810774, -0.1292274648535930714 ) ) ;
#58431 = CARTESIAN_POINT ( 'NONE',  ( -1.213910761154854745, 0.2952755905511810774, -0.1292274648535930714 ) ) ;
#58432 = CARTESIAN_POINT ( 'NONE',  ( 1.377952755905512472, -0.6692913385826771977, 8.415575281601705876E-17 ) ) ;
#58433 = CARTESIAN_POINT ( 'NONE',  ( 0.3917322834645670104, -0.1049643490035303411, -2.085958005249344271 ) ) ;
#58434 = PLANE ( 'NONE',  #37811 ) ;
#58435 = CARTESIAN_POINT ( 'NONE',  ( 0.4921259842519691285, -0.5400638737290845981, -0.3530559997133363437 ) ) ;
#58436 = CARTESIAN_POINT ( 'NONE',  ( 0.006561679790026889343, -0.3162353388693409650, -0.4822834645669289433 ) ) ;
#58437 = CARTESIAN_POINT ( 'NONE',  ( 0.1077553908667773369, 1.075127789244234577, -3.935562805465960601 ) ) ;
#58438 = DIRECTION ( 'NONE',  ( -0.000000000000000000, 1.000000000000000000, -0.000000000000000000 ) ) ;
#58439 = CARTESIAN_POINT ( 'NONE',  ( 0.8005249343832027131, -0.004921259842519576551, 0.3153832671262227771 ) ) ;
#58440 = EDGE_CURVE ( 'NONE', #45259, #65182, #22554, .T. ) ;
#58441 = CARTESIAN_POINT ( 'NONE',  ( 0.1070741851644053527, 0.3996062992125986590, -1.410761154855643129 ) ) ;
#58442 = VERTEX_POINT ( 'NONE', #53278 ) ;
#58444 = CARTESIAN_POINT ( 'NONE',  ( 0.3917322834645670104, 0.1049643490035304660, -0.1214103918973247487 ) ) ;
#58443 = AXIS2_PLACEMENT_3D ( 'NONE', #27949, #42230, #28779 ) ;
#58445 = ORIENTED_EDGE ( 'NONE', *, *, #61841, .F. ) ;
#58446 = CARTESIAN_POINT ( 'NONE',  ( 0.1837270341207354329, 0.2306618581243848609, 0.2411417322834645549 ) ) ;
#58447 = CARTESIAN_POINT ( 'NONE',  ( -1.581364829396324945, -0.05778040916215560624, -0.4822834645669293319 ) ) ;
#58448 = CARTESIAN_POINT ( 'NONE',  ( 0.7808398950131241190, -0.05778040916215560624, -0.4822834645669293319 ) ) ;
#58449 = CARTESIAN_POINT ( 'NONE',  ( 1.095800524934383846, -0.05778040916215560624, -0.4822834645669293319 ) ) ;
#58451 = EDGE_CURVE ( 'NONE', #65535, #5038, #62548, .T. ) ;
#58450 = CARTESIAN_POINT ( 'NONE',  ( 1.417322834645670104, -0.1870078740157479769, 0.4822834645669291653 ) ) ;
#58452 = CARTESIAN_POINT ( 'NONE',  ( -0.4855643044619415427, 0.05413385826771626580, -0.4176697321401330321 ) ) ;
#58453 = CARTESIAN_POINT ( 'NONE',  ( 0.2099737532808405305, 0.2306618581243847221, -0.2411417322834647770 ) ) ;
#58454 = CARTESIAN_POINT ( 'NONE',  ( -1.633858267716534529, 0.1660481256975885056, 0.3530559997133364547 ) ) ;
#58455 = CARTESIAN_POINT ( 'NONE',  ( 1.312335958005249825, 0.2306618581243847221, -0.2411417322834647770 ) ) ;
#58456 = CARTESIAN_POINT ( 'NONE',  ( 1.003937007874016407, -0.5400638737290844871, 0.3530559997133364547 ) ) ;
#58457 = CARTESIAN_POINT ( 'NONE',  ( 0.01312335958005323398, 0.05413385826771666132, 0.4176697321401328100 ) ) ;
#58458 = CARTESIAN_POINT ( 'NONE',  ( -0.2867679344610365999, 0.2867679344610364889, -0.01181102362204719709 ) ) ;
#58459 = CARTESIAN_POINT ( 'NONE',  ( 0.5774278215223104249, 0.1283753931104748280, 0.1820866141732283561 ) ) ;
#58460 = VERTEX_POINT ( 'NONE', #60435 ) ;
#58461 = CARTESIAN_POINT ( 'NONE',  ( 0.3420746716998659953, 0.1974969037888705536, -0.7611548556430446366 ) ) ;
#58462 = ORIENTED_EDGE ( 'NONE', *, *, #49126, .F. ) ;
#58463 = CARTESIAN_POINT ( 'NONE',  ( -0.3740157480314953431, -0.4536011799217368745, -0.2665933059059886201 ) ) ;
#58464 = CARTESIAN_POINT ( 'NONE',  ( 0.07217847769028949700, -0.3162353388693405765, 0.4822834645669290543 ) ) ;
#58465 = CARTESIAN_POINT ( 'NONE',  ( 2.554262525012262586, 1.528804020127598529, -0.4744094488188971281 ) ) ;
#58466 = CARTESIAN_POINT ( 'NONE',  ( 0.006561679790026889343, -0.05778040916215522460, 0.4822834645669289988 ) ) ;
#58467 = CARTESIAN_POINT ( 'NONE',  ( -0.03937007874015669567, -0.6692913385826771977, 8.415575281601705876E-17 ) ) ;
#58468 = CARTESIAN_POINT ( 'NONE',  ( -0.8267716535433065062, -0.6692913385826771977, 8.415575281601705876E-17 ) ) ;
#58469 = CARTESIAN_POINT ( 'NONE',  ( 1.279527559055118724, -0.4536011799217368745, -0.2665933059059886201 ) ) ;
#58470 = CARTESIAN_POINT ( 'NONE',  ( -1.443569553805773564, 0.2306618581243847221, -0.2411417322834647770 ) ) ;
#58471 = LINE ( 'NONE', #71111, #39708 ) ;
#58472 = CARTESIAN_POINT ( 'NONE',  ( 0.9251968503937015864, -0.4536011799217367080, 0.2665933059059888421 ) ) ;
#58473 = CARTESIAN_POINT ( 'NONE',  ( 0.2755905511811031494, 0.2952755905511811885, 0.000000000000000000 ) ) ;
#58474 = CARTESIAN_POINT ( 'NONE',  ( 0.7545931758530189937, 0.2952755905511810774, -0.1292274648535930714 ) ) ;
#58475 = CARTESIAN_POINT ( 'NONE',  ( -0.2925321140481930704, -0.2925321140481933480, -1.318897637795275690 ) ) ;
#58476 = CYLINDRICAL_SURFACE ( 'NONE', #10390, 0.07874015748031495954 ) ;
#58477 = CARTESIAN_POINT ( 'NONE',  ( 0.3996062992125985480, 2.446882876249141654E-17, -0.8248031496062991907 ) ) ;
#58478 = CARTESIAN_POINT ( 'NONE',  ( 0.1998031496062994128, -0.3460692066303957537, -0.3261154855643044748 ) ) ;
#58479 = CARTESIAN_POINT ( 'NONE',  ( -0.1902887139107604098, -0.6692913385826771977, 0.1292274648535927661 ) ) ;
#58480 = CARTESIAN_POINT ( 'NONE',  ( 0.3460692066303959757, -0.1998031496062991907, -2.782152230971128848 ) ) ;
#58481 = CARTESIAN_POINT ( 'NONE',  ( 0.1958661417322834775, 0.3392501089628018884, -1.961286089238845287 ) ) ;
#58482 = CARTESIAN_POINT ( 'NONE',  ( -1.200787401574802349, -0.4536011799217367080, 0.2665933059059888421 ) ) ;
#58483 = CARTESIAN_POINT ( 'NONE',  ( 1.187664041994751285, -0.3162353388693409650, -0.4822834645669289433 ) ) ;
#58484 = CARTESIAN_POINT ( 'NONE',  ( 1.456692913385827515, -0.6692913385826771977, 8.415575281601705876E-17 ) ) ;
#58485 = CARTESIAN_POINT ( 'NONE',  ( -0.4199475065616791736, -0.5023911411419708095, 0.1820866141732285504 ) ) ;
#58486 = CARTESIAN_POINT ( 'NONE',  ( 0.6233595800524939223, -0.3162353388693405765, 0.4822834645669290543 ) ) ;
#58487 = CARTESIAN_POINT ( 'NONE',  ( -0.1265901696524993347, 0.4724409448818895907, -1.343175853018372834 ) ) ;
#58488 = CARTESIAN_POINT ( 'NONE',  ( 0.2690288713910767848, 0.1771653543307087630, 0.09757992244046791164 ) ) ;
#58489 = CARTESIAN_POINT ( 'NONE',  ( -0.1443569553805768291, 0.05413385826771666132, 0.4176697321401328100 ) ) ;
#58490 = CARTESIAN_POINT ( 'NONE',  ( 0.1974969037888706092, -0.3420746716998660508, -1.270997375328083878 ) ) ;
#58491 = CARTESIAN_POINT ( 'NONE',  ( -1.279527559055116948, -0.5400638737290844871, 0.3530559997133364547 ) ) ;
#58492 = CARTESIAN_POINT ( 'NONE',  ( -0.1958661417322833942, -0.3392501089628018884, -1.637158423393387796 ) ) ;
#58493 = CARTESIAN_POINT ( 'NONE',  ( 0.3608923884514443348, 0.1771653543307087075, -0.09757992244046823083 ) ) ;
#58494 = CARTESIAN_POINT ( 'NONE',  ( -2.575297182719626043, 1.629972608277043822, -0.4653577321740525741 ) ) ;
#58495 = CARTESIAN_POINT ( 'NONE',  ( -0.7939632545931754048, -0.3162353388693405765, 0.4822834645669290543 ) ) ;
#58496 = CARTESIAN_POINT ( 'NONE',  ( -0.3083989501312330295, -0.2845877964562161244, -0.3641732283464567121 ) ) ;
#58497 = CARTESIAN_POINT ( 'NONE',  ( -1.306827173596998737, 0.000000000000000000, 0.4445507791589060065 ) ) ;
#58498 = CARTESIAN_POINT ( 'NONE',  ( -0.5643044619422565855, 0.05413385826771626580, -0.4176697321401330321 ) ) ;
#58499 = CARTESIAN_POINT ( 'NONE',  ( -0.3083989501312330295, -0.3162353388693409650, -0.4822834645669289433 ) ) ;
#58500 = CARTESIAN_POINT ( 'NONE',  ( 0.4658792650918640033, -0.2845877964562159024, 0.3641732283464567677 ) ) ;
#58501 = CARTESIAN_POINT ( 'NONE',  ( -0.2925321140481930149, -0.2925321140481933480, -2.025590551181102317 ) ) ;
#58502 = CARTESIAN_POINT ( 'NONE',  ( 0.09186351706036827158, 0.05413385826771666132, 0.4176697321401328100 ) ) ;
#58503 = CARTESIAN_POINT ( 'NONE',  ( -0.3917322834645670659, 0.1049643490035301607, -2.002605356134171455 ) ) ;
#58504 = VECTOR ( 'NONE', #31178, 39.37007874015748143 ) ;
#58505 = CARTESIAN_POINT ( 'NONE',  ( -1.469816272965878357, -0.5023911411419708095, -0.1820866141732282451 ) ) ;
#58506 = CARTESIAN_POINT ( 'NONE',  ( 0.6496062992125991586, -0.4536011799217368745, -0.2665933059059886201 ) ) ;
#58507 = CARTESIAN_POINT ( 'NONE',  ( 1.601049868766404982, 0.2306618581243848609, 0.2411417322834645549 ) ) ;
#58508 = CARTESIAN_POINT ( 'NONE',  ( -0.6758530183727028406, -0.5511811023622048555, -0.09757992244046775898 ) ) ;
#58509 = CARTESIAN_POINT ( 'NONE',  ( -1.338582677165353729, -0.1870078740157480601, -0.3641732283464567677 ) ) ;
#58510 = CARTESIAN_POINT ( 'NONE',  ( -0.7808398950131222316, -0.3162353388693409650, -0.4822834645669289433 ) ) ;
#58511 = CARTESIAN_POINT ( 'NONE',  ( -0.2296587926509179312, -0.3162353388693409650, -0.4822834645669289433 ) ) ;
#58512 = CARTESIAN_POINT ( 'NONE',  ( 0.5708661417322842269, 0.07958543189024085140, 0.2665933059059887866 ) ) ;
#58513 = CARTESIAN_POINT ( 'NONE',  ( -0.2952755905511810219, 0.005994596871347967343, 5.524802951929910222 ) ) ;
#58514 = CARTESIAN_POINT ( 'NONE',  ( 0.9580052493438326877, -0.004921259842519576551, 0.3153832671262227771 ) ) ;
#58515 = CARTESIAN_POINT ( 'NONE',  ( 0.4921259842519691285, -0.5400638737290845981, -0.3530559997133363437 ) ) ;
#58516 = CARTESIAN_POINT ( 'NONE',  ( -0.1070741851644056997, 0.3996062992125984925, 0.2316272965879264956 ) ) ;
#58517 = CARTESIAN_POINT ( 'NONE',  ( -0.1837270341207343505, -0.6046776061558807314, 0.2411417322834647770 ) ) ;
#58518 = CARTESIAN_POINT ( 'NONE',  ( 0.3917322834645670104, -0.1049643490035303411, -1.298556430446194510 ) ) ;
#58519 = CARTESIAN_POINT ( 'NONE',  ( 1.417322834645670104, -0.1870078740157479769, 0.3641732283464567677 ) ) ;
#58520 = CARTESIAN_POINT ( 'NONE',  ( 0.6627296587926517768, -0.6692913385826773087, -0.1292274648535924053 ) ) ;
#58521 = CARTESIAN_POINT ( 'NONE',  ( 0.09842519685039434474, 0.1660481256975885056, 0.3530559997133364547 ) ) ;
#58522 = CARTESIAN_POINT ( 'NONE',  ( 1.112371124080195450, -4.927456884911482678E-16, 0.4445507791589062840 ) ) ;
#58523 = CARTESIAN_POINT ( 'NONE',  ( -0.05249343832020911260, 0.1283753931104748280, 0.1820866141732283561 ) ) ;
#58524 = CARTESIAN_POINT ( 'NONE',  ( 0.7349081364829403995, 0.2306618581243848609, 0.2411417322834645549 ) ) ;
#58525 = CARTESIAN_POINT ( 'NONE',  ( -0.3280839895013117347, -0.3690944881889763329, 0.3153832671262228327 ) ) ;
#58526 = CARTESIAN_POINT ( 'NONE',  ( -0.6561679790026240244, 0.2306618581243847221, -0.2411417322834647770 ) ) ;
#58527 = CARTESIAN_POINT ( 'NONE',  ( 0.8333333333333340365, 0.2952755905511810219, -0.1292274648535930437 ) ) ;
#58528 = CARTESIAN_POINT ( 'NONE',  ( -0.3280839895013117347, -0.4281496062992124485, 0.4176697321401328655 ) ) ;
#58529 = ORIENTED_EDGE ( 'NONE', *, *, #69225, .F. ) ;
#58530 = CARTESIAN_POINT ( 'NONE',  ( -1.272965879265091305, 0.05413385826771626580, -0.4176697321401330321 ) ) ;
#58531 = CARTESIAN_POINT ( 'NONE',  ( -0.5839895013123351797, 0.1771653543307087075, -0.09757992244046823083 ) ) ;
#58532 = CARTESIAN_POINT ( 'NONE',  ( -0.07874015748031421014, -0.1870078740157480879, -0.4822834645669291653 ) ) ;
#58533 = CARTESIAN_POINT ( 'NONE',  ( -1.456692913385826182, -0.6692913385826771977, 8.415575281601705876E-17 ) ) ;
#58534 = CARTESIAN_POINT ( 'NONE',  ( -0.8202099737532799750, 0.2952755905511810774, -0.1292274648535930714 ) ) ;
#58535 = CARTESIAN_POINT ( 'NONE',  ( -0.4744094488188833059, 1.537401574803149984, -3.908320185825793658 ) ) ;
#58537 = CARTESIAN_POINT ( 'NONE',  ( 1.338582677165355062, -0.1870078740157480879, -0.4822834645669291653 ) ) ;
#58536 = CARTESIAN_POINT ( 'NONE',  ( 1.062992125984252745, 0.2952755905511811885, 0.000000000000000000 ) ) ;
#58538 = CARTESIAN_POINT ( 'NONE',  ( 1.371391076115485941, 0.2952755905511811885, 0.1292274648535926551 ) ) ;
#58539 = CARTESIAN_POINT ( 'NONE',  ( 0.1958661417322834775, 0.3392501089628018884, -2.656167979002624691 ) ) ;
#58540 = DIRECTION ( 'NONE',  ( -1.000000000000000000, -3.083952846180990281E-16, 0.000000000000000000 ) ) ;
#58541 = CARTESIAN_POINT ( 'NONE',  ( -1.128608923884513837, -0.6046776061558807314, 0.2411417322834647770 ) ) ;
#58542 = CARTESIAN_POINT ( 'NONE',  ( 0.2362204724409449064, 0.4091458600556404646, -0.6167979002624671692 ) ) ;
#58543 = EDGE_CURVE ( 'NONE', #78494, #10845, #80040, .T. ) ;
#58544 = CARTESIAN_POINT ( 'NONE',  ( -0.3996062992125987146, 0.1070741851644051862, -0.1902887139107611592 ) ) ;
#58545 = VERTEX_POINT ( 'NONE', #15420 ) ;
#58546 = CARTESIAN_POINT ( 'NONE',  ( -0.2296587926509179312, -0.08942795157527998196, 0.3641732283464567121 ) ) ;
#58547 = CARTESIAN_POINT ( 'NONE',  ( 0.3392501089628018884, -0.1958661417322834220, -1.671916010498687655 ) ) ;
#58548 = ORIENTED_EDGE ( 'NONE', *, *, #59446, .F. ) ;
#58549 = CARTESIAN_POINT ( 'NONE',  ( 0.1509186351706042484, -0.3162353388693405765, 0.4822834645669290543 ) ) ;
#58550 = CARTESIAN_POINT ( 'NONE',  ( 0.3149606299212603933, -0.1870078740157479769, 0.4822834645669291653 ) ) ;
#58551 = CARTESIAN_POINT ( 'NONE',  ( -0.01930322177395173144, 0.3957358693849742926, -2.755905511811586273 ) ) ;
#58552 = DIRECTION ( 'NONE',  ( -1.000000000000000000, -0.000000000000000000, -0.000000000000000000 ) ) ;
#58553 = CARTESIAN_POINT ( 'NONE',  ( -0.8923884514435688198, -0.5023911411419708095, 0.1820866141732285504 ) ) ;
#58554 = DIRECTION ( 'NONE',  ( 0.000000000000000000, 0.000000000000000000, -1.000000000000000000 ) ) ;
#58555 = CARTESIAN_POINT ( 'NONE',  ( 0.7020997375328090762, -0.3162353388693405765, 0.4822834645669290543 ) ) ;
#58556 = CARTESIAN_POINT ( 'NONE',  ( 0.8464566929133865436, 0.07958543189024071263, -0.2665933059059888421 ) ) ;
#58557 = CARTESIAN_POINT ( 'NONE',  ( -0.3477690288713902178, 0.2952755905511810774, -0.1292274648535930714 ) ) ;
#58558 = CARTESIAN_POINT ( 'NONE',  ( 0.1958661417322834497, 0.3392501089628018329, -1.326752337761467837 ) ) ;
#58559 = CARTESIAN_POINT ( 'NONE',  ( -0.8398950131233585692, 0.2306618581243848609, 0.2411417322834645549 ) ) ;
#58560 = PLANE ( 'NONE',  #31798 ) ;
#58561 = CARTESIAN_POINT ( 'NONE',  ( 1.181102362204725198, -0.1870078740157479769, 0.4822834645669291653 ) ) ;
#58562 = CARTESIAN_POINT ( 'NONE',  ( 1.633858267716535639, -0.4536011799217367080, 0.2665933059059888421 ) ) ;
#58563 = ORIENTED_EDGE ( 'NONE', *, *, #10855, .F. ) ;
#58564 = CARTESIAN_POINT ( 'NONE',  ( -0.1049643490035302301, -0.3917322834645671770, -2.588601992947193509 ) ) ;
#58565 = CARTESIAN_POINT ( 'NONE',  ( -0.1246719160104980823, -0.6692913385826773087, -0.1292274648535924053 ) ) ;
#58566 = VERTEX_POINT ( 'NONE', #33933 ) ;
#58567 = AXIS2_PLACEMENT_3D ( 'NONE', #528, #83019, #25342 ) ;
#58568 = CARTESIAN_POINT ( 'NONE',  ( -0.6430446194225716283, -0.4281496062992124485, 0.4176697321401328655 ) ) ;
#58569 = CARTESIAN_POINT ( 'NONE',  ( 1.220472440944882386, -0.6692913385826771977, 8.415575281601705876E-17 ) ) ;
#58570 = CARTESIAN_POINT ( 'NONE',  ( 1.056430446194226436, -0.6692913385826773087, -0.1292274648535924053 ) ) ;
#58571 = CARTESIAN_POINT ( 'NONE',  ( 0.4330708661417329575, -0.6692913385826771977, 8.415575281601705876E-17 ) ) ;
#58572 = CARTESIAN_POINT ( 'NONE',  ( -0.5708661417322825615, -0.5400638737290844871, 0.3530559997133364547 ) ) ;
#58573 = CARTESIAN_POINT ( 'NONE',  ( 0.1049643490035304938, -0.3917322834645669549, -1.902230971128608727 ) ) ;
#58574 = CARTESIAN_POINT ( 'NONE',  ( -0.9973753280839886548, -0.6046776061558809534, -0.2411417322834644161 ) ) ;
#58575 = CARTESIAN_POINT ( 'NONE',  ( -0.04593175853018302557, 0.2952755905511811885, 0.1292274648535926551 ) ) ;
#58576 = CARTESIAN_POINT ( 'NONE',  ( -0.1377952755905504645, -0.4536011799217368745, -0.2665933059059886201 ) ) ;
#58577 = CARTESIAN_POINT ( 'NONE',  ( 1.666666666666667185, 0.05413385826771666132, 0.4176697321401328100 ) ) ;
#58578 = CARTESIAN_POINT ( 'NONE',  ( 1.325459317585302665, -0.4281496062992124485, 0.4176697321401328655 ) ) ;
#58579 = CARTESIAN_POINT ( 'NONE',  ( -0.3149606299212590610, -0.1870078740157479769, 0.4822834645669291653 ) ) ;
#58580 = CARTESIAN_POINT ( 'NONE',  ( -0.6299212598425059095, 1.724409448818897905, -3.937007874015764131 ) ) ;
#58581 = CARTESIAN_POINT ( 'NONE',  ( 1.194225721784777594, -0.4281496062992127816, -0.4176697321401328100 ) ) ;
#58582 = LINE ( 'NONE', #39647, #38867 ) ;
#58583 = VERTEX_POINT ( 'NONE', #54942 ) ;
#58584 = CARTESIAN_POINT ( 'NONE',  ( 0.2887139107611556010, 0.2306618581243847221, -0.2411417322834647770 ) ) ;
#58585 = CARTESIAN_POINT ( 'NONE',  ( -0.3412073490813641308, -0.5023911411419708095, 0.1820866141732285504 ) ) ;
#58587 = CARTESIAN_POINT ( 'NONE',  ( -1.614173228346457378, 0.4410134679336882302, 0.1372047244094476981 ) ) ;
#58586 = CARTESIAN_POINT ( 'NONE',  ( 1.364829396325460076, 0.1283753931104748280, 0.1820866141732283561 ) ) ;
#58588 = CARTESIAN_POINT ( 'NONE',  ( -0.4724409448818895907, -0.1265901696524993070, -0.1227034120734908362 ) ) ;
#58589 = CARTESIAN_POINT ( 'NONE',  ( 1.561679790026247350, -0.004921259842519870586, -0.3153832671262229437 ) ) ;
#58590 = CARTESIAN_POINT ( 'NONE',  ( 1.194225721784777594, -0.4281496062992127816, -0.4176697321401328100 ) ) ;
#58591 = CARTESIAN_POINT ( 'NONE',  ( -0.3949938075777409963, -7.255918531996591613E-17, 0.04133858267716533641 ) ) ;
#58592 = CARTESIAN_POINT ( 'NONE',  ( 0.08530183727034192087, -0.3162353388693409650, -0.4822834645669289433 ) ) ;
#58593 = CARTESIAN_POINT ( 'NONE',  ( 1.348312163386739426, 0.000000000000000000, 0.7386866130305692613 ) ) ;
#58594 = CARTESIAN_POINT ( 'NONE',  ( 1.594488188976378673, 0.07958543189024085140, 0.2665933059059887866 ) ) ;
#58595 = CARTESIAN_POINT ( 'NONE',  ( 5.463695987328526437E-16, -0.1870078740157479769, 0.4822834645669291653 ) ) ;
#58596 = CARTESIAN_POINT ( 'NONE',  ( -0.2891555358219909388, -0.2891555358219912164, 0.02165354330708659999 ) ) ;
#58597 = CARTESIAN_POINT ( 'NONE',  ( 1.607611548556431069, -0.6692913385826773087, -0.1292274648535924053 ) ) ;
#58598 = CARTESIAN_POINT ( 'NONE',  ( 0.7217847769028878924, -0.4281496062992127816, -0.4176697321401328100 ) ) ;
#58599 = CARTESIAN_POINT ( 'NONE',  ( 0.8333333333333340365, -0.5511811023622046335, 0.09757992244046803654 ) ) ;
#58600 = CARTESIAN_POINT ( 'NONE',  ( -0.03280839895013062946, 0.2952755905511810219, -0.1292274648535930437 ) ) ;
#58601 = CARTESIAN_POINT ( 'NONE',  ( 0.8989501312335964611, 0.1771653543307087630, 0.09757992244046791164 ) ) ;
#58602 = CARTESIAN_POINT ( 'NONE',  ( -1.332020997375327642, -0.05778040916215522460, 0.4822834645669289988 ) ) ;
#58603 = CARTESIAN_POINT ( 'NONE',  ( 0.3460692066303958092, 0.1998031496062993018, -0.9954068241469815614 ) ) ;
#58604 = CARTESIAN_POINT ( 'NONE',  ( 1.325459317585302665, -0.4281496062992124485, 0.4176697321401328655 ) ) ;
#58605 = CARTESIAN_POINT ( 'NONE',  ( 0.3392501089628018329, 0.1958661417322835607, -0.5958005249343831800 ) ) ;
#58606 = CIRCLE ( 'NONE', #65365, 2.204724409448819422 ) ;
#58608 = CARTESIAN_POINT ( 'NONE',  ( -0.4724409448818898682, -8.678599364036362592E-17, -0.4311023622047244208 ) ) ;
#58607 = CARTESIAN_POINT ( 'NONE',  ( 0.6955380577427828781, -0.4281496062992124485, 0.4176697321401328655 ) ) ;
#58609 = CARTESIAN_POINT ( 'NONE',  ( -0.3812812444996365180, -2.294479370626195693E-15, 0.3464511005275217603 ) ) ;
#58610 = CARTESIAN_POINT ( 'NONE',  ( 0.5249343832021003964, 0.1283753931104746893, -0.1820866141732285504 ) ) ;
#58611 = CARTESIAN_POINT ( 'NONE',  ( 0.4790026246719168435, -0.3162353388693409650, -0.4822834645669289433 ) ) ;
#58612 = CARTESIAN_POINT ( 'NONE',  ( 1.666666666666667185, -0.004921259842519576551, 0.3153832671262227771 ) ) ;
#58613 = CARTESIAN_POINT ( 'NONE',  ( -1.017060367454067249, -0.2845877964562161244, -0.3641732283464567121 ) ) ;
#58614 = CARTESIAN_POINT ( 'NONE',  ( -0.8530183727034112984, -0.4281496062992127816, -0.4176697321401328100 ) ) ;
#58615 = CARTESIAN_POINT ( 'NONE',  ( -1.679790026246718693, 0.2306618581243847221, -0.2411417322834647770 ) ) ;
#58616 = CARTESIAN_POINT ( 'NONE',  ( 0.9580052493438327987, -0.4281496062992127816, -0.4176697321401328100 ) ) ;
#58617 = CARTESIAN_POINT ( 'NONE',  ( 1.535433070866142558, 0.2952755905511811885, 0.000000000000000000 ) ) ;
#58618 = CARTESIAN_POINT ( 'NONE',  ( 1.063819296904228162, 1.224016087139557341, -0.3574819075361487797 ) ) ;
#58619 = CARTESIAN_POINT ( 'NONE',  ( 0.8661417322834652488, -0.1870078740157480879, -0.4822834645669291653 ) ) ;
#58620 = CARTESIAN_POINT ( 'NONE',  ( -0.4724409448818898682, -8.678599364036362592E-17, -2.320866141732283783 ) ) ;
#58621 = VECTOR ( 'NONE', #4558, 39.37007874015748143 ) ;
#58622 = CARTESIAN_POINT ( 'NONE',  ( 0.2895750033033090975, 1.160328408095293806, 3.926430088202063295 ) ) ;
#58623 = CARTESIAN_POINT ( 'NONE',  ( 1.581364829396326277, -0.3162353388693409650, -0.4822834645669289433 ) ) ;
#58624 = CARTESIAN_POINT ( 'NONE',  ( -1.351706036745406347, -0.004921259842519870586, -0.3153832671262229437 ) ) ;
#58625 = CARTESIAN_POINT ( 'NONE',  ( 1.049868766404200349, 0.1283753931104748280, 0.1820866141732283561 ) ) ;
#58626 = CARTESIAN_POINT ( 'NONE',  ( -1.469816272965878357, 0.1283753931104748280, 0.1820866141732283561 ) ) ;
#58627 = CARTESIAN_POINT ( 'NONE',  ( -0.5839895013123351797, -0.5511811023622046335, 0.09757992244046803654 ) ) ;
#58628 = CARTESIAN_POINT ( 'NONE',  ( -1.522309711286088607, 0.1283753931104746893, -0.1820866141732285504 ) ) ;
#58629 = CARTESIAN_POINT ( 'NONE',  ( 1.102362204724410155, -0.1870078740157479769, 0.3641732283464567677 ) ) ;
#58630 = CARTESIAN_POINT ( 'NONE',  ( 0.4986876640419954376, -0.6046776061558809534, -0.2411417322834644161 ) ) ;
#58631 = CARTESIAN_POINT ( 'NONE',  ( 1.122047244094488860, 0.1660481256975885056, 0.3530559997133364547 ) ) ;
#58632 = CARTESIAN_POINT ( 'NONE',  ( -0.06561679790026180015, 0.05413385826771666132, 0.4176697321401328100 ) ) ;
#58633 = CARTESIAN_POINT ( 'NONE',  ( 0.6496062992125991586, 0.07958543189024085140, 0.2665933059059887866 ) ) ;
#58634 = CARTESIAN_POINT ( 'NONE',  ( 1.095800524934383846, -0.3162353388693405765, 0.4822834645669290543 ) ) ;
#58635 = EDGE_CURVE ( 'NONE', #53475, #12926, #39042, .T. ) ;
#58636 = CARTESIAN_POINT ( 'NONE',  ( -0.6299212598425202314, 1.968503937007873628, 0.000000000000000000 ) ) ;
#58637 = CARTESIAN_POINT ( 'NONE',  ( -0.6889763779527552368, -0.5400638737290845981, -0.3530559997133363437 ) ) ;
#58638 = CARTESIAN_POINT ( 'NONE',  ( -0.3996062992125985480, -0.1070741851644057135, -0.3608923884514435576 ) ) ;
#58639 = CARTESIAN_POINT ( 'NONE',  ( -0.2965319783527583519, 1.197814162742229627, 0.1004664927356394566 ) ) ;
#58640 = CARTESIAN_POINT ( 'NONE',  ( 0.08530183727034192087, -0.3162353388693409650, -0.4822834645669289433 ) ) ;
#58641 = CARTESIAN_POINT ( 'NONE',  ( -0.2296587926509179312, -0.05778040916215522460, 0.4822834645669289988 ) ) ;
#58642 = CARTESIAN_POINT ( 'NONE',  ( 0.1377952755905518800, -0.5400638737290844871, 0.3530559997133364547 ) ) ;
#58643 = CARTESIAN_POINT ( 'NONE',  ( 0.3996062992125986035, 0.1070741851644054776, -2.644356955380577912 ) ) ;
#58644 = CARTESIAN_POINT ( 'NONE',  ( -0.1974969037888706647, 0.3420746716998658843, -2.060367454068241067 ) ) ;
#58645 = CARTESIAN_POINT ( 'NONE',  ( 0.3917322834645669549, 0.1049643490035304660, -0.5892388451443569819 ) ) ;
#58647 = EDGE_CURVE ( 'NONE', #38771, #53888, #47380, .T. ) ;
#58646 = CARTESIAN_POINT ( 'NONE',  ( 0.2431027332089026050, -0.1676825148875300264, 5.760293869191739802 ) ) ;
#58648 = CARTESIAN_POINT ( 'NONE',  ( 0.3392501089628018329, 0.1958661417322835607, -0.9107611548556429071 ) ) ;
#58649 = CARTESIAN_POINT ( 'NONE',  ( -1.122047244094487306, -0.4536011799217367080, 0.2665933059059888421 ) ) ;
#58650 = CARTESIAN_POINT ( 'NONE',  ( 0.1958661417322834775, 0.3392501089628018884, -1.238845144356955252 ) ) ;
#58651 = CARTESIAN_POINT ( 'NONE',  ( -1.299212598425196097, -0.6692913385826771977, 8.415575281601705876E-17 ) ) ;
#58652 = CARTESIAN_POINT ( 'NONE',  ( -0.1049643490035301746, -0.3917322834645670659, 0.005268659613860090553 ) ) ;
#58653 = CARTESIAN_POINT ( 'NONE',  ( 0.3477690288713918276, -0.6692913385826773087, -0.1292274648535924053 ) ) ;
#58654 = CARTESIAN_POINT ( 'NONE',  ( -0.3346456692913377662, -0.4536011799217367080, 0.2665933059059888421 ) ) ;
#58655 = CARTESIAN_POINT ( 'NONE',  ( 1.469816272965879911, 0.2306618581243847221, -0.2411417322834647770 ) ) ;
#58656 = CARTESIAN_POINT ( 'NONE',  ( 0.4527559055118117182, -0.5400638737290844871, 0.3530559997133364547 ) ) ;
#58657 = CARTESIAN_POINT ( 'NONE',  ( 0.4490604499032361252, 1.383603895493148883, 1.028280011760609458 ) ) ;
#58658 = VECTOR ( 'NONE', #16702, 39.37007874015748143 ) ;
#58659 = CARTESIAN_POINT ( 'NONE',  ( -0.3996062992125986035, -7.340648628747425578E-17, -2.716535433070865757 ) ) ;
#58660 = CARTESIAN_POINT ( 'NONE',  ( 0.1049643490035303967, 0.3917322834645670659, -1.250019315781839113 ) ) ;
#58661 = CARTESIAN_POINT ( 'NONE',  ( 1.062992125984252745, 0.2952755905511811885, 0.000000000000000000 ) ) ;
#58662 = CIRCLE ( 'NONE', #69423, 0.09842519685039365085 ) ;
#58663 = CARTESIAN_POINT ( 'NONE',  ( 0.4921259842519691285, 0.1660481256975885056, 0.3530559997133364547 ) ) ;
#58664 = CARTESIAN_POINT ( 'NONE',  ( 0.1312335958005255154, -0.6046776061558807314, 0.2411417322834647770 ) ) ;
#58665 = CARTESIAN_POINT ( 'NONE',  ( 1.391076115485564868, 0.2306618581243847221, -0.2411417322834647770 ) ) ;
#58666 = CARTESIAN_POINT ( 'NONE',  ( 0.1049643490035304938, -0.3917322834645669549, -0.4849081364829396779 ) ) ;
#58667 = CARTESIAN_POINT ( 'NONE',  ( -0.02624671916010428221, -0.6046776061558807314, 0.2411417322834647770 ) ) ;
#58668 = CARTESIAN_POINT ( 'NONE',  ( 1.128608923884515169, -0.6046776061558809534, -0.2411417322834644161 ) ) ;
#58669 = CARTESIAN_POINT ( 'NONE',  ( 0.2230971128608932319, -0.4281496062992124485, 0.4176697321401328655 ) ) ;
#58670 = CARTESIAN_POINT ( 'NONE',  ( 0.9842519685039378130, -0.5511811023622047445, 6.969142054262312111E-17 ) ) ;
#58671 = CARTESIAN_POINT ( 'NONE',  ( -0.9120734908136475250, 0.2952755905511811885, 0.1292274648535926551 ) ) ;
#58672 = CARTESIAN_POINT ( 'NONE',  ( -1.227034120734907585, 0.2952755905511811885, 0.1292274648535926551 ) ) ;
#58673 = CARTESIAN_POINT ( 'NONE',  ( 0.7874015748031503170, -0.1870078740157479769, 0.4822834645669291653 ) ) ;
#58674 = CARTESIAN_POINT ( 'NONE',  ( 0.3149606299212736049, 2.559055118110236560, -3.924389226575467404 ) ) ;
#58675 = CARTESIAN_POINT ( 'NONE',  ( 0.3392501089628018329, 0.1958661417322835607, -2.013123359580052618 ) ) ;
#58676 = ORIENTED_EDGE ( 'NONE', *, *, #81439, .F. ) ;
#58677 = CARTESIAN_POINT ( 'NONE',  ( -0.1998031496062991907, -0.3460692066303959757, -0.06561679790026248016 ) ) ;
#58678 = ORIENTED_EDGE ( 'NONE', *, *, #56444, .T. ) ;
#58679 = CARTESIAN_POINT ( 'NONE',  ( 1.423884514435696413, -0.3162353388693409650, -0.4822834645669289433 ) ) ;
#58680 = CARTESIAN_POINT ( 'NONE',  ( 0.8530183727034126306, -0.004921259842519870586, -0.3153832671262229437 ) ) ;
#58681 = CARTESIAN_POINT ( 'NONE',  ( 0.3458507752293908943, 0.3458507752293908943, -2.419291338582677309 ) ) ;
#58682 = CARTESIAN_POINT ( 'NONE',  ( -0.09186351706036689768, 0.05413385826771626580, -0.4176697321401330321 ) ) ;
#58683 = CARTESIAN_POINT ( 'NONE',  ( -1.363814626685859288, 0.1354692512615922884, -0.3875633260700434568 ) ) ;
#58684 = CARTESIAN_POINT ( 'NONE',  ( -0.2867679344610364334, -0.2867679344610367109, -0.9311023622047245318 ) ) ;
#58685 = CARTESIAN_POINT ( 'NONE',  ( -1.305774278215222184, 0.1771653543307087630, 0.09757992244046791164 ) ) ;
#58686 = CARTESIAN_POINT ( 'NONE',  ( -1.502624671916009680, -0.08942795157528024563, -0.3641732283464568787 ) ) ;
#58687 = CARTESIAN_POINT ( 'NONE',  ( -0.3981765293560192709, -0.002049465651759719426, -1.929133858267716217 ) ) ;
#58688 = CARTESIAN_POINT ( 'NONE',  ( -0.4330708661417315697, 0.2952755905511811885, 0.000000000000000000 ) ) ;
#58689 = CARTESIAN_POINT ( 'NONE',  ( 1.082677165354331228, -0.5400638737290844871, 0.3530559997133364547 ) ) ;
#58690 = ORIENTED_EDGE ( 'NONE', *, *, #35732, .T. ) ;
#58691 = CARTESIAN_POINT ( 'NONE',  ( -1.515748031496062076, 0.1660481256975883668, -0.3530559997133364547 ) ) ;
#58692 = CARTESIAN_POINT ( 'NONE',  ( 0.5288531115723354992, 1.522331584275770089, 0.5046369196612368047 ) ) ;
#58693 = DIRECTION ( 'NONE',  ( -1.000000000000000000, 0.000000000000000000, -6.982962677686266711E-15 ) ) ;
#58694 = DIRECTION ( 'NONE',  ( 0.000000000000000000, -0.000000000000000000, 1.000000000000000000 ) ) ;
#58695 = DIRECTION ( 'NONE',  ( -1.000000000000000000, -0.000000000000000000, -0.000000000000000000 ) ) ;
#58696 = CARTESIAN_POINT ( 'NONE',  ( -0.8136482939632537770, 0.1283753931104746893, -0.1820866141732285504 ) ) ;
#58697 = CARTESIAN_POINT ( 'NONE',  ( -1.522309711286088607, -0.6046776061558807314, 0.2411417322834647770 ) ) ;
#58698 = CARTESIAN_POINT ( 'NONE',  ( 0.5052493438320218022, -0.6692913385826773087, -0.1292274648535924053 ) ) ;
#58699 = VERTEX_POINT ( 'NONE', #35595 ) ;
#58701 = DIRECTION ( 'NONE',  ( 1.000000000000000000, -0.000000000000000000, -0.000000000000000000 ) ) ;
#58700 = CARTESIAN_POINT ( 'NONE',  ( -0.7478466213799872531, 2.204724409448818978, 0.5309055118110236338 ) ) ;
#58702 = CARTESIAN_POINT ( 'NONE',  ( 1.358267716535433323, 0.1660481256975885056, 0.3530559997133364547 ) ) ;
#58703 = CARTESIAN_POINT ( 'NONE',  ( -1.692913385826770645, 0.2952755905511811885, 0.000000000000000000 ) ) ;
#58704 = CARTESIAN_POINT ( 'NONE',  ( -0.1958661417322834497, -0.3392501089628018884, -0.9330515503598931781 ) ) ;
#58705 = CARTESIAN_POINT ( 'NONE',  ( -0.9580052493438311334, -0.3690944881889763329, 0.3153832671262228327 ) ) ;
#58706 = EDGE_CURVE ( 'NONE', #78262, #21338, #61258, .T. ) ;
#58707 = CARTESIAN_POINT ( 'NONE',  ( -1.423884514435694859, -0.08942795157528024563, -0.3641732283464568787 ) ) ;
#58708 = CARTESIAN_POINT ( 'NONE',  ( -0.3458507752293909498, 0.3458507752293908388, -0.8070866141732283561 ) ) ;
#58709 = CARTESIAN_POINT ( 'NONE',  ( 0.3543307086614179147, 0.2952755905511811885, 0.000000000000000000 ) ) ;
#58710 = CARTESIAN_POINT ( 'NONE',  ( -0.7283464566929126471, -0.4536011799217367080, 0.2665933059059888421 ) ) ;
#58711 = CARTESIAN_POINT ( 'NONE',  ( 0.1443569553805781891, -0.3690944881889763329, 0.3153832671262228327 ) ) ;
#58712 = CARTESIAN_POINT ( 'NONE',  ( 0.2165354330708668673, 0.1660481256975883668, -0.3530559997133364547 ) ) ;
#58713 = CARTESIAN_POINT ( 'NONE',  ( -1.253280839895012377, -0.2845877964562161244, -0.3641732283464567121 ) ) ;
#58714 = CARTESIAN_POINT ( 'NONE',  ( 0.1958661417322834775, 0.3392501089628018884, 0.01638488369322645480 ) ) ;
#58715 = CARTESIAN_POINT ( 'NONE',  ( 0.7152230971128614723, -0.3162353388693409650, -0.4822834645669289433 ) ) ;
#58716 = AXIS2_PLACEMENT_3D ( 'NONE', #70969, #52841, #71807 ) ;
#58717 = AXIS2_PLACEMENT_3D ( 'NONE', #9443, #35948, #81403 ) ;
#58718 = CARTESIAN_POINT ( 'NONE',  ( -1.548556430446193399, -0.6046776061558809534, -0.2411417322834644161 ) ) ;
#58719 = CARTESIAN_POINT ( 'NONE',  ( -0.1265901696524986964, -0.4724409448818899238, -1.251312335958005173 ) ) ;
#58720 = AXIS2_PLACEMENT_3D ( 'NONE', #56569, #6475, #57801 ) ;
#58721 = CARTESIAN_POINT ( 'NONE',  ( -0.7939632545931754048, -0.3162353388693405765, 0.4822834645669290543 ) ) ;
#58722 = CARTESIAN_POINT ( 'NONE',  ( -0.3477690288713905509, -0.5511811023622046335, 0.09757992244046803654 ) ) ;
#58723 = CARTESIAN_POINT ( 'NONE',  ( -0.8070866141732276899, 0.1660481256975883668, -0.3530559997133364547 ) ) ;
#58724 = CARTESIAN_POINT ( 'NONE',  ( 0.9973753280839902091, -0.5023911411419708095, 0.1820866141732285504 ) ) ;
#58725 = CARTESIAN_POINT ( 'NONE',  ( -0.4133858267716528645, 0.07958543189024071263, -0.2665933059059888421 ) ) ;
#58726 = CARTESIAN_POINT ( 'NONE',  ( -0.6758530183727028406, -0.6692913385826773087, -0.1292274648535924053 ) ) ;
#58727 = CARTESIAN_POINT ( 'NONE',  ( -1.043307086614172707, 0.1660481256975883668, -0.3530559997133364547 ) ) ;
#58728 = CARTESIAN_POINT ( 'NONE',  ( 1.673228346456693494, 0.1660481256975885056, 0.3530559997133364547 ) ) ;
#58729 = CARTESIAN_POINT ( 'NONE',  ( 0.4091458600556403535, 0.2362204724409449896, -2.097769028871391050 ) ) ;
#58730 = CARTESIAN_POINT ( 'NONE',  ( 1.430446194225722500, -0.3690944881889765550, -0.3153832671262227771 ) ) ;
#58731 = PRODUCT_DEFINITION_SHAPE ( 'NONE', 'NONE',  #25919 ) ;
#58732 = CARTESIAN_POINT ( 'NONE',  ( 0.2559055118110243332, 0.1660481256975885056, 0.3530559997133364547 ) ) ;
#58733 = CARTESIAN_POINT ( 'NONE',  ( 1.220472440944882164, 0.2066929133858268208, 4.479895975645240118E-15 ) ) ;
#58734 = CARTESIAN_POINT ( 'NONE',  ( -1.660104986876639543, -0.05778040916215560624, -0.4822834645669293319 ) ) ;
#58735 = VERTEX_POINT ( 'NONE', #72653 ) ;
#58736 = CARTESIAN_POINT ( 'NONE',  ( 0.1070741851644054776, -0.3996062992125984925, -2.366797900262467280 ) ) ;
#58737 = CARTESIAN_POINT ( 'NONE',  ( -1.069553805774277722, -0.5511811023622048555, -0.09757992244046775898 ) ) ;
#58738 = CARTESIAN_POINT ( 'NONE',  ( 0.7611548556430451917, -0.6046776061558807314, 0.2411417322834647770 ) ) ;
#58739 = CARTESIAN_POINT ( 'NONE',  ( -1.102362204724408601, -0.1870078740157479769, 0.3641732283464567677 ) ) ;
#58740 = CARTESIAN_POINT ( 'NONE',  ( 0.2925321140481932369, 0.2925321140481932369, -1.946850393700787496 ) ) ;
#58741 = CARTESIAN_POINT ( 'NONE',  ( -1.128608923884513837, -0.6046776061558807314, 0.2411417322834647770 ) ) ;
#58742 = CARTESIAN_POINT ( 'NONE',  ( 0.7939632545931766261, -0.3162353388693409650, -0.4822834645669289433 ) ) ;
#58743 = CARTESIAN_POINT ( 'NONE',  ( 0.4527559055118117182, 0.1660481256975883668, -0.3530559997133364547 ) ) ;
#58744 = CARTESIAN_POINT ( 'NONE',  ( 1.279527559055118724, 0.1660481256975885056, 0.3530559997133364547 ) ) ;
#58745 = CARTESIAN_POINT ( 'NONE',  ( -1.489501312335957062, -0.2845877964562161244, -0.3641732283464567121 ) ) ;
#58746 = CARTESIAN_POINT ( 'NONE',  ( 0.1998031496062994128, -0.3460692066303957537, -1.113517060367454015 ) ) ;
#58747 = CARTESIAN_POINT ( 'NONE',  ( 0.1998031496062994405, -0.3460692066303958092, -1.351706036745406792 ) ) ;
#58748 = CARTESIAN_POINT ( 'NONE',  ( -0.1058382717557497937, -0.3949938075777411628, -0.7020997375328085210 ) ) ;
#58749 = CARTESIAN_POINT ( 'NONE',  ( 0.1181102362204724254, 8.537024980200824098E-18, 0.000000000000000000 ) ) ;
#58750 = CARTESIAN_POINT ( 'NONE',  ( 0.9251968503937015864, 0.07958543189024071263, -0.2665933059059888421 ) ) ;
#58751 = CARTESIAN_POINT ( 'NONE',  ( 0.4658792650918640033, -0.2845877964562159024, 0.3641732283464567677 ) ) ;
#58752 = CARTESIAN_POINT ( 'NONE',  ( 0.006561679790026889343, -0.05778040916215522460, 0.4822834645669289988 ) ) ;
#58753 = CARTESIAN_POINT ( 'NONE',  ( 1.292650918635171564, 0.2952755905511811885, 0.1292274648535926551 ) ) ;
#58754 = CARTESIAN_POINT ( 'NONE',  ( 0.3949938075777409963, 2.418639510665530743E-17, -1.927165354330708569 ) ) ;
#58755 = CARTESIAN_POINT ( 'NONE',  ( 0.2230971128608932319, -0.3690944881889763329, 0.3153832671262228327 ) ) ;
#58756 = CARTESIAN_POINT ( 'NONE',  ( -0.8398950131233585692, 0.2306618581243848609, 0.2411417322834645549 ) ) ;
#58757 = CARTESIAN_POINT ( 'NONE',  ( 1.417322834645670104, -0.1870078740157479769, 0.4822834645669291653 ) ) ;
#58758 = CARTESIAN_POINT ( 'NONE',  ( 0.9120734908136490793, 0.2952755905511810774, -0.1292274648535930714 ) ) ;
#58759 = CARTESIAN_POINT ( 'NONE',  ( -0.4724409448818895907, -0.1265901696524993070, -1.935695538057742526 ) ) ;
#58760 = CARTESIAN_POINT ( 'NONE',  ( 0.3698506310979001177, -0.1308238996069263915, -2.755905511811022723 ) ) ;
#58761 = ORIENTED_EDGE ( 'NONE', *, *, #55316, .F. ) ;
#58762 = ORIENTED_EDGE ( 'NONE', *, *, #29439, .T. ) ;
#58763 = CARTESIAN_POINT ( 'NONE',  ( -1.443569553805773564, -0.6046776061558807314, 0.2411417322834647770 ) ) ;
#58765 = CARTESIAN_POINT ( 'NONE',  ( -0.5774278215223089816, -0.6046776061558807314, 0.2411417322834647770 ) ) ;
#58764 = CARTESIAN_POINT ( 'NONE',  ( -0.6955380577427815458, -0.004921259842519576551, 0.3153832671262227771 ) ) ;
#58766 = CARTESIAN_POINT ( 'NONE',  ( 4.797336870675655290E-17, -0.3917322834645669549, -2.363497744585615123 ) ) ;
#58767 = CARTESIAN_POINT ( 'NONE',  ( -0.1998031496062994405, 0.3460692066303957537, -2.767060367454068359 ) ) ;
#58768 = CARTESIAN_POINT ( 'NONE',  ( -1.548556430446193399, -0.5023911411419708095, -0.1820866141732282451 ) ) ;
#58769 = CARTESIAN_POINT ( 'NONE',  ( -1.148293963254592542, -0.6692913385826773087, -0.1292274648535924053 ) ) ;
#58770 = CARTESIAN_POINT ( 'NONE',  ( 0.1312335958005255154, -0.6046776061558807314, 0.2411417322834647770 ) ) ;
#58771 = ADVANCED_FACE ( 'NONE', ( #80648 ), #48627, .F. ) ;
#58772 = CARTESIAN_POINT ( 'NONE',  ( -1.207349081364828436, -0.6046776061558807314, 0.2411417322834647770 ) ) ;
#58773 = CARTESIAN_POINT ( 'NONE',  ( -0.2867679344610364334, -0.2867679344610368219, -2.816253650097426231 ) ) ;
#58774 = ADVANCED_FACE ( 'NONE', ( #21308 ), #40660, .F. ) ;
#58775 = EDGE_CURVE ( 'NONE', #30834, #38086, #67246, .T. ) ;
#58776 = CARTESIAN_POINT ( 'NONE',  ( 0.4330708661417329575, -0.6692913385826771977, 8.415575281601705876E-17 ) ) ;
#58777 = CARTESIAN_POINT ( 'NONE',  ( -0.3392501089628017219, -0.1958661417322836718, -1.934383202099737575 ) ) ;
#58778 = CARTESIAN_POINT ( 'NONE',  ( -0.6627296587926501115, 0.1771653543307087075, -0.09757992244046823083 ) ) ;
#58779 = ORIENTED_EDGE ( 'NONE', *, *, #28811, .F. ) ;
#58780 = CARTESIAN_POINT ( 'NONE',  ( 0.3949938075777409963, 2.418639510665530435E-17, -1.850393700787401396 ) ) ;
#58781 = AXIS2_PLACEMENT_3D ( 'NONE', #58070, #436, #33670 ) ;
#58782 = VERTEX_POINT ( 'NONE', #81882 ) ;
#58783 = FACE_OUTER_BOUND ( 'NONE', #9994, .T. ) ;
#58784 = AXIS2_PLACEMENT_3D ( 'NONE', #65309, #33318, #491 ) ;
#58785 = CARTESIAN_POINT ( 'NONE',  ( -1.187664041994750175, -0.05778040916215560624, -0.4822834645669293319 ) ) ;
#58786 = CARTESIAN_POINT ( 'NONE',  ( -1.207349081364828436, -0.6046776061558807314, 0.2411417322834647770 ) ) ;
#58787 = CARTESIAN_POINT ( 'NONE',  ( 0.2925321140481932369, -0.2925321140481932369, -0.5708661417322833387 ) ) ;
#58788 = CARTESIAN_POINT ( 'NONE',  ( -1.017060367454067249, -0.3162353388693409650, -0.4822834645669289433 ) ) ;
#58789 = CARTESIAN_POINT ( 'NONE',  ( -1.174540682414697335, -0.3162353388693409650, -0.4822834645669289433 ) ) ;
#58790 = CARTESIAN_POINT ( 'NONE',  ( -1.259842519685038686, -0.1870078740157480879, -0.4822834645669291653 ) ) ;
#58791 = CARTESIAN_POINT ( 'NONE',  ( 1.348312163386739426, 0.000000000000000000, 0.5221511799597032821 ) ) ;
#58792 = DIRECTION ( 'NONE',  ( 1.047444401652940007E-14, -0.000000000000000000, -1.000000000000000000 ) ) ;
#58793 = CARTESIAN_POINT ( 'NONE',  ( 0.1443569553805781891, -0.004921259842519870586, -0.3153832671262229437 ) ) ;
#58794 = CARTESIAN_POINT ( 'NONE',  ( -2.795275590551184575, 0.7874015748031495399, -3.317813449798768424E-16 ) ) ;
#58795 = CARTESIAN_POINT ( 'NONE',  ( 0.1958661417322834775, 0.3392501089628018884, -0.2290026246719160941 ) ) ;
#58796 = CARTESIAN_POINT ( 'NONE',  ( -0.4790026246719154557, -0.2845877964562159024, 0.3641732283464567677 ) ) ;
#58797 = CARTESIAN_POINT ( 'NONE',  ( -0.8136482939632537770, 0.2306618581243847221, -0.2411417322834647770 ) ) ;
#58798 = CARTESIAN_POINT ( 'NONE',  ( 0.8989501312335963501, -0.6692913385826773087, -0.1292274648535924053 ) ) ;
#58799 = CARTESIAN_POINT ( 'NONE',  ( -0.5446194225721777693, -0.05778040916215522460, 0.4822834645669289988 ) ) ;
#58800 = VERTEX_POINT ( 'NONE', #55350 ) ;
#58801 = ORIENTED_EDGE ( 'NONE', *, *, #70218, .T. ) ;
#58802 = CARTESIAN_POINT ( 'NONE',  ( 0.3996062992125985480, 2.446882876249141654E-17, -1.927165354330708569 ) ) ;
#58803 = CARTESIAN_POINT ( 'NONE',  ( -0.9908136482939626788, 0.2952755905511811885, 0.1292274648535926551 ) ) ;
#58804 = CARTESIAN_POINT ( 'NONE',  ( 1.089238845144357537, -0.4281496062992124485, 0.4176697321401328655 ) ) ;
#58805 = CARTESIAN_POINT ( 'NONE',  ( -1.489501312335957062, -0.2845877964562161244, -0.3641732283464567121 ) ) ;
#58806 =( LENGTH_UNIT ( ) NAMED_UNIT ( * ) SI_UNIT ( $, .METRE. ) );
#58807 = CARTESIAN_POINT ( 'NONE',  ( 0.1265901696524989462, 0.4724409448818897572, -1.253280839895013044 ) ) ;
#58808 = CARTESIAN_POINT ( 'NONE',  ( -2.158445410120303443, 1.605872332714554096, 0.4695140184743379907 ) ) ;
#58809 = EDGE_CURVE ( 'NONE', #11181, #52658, #45027, .T. ) ;
#58810 = CARTESIAN_POINT ( 'NONE',  ( -0.3392501089628019995, 0.1958661417322832277, -0.4908136482939632339 ) ) ;
#58811 = DIRECTION ( 'NONE',  ( 0.000000000000000000, 0.000000000000000000, 1.000000000000000000 ) ) ;
#58812 = CARTESIAN_POINT ( 'NONE',  ( -0.2230971128608915943, 0.05413385826771666132, 0.4176697321401328100 ) ) ;
#58813 = CARTESIAN_POINT ( 'NONE',  ( -1.312335958005248715, 0.1283753931104748280, 0.1820866141732283561 ) ) ;
#58814 = CARTESIAN_POINT ( 'NONE',  ( -0.7217847769028863381, 0.05413385826771626580, -0.4176697321401330321 ) ) ;
#58815 = CARTESIAN_POINT ( 'NONE',  ( -0.1998031496062991630, -0.3460692066303959202, -0.1423884514435695692 ) ) ;
#58817 = CARTESIAN_POINT ( 'NONE',  ( 3.937007874015748143, 2.559055118110236560, 0.3149606299212599492 ) ) ;
#58816 = CARTESIAN_POINT ( 'NONE',  ( -1.122047244094487306, -0.5400638737290844871, 0.3530559997133364547 ) ) ;
#58818 = CARTESIAN_POINT ( 'NONE',  ( -0.8595800524934373854, -0.3162353388693409650, -0.4822834645669289433 ) ) ;
#58819 = CARTESIAN_POINT ( 'NONE',  ( -0.1837270341207343505, -0.6046776061558807314, 0.2411417322834647770 ) ) ;
#58820 = CARTESIAN_POINT ( 'NONE',  ( -0.3949938075777409963, -7.255918531996591613E-17, -2.793307086614173151 ) ) ;
#58821 = CARTESIAN_POINT ( 'NONE',  ( 0.8136482939632553313, 0.1283753931104748280, 0.1820866141732283561 ) ) ;
#58822 = CARTESIAN_POINT ( 'NONE',  ( 0.3917322834645670104, -0.1049643490035303273, -0.1961942257217848540 ) ) ;
#58823 = CARTESIAN_POINT ( 'NONE',  ( 0.9514435695538062676, -0.2845877964562161244, -0.3641732283464567121 ) ) ;
#58824 = CARTESIAN_POINT ( 'NONE',  ( 1.437007874015748810, 0.07958543189024085140, 0.2665933059059887866 ) ) ;
#58825 = CARTESIAN_POINT ( 'NONE',  ( 1.332020997375328974, -0.05778040916215560624, -0.4822834645669293319 ) ) ;
#58826 = CARTESIAN_POINT ( 'NONE',  ( 0.3280839895013130669, -0.3690944881889765550, -0.3153832671262227771 ) ) ;
#58827 = CARTESIAN_POINT ( 'NONE',  ( -0.2867679344610365999, 0.2867679344610364889, -1.744094488188976610 ) ) ;
#58828 = CARTESIAN_POINT ( 'NONE',  ( -1.410761154855641575, -0.3162353388693409650, -0.4822834645669289433 ) ) ;
#58829 = CARTESIAN_POINT ( 'NONE',  ( 1.443569553805774897, 0.2306618581243848609, 0.2411417322834645549 ) ) ;
#58830 = CARTESIAN_POINT ( 'NONE',  ( 0.4724409448818897572, -0.1265901696524988906, -0.03083989501312336262 ) ) ;
#58831 = CARTESIAN_POINT ( 'NONE',  ( -0.6955380577427815458, -0.004921259842519576551, 0.3153832671262227771 ) ) ;
#58832 = CARTESIAN_POINT ( 'NONE',  ( -0.4330708661417315697, 0.2952755905511811885, 0.000000000000000000 ) ) ;
#58833 = CARTESIAN_POINT ( 'NONE',  ( 0.4658792650918641698, -0.05778040916215560624, -0.4822834645669293319 ) ) ;
#58834 = CARTESIAN_POINT ( 'NONE',  ( 0.2362204724409449064, 0.4091458600556404646, -0.6935695538057742304 ) ) ;
#58835 = CARTESIAN_POINT ( 'NONE',  ( 0.7480314960629927956, -0.5511811023622047445, 6.969142054262312111E-17 ) ) ;
#58836 = CARTESIAN_POINT ( 'NONE',  ( -0.04593175853018302557, -0.5511811023622048555, -0.09757992244046775898 ) ) ;
#58837 = CARTESIAN_POINT ( 'NONE',  ( -0.4133858267716528645, -0.5400638737290844871, 0.3530559997133364547 ) ) ;
#58838 = CARTESIAN_POINT ( 'NONE',  ( -1.200787401574802349, 0.1660481256975883668, -0.3530559997133364547 ) ) ;
#58839 = CARTESIAN_POINT ( 'NONE',  ( -0.8595800524934373854, -0.08942795157527998196, 0.3641732283464567121 ) ) ;
#58840 = DIRECTION ( 'NONE',  ( 0.000000000000000000, -1.000000000000000000, 0.000000000000000000 ) ) ;
#58841 = CARTESIAN_POINT ( 'NONE',  ( 0.7480314960629927956, 0.2952755905511811885, 0.000000000000000000 ) ) ;
#58842 = CARTESIAN_POINT ( 'NONE',  ( -0.9448818897637790704, -0.1870078740157480879, -0.4822834645669291653 ) ) ;
#58843 = CARTESIAN_POINT ( 'NONE',  ( -9.787531504996566615E-17, 0.3996062992125985480, -1.021653543307086576 ) ) ;
#58844 = CARTESIAN_POINT ( 'NONE',  ( 0.2867679344610365999, -0.2867679344610365444, -2.545275590551181022 ) ) ;
#58845 = CARTESIAN_POINT ( 'NONE',  ( 0.2624671916010504757, -0.5023911411419708095, -0.1820866141732282451 ) ) ;
#58847 = CONICAL_SURFACE ( 'NONE', #41369, 1.220472440944881942, 0.7853981633974621568 ) ;
#58846 = CARTESIAN_POINT ( 'NONE',  ( -0.8858267716535425107, -0.5400638737290844871, 0.3530559997133364547 ) ) ;
#58848 = CARTESIAN_POINT ( 'NONE',  ( -1.102362204724408601, -0.1870078740157480879, -0.4822834645669291653 ) ) ;
#58849 = CARTESIAN_POINT ( 'NONE',  ( -1.312335958005248715, 0.1283753931104748280, 0.1820866141732283561 ) ) ;
#58850 = CARTESIAN_POINT ( 'NONE',  ( -0.1742125984251974291, 0.1742125984251973736, -0.3937007874015748254 ) ) ;
#58851 = CARTESIAN_POINT ( 'NONE',  ( -0.7283464566929126471, -0.4536011799217367080, 0.2665933059059888421 ) ) ;
#58852 = DIRECTION ( 'NONE',  ( 1.000000000000000000, -0.000000000000000000, -0.000000000000000000 ) ) ;
#58853 = CARTESIAN_POINT ( 'NONE',  ( 1.220472440944882386, -0.6692913385826771977, 8.415575281601705876E-17 ) ) ;
#58854 = CARTESIAN_POINT ( 'NONE',  ( -0.1998031496062991907, -0.3460692066303959757, 0.09186351706036742504 ) ) ;
#58855 = CARTESIAN_POINT ( 'NONE',  ( 0.3917322834645670659, -0.1049643490035303273, -2.470491756726720833 ) ) ;
#58856 = ORIENTED_EDGE ( 'NONE', *, *, #73238, .F. ) ;
#58857 = FACE_OUTER_BOUND ( 'NONE', #67286, .T. ) ;
#58858 = CARTESIAN_POINT ( 'NONE',  ( -1.587926509186350810, -0.4281496062992124485, 0.4176697321401328655 ) ) ;
#58859 = CARTESIAN_POINT ( 'NONE',  ( -1.371391076115484831, 0.2952755905511810774, -0.1292274648535930714 ) ) ;
#58860 = EDGE_CURVE ( 'NONE', #59294, #70804, #82287, .T. ) ;
#58861 = CARTESIAN_POINT ( 'NONE',  ( 1.404199475065617264, -0.4281496062992124485, 0.4176697321401328655 ) ) ;
#58862 = CARTESIAN_POINT ( 'NONE',  ( 0.1049643490035303689, 0.3917322834645670104, -2.440288713910760521 ) ) ;
#58863 = LINE ( 'NONE', #20979, #60662 ) ;
#58864 = CARTESIAN_POINT ( 'NONE',  ( 0.4330708661417329575, 0.2952755905511811885, 0.000000000000000000 ) ) ;
#58865 = CARTESIAN_POINT ( 'NONE',  ( -0.3018372703412066094, -0.4281496062992127816, -0.4176697321401328100 ) ) ;
#58866 = CARTESIAN_POINT ( 'NONE',  ( 0.4585086550082259071, 1.414613662877127531, -3.910220139313873133 ) ) ;
#58867 = CARTESIAN_POINT ( 'NONE',  ( 0.06724401132815006898, 1.722984403643211298E-16, -0.3791483426435174331 ) ) ;
#58868 = CARTESIAN_POINT ( 'NONE',  ( 0.7283464566929140904, -0.4536011799217368745, -0.2665933059059886201 ) ) ;
#58869 = CARTESIAN_POINT ( 'NONE',  ( -0.1998031496062991907, -0.3460692066303959757, -1.167979002624671914 ) ) ;
#58870 = EDGE_LOOP ( 'NONE', ( #6821, #23576, #3734, #44060 ) ) ;
#58871 = CARTESIAN_POINT ( 'NONE',  ( 0.1958661417322836718, -0.3392501089628017219, 0.06887832201343642435 ) ) ;
#58872 = ORIENTED_EDGE ( 'NONE', *, *, #52742, .F. ) ;
#58873 = CARTESIAN_POINT ( 'NONE',  ( 0.1902887139107617975, 0.2952755905511811885, 0.1292274648535926551 ) ) ;
#58874 = CARTESIAN_POINT ( 'NONE',  ( 1.482939632545932307, 0.05413385826771626580, -0.4176697321401330321 ) ) ;
#58875 = CARTESIAN_POINT ( 'NONE',  ( 0.01968503937007957949, -0.5400638737290845981, -0.3530559997133363437 ) ) ;
#58876 = CARTESIAN_POINT ( 'NONE',  ( 1.371391076115485941, 0.2952755905511811885, 0.1292274648535926551 ) ) ;
#58877 = CARTESIAN_POINT ( 'NONE',  ( -0.4002624671916004129, -0.3162353388693405765, 0.4822834645669290543 ) ) ;
#58878 = CARTESIAN_POINT ( 'NONE',  ( -0.03280839895013062252, -0.6692913385826771977, 0.1292274648535927661 ) ) ;
#58879 = CARTESIAN_POINT ( 'NONE',  ( -1.653543307086613234, -0.1870078740157479769, 0.4822834645669291653 ) ) ;
#58880 = CARTESIAN_POINT ( 'NONE',  ( 1.358267716535433323, -0.5400638737290845981, -0.3530559997133363437 ) ) ;
#58881 = CARTESIAN_POINT ( 'NONE',  ( 1.069553805774278832, 0.2952755905511810774, -0.1292274648535930714 ) ) ;
#58882 = CARTESIAN_POINT ( 'NONE',  ( 0.3392501089628018884, -0.1958661417322834220, -0.2545931758530183275 ) ) ;
#58883 = CARTESIAN_POINT ( 'NONE',  ( 0.3937007874015754361, -0.1870078740157479769, 0.3641732283464567677 ) ) ;
#58884 = ORIENTED_EDGE ( 'NONE', *, *, #76145, .T. ) ;
#58885 = CARTESIAN_POINT ( 'NONE',  ( -0.1974969037888703871, -0.3420746716998661063, -0.5380577427821522374 ) ) ;
#58886 = ORIENTED_EDGE ( 'NONE', *, *, #46015, .F. ) ;
#58887 = CARTESIAN_POINT ( 'NONE',  ( -0.3543307086614165824, -0.5511811023622047445, 6.969142054262312111E-17 ) ) ;
#58888 = CARTESIAN_POINT ( 'NONE',  ( -0.02624671916010428221, 0.2306618581243847221, -0.2411417322834647770 ) ) ;
#58889 = CARTESIAN_POINT ( 'NONE',  ( 1.586052503253845281, 0.4724409448818907564, -0.1653254495020589354 ) ) ;
#58890 = CARTESIAN_POINT ( 'NONE',  ( 0.2427821522309716595, -0.3162353388693409650, -0.4822834645669289433 ) ) ;
#58891 = CARTESIAN_POINT ( 'NONE',  ( 0.04593175853018440641, 0.2952755905511810774, -0.1292274648535930714 ) ) ;
#58892 = CARTESIAN_POINT ( 'NONE',  ( -0.7742782152230962556, -0.4281496062992127816, -0.4176697321401328100 ) ) ;
#58893 = CARTESIAN_POINT ( 'NONE',  ( -0.8136482939632537770, -0.6046776061558807314, 0.2411417322834647770 ) ) ;
#58894 = CARTESIAN_POINT ( 'NONE',  ( 1.312335958005250269, -0.5023911411419708095, 0.1820866141732285504 ) ) ;
#58895 = CARTESIAN_POINT ( 'NONE',  ( -1.548556430446193399, -0.6046776061558809534, -0.2411417322834644161 ) ) ;
#58896 = CARTESIAN_POINT ( 'NONE',  ( -0.3025410870193214197, 0.000000000000000000, 0.3464511005275205946 ) ) ;
#58897 = CARTESIAN_POINT ( 'NONE',  ( 0.7939632545931766261, -0.08942795157527998196, 0.3641732283464567121 ) ) ;
#58898 = CARTESIAN_POINT ( 'NONE',  ( 0.5052493438320218022, -0.6692913385826773087, -0.1292274648535924053 ) ) ;
#58899 = CARTESIAN_POINT ( 'NONE',  ( 0.7611548556430454138, 0.2306618581243847221, -0.2411417322834647770 ) ) ;
#58900 = CARTESIAN_POINT ( 'NONE',  ( 0.1070741851644054915, -0.3996062992125986035, -1.187664041994750619 ) ) ;
#58901 = CARTESIAN_POINT ( 'NONE',  ( 0.4744094488188839720, 1.537401574803149984, 3.908320185825793658 ) ) ;
#58902 = CARTESIAN_POINT ( 'NONE',  ( 0.1998031496062992463, 0.3460692066303959202, -0.6935695538057742304 ) ) ;
#58903 = CARTESIAN_POINT ( 'NONE',  ( 0.1070741851644054776, -0.3996062992125984925, -0.004593175853018396058 ) ) ;
#58904 = CARTESIAN_POINT ( 'NONE',  ( -0.5249343832020990641, -0.6046776061558809534, -0.2411417322834644161 ) ) ;
#58905 = CARTESIAN_POINT ( 'NONE',  ( -0.3460692066303960868, 0.1998031496062990242, -2.703412073490813583 ) ) ;
#58906 = CARTESIAN_POINT ( 'NONE',  ( 0.1958661417322836440, -0.3392501089628017219, -2.223753280839895208 ) ) ;
#58907 = CARTESIAN_POINT ( 'NONE',  ( -1.167979002624671470, -0.004921259842519576551, 0.3153832671262227771 ) ) ;
#58908 = CARTESIAN_POINT ( 'NONE',  ( 1.266404199475066328, -0.05778040916215522460, 0.4822834645669289988 ) ) ;
#58909 = CONICAL_SURFACE ( 'NONE', #76394, 1.220472440944881942, 0.7853981633974621568 ) ;
#58910 = CARTESIAN_POINT ( 'NONE',  ( 0.8595800524934390507, -0.3162353388693405765, 0.4822834645669290543 ) ) ;
#58911 = CARTESIAN_POINT ( 'NONE',  ( -0.3674540682414689785, 0.1283753931104748280, 0.1820866141732283561 ) ) ;
#58912 = CARTESIAN_POINT ( 'NONE',  ( 0.5380577427821529035, 0.05413385826771626580, -0.4176697321401330321 ) ) ;
#58913 = CARTESIAN_POINT ( 'NONE',  ( 0.4091458600556404646, -0.2362204724409448231, -1.441601049868766582 ) ) ;
#58914 = CARTESIAN_POINT ( 'NONE',  ( 0.1968503937007881344, -0.5511811023622047445, 6.969142054262312111E-17 ) ) ;
#58915 = CARTESIAN_POINT ( 'NONE',  ( -0.07217847769028813698, -0.3162353388693409650, -0.4822834645669289433 ) ) ;
#58916 = CARTESIAN_POINT ( 'NONE',  ( 0.1974969037888704704, 0.3420746716998660508, -1.480971128608923548 ) ) ;
#58917 = CARTESIAN_POINT ( 'NONE',  ( -1.089238845144356427, 0.05413385826771666132, 0.4176697321401328100 ) ) ;
#58918 = CARTESIAN_POINT ( 'NONE',  ( 0.5839895013123367340, -0.5511811023622048555, -0.09757992244046775898 ) ) ;
#58919 = LINE ( 'NONE', #63978, #81020 ) ;
#58920 = CARTESIAN_POINT ( 'NONE',  ( -0.8070866141732276899, -0.5400638737290844871, 0.3530559997133364547 ) ) ;
#58921 = CARTESIAN_POINT ( 'NONE',  ( -0.4461942257217840213, -0.5023911411419708095, -0.1820866141732282451 ) ) ;
#58922 = CARTESIAN_POINT ( 'NONE',  ( 0.3503937007874015075, 0.3044824468161027586, -0.01968503937007903132 ) ) ;
#58923 = CARTESIAN_POINT ( 'NONE',  ( -0.7020997375328076329, -0.3162353388693409650, -0.4822834645669289433 ) ) ;
#58924 = CARTESIAN_POINT ( 'NONE',  ( -0.7874015748031489847, -0.1870078740157480879, -0.4822834645669291653 ) ) ;
#58925 = CARTESIAN_POINT ( 'NONE',  ( -0.1771653543307080136, 0.1660481256975883668, -0.3530559997133364547 ) ) ;
#58926 = CARTESIAN_POINT ( 'NONE',  ( -0.1998031496062991630, -0.3460692066303959202, -2.347112860892388575 ) ) ;
#58927 = CARTESIAN_POINT ( 'NONE',  ( -0.3917322834645669549, -7.196005306013483243E-17, -2.166647350884827183 ) ) ;
#58928 = CARTESIAN_POINT ( 'NONE',  ( -1.555118110236219930, 0.07958543189024085140, 0.2665933059059887866 ) ) ;
#58929 = CARTESIAN_POINT ( 'NONE',  ( 0.9186351706036752773, 0.1283753931104746893, -0.1820866141732285504 ) ) ;
#58930 = CARTESIAN_POINT ( 'NONE',  ( 1.456692913385827515, 0.2952755905511811885, 0.000000000000000000 ) ) ;
#58931 = CARTESIAN_POINT ( 'NONE',  ( -0.8923884514435688198, 0.1283753931104746893, -0.1820866141732285504 ) ) ;
#58932 = EDGE_CURVE ( 'NONE', #21240, #400, #42722, .T. ) ;
#58933 = CARTESIAN_POINT ( 'NONE',  ( -0.9842519685039365918, -0.5511811023622047445, 6.969142054262312111E-17 ) ) ;
#58934 = CARTESIAN_POINT ( 'NONE',  ( -0.7414698162729651543, -0.6692913385826771977, 0.1292274648535927661 ) ) ;
#58935 = CARTESIAN_POINT ( 'NONE',  ( -0.1968503937007867743, -0.6692913385826771977, 8.415575281601705876E-17 ) ) ;
#58936 = CARTESIAN_POINT ( 'NONE',  ( 0.6824146981627303710, -0.5023911411419708095, 0.1820866141732285504 ) ) ;
#58937 = DIRECTION ( 'NONE',  ( 1.047444401652940007E-14, -0.000000000000000000, -1.000000000000000000 ) ) ;
#58938 = CARTESIAN_POINT ( 'NONE',  ( 1.220472440944882386, -0.5511811023622047445, 6.969142054262312111E-17 ) ) ;
#58939 = ADVANCED_FACE ( 'NONE', ( #24605 ), #11170, .F. ) ;
#58940 = CARTESIAN_POINT ( 'NONE',  ( 0.3608923884514443348, -0.6692913385826771977, 0.1292274648535927661 ) ) ;
#58941 = CARTESIAN_POINT ( 'NONE',  ( -0.3460692066303960313, 0.1998031496062989965, 0.2119422572178477626 ) ) ;
#58942 = CARTESIAN_POINT ( 'NONE',  ( -0.7874015748031489847, -0.1870078740157479769, 0.4822834645669291653 ) ) ;
#58943 = CARTESIAN_POINT ( 'NONE',  ( 4.797336870675656522E-17, -0.3917322834645670104, -1.580708661417322913 ) ) ;
#58944 = CARTESIAN_POINT ( 'NONE',  ( 1.272965879265092637, -0.004921259842519576551, 0.3153832671262227771 ) ) ;
#58945 = CARTESIAN_POINT ( 'NONE',  ( 0.3477690288713918276, -0.6692913385826773087, -0.1292274648535924053 ) ) ;
#58946 = CARTESIAN_POINT ( 'NONE',  ( 0.02624671916010564918, -0.6046776061558809534, -0.2411417322834644161 ) ) ;
#58947 = CARTESIAN_POINT ( 'NONE',  ( 0.1246719160104994284, 0.1771653543307087075, -0.09757992244046823083 ) ) ;
#58948 = DIRECTION ( 'NONE',  ( -0.000000000000000000, -1.000000000000000000, -0.000000000000000000 ) ) ;
#58949 = CARTESIAN_POINT ( 'NONE',  ( 0.05905511811023709395, -0.4536011799217367080, 0.2665933059059888421 ) ) ;
#58950 = CARTESIAN_POINT ( 'NONE',  ( 0.9711286089238851948, -0.6046776061558809534, -0.2411417322834644161 ) ) ;
#58951 = CARTESIAN_POINT ( 'NONE',  ( -0.7545931758530177724, 0.1771653543307087630, 0.09757992244046791164 ) ) ;
#58952 = CARTESIAN_POINT ( 'NONE',  ( -0.5774278215223089816, -0.6046776061558807314, 0.2411417322834647770 ) ) ;
#58953 = CARTESIAN_POINT ( 'NONE',  ( 0.1706036745406830368, 0.009842519685039463617, 0.3409548833797002576 ) ) ;
#58954 = ORIENTED_EDGE ( 'NONE', *, *, #43837, .T. ) ;
#58955 = CARTESIAN_POINT ( 'NONE',  ( -1.089238845144356427, -0.4281496062992127816, -0.4176697321401328100 ) ) ;
#58956 = CARTESIAN_POINT ( 'NONE',  ( -1.056430446194224881, 0.1771653543307087075, -0.09757992244046823083 ) ) ;
#58957 = CARTESIAN_POINT ( 'NONE',  ( 0.07874015748031558404, -0.1870078740157480879, -0.4822834645669291653 ) ) ;
#58958 = EDGE_CURVE ( 'NONE', #69752, #29072, #44976, .T. ) ;
#58959 = CARTESIAN_POINT ( 'NONE',  ( -1.528871391076114250, 0.2952755905511810774, -0.1292274648535930714 ) ) ;
#58960 = CARTESIAN_POINT ( 'NONE',  ( -0.8858267716535425107, -0.5400638737290844871, 0.3530559997133364547 ) ) ;
#58961 = DIRECTION ( 'NONE',  ( 0.000000000000000000, 0.000000000000000000, -1.000000000000000000 ) ) ;
#58963 = CARTESIAN_POINT ( 'NONE',  ( 0.7545931758530188826, -0.6692913385826771977, 0.1292274648535927661 ) ) ;
#58962 = CARTESIAN_POINT ( 'NONE',  ( -0.9317585301837263412, 0.05413385826771666132, 0.4176697321401328100 ) ) ;
#58964 = CARTESIAN_POINT ( 'NONE',  ( 1.397637795275591177, 0.1660481256975883668, -0.3530559997133364547 ) ) ;
#58965 = CARTESIAN_POINT ( 'NONE',  ( 4.797336870675656522E-17, -0.3917322834645670104, -2.275590551181102317 ) ) ;
#58966 = CARTESIAN_POINT ( 'NONE',  ( 1.574803149606299746, -0.1870078740157479769, 0.4822834645669291653 ) ) ;
#58967 = CARTESIAN_POINT ( 'NONE',  ( -1.148293963254592542, -0.6692913385826773087, -0.1292274648535924053 ) ) ;
#58968 = CARTESIAN_POINT ( 'NONE',  ( -0.3458507752293906723, -0.3458507752293910609, -0.6889763779527556808 ) ) ;
#58969 = CARTESIAN_POINT ( 'NONE',  ( -0.3460692066303958092, -0.1998031496062994683, -0.2099737532808399199 ) ) ;
#58971 = EDGE_CURVE ( 'NONE', #12926, #48838, #2838, .T. ) ;
#58970 = ORIENTED_EDGE ( 'NONE', *, *, #47715, .F. ) ;
#58972 = CARTESIAN_POINT ( 'NONE',  ( -0.2559055118110227234, -0.4536011799217367080, 0.2665933059059888421 ) ) ;
#58973 = CARTESIAN_POINT ( 'NONE',  ( 0.3392501089628018884, -0.1958661417322834220, -1.829396325459317518 ) ) ;
#58974 = ORIENTED_EDGE ( 'NONE', *, *, #45936, .T. ) ;
#58975 = CARTESIAN_POINT ( 'NONE',  ( 0.3805774278215230400, 0.05413385826771626580, -0.4176697321401330321 ) ) ;
#58976 = CARTESIAN_POINT ( 'NONE',  ( -0.1509186351706028884, -0.05778040916215522460, 0.4822834645669289988 ) ) ;
#58977 = CARTESIAN_POINT ( 'NONE',  ( -0.5708661417322825615, -0.5400638737290844871, 0.3530559997133364547 ) ) ;
#58978 = CARTESIAN_POINT ( 'NONE',  ( -1.646051170424378096, -0.1870078740157480046, 1.254653134982923898E-17 ) ) ;
#58979 = CARTESIAN_POINT ( 'NONE',  ( -0.8858267716535425107, -0.4536011799217367080, 0.2665933059059888421 ) ) ;
#58980 = CARTESIAN_POINT ( 'NONE',  ( 0.4935044252197983150, 1.488513638086841118, -0.5309055118110237448 ) ) ;
#58981 = CARTESIAN_POINT ( 'NONE',  ( 0.9186351706036752773, 0.2306618581243847221, -0.2411417322834647770 ) ) ;
#58982 = CARTESIAN_POINT ( 'NONE',  ( 0.4527559055118117182, -0.4536011799217367080, 0.2665933059059888421 ) ) ;
#58983 = CARTESIAN_POINT ( 'NONE',  ( -0.4855643044619415427, 0.05413385826771626580, -0.4176697321401330321 ) ) ;
#58984 = CARTESIAN_POINT ( 'NONE',  ( 0.2867679344610365999, -0.2867679344610365999, -1.123340264270654698 ) ) ;
#58985 = CARTESIAN_POINT ( 'NONE',  ( -0.7349081364829387342, -0.6046776061558807314, 0.2411417322834647770 ) ) ;
#58986 = CARTESIAN_POINT ( 'NONE',  ( -1.561679790026246017, -0.004921259842519576551, 0.3153832671262227771 ) ) ;
#58987 = CARTESIAN_POINT ( 'NONE',  ( 1.154855643044620184, -0.6046776061558807314, 0.2411417322834647770 ) ) ;
#58988 = CARTESIAN_POINT ( 'NONE',  ( 1.489501312335958172, -0.2845877964562159024, 0.3641732283464567677 ) ) ;
#58989 = EDGE_LOOP ( 'NONE', ( #18746, #7867, #23974, #34029, #9014, #71838 ) ) ;
#58990 = CARTESIAN_POINT ( 'NONE',  ( -0.2867679344610367109, 0.2867679344610365444, -2.536108554626983480 ) ) ;
#58991 = CARTESIAN_POINT ( 'NONE',  ( 0.1115485564304470323, 0.2952755905511811885, 0.1292274648535926551 ) ) ;
#58992 = VERTEX_POINT ( 'NONE', #75563 ) ;
#58993 = CARTESIAN_POINT ( 'NONE',  ( -0.8858267716535425107, 0.1660481256975883668, -0.3530559997133364547 ) ) ;
#58994 = CARTESIAN_POINT ( 'NONE',  ( 1.437007874015748810, 0.1660481256975885056, 0.3530559997133364547 ) ) ;
#58995 = CARTESIAN_POINT ( 'NONE',  ( 1.187664041994751285, -0.3162353388693409650, -0.4822834645669289433 ) ) ;
#58996 = CARTESIAN_POINT ( 'NONE',  ( 0.3149606299212603933, -0.1870078740157479769, 0.4822834645669291653 ) ) ;
#58997 = CARTESIAN_POINT ( 'NONE',  ( -0.2821522309711278487, -0.6692913385826773087, -0.1292274648535924053 ) ) ;
#58998 = CARTESIAN_POINT ( 'NONE',  ( 0.3917322834645669549, 0.1049643490035304660, -1.784120734908136274 ) ) ;
#59000 = MANIFOLD_SOLID_BREP ( 'Chamfer1', #72927 ) ;
#58999 = CARTESIAN_POINT ( 'NONE',  ( -0.9908136482939626788, -0.6692913385826773087, -0.1292274648535924053 ) ) ;
#59001 = CARTESIAN_POINT ( 'NONE',  ( -0.7152230971128602510, -0.3162353388693405765, 0.4822834645669290543 ) ) ;
#59002 = CARTESIAN_POINT ( 'NONE',  ( 8.195543980992789655E-16, -0.1870078740157480601, -0.3641732283464567677 ) ) ;
#59003 = CARTESIAN_POINT ( 'NONE',  ( -0.4624320255261038515, -2.191421614605370878E-15, 0.4445507791589071167 ) ) ;
#59004 = CARTESIAN_POINT ( 'NONE',  ( -0.5446194225721777693, -0.3162353388693409650, -0.4822834645669289433 ) ) ;
#59005 = DIRECTION ( 'NONE',  ( 0.000000000000000000, 0.000000000000000000, 1.000000000000000000 ) ) ;
#59006 = CARTESIAN_POINT ( 'NONE',  ( 0.8727034120734912248, -0.3162353388693409650, -0.4822834645669289433 ) ) ;
#59007 = CARTESIAN_POINT ( 'NONE',  ( 3.910225209392130363, 1.414458570209803812, -0.4584652947720309069 ) ) ;
#59008 = VERTEX_POINT ( 'NONE', #56179 ) ;
#59009 = CARTESIAN_POINT ( 'NONE',  ( 8.195543980992789655E-16, -0.1870078740157480879, -0.4822834645669291653 ) ) ;
#59010 = CARTESIAN_POINT ( 'NONE',  ( -0.2821522309711278487, 0.1771653543307087630, 0.09757992244046791164 ) ) ;
#59012 = DIRECTION ( 'NONE',  ( 0.000000000000000000, 0.000000000000000000, 1.000000000000000000 ) ) ;
#59011 = CARTESIAN_POINT ( 'NONE',  ( 0.8858267716535438430, 0.07958543189024085140, 0.2665933059059887866 ) ) ;
#59013 = CARTESIAN_POINT ( 'NONE',  ( 0.3458507752293908943, 0.3458507752293908943, -0.05708661417322836301 ) ) ;
#59014 = DIRECTION ( 'NONE',  ( -1.000000000000000000, -0.000000000000000000, -0.000000000000000000 ) ) ;
#59015 = CARTESIAN_POINT ( 'NONE',  ( 1.364829396325459854, -0.6046776061558809534, -0.2411417322834644161 ) ) ;
#59016 = CARTESIAN_POINT ( 'NONE',  ( -0.2891555358219911054, 0.2891555358219909388, 0.06102362204724409017 ) ) ;
#59017 = CARTESIAN_POINT ( 'NONE',  ( 5.463695987328526437E-16, -0.1870078740157479769, 0.4822834645669291653 ) ) ;
#59018 = CARTESIAN_POINT ( 'NONE',  ( 0.000000000000000000, 0.7086614173228346081, 0.4527559055118110520 ) ) ;
#59019 = CARTESIAN_POINT ( 'NONE',  ( -1.535433070866141225, 0.2952755905511811885, 0.000000000000000000 ) ) ;
#59020 = CARTESIAN_POINT ( 'NONE',  ( -0.3543307086614165824, -0.6692913385826771977, 8.415575281601705876E-17 ) ) ;
#59021 = CARTESIAN_POINT ( 'NONE',  ( 0.1974969037888704704, 0.3420746716998660508, -0.2211286089238845842 ) ) ;
#59022 = CARTESIAN_POINT ( 'NONE',  ( -1.469816272965878357, 0.1283753931104748280, 0.1820866141732283561 ) ) ;
#59023 = CARTESIAN_POINT ( 'NONE',  ( 0.7152230971128614723, -0.3162353388693409650, -0.4822834645669289433 ) ) ;
#59024 = CARTESIAN_POINT ( 'NONE',  ( 1.017060367454068803, -0.2845877964562159024, 0.3641732283464567677 ) ) ;
#59025 = CARTESIAN_POINT ( 'NONE',  ( 0.3128291612561666657, 1.393967258436938472, 0.01053485884714776798 ) ) ;
#59026 = CARTESIAN_POINT ( 'NONE',  ( 0.5380577427821529035, -0.3690944881889763329, 0.3153832671262228327 ) ) ;
#59027 = CARTESIAN_POINT ( 'NONE',  ( -1.286089238845143479, 0.2306618581243847221, -0.2411417322834647770 ) ) ;
#59028 = CARTESIAN_POINT ( 'NONE',  ( -0.1998031496062994405, 0.3460692066303957537, -1.034776902887139194 ) ) ;
#59029 = CARTESIAN_POINT ( 'NONE',  ( 1.371391076115485941, 0.2952755905511811885, 0.1292274648535926551 ) ) ;
#59030 = CARTESIAN_POINT ( 'NONE',  ( -0.1958661417322834220, -0.3392501089628018884, -0.8451443569553805935 ) ) ;
#59032 = CARTESIAN_POINT ( 'NONE',  ( -0.7137454485294953965, 2.165354330708661124, -0.4917280318828585184 ) ) ;
#59031 = CARTESIAN_POINT ( 'NONE',  ( 0.8398950131233602345, -0.6046776061558807314, 0.2411417322834647770 ) ) ;
#59033 = CARTESIAN_POINT ( 'NONE',  ( -3.937007874015748143, 2.165354330708662012, -0.6299212598425202314 ) ) ;
#59034 = CARTESIAN_POINT ( 'NONE',  ( 0.5971128608923890191, -0.5511811023622046335, 0.09757992244046803654 ) ) ;
#59035 = ADVANCED_FACE ( 'NONE', ( #43540 ), #11587, .F. ) ;
#59036 = CARTESIAN_POINT ( 'NONE',  ( 0.5839895013123367340, 0.2952755905511811885, 0.1292274648535926551 ) ) ;
#59037 = CARTESIAN_POINT ( 'NONE',  ( -0.2642592750917004962, 0.1321325610835859254, 0.1571896754257856577 ) ) ;
#59038 = CARTESIAN_POINT ( 'NONE',  ( -0.9317585301837263412, -0.004921259842519576551, 0.3153832671262227771 ) ) ;
#59039 = CARTESIAN_POINT ( 'NONE',  ( -0.8727034120734901146, -0.05778040916215560624, -0.4822834645669293319 ) ) ;
#59040 = CARTESIAN_POINT ( 'NONE',  ( -1.482939632545930975, -0.4281496062992127816, -0.4176697321401328100 ) ) ;
#59041 = CARTESIAN_POINT ( 'NONE',  ( 1.115485564304462551, -0.4281496062992127816, -0.4176697321401328100 ) ) ;
#59042 = CARTESIAN_POINT ( 'NONE',  ( 1.456692913385827515, -0.6692913385826771977, 8.415575281601705876E-17 ) ) ;
#59043 = CARTESIAN_POINT ( 'NONE',  ( -0.3928700489057014855, 0.01966910102760518683, -1.220472440944881276 ) ) ;
#59044 = CARTESIAN_POINT ( 'NONE',  ( 0.5971128608923890191, -0.6692913385826771977, 0.1292274648535927661 ) ) ;
#59045 = CARTESIAN_POINT ( 'NONE',  ( 0.4724409448818898682, 2.892866454678787531E-17, -2.714566929133858331 ) ) ;
#59046 = CARTESIAN_POINT ( 'NONE',  ( 1.620734908136483465, -0.6692913385826771977, 0.1292274648535927661 ) ) ;
#59047 = CARTESIAN_POINT ( 'NONE',  ( 1.351706036745407680, 0.05413385826771666132, 0.4176697321401328100 ) ) ;
#59048 = CARTESIAN_POINT ( 'NONE',  ( -1.515748031496062076, 0.07958543189024071263, -0.2665933059059888421 ) ) ;
#59049 = CARTESIAN_POINT ( 'NONE',  ( 1.233595800524935227, 0.1283753931104746893, -0.1820866141732285504 ) ) ;
#59050 = CARTESIAN_POINT ( 'NONE',  ( -1.141732283464566011, 0.1771653543307087630, 0.000000000000000000 ) ) ;
#59051 = CARTESIAN_POINT ( 'NONE',  ( -0.5314960629921250401, 0.07958543189024085140, 0.2665933059059887866 ) ) ;
#59052 = CARTESIAN_POINT ( 'NONE',  ( 0.4606732211678793432, 1.929133858267716439, 0.5309055118110234117 ) ) ;
#59053 = CARTESIAN_POINT ( 'NONE',  ( 1.089238845144357537, -0.3690944881889763329, 0.3153832671262228327 ) ) ;
#59054 = CARTESIAN_POINT ( 'NONE',  ( 0.4658792650918641698, -0.05778040916215560624, -0.4822834645669293319 ) ) ;
#59055 = CARTESIAN_POINT ( 'NONE',  ( 1.233595800524935227, -0.6046776061558807314, 0.2411417322834647770 ) ) ;
#59056 = CARTESIAN_POINT ( 'NONE',  ( 0.04593175853018440641, -0.6692913385826771977, 0.1292274648535927661 ) ) ;
#59057 = CARTESIAN_POINT ( 'NONE',  ( 0.4593175853018379162, -0.3690944881889763329, 0.3153832671262228327 ) ) ;
#59058 = CARTESIAN_POINT ( 'NONE',  ( 1.430446194225722500, 0.05413385826771666132, 0.4176697321401328100 ) ) ;
#59059 = CARTESIAN_POINT ( 'NONE',  ( 0.000000000000000000, 2.755905511811024056, 0.000000000000000000 ) ) ;
#59060 = CARTESIAN_POINT ( 'NONE',  ( -0.3215223097112853146, -0.3162353388693405765, 0.4822834645669290543 ) ) ;
#59061 = CARTESIAN_POINT ( 'NONE',  ( -9.787531504996567848E-17, 0.3996062992125986035, -0.9448818897637796255 ) ) ;
#59062 = CARTESIAN_POINT ( 'NONE',  ( 0.03937007874015806264, 0.2066929133858268208, 0.000000000000000000 ) ) ;
#59063 = CARTESIAN_POINT ( 'NONE',  ( 0.1968503937007881344, 0.2952755905511811885, 0.000000000000000000 ) ) ;
#59064 = CARTESIAN_POINT ( 'NONE',  ( -0.7414698162729651543, -0.6692913385826771977, 0.1292274648535927661 ) ) ;
#59065 = CARTESIAN_POINT ( 'NONE',  ( -0.1509186351706028884, -0.05778040916215522460, 0.4822834645669289988 ) ) ;
#59066 = CARTESIAN_POINT ( 'NONE',  ( 0.1070741851644053527, 0.3996062992125986590, -2.828083989501312345 ) ) ;
#59067 = CARTESIAN_POINT ( 'NONE',  ( -0.1974969037888703871, -0.3420746716998661063, -1.797900262467191590 ) ) ;
#59068 = CARTESIAN_POINT ( 'NONE',  ( -0.3392501089628019995, 0.1958661417322832277, -0.3333333333333333148 ) ) ;
#59069 = CARTESIAN_POINT ( 'NONE',  ( 0.3392501089628018329, 0.1958661417322835607, -1.068241469816272771 ) ) ;
#59070 = CARTESIAN_POINT ( 'NONE',  ( -1.076115485564303809, 0.1283753931104748280, 0.1820866141732283561 ) ) ;
#59071 = CARTESIAN_POINT ( 'NONE',  ( 0.1958661417322834775, 0.3392501089628018884, -1.081364829396325389 ) ) ;
#59072 = CARTESIAN_POINT ( 'NONE',  ( -1.167979002624671470, -0.4281496062992127816, -0.4176697321401328100 ) ) ;
#59073 = CARTESIAN_POINT ( 'NONE',  ( -0.2891555358219909388, -0.2891555358219912164, -2.812992125984251857 ) ) ;
#59074 = CARTESIAN_POINT ( 'NONE',  ( 0.4790026246719168435, -0.3162353388693409650, -0.4822834645669289433 ) ) ;
#59075 = CARTESIAN_POINT ( 'NONE',  ( -0.4068241469816267775, -0.004921259842519870586, -0.3153832671262229437 ) ) ;
#59076 = CARTESIAN_POINT ( 'NONE',  ( 1.384514435695538337, -0.6692913385826771977, 0.1292274648535927661 ) ) ;
#59077 = CARTESIAN_POINT ( 'NONE',  ( 0.1574803149606306130, -0.1870078740157479769, 0.4822834645669291653 ) ) ;
#59078 = DIRECTION ( 'NONE',  ( -0.000000000000000000, -1.000000000000000000, -0.000000000000000000 ) ) ;
#59079 = CARTESIAN_POINT ( 'NONE',  ( -0.3996062992125986035, -7.340648628747425578E-17, -2.559055118110236560 ) ) ;
#59080 = CARTESIAN_POINT ( 'NONE',  ( -0.1049643490035307158, 0.3917322834645670104, -1.263142675361891731 ) ) ;
#59081 = CARTESIAN_POINT ( 'NONE',  ( 1.377952755905512472, 0.2952755905511811885, 0.000000000000000000 ) ) ;
#59082 = CARTESIAN_POINT ( 'NONE',  ( 0.5446194225721792126, -0.05778040916215560624, -0.4822834645669293319 ) ) ;
#59083 = CARTESIAN_POINT ( 'NONE',  ( 0.1574803149606306130, -0.1870078740157479769, 0.4822834645669291653 ) ) ;
#59084 = CARTESIAN_POINT ( 'NONE',  ( 1.417322834645670104, -0.1870078740157479769, 0.4822834645669291653 ) ) ;
#59085 = CARTESIAN_POINT ( 'NONE',  ( 1.003937007874016407, -0.5400638737290844871, 0.3530559997133364547 ) ) ;
#59086 = CARTESIAN_POINT ( 'NONE',  ( -0.2867679344610364334, -0.2867679344610367109, -0.6161417322834646937 ) ) ;
#59087 = CARTESIAN_POINT ( 'NONE',  ( 0.1706036745406830368, 0.05413385826771666132, 0.4176697321401328100 ) ) ;
#59088 = CARTESIAN_POINT ( 'NONE',  ( 1.167979002624672580, -0.4281496062992124485, 0.4176697321401328655 ) ) ;
#59089 = CARTESIAN_POINT ( 'NONE',  ( 0.3674540682414705883, -0.6046776061558807314, 0.2411417322834647770 ) ) ;
#59090 = CARTESIAN_POINT ( 'NONE',  ( 1.115485564304462551, -0.3690944881889765550, -0.3153832671262227771 ) ) ;
#59091 = CARTESIAN_POINT ( 'NONE',  ( -1.469816272965878357, -0.6046776061558809534, -0.2411417322834644161 ) ) ;
#59092 = CARTESIAN_POINT ( 'NONE',  ( -1.469816272965878357, -0.6046776061558809534, -0.2411417322834644161 ) ) ;
#59093 = CARTESIAN_POINT ( 'NONE',  ( 0.9580052493438326877, 0.05413385826771666132, 0.4176697321401328100 ) ) ;
#59094 = CARTESIAN_POINT ( 'NONE',  ( -0.06912221444153182626, -0.3857315817376797962, -1.929133858267716661 ) ) ;
#59095 = CARTESIAN_POINT ( 'NONE',  ( 0.2867679344610365999, -0.2867679344610365444, -2.137795275590551380 ) ) ;
#59096 = ORIENTED_EDGE ( 'NONE', *, *, #25809, .T. ) ;
#59097 = CARTESIAN_POINT ( 'NONE',  ( 0.1070741851644054915, -0.3996062992125986035, -0.2427821522309711877 ) ) ;
#59098 = VERTEX_POINT ( 'NONE', #30920 ) ;
#59099 = CARTESIAN_POINT ( 'NONE',  ( 1.348312163386739426, 0.2755905511811023723, 0.7386866130305692613 ) ) ;
#59100 = CARTESIAN_POINT ( 'NONE',  ( 0.8070866141732288002, 0.07958543189024085140, 0.2665933059059887866 ) ) ;
#59101 = DIRECTION ( 'NONE',  ( -1.000000000000000000, -0.000000000000000000, -0.000000000000000000 ) ) ;
#59102 = CARTESIAN_POINT ( 'NONE',  ( -0.4257672537616706832, 1.326168777627700246, 2.647052616966094618 ) ) ;
#59103 = CARTESIAN_POINT ( 'NONE',  ( -2.362204724409448620, 1.724409448818897905, -2.474278114140802984E-14 ) ) ;
#59104 = CARTESIAN_POINT ( 'NONE',  ( 0.3917322834645670104, 2.398668435337828261E-17, -0.9901574803149607584 ) ) ;
#59105 = CARTESIAN_POINT ( 'NONE',  ( 1.187664041994751285, -0.3162353388693409650, -0.4822834645669289433 ) ) ;
#59106 = CARTESIAN_POINT ( 'NONE',  ( -1.502624671916009680, -0.3162353388693405765, 0.4822834645669290543 ) ) ;
#59107 = CARTESIAN_POINT ( 'NONE',  ( -0.2099737532808391705, -0.6046776061558809534, -0.2411417322834644161 ) ) ;
#59108 = CARTESIAN_POINT ( 'NONE',  ( 0.9776902887139113929, 0.2952755905511811885, 0.1292274648535926551 ) ) ;
#59109 = ORIENTED_EDGE ( 'NONE', *, *, #30503, .T. ) ;
#59110 = CARTESIAN_POINT ( 'NONE',  ( -1.614173228346456268, -0.6692913385826771977, 8.415575281601705876E-17 ) ) ;
#59111 = CARTESIAN_POINT ( 'NONE',  ( -1.047434348705044815, 1.285715225710756249, -0.4024367083785531651 ) ) ;
#59112 = APPLICATION_PROTOCOL_DEFINITION ( 'draft international standard', 'automotive_design', 1998, #48197 ) ;
#59113 = CARTESIAN_POINT ( 'NONE',  ( -3.937007874015748143, 2.559055118110236560, -0.3149606299212599492 ) ) ;
#59114 = CARTESIAN_POINT ( 'NONE',  ( 0.000000000000000000, 0.07874015748031502893, 3.858267716535433323 ) ) ;
#59115 = CARTESIAN_POINT ( 'NONE',  ( -1.003937007874014853, 0.07958543189024085140, 0.2665933059059887866 ) ) ;
#59116 = ADVANCED_FACE ( 'NONE', ( #56586 ), #75971, .F. ) ;
#59117 = CARTESIAN_POINT ( 'NONE',  ( 0.8923884514435701520, 0.1539470093639523085, 0.1968503937007873850 ) ) ;
#59118 = CARTESIAN_POINT ( 'NONE',  ( 0.6233595800524942554, -0.05778040916215560624, -0.4822834645669293319 ) ) ;
#59119 = EDGE_LOOP ( 'NONE', ( #58036, #30186, #74119, #13762 ) ) ;
#59121 = CARTESIAN_POINT ( 'NONE',  ( -0.4596682205436332658, 0.004960608223778823628, 0.3437734562760190182 ) ) ;
#59120 = CARTESIAN_POINT ( 'NONE',  ( -0.5314960629921194890, 2.742776589625216754, -1.881759000869286158 ) ) ;
#59122 = CARTESIAN_POINT ( 'NONE',  ( 0.7020997375328090762, -0.3162353388693405765, 0.4822834645669290543 ) ) ;
#59123 = CARTESIAN_POINT ( 'NONE',  ( -1.594488188976377563, -0.5400638737290844871, 0.3530559997133364547 ) ) ;
#59124 = CARTESIAN_POINT ( 'NONE',  ( 0.3392501089628018329, -0.1958661417322834497, -0.9724216291000506995 ) ) ;
#59125 = CARTESIAN_POINT ( 'NONE',  ( -0.7020997375328076329, -0.2845877964562161244, -0.3641732283464567121 ) ) ;
#59126 = CARTESIAN_POINT ( 'NONE',  ( 1.660104986876641320, -0.05778040916215522460, 0.4822834645669289988 ) ) ;
#59127 = CARTESIAN_POINT ( 'NONE',  ( -0.1958661417322836718, 0.3392501089628017219, -1.200131233595800540 ) ) ;
#59128 = CARTESIAN_POINT ( 'NONE',  ( 0.6430446194225728496, 0.05413385826771666132, 0.4176697321401328100 ) ) ;
#59129 = CARTESIAN_POINT ( 'NONE',  ( -1.076115485564303809, -0.5023911411419708095, -0.1820866141732282451 ) ) ;
#59130 = CARTESIAN_POINT ( 'NONE',  ( 0.1837270341207354329, 0.1283753931104748280, 0.1820866141732283561 ) ) ;
#59131 = CARTESIAN_POINT ( 'NONE',  ( -0.3280839895013117347, -0.4281496062992124485, 0.4176697321401328655 ) ) ;
#59132 = CARTESIAN_POINT ( 'NONE',  ( -1.010498687664041384, -0.004921259842519576551, 0.3153832671262227771 ) ) ;
#59133 = CARTESIAN_POINT ( 'NONE',  ( 0.3917322834645670659, 2.398668435337828261E-17, 0.04263160285333144478 ) ) ;
#59134 = CARTESIAN_POINT ( 'NONE',  ( 0.6167979002624678353, -0.4281496062992124485, 0.4176697321401328655 ) ) ;
#59135 = B_SPLINE_CURVE_WITH_KNOTS ( 'NONE', 3,
 ( #65167, #46199, #71473, #13821 ),
 .UNSPECIFIED., .F., .F.,
 ( 4, 4 ),
 ( 0.09524935589747281217, 0.09667867193306639573 ),
 .UNSPECIFIED. ) ;
#59136 = CARTESIAN_POINT ( 'NONE',  ( -1.469816272965878357, 0.2306618581243848609, 0.2411417322834645549 ) ) ;
#59137 = CARTESIAN_POINT ( 'NONE',  ( -0.3458507752293909498, 0.3458507752293907833, -1.513779527559054872 ) ) ;
#59138 = CARTESIAN_POINT ( 'NONE',  ( -0.7545931758530177724, 0.2952755905511811885, 0.1292274648535926551 ) ) ;
#59139 = CARTESIAN_POINT ( 'NONE',  ( -0.01968503937007793844, -0.4536011799217367080, 0.2665933059059888421 ) ) ;
#59140 = CARTESIAN_POINT ( 'NONE',  ( -1.220472440944881054, -0.6692913385826771977, 8.415575281601705876E-17 ) ) ;
#59141 = CARTESIAN_POINT ( 'NONE',  ( 0.8727034120734913358, -0.08942795157527998196, 0.3641732283464567121 ) ) ;
#59142 = CARTESIAN_POINT ( 'NONE',  ( -0.9055118110236215490, 0.1771653543307087630, 0.000000000000000000 ) ) ;
#59143 = CARTESIAN_POINT ( 'NONE',  ( -1.036745406824146176, 0.05413385826771626580, -0.4176697321401330321 ) ) ;
#59145 = B_SPLINE_CURVE_WITH_KNOTS ( 'NONE', 3,
 ( #20844, #72195, #14550, #33884 ),
 .UNSPECIFIED., .F., .F.,
 ( 4, 4 ),
 ( 0.1307222445546318834, 0.1321409493595271933 ),
 .UNSPECIFIED. ) ;
#59144 = CARTESIAN_POINT ( 'NONE',  ( -1.049868766404198794, 0.2306618581243847221, -0.2411417322834647770 ) ) ;
#59146 = CARTESIAN_POINT ( 'NONE',  ( -1.430446194225720724, 0.05413385826771626580, -0.4176697321401330321 ) ) ;
#59147 = CARTESIAN_POINT ( 'NONE',  ( 0.2362204724409449064, 0.4091458600556404646, -2.110892388451443225 ) ) ;
#59148 = CARTESIAN_POINT ( 'NONE',  ( 0.8727034120734913358, -0.08942795157527998196, 0.3641732283464567121 ) ) ;
#59149 = CARTESIAN_POINT ( 'NONE',  ( 0.5446194225721792126, -0.3162353388693405765, 0.4822834645669290543 ) ) ;
#59150 = CARTESIAN_POINT ( 'NONE',  ( -1.345144356955379816, -0.3162353388693405765, 0.4822834645669290543 ) ) ;
#59151 = CARTESIAN_POINT ( 'NONE',  ( -1.581364829396324945, -0.3162353388693405765, 0.4822834645669290543 ) ) ;
#59152 = ORIENTED_EDGE ( 'NONE', *, *, #23233, .F. ) ;
#59153 = CARTESIAN_POINT ( 'NONE',  ( -0.3460692066303960313, 0.1998031496062989965, -2.780183727034120977 ) ) ;
#59154 = CARTESIAN_POINT ( 'NONE',  ( -1.397637795275589623, -0.4536011799217368745, -0.2665933059059886201 ) ) ;
#59155 = CARTESIAN_POINT ( 'NONE',  ( 0.5446194225721792126, -0.05778040916215560624, -0.4822834645669293319 ) ) ;
#59156 = CARTESIAN_POINT ( 'NONE',  ( -1.430446194225721390, -0.3690944881889763329, 0.3153832671262228327 ) ) ;
#59157 = CARTESIAN_POINT ( 'NONE',  ( 0.3996062992125984925, 0.1070741851644054637, -1.776246719160104570 ) ) ;
#59158 = CARTESIAN_POINT ( 'NONE',  ( -1.581364829396324945, -0.3162353388693405765, 0.4822834645669290543 ) ) ;
#59159 = CARTESIAN_POINT ( 'NONE',  ( 0.8070866141732289112, -0.5400638737290845981, -0.3530559997133363437 ) ) ;
#59160 = CARTESIAN_POINT ( 'NONE',  ( 0.6561679790026253567, -0.6046776061558809534, -0.2411417322834644161 ) ) ;
#59161 = CARTESIAN_POINT ( 'NONE',  ( 1.128608923884514947, 0.2306618581243848609, 0.2411417322834645549 ) ) ;
#59162 = CARTESIAN_POINT ( 'NONE',  ( -0.2925321140481932369, 0.2925321140481930704, -0.8838582677165351953 ) ) ;
#59163 = CARTESIAN_POINT ( 'NONE',  ( -0.3996062992125986035, -0.1070741851644056997, -1.463254593175853158 ) ) ;
#59164 = CARTESIAN_POINT ( 'NONE',  ( -0.3949938075777411628, 0.1058382717557497937, -0.5052493438320211361 ) ) ;
#59165 = CARTESIAN_POINT ( 'NONE',  ( 0.4102808022082901629, 1.299212598425196985, -1.736178228450289573 ) ) ;
#59166 = CARTESIAN_POINT ( 'NONE',  ( 0.1377952755905518800, -0.4536011799217367080, 0.2665933059059888421 ) ) ;
#59167 = CARTESIAN_POINT ( 'NONE',  ( 0.2624671916010504757, -0.6046776061558809534, -0.2411417322834644161 ) ) ;
#59168 = CARTESIAN_POINT ( 'NONE',  ( 1.227034120734908917, -0.6692913385826771977, 0.1292274648535927661 ) ) ;
#59169 = CARTESIAN_POINT ( 'NONE',  ( 0.1058382717557499880, 0.3949938075777409408, -1.802493438320210251 ) ) ;
#59170 = CARTESIAN_POINT ( 'NONE',  ( 0.1837270341207357105, -0.5023911411419708095, -0.1820866141732282451 ) ) ;
#59171 = CARTESIAN_POINT ( 'NONE',  ( -0.7611548556430438595, -0.6046776061558809534, -0.2411417322834644161 ) ) ;
#59172 = CARTESIAN_POINT ( 'NONE',  ( 1.581364829396326277, -0.05778040916215522460, 0.4822834645669289988 ) ) ;
#59173 = CARTESIAN_POINT ( 'NONE',  ( 0.3608923884514443348, -0.6692913385826771977, 0.1292274648535927661 ) ) ;
#59174 = CARTESIAN_POINT ( 'NONE',  ( 0.2362204724409451007, -0.4091458600556402980, -1.981627296587926690 ) ) ;
#59175 = LINE ( 'NONE', #39826, #82880 ) ;
#59176 = ORIENTED_EDGE ( 'NONE', *, *, #8974, .T. ) ;
#59177 = ORIENTED_EDGE ( 'NONE', *, *, #56716, .F. ) ;
#59178 = CARTESIAN_POINT ( 'NONE',  ( -1.660104986876639543, -0.05778040916215560624, -0.4822834645669293319 ) ) ;
#59179 = AXIS2_PLACEMENT_3D ( 'NONE', #22392, #72908, #16089 ) ;
#59181 = CARTESIAN_POINT ( 'NONE',  ( -1.135170603674539924, 0.2952755905511810774, -0.1292274648535930714 ) ) ;
#59180 = CARTESIAN_POINT ( 'NONE',  ( -1.253280839895012377, -0.2845877964562161244, -0.3641732283464567121 ) ) ;
#59182 = CARTESIAN_POINT ( 'NONE',  ( 0.3392501089628018329, 0.1958661417322835052, -2.415991182905824708 ) ) ;
#59183 = CARTESIAN_POINT ( 'NONE',  ( -0.2925321140481932369, 0.2925321140481931259, -2.773622047244094002 ) ) ;
#59184 = CARTESIAN_POINT ( 'NONE',  ( 1.515748031496063408, 0.1660481256975885056, 0.3530559997133364547 ) ) ;
#59185 = CARTESIAN_POINT ( 'NONE',  ( -1.181102362204723644, -0.1870078740157480879, -0.4822834645669291653 ) ) ;
#59186 = CARTESIAN_POINT ( 'NONE',  ( 0.4396325459317590445, -0.6692913385826771977, 0.1292274648535927661 ) ) ;
#59187 = CARTESIAN_POINT ( 'NONE',  ( -1.430446194225720724, 0.05413385826771626580, -0.4176697321401330321 ) ) ;
#59188 = CARTESIAN_POINT ( 'NONE',  ( 4.797336870675656522E-17, -0.3917322834645670104, 0.1515748031496061965 ) ) ;
#59189 = CARTESIAN_POINT ( 'NONE',  ( 0.7020997375328090762, -0.05778040916215560624, -0.4822834645669293319 ) ) ;
#59190 = CARTESIAN_POINT ( 'NONE',  ( 0.3917322834645670104, -0.1049643490035303411, -1.835958005249343827 ) ) ;
#59191 = CARTESIAN_POINT ( 'NONE',  ( -1.200787401574802349, -0.4536011799217367080, 0.2665933059059888421 ) ) ;
#59192 = ORIENTED_EDGE ( 'NONE', *, *, #48124, .T. ) ;
#59193 = CARTESIAN_POINT ( 'NONE',  ( 0.1974969037888704704, 0.3420746716998660508, -1.876640419947506633 ) ) ;
#59194 = ORIENTED_EDGE ( 'NONE', *, *, #79456, .F. ) ;
#59195 = CARTESIAN_POINT ( 'NONE',  ( -1.528871391076114250, 0.1771653543307087075, -0.09757992244046823083 ) ) ;
#59196 = CARTESIAN_POINT ( 'NONE',  ( -1.049868766404198794, 0.2306618581243847221, -0.2411417322834647770 ) ) ;
#59197 = CARTESIAN_POINT ( 'NONE',  ( -1.102362204724408601, -0.1870078740157480879, -0.4822834645669291653 ) ) ;
#59198 = CARTESIAN_POINT ( 'NONE',  ( -0.1998031496062994683, 0.3460692066303958092, -0.4855643044619422644 ) ) ;
#59199 = CARTESIAN_POINT ( 'NONE',  ( -1.555118110236219930, 0.1660481256975885056, 0.3530559997133364547 ) ) ;
#59200 = CARTESIAN_POINT ( 'NONE',  ( -1.686351706036744558, 0.2952755905511810774, -0.1292274648535930714 ) ) ;
#59201 = CARTESIAN_POINT ( 'NONE',  ( -1.246719160104985846, -0.4281496062992127816, -0.4176697321401328100 ) ) ;
#59202 = DIRECTION ( 'NONE',  ( -1.000000000000000000, -0.000000000000000000, -0.000000000000000000 ) ) ;
#59203 = CARTESIAN_POINT ( 'NONE',  ( 0.1574803149606306130, -0.1870078740157480601, -0.3641732283464567677 ) ) ;
#59204 = DIRECTION ( 'NONE',  ( -1.000000000000000000, -3.083952846180989294E-16, 0.000000000000000000 ) ) ;
#59205 = CARTESIAN_POINT ( 'NONE',  ( -0.1049643490035302024, -0.3917322834645671215, -0.4717847769028871152 ) ) ;
#59206 = CARTESIAN_POINT ( 'NONE',  ( -0.5249343832020990641, -0.5023911411419708095, -0.1820866141732282451 ) ) ;
#59207 = CARTESIAN_POINT ( 'NONE',  ( -0.5839895013123351797, -0.6692913385826771977, 0.1292274648535927661 ) ) ;
#59208 = CARTESIAN_POINT ( 'NONE',  ( 1.030183727034121421, -0.3162353388693409650, -0.4822834645669289433 ) ) ;
#59209 = CARTESIAN_POINT ( 'NONE',  ( -0.8005249343832011588, 0.05413385826771626580, -0.4176697321401330321 ) ) ;
#59210 = ORIENTED_EDGE ( 'NONE', *, *, #18560, .F. ) ;
#59211 = ORIENTED_EDGE ( 'NONE', *, *, #76734, .T. ) ;
#59212 = CARTESIAN_POINT ( 'NONE',  ( -0.9251968503937002541, -0.5400638737290845981, -0.3530559997133363437 ) ) ;
#59213 = CARTESIAN_POINT ( 'NONE',  ( 0.6955380577427828781, 0.05413385826771626580, -0.4176697321401330321 ) ) ;
#59214 = CARTESIAN_POINT ( 'NONE',  ( -1.391076115485563758, 0.1283753931104748280, 0.1820866141732283561 ) ) ;
#59215 = CARTESIAN_POINT ( 'NONE',  ( 5.785732909357575061E-17, -0.4724409448818898682, -1.181102362204724310 ) ) ;
#59216 = DIRECTION ( 'NONE',  ( -3.096699300667737957E-16, 1.000000000000000000, -0.000000000000000000 ) ) ;
#59217 = ADVANCED_FACE ( 'NONE', ( #63324 ), #26693, .T. ) ;
#59218 = CARTESIAN_POINT ( 'NONE',  ( -0.3917322834645671215, 0.1049643490035301469, -0.3398950131233596239 ) ) ;
#59219 = CARTESIAN_POINT ( 'NONE',  ( 0.3392501089628018329, 0.1958661417322835607, -2.420603674540682260 ) ) ;
#59220 = CARTESIAN_POINT ( 'NONE',  ( -0.1181102362204717315, -0.6692913385826771977, 8.415575281601705876E-17 ) ) ;
#59221 = CARTESIAN_POINT ( 'NONE',  ( -1.358267716535432434, -0.4536011799217367080, 0.2665933059059888421 ) ) ;
#59222 = CARTESIAN_POINT ( 'NONE',  ( 0.1998031496062994128, -0.3460692066303957537, -0.1686351706036745557 ) ) ;
#59224 = CARTESIAN_POINT ( 'NONE',  ( 0.1938976377952755792, 0.1938976377952755792, 0.07874015748031495954 ) ) ;
#59223 = CARTESIAN_POINT ( 'NONE',  ( -1.476377952755905110, -0.5400638737290845981, -0.3530559997133363437 ) ) ;
#59225 = CARTESIAN_POINT ( 'NONE',  ( -1.450131233595799651, -0.6692913385826771977, 0.1292274648535927661 ) ) ;
#59226 = CARTESIAN_POINT ( 'NONE',  ( -0.4724409448818890911, -0.1870078740157479769, 0.4822834645669291653 ) ) ;
#59227 = CARTESIAN_POINT ( 'NONE',  ( 0.2891555358219910499, -0.2891555358219909944, -2.537401574803150428 ) ) ;
#59228 = CARTESIAN_POINT ( 'NONE',  ( 0.2493438320209980519, -0.3690944881889765550, -0.3153832671262227771 ) ) ;
#59229 = CARTESIAN_POINT ( 'NONE',  ( 0.1958661417322836440, -0.3392501089628017219, -0.01902887139107619849 ) ) ;
#59230 = CARTESIAN_POINT ( 'NONE',  ( 0.2362204724409456558, -0.1870078740157479769, 0.3641732283464567677 ) ) ;
#59231 = CARTESIAN_POINT ( 'NONE',  ( 1.167979002624672580, -0.004921259842519870586, -0.3153832671262229437 ) ) ;
#59232 = CARTESIAN_POINT ( 'NONE',  ( 0.7808398950131240079, -0.3162353388693405765, 0.4822834645669290543 ) ) ;
#59233 = CARTESIAN_POINT ( 'NONE',  ( 0.2099737532808405305, -0.5023911411419708095, 0.1820866141732285504 ) ) ;
#59234 = CARTESIAN_POINT ( 'NONE',  ( 0.3392501089628018329, 0.1958661417322835607, -1.855643044619422533 ) ) ;
#59235 = CARTESIAN_POINT ( 'NONE',  ( -1.469816272965878357, 0.2306618581243848609, 0.2411417322834645549 ) ) ;
#59236 = CARTESIAN_POINT ( 'NONE',  ( 0.02624671916010564918, 0.1283753931104748280, 0.1820866141732283561 ) ) ;
#59237 =( BOUNDED_CURVE ( )  B_SPLINE_CURVE ( 2, ( #55884, #49577, #31042, #57117, #5381, #44079, #43247, #68945, #4975, #62631, #37372, #24728, #12116 ),
 .UNSPECIFIED., .F., .F. ) 
 B_SPLINE_CURVE_WITH_KNOTS ( ( 3, 2, 2, 2, 2, 2, 3 ),
 ( 0.7194878114796872115, 0.7196969696969697239, 0.7234848484848485084, 0.7272727272727272929, 0.7310606060606060774, 0.7348484848484848619, 0.7350576430657673743 ),
 .UNSPECIFIED. ) 
 CURVE ( )  GEOMETRIC_REPRESENTATION_ITEM ( )  RATIONAL_B_SPLINE_CURVE ( ( 0.9964447847208419695, 0.9981185001348091834, 1.000000000000000000, 0.9659258262890683122, 1.000000000000000000, 0.9659258262890683122, 1.000000000000000000, 0.9659258262890683122, 1.000000000000000000, 0.9659258262890683122, 1.000000000000000000, 0.9981185001348091834, 0.9964447847208420805 ) ) 
 REPRESENTATION_ITEM ( '' )  );
#59238 = DIRECTION ( 'NONE',  ( -0.000000000000000000, -1.000000000000000000, -0.000000000000000000 ) ) ;
#59239 = CARTESIAN_POINT ( 'NONE',  ( -0.3280839895013117347, -0.004921259842519870586, -0.3153832671262229437 ) ) ;
#59240 = CARTESIAN_POINT ( 'NONE',  ( -0.4359958488159683676, 1.724409448818897905, -1.033875059083678272 ) ) ;
#59241 = CARTESIAN_POINT ( 'NONE',  ( 0.07874015748031558404, -0.1870078740157479769, 0.4822834645669291653 ) ) ;
#59242 = DIRECTION ( 'NONE',  ( -0.000000000000000000, 0.000000000000000000, -1.000000000000000000 ) ) ;
#59243 = CARTESIAN_POINT ( 'NONE',  ( 1.154855643044620184, 0.1283753931104746893, -0.1820866141732285504 ) ) ;
#59244 = CARTESIAN_POINT ( 'NONE',  ( -0.2952755905511804668, 0.07958543189024085140, 0.2665933059059887866 ) ) ;
#59245 = CARTESIAN_POINT ( 'NONE',  ( -0.3608923884514428360, 0.2952755905511811885, 0.1292274648535926551 ) ) ;
#59246 = CARTESIAN_POINT ( 'NONE',  ( -1.666666666666665853, 0.05413385826771626580, -0.4176697321401330321 ) ) ;
#59247 = CARTESIAN_POINT ( 'NONE',  ( -1.299212598425196097, 0.1771653543307087630, 0.000000000000000000 ) ) ;
#59248 = CARTESIAN_POINT ( 'NONE',  ( -2.795275590551181910, 1.850393700787402729, -6.635626899597537341E-17 ) ) ;
#59249 = EDGE_CURVE ( 'NONE', #51988, #29367, #75107, .T. ) ;
#59250 = CARTESIAN_POINT ( 'NONE',  ( 0.7020997375328090762, -0.3162353388693405765, 0.4822834645669290543 ) ) ;
#59251 = VECTOR ( 'NONE', #25128, 39.37007874015748143 ) ;
#59252 = CARTESIAN_POINT ( 'NONE',  ( -0.8070866141732276899, 0.1660481256975883668, -0.3530559997133364547 ) ) ;
#59253 = CARTESIAN_POINT ( 'NONE',  ( 0.1070741851644054776, -0.3996062992125984925, -1.106955380577427706 ) ) ;
#59254 = CARTESIAN_POINT ( 'NONE',  ( -0.1049643490035307020, 0.3917322834645669549, -2.768372703412072866 ) ) ;
#59255 = CARTESIAN_POINT ( 'NONE',  ( 0.3543307086614179147, 0.1771653543307087630, 0.000000000000000000 ) ) ;
#59256 = CARTESIAN_POINT ( 'NONE',  ( -0.9776902887139098386, 0.2952755905511810774, -0.1292274648535930714 ) ) ;
#59257 = CARTESIAN_POINT ( 'NONE',  ( -1.259842519685038686, -0.1870078740157480879, -0.4822834645669291653 ) ) ;
#59258 = CARTESIAN_POINT ( 'NONE',  ( -1.437007874015747477, 0.07958543189024071263, -0.2665933059059888421 ) ) ;
#59259 = FACE_OUTER_BOUND ( 'NONE', #50719, .T. ) ;
#59260 = CARTESIAN_POINT ( 'NONE',  ( -0.7086614173228339419, -0.1870078740157479769, 0.3641732283464567677 ) ) ;
#59261 = CARTESIAN_POINT ( 'NONE',  ( 0.4677827689124922084, 0.03937007874015747977, 2.154527559055118946 ) ) ;
#59262 = CARTESIAN_POINT ( 'NONE',  ( 0.6824146981627303710, 0.2306618581243847221, -0.2411417322834647770 ) ) ;
#59263 = CARTESIAN_POINT ( 'NONE',  ( -0.2925321140481930704, -0.2925321140481933480, -0.2165354330708661734 ) ) ;
#59264 = CARTESIAN_POINT ( 'NONE',  ( -0.1049643490035307158, 0.3917322834645670104, -2.680465510007561836 ) ) ;
#59265 = CARTESIAN_POINT ( 'NONE',  ( 0.4732023222440338017, 1.572318554836809046, -2.557221887108173775 ) ) ;
#59266 = CARTESIAN_POINT ( 'NONE',  ( -1.633858267716534529, -0.5400638737290845981, -0.3530559997133363437 ) ) ;
#59267 = CARTESIAN_POINT ( 'NONE',  ( -1.194225721784776262, 0.05413385826771626580, -0.4176697321401330321 ) ) ;
#59268 = CARTESIAN_POINT ( 'NONE',  ( 1.115485564304462551, 0.05413385826771666132, 0.4176697321401328100 ) ) ;
#59269 = CARTESIAN_POINT ( 'NONE',  ( -0.2867679344610364334, -0.2867679344610367109, -2.505905511811023612 ) ) ;
#59270 = DIRECTION ( 'NONE',  ( -2.664535259100375697E-15, 9.738798461624180871E-16, 1.000000000000000000 ) ) ;
#59271 = EDGE_CURVE ( 'NONE', #17299, #23493, #67087, .T. ) ;
#59272 = CARTESIAN_POINT ( 'NONE',  ( 0.4396325459317593221, 0.2952755905511810774, -0.1292274648535930714 ) ) ;
#59273 = CARTESIAN_POINT ( 'NONE',  ( -0.3937007874015740483, -0.1870078740157479769, 0.4822834645669291653 ) ) ;
#59274 = DIRECTION ( 'NONE',  ( -0.000000000000000000, -1.000000000000000000, -0.000000000000000000 ) ) ;
#59275 = CARTESIAN_POINT ( 'NONE',  ( -0.1070741851644057135, 0.3996062992125985480, -2.053805774278214979 ) ) ;
#59276 = CARTESIAN_POINT ( 'NONE',  ( 0.6102362204724416372, -0.4536011799217367080, 0.2665933059059888421 ) ) ;
#59277 = CARTESIAN_POINT ( 'NONE',  ( -0.1998031496062994683, 0.3460692066303958092, -1.745406824146981561 ) ) ;
#59278 = ORIENTED_EDGE ( 'NONE', *, *, #890, .T. ) ;
#59279 = CARTESIAN_POINT ( 'NONE',  ( -0.2867679344610367109, 0.2867679344610365444, -0.4888644601387945876 ) ) ;
#59280 = ORIENTED_EDGE ( 'NONE', *, *, #13561, .T. ) ;
#59281 = CARTESIAN_POINT ( 'NONE',  ( 0.09842519685039434474, -0.5400638737290845981, -0.3530559997133363437 ) ) ;
#59282 = CARTESIAN_POINT ( 'NONE',  ( 1.476377952755906220, 0.1660481256975883668, -0.3530559997133364547 ) ) ;
#59283 = CARTESIAN_POINT ( 'NONE',  ( 0.2559055118110243332, 0.1660481256975885056, 0.3530559997133364547 ) ) ;
#59284 = CARTESIAN_POINT ( 'NONE',  ( -0.5577427821522301654, -0.2845877964562159024, 0.3641732283464567677 ) ) ;
#59285 = CARTESIAN_POINT ( 'NONE',  ( 1.181102362204725198, -0.1870078740157479769, 0.4822834645669291653 ) ) ;
#59286 = CARTESIAN_POINT ( 'NONE',  ( -0.4068241469816264999, -0.4281496062992124485, 0.4176697321401328655 ) ) ;
#59287 = CARTESIAN_POINT ( 'NONE',  ( 0.05249343832021075018, 0.2306618581243847221, -0.2411417322834647770 ) ) ;
#59288 = CARTESIAN_POINT ( 'NONE',  ( -1.594488188976377119, 0.1660481256975883668, -0.3530559997133364547 ) ) ;
#59289 = CARTESIAN_POINT ( 'NONE',  ( 0.7545931758530188826, -0.6692913385826771977, 0.1292274648535927661 ) ) ;
#59290 = B_SPLINE_CURVE_WITH_KNOTS ( 'NONE', 3,
 ( #29241, #22516, #15805, #74285, #23748, #81847, #80611, #4801, #75116, #17048, #11133, #67968, #73455, #56142, #9887, #74703, #10311, #42689, #54487, #55723, #80198, #36790, #48177, #49004, #41456, #73873, #3574, #3987, #55313, #35976, #81022, #24159 ),
 .UNSPECIFIED., .F., .F.,
 ( 4, 2, 2, 2, 2, 2, 2, 2, 2, 2, 2, 2, 2, 2, 2, 4 ),
 ( 0.03390883336407266024, 0.03455365212229282584, 0.03519847088051299144, 0.03648810839695332264, 0.03777774591339366078, 0.03906738342983399198, 0.04035702094627433012, 0.04164665846271466132, 0.04422593349559533066, 0.04680520852847600000, 0.04938448356135666933, 0.05067412107779700747, 0.05196375859423733867, 0.05325339611067767681, 0.05389821486889784241, 0.05454303362711801495 ),
 .UNSPECIFIED. ) ;
#59291 = CARTESIAN_POINT ( 'NONE',  ( 1.332020997375329197, -0.3162353388693405765, 0.4822834645669290543 ) ) ;
#59292 = CARTESIAN_POINT ( 'NONE',  ( 0.3917322834645670104, -0.1049643490035303411, -0.7335958005249343383 ) ) ;
#59293 = CARTESIAN_POINT ( 'NONE',  ( 0.4330708661417329575, 0.1771653543307087630, 0.000000000000000000 ) ) ;
#59294 = VERTEX_POINT ( 'NONE', #58674 ) ;
#59295 = CARTESIAN_POINT ( 'NONE',  ( -0.2891555358219908833, -0.2891555358219912164, -0.6889763779527559029 ) ) ;
#59296 = ORIENTED_EDGE ( 'NONE', *, *, #14203, .T. ) ;
#59297 = CARTESIAN_POINT ( 'NONE',  ( -0.6167979002624665030, -0.004921259842519576551, 0.3153832671262227771 ) ) ;
#59298 = CARTESIAN_POINT ( 'NONE',  ( -0.04593175853018302557, 0.2952755905511811885, 0.1292274648535926551 ) ) ;
#59299 = CARTESIAN_POINT ( 'NONE',  ( 2.554262525012302110, 1.537401574803149984, 0.4744094488188975722 ) ) ;
#59300 = CARTESIAN_POINT ( 'NONE',  ( -0.1509186351706028884, -0.05778040916215522460, 0.4822834645669289988 ) ) ;
#59301 = CARTESIAN_POINT ( 'NONE',  ( -0.07217847769028813698, -0.3162353388693409650, -0.4822834645669289433 ) ) ;
#59302 = CARTESIAN_POINT ( 'NONE',  ( -0.9645669291338575535, 0.1660481256975883668, -0.3530559997133364547 ) ) ;
#59303 = CARTESIAN_POINT ( 'NONE',  ( -0.9514435695538050464, -0.3162353388693405765, 0.4822834645669290543 ) ) ;
#59304 = CARTESIAN_POINT ( 'NONE',  ( 1.299212598425197429, -0.5511811023622047445, 6.969142054262312111E-17 ) ) ;
#59305 = CARTESIAN_POINT ( 'NONE',  ( -1.646981627296586703, -0.05778040916215522460, 0.4822834645669289988 ) ) ;
#59306 = CARTESIAN_POINT ( 'NONE',  ( 0.3392501089628018884, -0.1958661417322834220, -2.866797900262466836 ) ) ;
#59307 = CARTESIAN_POINT ( 'NONE',  ( 1.003937007874016185, 0.07958543189024071263, -0.2665933059059888421 ) ) ;
#59308 = CARTESIAN_POINT ( 'NONE',  ( 0.4199475065616805614, 0.2306618581243848609, 0.2411417322834645549 ) ) ;
#59309 = CARTESIAN_POINT ( 'NONE',  ( 0.2624671916010504757, 0.2306618581243848609, 0.2411417322834645549 ) ) ;
#59310 = AXIS2_PLACEMENT_3D ( 'NONE', #66717, #28812, #9876 ) ;
#59311 = CARTESIAN_POINT ( 'NONE',  ( 0.3996062992125986590, -0.1070741851644053111, -1.213910761154855189 ) ) ;
#59312 = CARTESIAN_POINT ( 'NONE',  ( -2.620894764083836925, 1.710972922415817665, 0.4417590601942920636 ) ) ;
#59313 = CARTESIAN_POINT ( 'NONE',  ( 0.1070741851644054776, -0.3996062992125984925, -0.9494750656167976199 ) ) ;
#59314 = CARTESIAN_POINT ( 'NONE',  ( 0.3996062992125985480, 2.446882876249141654E-17, -0.5098425196850393526 ) ) ;
#59315 = CARTESIAN_POINT ( 'NONE',  ( -0.3477690288713905509, -0.6692913385826771977, 0.1292274648535927661 ) ) ;
#59316 = CARTESIAN_POINT ( 'NONE',  ( -0.1265901696524993347, 0.4724409448818895907, 0.1509186351706036378 ) ) ;
#59317 = CARTESIAN_POINT ( 'NONE',  ( -0.3917322834645669549, -0.1049643490035306603, -2.020341207349081181 ) ) ;
#59318 = CARTESIAN_POINT ( 'NONE',  ( -1.233595800524933894, -0.5023911411419708095, -0.1820866141732282451 ) ) ;
#59319 = CARTESIAN_POINT ( 'NONE',  ( 0.9645669291338588858, 0.1660481256975885056, 0.3530559997133364547 ) ) ;
#59320 = CARTESIAN_POINT ( 'NONE',  ( 1.030183727034121421, -0.05778040916215522460, 0.4822834645669289988 ) ) ;
#59321 = CARTESIAN_POINT ( 'NONE',  ( -0.07217847769028787330, -0.08942795157527998196, 0.3641732283464567121 ) ) ;
#59322 = CARTESIAN_POINT ( 'NONE',  ( 0.5839895013123367340, -0.6692913385826773087, -0.1292274648535924053 ) ) ;
#59323 = CARTESIAN_POINT ( 'NONE',  ( 0.4091458600556403535, 0.2362204724409449896, -1.782808398950131101 ) ) ;
#59324 = CARTESIAN_POINT ( 'NONE',  ( -0.1968503937007867743, 0.1771653543307087630, 0.000000000000000000 ) ) ;
#59325 = CARTESIAN_POINT ( 'NONE',  ( 0.03280839895013198948, 0.2952755905511811885, 0.1292274648535926551 ) ) ;
#59326 = CARTESIAN_POINT ( 'NONE',  ( -0.2891555358219909388, -0.2891555358219912164, -1.238188976377952999 ) ) ;
#59327 = CARTESIAN_POINT ( 'NONE',  ( -1.587926509186350810, -0.4281496062992124485, 0.4176697321401328655 ) ) ;
#59328 = CARTESIAN_POINT ( 'NONE',  ( 0.7020997375328090762, -0.08942795157528024563, -0.3641732283464568787 ) ) ;
#59329 = CARTESIAN_POINT ( 'NONE',  ( 1.469816272965879911, -0.5023911411419708095, 0.1820866141732285504 ) ) ;
#59330 = CARTESIAN_POINT ( 'NONE',  ( -0.8858267716535425107, 0.1660481256975883668, -0.3530559997133364547 ) ) ;
#59331 = CARTESIAN_POINT ( 'NONE',  ( -0.1509186351706028884, -0.2845877964562161244, -0.3641732283464567121 ) ) ;
#59332 = DIRECTION ( 'NONE',  ( -1.734723475976806848E-16, -1.000000000000000000, 0.000000000000000000 ) ) ;
#59333 = CARTESIAN_POINT ( 'NONE',  ( -0.8595800524934373854, -0.3162353388693409650, -0.4822834645669289433 ) ) ;
#59334 = CARTESIAN_POINT ( 'NONE',  ( -0.7152230971128602510, -0.3162353388693405765, 0.4822834645669290543 ) ) ;
#59335 = CARTESIAN_POINT ( 'NONE',  ( -0.1509186351706028884, -0.3162353388693409650, -0.4822834645669289433 ) ) ;
#59336 = CARTESIAN_POINT ( 'NONE',  ( 0.3460692066303959202, -0.1998031496062991630, -2.701443569553806157 ) ) ;
#59337 = CARTESIAN_POINT ( 'NONE',  ( 0.2867679344610365999, 0.2867679344610365999, -2.107592232774591068 ) ) ;
#59338 = CARTESIAN_POINT ( 'NONE',  ( -0.5314960629921122726, 2.682389230697236115, -3.900966923095591010 ) ) ;
#59339 = CARTESIAN_POINT ( 'NONE',  ( 0.7742782152230979209, -0.004921259842519870586, -0.3153832671262229437 ) ) ;
#59340 = CARTESIAN_POINT ( 'NONE',  ( 1.207349081364829990, -0.6046776061558809534, -0.2411417322834644161 ) ) ;
#59341 = CARTESIAN_POINT ( 'NONE',  ( -0.7545931758530177724, 0.1771653543307087630, 0.09757992244046791164 ) ) ;
#59342 = CARTESIAN_POINT ( 'NONE',  ( -1.233595800524933894, 0.1283753931104748280, 0.1820866141732283561 ) ) ;
#59343 = CARTESIAN_POINT ( 'NONE',  ( -0.8202099737532799750, 0.2952755905511810774, -0.1292274648535930714 ) ) ;
#59344 = CARTESIAN_POINT ( 'NONE',  ( -0.5183727034120726440, -0.6692913385826773087, -0.1292274648535924053 ) ) ;
#59345 = CARTESIAN_POINT ( 'NONE',  ( 0.6233595800524942554, -0.08942795157528024563, -0.3641732283464568787 ) ) ;
#59346 = CARTESIAN_POINT ( 'NONE',  ( -0.2938400550950686085, 0.02965148040547831848, 5.527203440556597513 ) ) ;
#59347 = CARTESIAN_POINT ( 'NONE',  ( 1.076115485564305141, -0.5023911411419708095, 0.1820866141732285504 ) ) ;
#59348 = CARTESIAN_POINT ( 'NONE',  ( 0.2624671916010504757, 0.2306618581243848609, 0.2411417322834645549 ) ) ;
#59349 = CARTESIAN_POINT ( 'NONE',  ( 4.893765752498283308E-17, -0.3996062992125985480, 0.1594488188976377896 ) ) ;
#59350 = CARTESIAN_POINT ( 'NONE',  ( -0.6496062992125976043, -0.5400638737290844871, 0.3530559997133364547 ) ) ;
#59351 = CARTESIAN_POINT ( 'NONE',  ( 0.1049643490035304938, -0.3917322834645669549, -1.429790026246719359 ) ) ;
#59352 = CARTESIAN_POINT ( 'NONE',  ( 1.377952755905512472, -0.5511811023622047445, 6.969142054262312111E-17 ) ) ;
#59353 = CARTESIAN_POINT ( 'NONE',  ( 0.4002624671916016896, -0.05778040916215522460, 0.4822834645669289988 ) ) ;
#59354 = CARTESIAN_POINT ( 'NONE',  ( 0.1509186351706045259, -0.05778040916215560624, -0.4822834645669293319 ) ) ;
#59355 = CARTESIAN_POINT ( 'NONE',  ( -0.03937007874015669567, 0.1771653543307087630, 0.000000000000000000 ) ) ;
#59356 = CARTESIAN_POINT ( 'NONE',  ( 0.5643044619422579178, 0.009842519685039467087, 0.3409548833797002021 ) ) ;
#59357 = CARTESIAN_POINT ( 'NONE',  ( -0.1771653543307080136, 0.07958543189024071263, -0.2665933059059888421 ) ) ;
#59358 = CARTESIAN_POINT ( 'NONE',  ( 0.8661417322834653598, -0.1870078740157479769, 0.4822834645669291653 ) ) ;
#59359 = CARTESIAN_POINT ( 'NONE',  ( -0.7677165354330699465, 0.07958543189024085140, 0.2665933059059887866 ) ) ;
#59360 = CARTESIAN_POINT ( 'NONE',  ( -1.213910761154854745, -0.6692913385826771977, 0.1292274648535927661 ) ) ;
#59361 = CARTESIAN_POINT ( 'NONE',  ( 1.348312163386739426, 1.062992125984252079, 0.7386866130305692613 ) ) ;
#59362 = EDGE_LOOP ( 'NONE', ( #70224, #20472, #44981, #18223 ) ) ;
#59363 = CARTESIAN_POINT ( 'NONE',  ( -1.318897637795274802, 0.1660481256975885056, 0.3530559997133364547 ) ) ;
#59364 = CARTESIAN_POINT ( 'NONE',  ( -1.135170603674539924, -0.5511811023622046335, 0.09757992244046803654 ) ) ;
#59365 = COLOUR_RGB ( '', 0.40784314, 0.44705882, 0.49803922) ;
#59366 = CARTESIAN_POINT ( 'NONE',  ( -0.05249343832020938322, -0.6046776061558809534, -0.2411417322834644161 ) ) ;
#59367 = DIRECTION ( 'NONE',  ( 0.000000000000000000, 0.000000000000000000, -1.000000000000000000 ) ) ;
#59368 = CARTESIAN_POINT ( 'NONE',  ( -0.8005249343832011588, 0.05413385826771626580, -0.4176697321401330321 ) ) ;
#59369 = LINE ( 'NONE', #79177, #24291 ) ;
#59371 = CARTESIAN_POINT ( 'NONE',  ( 0.7874015748031503170, -0.1870078740157479769, 0.4822834645669291653 ) ) ;
#59370 = CARTESIAN_POINT ( 'NONE',  ( 1.620734908136483465, -0.6692913385826771977, 0.1292274648535927661 ) ) ;
#59372 = CARTESIAN_POINT ( 'NONE',  ( 1.036745406824147731, 0.05413385826771666132, 0.4176697321401328100 ) ) ;
#59373 = CARTESIAN_POINT ( 'NONE',  ( -0.3917322834645671215, 0.1049643490035301469, -2.387139107611548461 ) ) ;
#59374 = CARTESIAN_POINT ( 'NONE',  ( 1.581364829396326277, -0.05778040916215522460, 0.4822834645669289988 ) ) ;
#59375 = EDGE_CURVE ( 'NONE', #14913, #18027, #74090, .T. ) ;
#59376 = CARTESIAN_POINT ( 'NONE',  ( -1.332020997375327642, -0.3162353388693409650, -0.4822834645669289433 ) ) ;
#59377 = CARTESIAN_POINT ( 'NONE',  ( 0.2925321140481932369, -0.2925321140481932369, 0.05905511811023619884 ) ) ;
#59378 = ORIENTED_EDGE ( 'NONE', *, *, #46991, .F. ) ;
#59379 = CARTESIAN_POINT ( 'NONE',  ( -0.6102362204724400829, -0.4536011799217368745, -0.2665933059059886201 ) ) ;
#59380 = CARTESIAN_POINT ( 'NONE',  ( 0.2867679344610365999, -0.2867679344610365444, -1.822834645669291653 ) ) ;
#59381 = ORIENTED_EDGE ( 'NONE', *, *, #59829, .T. ) ;
#59382 = CARTESIAN_POINT ( 'NONE',  ( 0.3412073490813655186, 0.2306618581243848609, 0.2411417322834645549 ) ) ;
#59383 = CARTESIAN_POINT ( 'NONE',  ( 0.03937007874015806264, 0.2952755905511811885, 0.000000000000000000 ) ) ;
#59384 = CARTESIAN_POINT ( 'NONE',  ( -0.5446194225721777693, -0.05778040916215522460, 0.4822834645669289988 ) ) ;
#59385 = CARTESIAN_POINT ( 'NONE',  ( 1.482939632545932307, -0.4281496062992124485, 0.4176697321401328655 ) ) ;
#59386 = CARTESIAN_POINT ( 'NONE',  ( -0.7742782152230962556, -0.3690944881889765550, -0.3153832671262227771 ) ) ;
#59387 = CARTESIAN_POINT ( 'NONE',  ( -0.7426113562972006532, 2.209901789876323797, -0.5309055118110235227 ) ) ;
#59388 = CARTESIAN_POINT ( 'NONE',  ( 0.8464566929133866546, -0.5400638737290844871, 0.3530559997133364547 ) ) ;
#59389 = CARTESIAN_POINT ( 'NONE',  ( 0.5380577427821529035, -0.004921259842519870586, -0.3153832671262229437 ) ) ;
#59390 = CARTESIAN_POINT ( 'NONE',  ( -0.2427821522309703550, -0.3162353388693405765, 0.4822834645669290543 ) ) ;
#59391 = CARTESIAN_POINT ( 'NONE',  ( -0.1049643490035301746, -0.3917322834645670659, -1.097093545110549462 ) ) ;
#59392 = CARTESIAN_POINT ( 'NONE',  ( -0.6889763779527552368, 0.1660481256975885056, 0.3530559997133364547 ) ) ;
#59393 = CARTESIAN_POINT ( 'NONE',  ( -1.633858267716534529, -0.4536011799217368745, -0.2665933059059886201 ) ) ;
#59394 = CARTESIAN_POINT ( 'NONE',  ( 1.286089238845145033, -0.6046776061558809534, -0.2411417322834644161 ) ) ;
#59395 = CARTESIAN_POINT ( 'NONE',  ( 1.502624671916010790, -0.08942795157527998196, 0.3641732283464567121 ) ) ;
#59396 = ORIENTED_EDGE ( 'NONE', *, *, #64825, .T. ) ;
#59397 = CARTESIAN_POINT ( 'NONE',  ( -9.594673741351313045E-17, 0.3917322834645670659, -2.358943200296274689 ) ) ;
#59398 = CARTESIAN_POINT ( 'NONE',  ( 0.01968503937007957949, -0.5400638737290845981, -0.3530559997133363437 ) ) ;
#59399 = ORIENTED_EDGE ( 'NONE', *, *, #15762, .T. ) ;
#59400 = CARTESIAN_POINT ( 'NONE',  ( -1.122047244094487306, -0.5400638737290844871, 0.3530559997133364547 ) ) ;
#59401 = CARTESIAN_POINT ( 'NONE',  ( 1.069553805774278610, -0.6692913385826771977, 0.1292274648535927661 ) ) ;
#59402 = CARTESIAN_POINT ( 'NONE',  ( 1.259842519685040019, -0.1870078740157479769, 0.4822834645669291653 ) ) ;
#59403 = EDGE_CURVE ( 'NONE', #56613, #70572, #1861, .T. ) ;
#59404 = CARTESIAN_POINT ( 'NONE',  ( 0.4265091863517067039, -0.6692913385826773087, -0.1292274648535924053 ) ) ;
#59405 = CARTESIAN_POINT ( 'NONE',  ( -0.3871391076115476282, -0.05778040916215522460, 0.4822834645669289988 ) ) ;
#59406 = CARTESIAN_POINT ( 'NONE',  ( -9.594673741351313045E-17, 0.3917322834645670104, -1.974409448818897683 ) ) ;
#59407 = CARTESIAN_POINT ( 'NONE',  ( -1.299212598425196097, -0.6692913385826771977, 8.415575281601705876E-17 ) ) ;
#59408 = CARTESIAN_POINT ( 'NONE',  ( -0.5511811023622038563, -0.1870078740157479769, 0.4822834645669291653 ) ) ;
#59409 = EDGE_CURVE ( 'NONE', #40881, #66560, #80965, .T. ) ;
#59410 = CARTESIAN_POINT ( 'NONE',  ( -0.3937007874015740483, -0.1870078740157479769, 0.3641732283464567677 ) ) ;
#59411 = CARTESIAN_POINT ( 'NONE',  ( 1.348312163386739426, 1.062992125984252079, 0.6402614161801758463 ) ) ;
#59412 = CARTESIAN_POINT ( 'NONE',  ( -0.6758530183727028406, -0.6692913385826773087, -0.1292274648535924053 ) ) ;
#59413 = CARTESIAN_POINT ( 'NONE',  ( -0.5314960629921395840, 2.725419031863056674, 3.884512598959603658 ) ) ;
#59414 = CARTESIAN_POINT ( 'NONE',  ( 0.8070866141732288002, 0.1660481256975885056, 0.3530559997133364547 ) ) ;
#59415 = CARTESIAN_POINT ( 'NONE',  ( 0.2925321140481932369, -0.2925321140481932369, -1.988188976377952777 ) ) ;
#59416 = CARTESIAN_POINT ( 'NONE',  ( 3.929894648360968024, 1.125820779260225502, -0.2379601796926557877 ) ) ;
#59417 =( BOUNDED_CURVE ( )  B_SPLINE_CURVE ( 2, ( #50720, #56221, #5695, #37686, #50309, #4881, #75600, #10793, #37284, #63361, #63770, #17127, #42759 ),
 .UNSPECIFIED., .F., .F. ) 
 B_SPLINE_CURVE_WITH_KNOTS ( ( 3, 2, 2, 2, 2, 2, 3 ),
 ( 0.2642401855438917813, 0.2651515151515151381, 0.2689393939393939226, 0.2727272727272727071, 0.2765151515151514916, 0.2803030303030302761, 0.2812143599106537439 ),
 .UNSPECIFIED. ) 
 CURVE ( )  GEOMETRIC_REPRESENTATION_ITEM ( )  RATIONAL_B_SPLINE_CURVE ( ( 0.9875488213027530104, 0.9918020599134685922, 1.000000000000000000, 0.9659258262890683122, 1.000000000000000000, 0.9659258262890683122, 1.000000000000000000, 0.9659258262890683122, 1.000000000000000000, 0.9659258262890683122, 1.000000000000000000, 0.9918020599134677040, 0.9875488213027521223 ) ) 
 REPRESENTATION_ITEM ( '' )  );
#59418 = CARTESIAN_POINT ( 'NONE',  ( -0.2755905511811015396, -0.6692913385826771977, 8.415575281601705876E-17 ) ) ;
#59420 = CARTESIAN_POINT ( 'NONE',  ( -0.8792650918635160906, 0.009842519685039144428, -0.3409548833797004797 ) ) ;
#59419 = CARTESIAN_POINT ( 'NONE',  ( 0.8530183727034128527, -0.3690944881889763329, 0.3153832671262228327 ) ) ;
#59421 = CARTESIAN_POINT ( 'NONE',  ( 0.3458507752293908943, -0.3458507752293908943, -0.6476377952755905110 ) ) ;
#59422 = CARTESIAN_POINT ( 'NONE',  ( 1.351706036745407680, -0.004921259842519576551, 0.3153832671262227771 ) ) ;
#59423 = CARTESIAN_POINT ( 'NONE',  ( 1.122047244094488860, 0.1660481256975885056, 0.3530559997133364547 ) ) ;
#59424 = CARTESIAN_POINT ( 'NONE',  ( -0.3949938075777409963, -7.255918531996591613E-17, -0.2736220472440945017 ) ) ;
#59425 = PRODUCT ( 'Chuck Body Assembly Bolts', 'Chuck Body Assembly Bolts', '', ( #66693 ) ) ;
#59426 = CARTESIAN_POINT ( 'NONE',  ( -0.006561679790025524116, -0.3162353388693405765, 0.4822834645669290543 ) ) ;
#59427 = CARTESIAN_POINT ( 'NONE',  ( -1.463254593175852492, 0.2952755905511811885, 0.1292274648535926551 ) ) ;
#59428 = CARTESIAN_POINT ( 'NONE',  ( -1.601049868766403650, -0.6046776061558807314, 0.2411417322834647770 ) ) ;
#59429 = CARTESIAN_POINT ( 'NONE',  ( -0.04593175853018302557, -0.6692913385826773087, -0.1292274648535924053 ) ) ;
#59430 = CARTESIAN_POINT ( 'NONE',  ( -0.1058382717557497660, -0.3949938075777411073, -0.3064304461942257696 ) ) ;
#59431 = CARTESIAN_POINT ( 'NONE',  ( 1.220472440944882608, 0.2952755905511811885, 0.000000000000000000 ) ) ;
#59432 = CARTESIAN_POINT ( 'NONE',  ( 0.5839895013123367340, -0.6692913385826773087, -0.1292274648535924053 ) ) ;
#59433 = AXIS2_PLACEMENT_3D ( 'NONE', #48082, #22832, #48910 ) ;
#59434 = CARTESIAN_POINT ( 'NONE',  ( 0.8792650918635177559, -0.004921259842519576551, 0.3153832671262227771 ) ) ;
#59435 = CARTESIAN_POINT ( 'NONE',  ( 0.2588821398346105584, 1.118542505099386908, 0.1762126857782035649 ) ) ;
#59436 = CARTESIAN_POINT ( 'NONE',  ( 0.5183727034120741983, -0.5511811023622046335, 0.09757992244046803654 ) ) ;
#59437 = CARTESIAN_POINT ( 'NONE',  ( -1.430446194225720724, 0.05413385826771626580, -0.4176697321401330321 ) ) ;
#59438 = ADVANCED_FACE ( 'NONE', ( #74650 ), #3652, .F. ) ;
#59439 = CARTESIAN_POINT ( 'NONE',  ( -0.3460692066303957537, -0.1998031496062994405, -1.074146981627296604 ) ) ;
#59440 = CARTESIAN_POINT ( 'NONE',  ( 1.161417322834646493, -0.5400638737290844871, 0.3530559997133364547 ) ) ;
#59441 = CARTESIAN_POINT ( 'NONE',  ( -9.594673741351313045E-17, 0.3917322834645670104, -0.6220472440944880832 ) ) ;
#59443 = DIRECTION ( 'NONE',  ( -0.000000000000000000, -0.000000000000000000, -1.000000000000000000 ) ) ;
#59442 = CARTESIAN_POINT ( 'NONE',  ( 0.2821522309711292364, 0.2952755905511810774, -0.1292274648535930714 ) ) ;
#59444 = CARTESIAN_POINT ( 'NONE',  ( -0.3277333542595150528, 0.004960608223778509643, -0.3437734562760191848 ) ) ;
#59445 = CARTESIAN_POINT ( 'NONE',  ( 0.4921259842519691285, 0.07958543189024085140, 0.2665933059059887866 ) ) ;
#59446 = EDGE_CURVE ( 'NONE', #42501, #34982, #37219, .T. ) ;
#59447 = CARTESIAN_POINT ( 'NONE',  ( 0.6364829396325465405, -0.3162353388693409650, -0.4822834645669289433 ) ) ;
#59448 = DIRECTION ( 'NONE',  ( -0.000000000000000000, -1.000000000000000000, -0.000000000000000000 ) ) ;
#59449 = CARTESIAN_POINT ( 'NONE',  ( -0.8858267716535425107, 0.07958543189024071263, -0.2665933059059888421 ) ) ;
#59450 = CARTESIAN_POINT ( 'NONE',  ( -1.108923884514435132, -0.3162353388693405765, 0.4822834645669290543 ) ) ;
#59451 = CARTESIAN_POINT ( 'NONE',  ( -1.620734908136482577, -0.6692913385826773087, -0.1292274648535924053 ) ) ;
#59452 = CARTESIAN_POINT ( 'NONE',  ( 0.5905511811023629321, 0.2952755905511811885, 0.000000000000000000 ) ) ;
#59453 = B_SPLINE_CURVE_WITH_KNOTS ( 'NONE', 3,
 ( #30134, #43163, #36867, #69686 ),
 .UNSPECIFIED., .F., .F.,
 ( 4, 4 ),
 ( 0.08702371034448116993, 0.08847090869701865201 ),
 .UNSPECIFIED. ) ;
#59454 = CARTESIAN_POINT ( 'NONE',  ( 1.686351706036745890, 0.2952755905511811885, 0.1292274648535926551 ) ) ;
#59455 = EDGE_CURVE ( 'NONE', #47884, #17151, #62000, .T. ) ;
#59456 = CARTESIAN_POINT ( 'NONE',  ( 1.109416077537178191, 1.093657130816544143, -0.1685245874982175818 ) ) ;
#59457 = CARTESIAN_POINT ( 'NONE',  ( 0.6496062992125991586, 0.1660481256975885056, 0.3530559997133364547 ) ) ;
#59458 = CARTESIAN_POINT ( 'NONE',  ( -0.4091458600556402980, -0.2362204724409451284, -2.806430446194225770 ) ) ;
#59459 = CARTESIAN_POINT ( 'NONE',  ( -1.646051170424378096, 0.000000000000000000, 0.3464511005275205946 ) ) ;
#59460 = CARTESIAN_POINT ( 'NONE',  ( 1.496062992125985147, -0.1870078740157479769, 0.4822834645669291653 ) ) ;
#59461 = CARTESIAN_POINT ( 'NONE',  ( -1.535433070866141225, 0.1771653543307087630, 0.000000000000000000 ) ) ;
#59462 = CARTESIAN_POINT ( 'NONE',  ( 1.167979002624672580, -0.3690944881889763329, 0.3153832671262228327 ) ) ;
#59463 = CARTESIAN_POINT ( 'NONE',  ( -1.456692913385826182, 0.1771653543307087630, 0.000000000000000000 ) ) ;
#59464 = CARTESIAN_POINT ( 'NONE',  ( -0.6889763779527552368, 0.07958543189024085140, 0.2665933059059887866 ) ) ;
#59465 = CARTESIAN_POINT ( 'NONE',  ( 0.2362204724409449064, 0.4091458600556404646, -2.034120734908136718 ) ) ;
#59466 = CARTESIAN_POINT ( 'NONE',  ( 0.7217847769028878924, -0.3690944881889765550, -0.3153832671262227771 ) ) ;
#59467 = CARTESIAN_POINT ( 'NONE',  ( 0.4330708661417329575, 0.2952755905511811885, 0.000000000000000000 ) ) ;
#59468 = CARTESIAN_POINT ( 'NONE',  ( 1.036745406824147508, -0.4281496062992127816, -0.4176697321401328100 ) ) ;
#59469 = CARTESIAN_POINT ( 'NONE',  ( 0.2427821522309719648, -0.05778040916215522460, 0.4822834645669289988 ) ) ;
#59470 = CARTESIAN_POINT ( 'NONE',  ( 0.09186351706036799403, -0.3690944881889765550, -0.3153832671262227771 ) ) ;
#59471 = CARTESIAN_POINT ( 'NONE',  ( 1.148293963254593653, 0.2952755905511810774, -0.1292274648535930714 ) ) ;
#59472 = CARTESIAN_POINT ( 'NONE',  ( -0.1698998578625667832, -2.609869883881465018E-15, -0.3464511005275220379 ) ) ;
#59473 = CARTESIAN_POINT ( 'NONE',  ( -0.7414698162729651543, 0.2952755905511810774, -0.1292274648535930714 ) ) ;
#59474 = CARTESIAN_POINT ( 'NONE',  ( 0.1998031496062992740, 0.3460692066303959757, -0.9317585301837270073 ) ) ;
#59475 = CARTESIAN_POINT ( 'NONE',  ( 0.1181102362204724254, 0.04921259842519697808, 0.08523872084492500889 ) ) ;
#59476 = CARTESIAN_POINT ( 'NONE',  ( 0.1049868766404206816, -0.6046776061558809534, -0.2411417322834644161 ) ) ;
#59477 = CARTESIAN_POINT ( 'NONE',  ( -0.9842519685039360366, 0.2952755905511811885, 0.000000000000000000 ) ) ;
#59478 = CARTESIAN_POINT ( 'NONE',  ( -0.01968503937007793844, -0.5400638737290844871, 0.3530559997133364547 ) ) ;
#59479 = CARTESIAN_POINT ( 'NONE',  ( 0.1070741851644053527, 0.3996062992125986590, -2.670603674540682260 ) ) ;
#59480 = CARTESIAN_POINT ( 'NONE',  ( 0.2891555358219910499, -0.2891555358219909944, -1.830708661417323135 ) ) ;
#59482 = CARTESIAN_POINT ( 'NONE',  ( 0.3917322834645670104, 2.398668435337828261E-17, -0.7401574803149605364 ) ) ;
#59481 = AXIS2_PLACEMENT_3D ( 'NONE', #74769, #61712, #80678 ) ;
#59483 = CARTESIAN_POINT ( 'NONE',  ( 0.4153800209585299386, 1.308165027668613645, -1.396905599340544368 ) ) ;
#59484 = CARTESIAN_POINT ( 'NONE',  ( -1.220472440944881054, 0.1771653543307087630, 0.000000000000000000 ) ) ;
#59485 = CARTESIAN_POINT ( 'NONE',  ( 0.3392501089628018329, 0.1958661417322835607, -1.068241469816272771 ) ) ;
#59486 = CARTESIAN_POINT ( 'NONE',  ( -1.391076115485563758, 0.2306618581243848609, 0.2411417322834645549 ) ) ;
#59487 = CARTESIAN_POINT ( 'NONE',  ( 0.1049643490035303689, 0.3917322834645668994, 0.08400881709417505616 ) ) ;
#59488 = CARTESIAN_POINT ( 'NONE',  ( 0.4330708661417329575, 0.2952755905511811885, 0.000000000000000000 ) ) ;
#59489 = CARTESIAN_POINT ( 'NONE',  ( -0.6758530183727028406, -0.5511811023622048555, -0.09757992244046775898 ) ) ;
#59490 = CARTESIAN_POINT ( 'NONE',  ( 0.6889763779527563470, 0.1660481256975883668, -0.3530559997133364547 ) ) ;
#59491 = CARTESIAN_POINT ( 'NONE',  ( 0.3477690288713918276, 0.2952755905511811885, 0.1292274648535926551 ) ) ;
#59492 = CARTESIAN_POINT ( 'NONE',  ( 0.1239713036211918251, 1.079207359476603845, 1.115280228140321350 ) ) ;
#59493 = CARTESIAN_POINT ( 'NONE',  ( 0.3996062992125986035, 2.446882876249141962E-17, -2.795275590551181022 ) ) ;
#59494 = CARTESIAN_POINT ( 'NONE',  ( -0.1049643490035307158, 0.3917322834645670104, -1.105662360401261868 ) ) ;
#59495 = CARTESIAN_POINT ( 'NONE',  ( 1.325459317585302665, -0.4281496062992124485, 0.4176697321401328655 ) ) ;
#59496 = CARTESIAN_POINT ( 'NONE',  ( -0.08530183727034056085, -0.05778040916215560624, -0.4822834645669293319 ) ) ;
#59497 = ADVANCED_FACE ( 'NONE', ( #49363 ), #43930, .F. ) ;
#59498 = CARTESIAN_POINT ( 'NONE',  ( 1.358267716535433323, -0.5400638737290845981, -0.3530559997133363437 ) ) ;
#59499 = CARTESIAN_POINT ( 'NONE',  ( 0.9580052493438327987, -0.4281496062992127816, -0.4176697321401328100 ) ) ;
#59500 = CARTESIAN_POINT ( 'NONE',  ( 0.1958661417322834775, 0.3392501089628018884, -0.3864829396325459854 ) ) ;
#59501 = CARTESIAN_POINT ( 'NONE',  ( 0.2099737532808405305, 0.2306618581243847221, -0.2411417322834647770 ) ) ;
#59502 = CARTESIAN_POINT ( 'NONE',  ( 0.8136482939632553313, -0.6046776061558809534, -0.2411417322834644161 ) ) ;
#59503 = CARTESIAN_POINT ( 'NONE',  ( -0.2165354330708654795, 0.1660481256975885056, 0.3530559997133364547 ) ) ;
#59504 = CARTESIAN_POINT ( 'NONE',  ( 0.7742782152230979209, -0.004921259842519870586, -0.3153832671262229437 ) ) ;
#59505 = CARTESIAN_POINT ( 'NONE',  ( -1.181102362204723644, -0.1870078740157480879, -0.4822834645669291653 ) ) ;
#59506 = CARTESIAN_POINT ( 'NONE',  ( -1.515748031496062076, 0.1660481256975883668, -0.3530559997133364547 ) ) ;
#59507 = CARTESIAN_POINT ( 'NONE',  ( 0.9514435695538062676, -0.05778040916215522460, 0.4822834645669289988 ) ) ;
#59508 = CARTESIAN_POINT ( 'NONE',  ( 0.3428707098289829891, -0.1906283239480039415, -1.929133858267717549 ) ) ;
#59509 = CARTESIAN_POINT ( 'NONE',  ( 0.3392501089628018884, -0.1958661417322834220, -1.829396325459317518 ) ) ;
#59510 = ORIENTED_EDGE ( 'NONE', *, *, #24528, .F. ) ;
#59511 = CARTESIAN_POINT ( 'NONE',  ( 0.1998031496062994405, -0.3460692066303958092, -0.2493438320209974135 ) ) ;
#59512 = VERTEX_POINT ( 'NONE', #60755 ) ;
#59513 = CARTESIAN_POINT ( 'NONE',  ( 1.266404199475066328, -0.3162353388693409650, -0.4822834645669289433 ) ) ;
#59514 = CARTESIAN_POINT ( 'NONE',  ( 0.8267716535433077274, 0.1771653543307087630, 0.000000000000000000 ) ) ;
#59515 = CARTESIAN_POINT ( 'NONE',  ( 0.4177787735907000366, 1.299212598425196985, -1.559171609364239375 ) ) ;
#59516 = CARTESIAN_POINT ( 'NONE',  ( 1.348312163386739426, 0.2929341459200028863, 0.7386866130305692613 ) ) ;
#59517 = CARTESIAN_POINT ( 'NONE',  ( -0.1958661417322836718, 0.3392501089628017219, -1.200131233595800540 ) ) ;
#59518 = CARTESIAN_POINT ( 'NONE',  ( 1.496062992125984703, -0.1870078740157480879, -0.4822834645669291653 ) ) ;
#59519 = CARTESIAN_POINT ( 'NONE',  ( -0.3992723400743253825, -6.536159750466813772E-18, -1.929133858267716661 ) ) ;
#59520 = CARTESIAN_POINT ( 'NONE',  ( -0.5118110236220466680, -0.6692913385826771977, 8.415575281601705876E-17 ) ) ;
#59521 = CARTESIAN_POINT ( 'NONE',  ( 0.8989501312335963501, -0.6692913385826773087, -0.1292274648535924053 ) ) ;
#59522 = VERTEX_POINT ( 'NONE', #23689 ) ;
#59523 = CARTESIAN_POINT ( 'NONE',  ( -1.450131233595799651, -0.6692913385826771977, 0.1292274648535927661 ) ) ;
#59524 = CARTESIAN_POINT ( 'NONE',  ( 0.6299212598425337761, 1.724409448818898127, -3.886287458032460229 ) ) ;
#59525 = CARTESIAN_POINT ( 'NONE',  ( 3.523619145740946923, 4.103338224919997224, 3.796341255999502451 ) ) ;
#59526 = CARTESIAN_POINT ( 'NONE',  ( 1.515748031496063408, 0.07958543189024085140, 0.2665933059059887866 ) ) ;
#59527 = DIRECTION ( 'NONE',  ( -1.000000000000000000, 0.000000000000000000, 0.000000000000000000 ) ) ;
#59528 = CARTESIAN_POINT ( 'NONE',  ( -0.7611548556430438595, -0.5023911411419708095, -0.1820866141732282451 ) ) ;
#59529 = CARTESIAN_POINT ( 'NONE',  ( -1.555118110236219930, -0.5400638737290845981, -0.3530559997133363437 ) ) ;
#59530 = CARTESIAN_POINT ( 'NONE',  ( 0.5511811023622055217, -0.1870078740157479769, 0.4822834645669291653 ) ) ;
#59531 = ORIENTED_EDGE ( 'NONE', *, *, #19583, .T. ) ;
#59533 = DIRECTION ( 'NONE',  ( -3.096699300667737957E-16, 1.000000000000000000, -0.000000000000000000 ) ) ;
#59532 = CARTESIAN_POINT ( 'NONE',  ( 1.535433070866142558, 0.2952755905511811885, 0.000000000000000000 ) ) ;
#59534 = CARTESIAN_POINT ( 'NONE',  ( -0.8858267716535425107, 0.07958543189024071263, -0.2665933059059888421 ) ) ;
#59535 = CARTESIAN_POINT ( 'NONE',  ( 1.010498687664042716, -0.4281496062992124485, 0.4176697321401328655 ) ) ;
#59536 = CARTESIAN_POINT ( 'NONE',  ( -1.640419947506561060, -0.4281496062992127816, -0.4176697321401328100 ) ) ;
#59537 = CARTESIAN_POINT ( 'NONE',  ( 0.2867679344610365999, -0.2867679344610365999, -1.123340264270654698 ) ) ;
#59538 = AXIS2_PLACEMENT_3D ( 'NONE', #3162, #37510, #79784 ) ;
#59539 = CARTESIAN_POINT ( 'NONE',  ( -0.6561679790026240244, -0.5023911411419708095, 0.1820866141732285504 ) ) ;
#59540 = CARTESIAN_POINT ( 'NONE',  ( 1.581364829396326277, -0.3162353388693409650, -0.4822834645669289433 ) ) ;
#59541 = MANIFOLD_SOLID_BREP ( 'Cut-Sweep1', #36623 ) ;
#59542 = CARTESIAN_POINT ( 'NONE',  ( 1.436417322834644184, 0.8346805926620878280, -0.3149606299212601157 ) ) ;
#59543 = CARTESIAN_POINT ( 'NONE',  ( 0.6233595800524939223, -0.3162353388693405765, 0.4822834645669290543 ) ) ;
#59544 = CARTESIAN_POINT ( 'NONE',  ( -1.017060367454067249, -0.08942795157527998196, 0.3641732283464567121 ) ) ;
#59545 = CARTESIAN_POINT ( 'NONE',  ( -0.4133858267716528645, 0.07958543189024071263, -0.2665933059059888421 ) ) ;
#59546 = CARTESIAN_POINT ( 'NONE',  ( -0.2034120734908131112, -0.6692913385826773087, -0.1292274648535924053 ) ) ;
#59547 = CARTESIAN_POINT ( 'NONE',  ( -1.023622047244093558, -0.1870078740157479769, 0.3641732283464567677 ) ) ;
#59548 = CARTESIAN_POINT ( 'NONE',  ( 0.1049643490035304799, -0.3917322834645670104, -0.2395206281177972019 ) ) ;
#59549 = CARTESIAN_POINT ( 'NONE',  ( 0.8792650918635177559, -0.4281496062992127816, -0.4176697321401328100 ) ) ;
#59550 = CARTESIAN_POINT ( 'NONE',  ( 0.8780747636526964328, 6.817843310734658629E-16, 0.3627989612356145588 ) ) ;
#59551 = CARTESIAN_POINT ( 'NONE',  ( -0.4724409448818895907, -0.1265901696524993070, -1.697506561679789971 ) ) ;
#59552 = CARTESIAN_POINT ( 'NONE',  ( -0.9580052493438311334, -0.4281496062992124485, 0.4176697321401328655 ) ) ;
#59553 = CARTESIAN_POINT ( 'NONE',  ( -0.1837270341207343505, -0.5023911411419708095, 0.1820866141732285504 ) ) ;
#59554 = CARTESIAN_POINT ( 'NONE',  ( -1.410761154855641575, -0.3162353388693409650, -0.4822834645669289433 ) ) ;
#59555 = CARTESIAN_POINT ( 'NONE',  ( 0.7414698162729663755, 0.1771653543307087630, 0.09757992244046791164 ) ) ;
#59556 = CARTESIAN_POINT ( 'NONE',  ( -0.5314960629921254842, -0.4536011799217368745, -0.2665933059059886201 ) ) ;
#59557 = CARTESIAN_POINT ( 'NONE',  ( -0.9711286089238838626, -0.6046776061558807314, 0.2411417322834647770 ) ) ;
#59558 = CARTESIAN_POINT ( 'NONE',  ( -1.496062992125983815, -0.1870078740157480879, -0.4822834645669291653 ) ) ;
#59559 = CARTESIAN_POINT ( 'NONE',  ( -1.594488188976377119, 0.1660481256975883668, -0.3530559997133364547 ) ) ;
#59560 = DIRECTION ( 'NONE',  ( 0.000000000000000000, 0.000000000000000000, -1.000000000000000000 ) ) ;
#59561 = CARTESIAN_POINT ( 'NONE',  ( 0.9317585301837276734, -0.004921259842519870586, -0.3153832671262229437 ) ) ;
#59562 = CARTESIAN_POINT ( 'NONE',  ( 0.3280839895013130669, -0.4281496062992127816, -0.4176697321401328100 ) ) ;
#59563 = CARTESIAN_POINT ( 'NONE',  ( -1.299212598425196097, 0.2952755905511811885, 0.000000000000000000 ) ) ;
#59564 = CARTESIAN_POINT ( 'NONE',  ( 1.246719160104987623, -0.3690944881889763329, 0.3153832671262228327 ) ) ;
#59565 = ORIENTED_EDGE ( 'NONE', *, *, #64580, .T. ) ;
#59566 = CARTESIAN_POINT ( 'NONE',  ( 0.3460692066303958092, 0.1998031496062993018, -2.727690288713910949 ) ) ;
#59567 = CARTESIAN_POINT ( 'NONE',  ( -1.233595800524933894, -0.5023911411419708095, -0.1820866141732282451 ) ) ;
#59568 = CARTESIAN_POINT ( 'NONE',  ( -0.4199475065616791736, -0.6046776061558807314, 0.2411417322834647770 ) ) ;
#59569 = CARTESIAN_POINT ( 'NONE',  ( 0.1312335958005255154, -0.6046776061558807314, 0.2411417322834647770 ) ) ;
#59570 = CARTESIAN_POINT ( 'NONE',  ( -1.292650918635170010, -0.5511811023622046335, 0.09757992244046803654 ) ) ;
#59571 = CARTESIAN_POINT ( 'NONE',  ( 0.1070741851644053388, 0.3996062992125986035, -1.645013123359579943 ) ) ;
#59572 = CARTESIAN_POINT ( 'NONE',  ( -1.332020997375327642, -0.3162353388693409650, -0.4822834645669289433 ) ) ;
#59573 = CARTESIAN_POINT ( 'NONE',  ( 0.5905511811023629321, 0.2952755905511811885, 0.000000000000000000 ) ) ;
#59574 = CARTESIAN_POINT ( 'NONE',  ( 8.195543980992789655E-16, -0.1870078740157480879, -0.4822834645669291653 ) ) ;
#59575 = CARTESIAN_POINT ( 'NONE',  ( 1.174540682414699111, -0.05778040916215560624, -0.4822834645669293319 ) ) ;
#59576 = DIRECTION ( 'NONE',  ( 0.7071067811865333619, 8.659560562354760295E-17, -0.7071067811865615615 ) ) ;
#59577 = CARTESIAN_POINT ( 'NONE',  ( 0.3996062992125986590, -0.1070741851644053111, -1.528871391076114916 ) ) ;
#59578 = CARTESIAN_POINT ( 'NONE',  ( 0.3949938075777411073, -0.1058382717557499464, -0.7414698162729659314 ) ) ;
#59579 = CIRCLE ( 'NONE', #32727, 0.1771653543307088186 ) ;
#59580 = CARTESIAN_POINT ( 'NONE',  ( 0.2850944291156183308, 1.158178041707070172, -1.676740862593898207 ) ) ;
#59581 = CARTESIAN_POINT ( 'NONE',  ( 0.4330708661417329575, -0.5511811023622047445, 6.969142054262312111E-17 ) ) ;
#59582 = CARTESIAN_POINT ( 'NONE',  ( -0.4658792650918627265, -0.05778040916215522460, 0.4822834645669289988 ) ) ;
#59583 = CARTESIAN_POINT ( 'NONE',  ( 1.220472440944882386, -0.6692913385826771977, 8.415575281601705876E-17 ) ) ;
#59584 = CARTESIAN_POINT ( 'NONE',  ( -0.1974969037888704149, -0.3420746716998661063, -1.559711286089239035 ) ) ;
#59585 = CARTESIAN_POINT ( 'NONE',  ( -0.09842519685039295696, -0.4536011799217367080, 0.2665933059059888421 ) ) ;
#59586 = CARTESIAN_POINT ( 'NONE',  ( -1.115485564304461219, 0.05413385826771626580, -0.4176697321401330321 ) ) ;
#59587 = CARTESIAN_POINT ( 'NONE',  ( -1.633858267716534529, 0.1660481256975885056, 0.3530559997133364547 ) ) ;
#59588 = CARTESIAN_POINT ( 'NONE',  ( 0.4724409448818898682, 2.892866454678787531E-17, -2.007874015748031482 ) ) ;
#59589 = CARTESIAN_POINT ( 'NONE',  ( 0.3913445824879516199, -0.02733964191756152462, -2.755905511811024056 ) ) ;
#59590 = ORIENTED_EDGE ( 'NONE', *, *, #55337, .T. ) ;
#59591 = ADVANCED_FACE ( 'NONE', ( #30003 ), #17407, .T. ) ;
#59592 = ORIENTED_EDGE ( 'NONE', *, *, #45224, .T. ) ;
#59593 = CIRCLE ( 'NONE', #67736, 0.1937007874015747588 ) ;
#59594 = CARTESIAN_POINT ( 'NONE',  ( 1.548556430446194954, -0.5023911411419708095, 0.1820866141732285504 ) ) ;
#59596 = CARTESIAN_POINT ( 'NONE',  ( -1.062992125984250968, -0.6692913385826771977, 8.415575281601705876E-17 ) ) ;
#59595 = CARTESIAN_POINT ( 'NONE',  ( -1.292650918635170010, 0.1771653543307087075, -0.09757992244046823083 ) ) ;
#59597 = CARTESIAN_POINT ( 'NONE',  ( 0.2867679344610365999, 0.2867679344610365999, -2.422552862695851683 ) ) ;
#59598 = CARTESIAN_POINT ( 'NONE',  ( -1.603475055217291612, 1.267857067133556281, -0.04573490813648263542 ) ) ;
#59599 = CARTESIAN_POINT ( 'NONE',  ( 1.332020997375329197, -0.3162353388693405765, 0.4822834645669290543 ) ) ;
#59600 = CARTESIAN_POINT ( 'NONE',  ( -1.391076115485563758, 0.2306618581243848609, 0.2411417322834645549 ) ) ;
#59601 = CARTESIAN_POINT ( 'NONE',  ( -0.01968503937007793844, -0.5400638737290844871, 0.3530559997133364547 ) ) ;
#59602 = CARTESIAN_POINT ( 'NONE',  ( -1.377952755905511140, -0.6692913385826771977, 8.415575281601705876E-17 ) ) ;
#59603 = CARTESIAN_POINT ( 'NONE',  ( 0.1049643490035303689, 0.3917322834645668994, -2.750636852197163584 ) ) ;
#59604 = CARTESIAN_POINT ( 'NONE',  ( 0.7611548556430451917, -0.6046776061558807314, 0.2411417322834647770 ) ) ;
#59605 = CARTESIAN_POINT ( 'NONE',  ( -0.3392501089628019995, 0.1958661417322832277, -1.750656167979002698 ) ) ;
#59606 = CARTESIAN_POINT ( 'NONE',  ( -1.043307086614172041, -0.4536011799217367080, 0.2665933059059888421 ) ) ;
#59607 = VERTEX_POINT ( 'NONE', #60346 ) ;
#59608 = CARTESIAN_POINT ( 'NONE',  ( -0.3949938075777411628, 0.1058382717557497937, -2.395013123359580387 ) ) ;
#59609 = ORIENTED_EDGE ( 'NONE', *, *, #77894, .F. ) ;
#59610 = CARTESIAN_POINT ( 'NONE',  ( 1.604771003085129211, 1.278209470906375378, 0.1466069496707752828 ) ) ;
#59611 = CARTESIAN_POINT ( 'NONE',  ( -0.9251968503937002541, 0.1660481256975885056, 0.3530559997133364547 ) ) ;
#59612 = CARTESIAN_POINT ( 'NONE',  ( -1.167979002624671470, 0.05413385826771666132, 0.4176697321401328100 ) ) ;
#59613 = CARTESIAN_POINT ( 'NONE',  ( 4.893765752498283924E-17, -0.3996062992125986035, -0.7086614173228346081 ) ) ;
#59614 = CARTESIAN_POINT ( 'NONE',  ( -1.450131233595799651, -0.6692913385826771977, 0.1292274648535927661 ) ) ;
#59615 = CARTESIAN_POINT ( 'NONE',  ( -1.482939632545930975, -0.4281496062992127816, -0.4176697321401328100 ) ) ;
#59616 = CARTESIAN_POINT ( 'NONE',  ( -1.272965879265091305, 0.05413385826771626580, -0.4176697321401330321 ) ) ;
#59617 = FILL_AREA_STYLE_COLOUR ( '', #78129 ) ;
#59618 = CARTESIAN_POINT ( 'NONE',  ( -0.2867679344610364334, -0.2867679344610367109, -0.1437007874015748810 ) ) ;
#59619 = CARTESIAN_POINT ( 'NONE',  ( 0.1640419947506569498, -0.2845877964562161244, -0.3641732283464567121 ) ) ;
#59620 = CARTESIAN_POINT ( 'NONE',  ( 0.3392501089628018884, -0.1958661417322834220, -0.8195538057742782767 ) ) ;
#59621 = CARTESIAN_POINT ( 'NONE',  ( -0.7349081364829390672, 0.1283753931104746893, -0.1820866141732285504 ) ) ;
#59622 = CARTESIAN_POINT ( 'NONE',  ( -1.089238845144356427, -0.4281496062992127816, -0.4176697321401328100 ) ) ;
#59623 = CARTESIAN_POINT ( 'NONE',  ( 1.010498687664042716, 0.05413385826771626580, -0.4176697321401330321 ) ) ;
#59624 = CARTESIAN_POINT ( 'NONE',  ( -0.8792650918635160906, -0.4281496062992124485, 0.4176697321401328655 ) ) ;
#59625 = CARTESIAN_POINT ( 'NONE',  ( 0.3917322834645669549, 0.1049643490035304660, 0.04068241469816277767 ) ) ;
#59626 = ORIENTED_EDGE ( 'NONE', *, *, #20226, .T. ) ;
#59627 = CARTESIAN_POINT ( 'NONE',  ( -1.003937007874014853, 0.1660481256975885056, 0.3530559997133364547 ) ) ;
#59628 = CARTESIAN_POINT ( 'NONE',  ( 0.7545931758530188826, -0.6692913385826771977, 0.1292274648535927661 ) ) ;
#59629 = CARTESIAN_POINT ( 'NONE',  ( -1.417322834645668772, -0.1870078740157479769, 0.3641732283464567677 ) ) ;
#59630 = CARTESIAN_POINT ( 'NONE',  ( 0.2362204724409451007, -0.4091458600556402980, -1.351706036745406792 ) ) ;
#59631 = CARTESIAN_POINT ( 'NONE',  ( 2.058019426306444633, 1.301092492065848649, -0.4123476441529899117 ) ) ;
#59632 = CARTESIAN_POINT ( 'NONE',  ( -0.2867679344610365999, 0.2867679344610364889, -0.1692913385826771144 ) ) ;
#59633 = CARTESIAN_POINT ( 'NONE',  ( 0.1049643490035304799, -0.3917322834645669549, -2.532152230971127960 ) ) ;
#59634 = CARTESIAN_POINT ( 'NONE',  ( -0.5118110236220466680, 0.2952755905511811885, 0.000000000000000000 ) ) ;
#59635 = CARTESIAN_POINT ( 'NONE',  ( 1.660104986876641320, -0.05778040916215522460, 0.4822834645669289988 ) ) ;
#59636 = CARTESIAN_POINT ( 'NONE',  ( -0.3996062992125984925, -0.1070741851644056858, -0.1227034120734908501 ) ) ;
#59638 = DIRECTION ( 'NONE',  ( 1.049727191138618079E-16, -0.5150380749100549327, 0.8571673007021117785 ) ) ;
#59637 = CARTESIAN_POINT ( 'NONE',  ( -1.358267716535432434, 0.1660481256975883668, -0.3530559997133364547 ) ) ;
#59639 = CARTESIAN_POINT ( 'NONE',  ( -1.443569553805773564, -0.6046776061558807314, 0.2411417322834647770 ) ) ;
#59640 = CARTESIAN_POINT ( 'NONE',  ( -0.5839895013123351797, 0.2952755905511810774, -0.1292274648535930714 ) ) ;
#59641 = CARTESIAN_POINT ( 'NONE',  ( -9.674558042662122972E-17, 0.3949938075777409963, -2.596456692913385655 ) ) ;
#59642 = CARTESIAN_POINT ( 'NONE',  ( 0.6561679790026253567, 0.1283753931104748280, 0.1820866141732283561 ) ) ;
#59643 = CARTESIAN_POINT ( 'NONE',  ( -0.2867679344610366554, 0.2867679344610365444, -0.1043307086614174151 ) ) ;
#59644 = AXIS2_PLACEMENT_3D ( 'NONE', #67244, #73138, #52923 ) ;
#59645 = CARTESIAN_POINT ( 'NONE',  ( 0.4068241469816281097, -0.004921259842519576551, 0.3153832671262227771 ) ) ;
#59646 = CARTESIAN_POINT ( 'NONE',  ( 1.482939632545932307, -0.004921259842519870586, -0.3153832671262229437 ) ) ;
#59647 = CARTESIAN_POINT ( 'NONE',  ( 1.122047244094488860, 0.1660481256975885056, 0.3530559997133364547 ) ) ;
#59648 = CARTESIAN_POINT ( 'NONE',  ( 0.1246719160104994284, 0.1771653543307087075, -0.09757992244046823083 ) ) ;
#59649 = CARTESIAN_POINT ( 'NONE',  ( -0.3917322834645670104, -7.196005306013484475E-17, -2.078740157480314821 ) ) ;
#59650 = CARTESIAN_POINT ( 'NONE',  ( -1.141732283464566011, 0.2952755905511811885, 0.000000000000000000 ) ) ;
#59651 = CARTESIAN_POINT ( 'NONE',  ( -0.01968503937007793844, -0.4536011799217367080, 0.2665933059059888421 ) ) ;
#59652 = CARTESIAN_POINT ( 'NONE',  ( -1.167979002624671470, -0.004921259842519576551, 0.3153832671262227771 ) ) ;
#59653 = CARTESIAN_POINT ( 'NONE',  ( 0.3458507752293908943, 0.3458507752293908943, -0.3720472440944882497 ) ) ;
#59654 = CARTESIAN_POINT ( 'NONE',  ( -0.2952755905511803003, -0.4536011799217368745, -0.2665933059059886201 ) ) ;
#59655 = CARTESIAN_POINT ( 'NONE',  ( 0.4468661194710661366, 1.378074791477804206, -1.523351412176985775 ) ) ;
#59656 = CARTESIAN_POINT ( 'NONE',  ( -0.1443569553805765515, -0.4281496062992127816, -0.4176697321401328100 ) ) ;
#59657 = DIRECTION ( 'NONE',  ( -0.7071067811865437980, 8.659560562354978464E-17, -0.7071067811865512365 ) ) ;
#59658 = CARTESIAN_POINT ( 'NONE',  ( 0.7152230971128614723, -0.2845877964562161244, -0.3641732283464567121 ) ) ;
#59659 = CARTESIAN_POINT ( 'NONE',  ( -0.2362204724409442680, -0.1870078740157480601, -0.3641732283464567677 ) ) ;
#59660 = CARTESIAN_POINT ( 'NONE',  ( -0.1902887139107604098, 0.2952755905511810774, -0.1292274648535930714 ) ) ;
#59661 = CARTESIAN_POINT ( 'NONE',  ( -1.581364829396324945, -0.3162353388693405765, 0.4822834645669290543 ) ) ;
#59662 = CARTESIAN_POINT ( 'NONE',  ( -1.154855643044618851, 0.1283753931104748280, 0.1820866141732283561 ) ) ;
#59663 = DIRECTION ( 'NONE',  ( 0.000000000000000000, 1.000000000000000000, 0.000000000000000000 ) ) ;
#59664 = CARTESIAN_POINT ( 'NONE',  ( 0.4790026246719168435, -0.3162353388693409650, -0.4822834645669289433 ) ) ;
#59665 = ORIENTED_EDGE ( 'NONE', *, *, #10585, .F. ) ;
#59666 = CARTESIAN_POINT ( 'NONE',  ( -0.9711286089238838626, 0.2306618581243847221, -0.2411417322834647770 ) ) ;
#59667 = CARTESIAN_POINT ( 'NONE',  ( 4.893765752498283308E-17, -0.3996062992125985480, -1.572834645669291431 ) ) ;
#59668 = CARTESIAN_POINT ( 'NONE',  ( -0.1049643490035302024, -0.3917322834645671215, -2.833989501312335957 ) ) ;
#59669 = CARTESIAN_POINT ( 'NONE',  ( -0.1968503937007867743, -0.5511811023622047445, 6.969142054262312111E-17 ) ) ;
#59670 = CARTESIAN_POINT ( 'NONE',  ( -1.371391076115484609, -0.6692913385826771977, 0.1292274648535927661 ) ) ;
#59671 = CARTESIAN_POINT ( 'NONE',  ( -1.620734908136482577, 0.1771653543307087630, 0.09757992244046791164 ) ) ;
#59672 = CARTESIAN_POINT ( 'NONE',  ( -3.908412016409563261, 1.506477424558240630, -0.4736547731912041925 ) ) ;
#59673 = CARTESIAN_POINT ( 'NONE',  ( -0.6758530183727028406, -0.5511811023622048555, -0.09757992244046775898 ) ) ;
#59674 = CARTESIAN_POINT ( 'NONE',  ( -0.5411721830064186722, -2.191421614605370878E-15, 0.4445507791589071167 ) ) ;
#59675 = CARTESIAN_POINT ( 'NONE',  ( 1.003937007874016185, 0.1660481256975883668, -0.3530559997133364547 ) ) ;
#59676 = CARTESIAN_POINT ( 'NONE',  ( 0.3996062992125986590, -0.1070741851644053111, 0.04593175853018371946 ) ) ;
#59677 = CARTESIAN_POINT ( 'NONE',  ( 0.3392501089628018884, -0.1958661417322833942, -2.463930076936694746 ) ) ;
#59678 = CARTESIAN_POINT ( 'NONE',  ( -3.846978723397335376, 2.751923335154144556, -0.5314960629921260393 ) ) ;
#59679 = CARTESIAN_POINT ( 'NONE',  ( -1.640419947506561060, -0.4281496062992127816, -0.4176697321401328100 ) ) ;
#59680 = CARTESIAN_POINT ( 'NONE',  ( -1.253280839895012377, -0.05778040916215522460, 0.4822834645669289988 ) ) ;
#59681 = CARTESIAN_POINT ( 'NONE',  ( 1.220472440944882386, -0.6692913385826771977, 8.415575281601705876E-17 ) ) ;
#59682 = CARTESIAN_POINT ( 'NONE',  ( -0.1958661417322836718, 0.3392501089628017219, -2.302493438320210029 ) ) ;
#59683 = CARTESIAN_POINT ( 'NONE',  ( 1.489501312335958172, -0.2845877964562159024, 0.3641732283464567677 ) ) ;
#59684 = EDGE_CURVE ( 'NONE', #42693, #49366, #61590, .T. ) ;
#59685 = CARTESIAN_POINT ( 'NONE',  ( 0.6955380577427828781, -0.4281496062992124485, 0.4176697321401328655 ) ) ;
#59686 = CARTESIAN_POINT ( 'NONE',  ( -0.5774278215223089816, -0.6046776061558807314, 0.2411417322834647770 ) ) ;
#59687 = CARTESIAN_POINT ( 'NONE',  ( -3.909107915504009600, 1.617412091359350823, 0.4678854304693115806 ) ) ;
#59688 = CARTESIAN_POINT ( 'NONE',  ( 3.841955293929017135, 2.753420937170568461, 0.5314960629921260393 ) ) ;
#59689 = CARTESIAN_POINT ( 'NONE',  ( 0.9383202099737536495, -0.2845877964562159024, 0.3641732283464567677 ) ) ;
#59690 = ORIENTED_EDGE ( 'NONE', *, *, #56144, .F. ) ;
#59691 = CARTESIAN_POINT ( 'NONE',  ( -0.1049643490035302301, -0.3917322834645671770, -0.3838775834983745860 ) ) ;
#59692 = VERTEX_POINT ( 'NONE', #48123 ) ;
#59693 = CARTESIAN_POINT ( 'NONE',  ( -0.2755905511811018171, 0.2952755905511811885, 0.000000000000000000 ) ) ;
#59694 = CARTESIAN_POINT ( 'NONE',  ( 1.187664041994751285, -0.3162353388693409650, -0.4822834645669289433 ) ) ;
#59695 = CARTESIAN_POINT ( 'NONE',  ( 0.4068241469816281097, 0.05413385826771666132, 0.4176697321401328100 ) ) ;
#59696 = CARTESIAN_POINT ( 'NONE',  ( -0.2362204724409440182, -0.1870078740157479769, 0.3641732283464567677 ) ) ;
#59697 = VECTOR ( 'NONE', #22151, 39.37007874015748143 ) ;
#59698 = CARTESIAN_POINT ( 'NONE',  ( 1.358267716535433323, 0.1660481256975885056, 0.3530559997133364547 ) ) ;
#59699 = CARTESIAN_POINT ( 'NONE',  ( -1.069553805774277722, -0.6692913385826773087, -0.1292274648535924053 ) ) ;
#59700 = CARTESIAN_POINT ( 'NONE',  ( -0.04593175853018302557, -0.6692913385826773087, -0.1292274648535924053 ) ) ;
#59701 = CARTESIAN_POINT ( 'NONE',  ( -0.7283464566929126471, 0.1660481256975883668, -0.3530559997133364547 ) ) ;
#59702 = CARTESIAN_POINT ( 'NONE',  ( 1.187664041994751285, -0.3162353388693409650, -0.4822834645669289433 ) ) ;
#59703 = CARTESIAN_POINT ( 'NONE',  ( 0.8333333333333340365, 0.2952755905511810774, -0.1292274648535930714 ) ) ;
#59704 = CARTESIAN_POINT ( 'NONE',  ( 1.377952755905512472, 0.2952755905511811885, 0.000000000000000000 ) ) ;
#59705 = CARTESIAN_POINT ( 'NONE',  ( -0.3917322834645670104, -7.196005306013484475E-17, -0.6614173228346454936 ) ) ;
#59706 = CARTESIAN_POINT ( 'NONE',  ( 0.01968503937007957949, -0.4536011799217368745, -0.2665933059059886201 ) ) ;
#59707 = VERTEX_POINT ( 'NONE', #80558 ) ;
#59708 = CARTESIAN_POINT ( 'NONE',  ( -0.3420746716998661618, 0.1974969037888702206, -1.128608923884514503 ) ) ;
#59709 = ORIENTED_EDGE ( 'NONE', *, *, #67626, .F. ) ;
#59710 = CARTESIAN_POINT ( 'NONE',  ( -0.3608923884514428360, -0.5511811023622048555, -0.09757992244046775898 ) ) ;
#59711 = CARTESIAN_POINT ( 'NONE',  ( 0.1640419947506569498, -0.3162353388693409650, -0.4822834645669289433 ) ) ;
#59712 = CARTESIAN_POINT ( 'NONE',  ( -1.397575190283976365, 1.210854158823307269, 0.3443910704722475402 ) ) ;
#59713 = CARTESIAN_POINT ( 'NONE',  ( -0.3543307086614165824, -0.6692913385826771977, 8.415575281601705876E-17 ) ) ;
#59714 = CARTESIAN_POINT ( 'NONE',  ( -0.4068241469816267775, 0.05413385826771626580, -0.4176697321401330321 ) ) ;
#59715 = CARTESIAN_POINT ( 'NONE',  ( -0.7939632545931750718, -0.05778040916215560624, -0.4822834645669293319 ) ) ;
#59716 = CARTESIAN_POINT ( 'NONE',  ( -0.9973753280839886548, -0.6046776061558809534, -0.2411417322834644161 ) ) ;
#59717 = AXIS2_PLACEMENT_3D ( 'NONE', #43839, #36715, #30402 ) ;
#59718 = CARTESIAN_POINT ( 'NONE',  ( 1.397637795275591177, 0.07958543189024071263, -0.2665933059059888421 ) ) ;
#59719 = CARTESIAN_POINT ( 'NONE',  ( 1.614173228346456712, 0.4410134679336843999, 0.1372047244094478646 ) ) ;
#59720 = CARTESIAN_POINT ( 'NONE',  ( -0.2362204724409447953, -0.4091458600556404646, -2.742782152230971437 ) ) ;
#59721 = CARTESIAN_POINT ( 'NONE',  ( 0.4855643044619428750, -0.004921259842519576551, 0.3153832671262227771 ) ) ;
#59722 = CARTESIAN_POINT ( 'NONE',  ( 0.4790026246719168435, -0.3162353388693409650, -0.4822834645669289433 ) ) ;
#59723 = CARTESIAN_POINT ( 'NONE',  ( 0.4330708661417329575, 0.2952755905511811885, 0.000000000000000000 ) ) ;
#59724 = EDGE_LOOP ( 'NONE', ( #27610, #20889, #54952, #34884 ) ) ;
#59725 = CARTESIAN_POINT ( 'NONE',  ( -0.3996062992125986035, -0.1070741851644056997, -1.305774278215223072 ) ) ;
#59726 = CARTESIAN_POINT ( 'NONE',  ( -0.5627669687126057863, 0.02791078216816347476, -0.4328096321851898631 ) ) ;
#59727 = CARTESIAN_POINT ( 'NONE',  ( 4.893765752498283308E-17, -0.3996062992125985480, -1.257874015748031260 ) ) ;
#59728 = CARTESIAN_POINT ( 'NONE',  ( -0.1070741851644056997, 0.3996062992125984925, -0.5557742782152230721 ) ) ;
#59729 = CARTESIAN_POINT ( 'NONE',  ( -0.6167979002624665030, 0.05413385826771666132, 0.4176697321401328100 ) ) ;
#59730 = CARTESIAN_POINT ( 'NONE',  ( -0.4724409448818898682, -8.678599364036362592E-17, -0.03937007874015747977 ) ) ;
#59731 =( BOUNDED_CURVE ( )  B_SPLINE_CURVE ( 2, ( #27960, #48144, #72997, #48556, #73841, #9030, #3542, #61613, #74253, #40591, #34703, #9855, #15772, #79747, #22482, #23301, #16595, #66273, #2300, #59944, #28791, #16181, #53619, #10276, #60365, #48971, #2712, #54454, #28373, #8612, #34282, #22064, #67107, #73422, #9438, #35109, #35525, #61187, #54875, #80581, #75331, #23145, #17275, #74098, #36193, #3388, #29869, #55531, #61864, #43308, #74930, #69425, #54722, #80428, #37431, #4205, #22738, #42903, #29464, #82066, #67784, #49638, #68598, #62695, #81240, #23556, #61453, #49225, #75745, #10122, #10537, #11357, #69006, #30282, #3801, #10938, #74513, #48814, #16860, #36595, #17678, #37015, #42498, #35785, #81660, #24379, #5035, #62273, #4610, #29052, #30703, #55122, #80831, #56367, #50051, #68199, #18086, #55947, #16444, #43721, #23971, #11778, #48398, #42089, #19307, #12590, #38248, #64762, #800, #26463, #13847, #83289, #56771, #6262, #50867, #51693, #25612, #32352, #51275, #20152, #63104, #25201, #70235, #13425, #44959, #63926, #63516, #76158, #7101 ),
 .UNSPECIFIED., .F., .F. ) 
 B_SPLINE_CURVE_WITH_KNOTS ( ( 3, 2, 2, 2, 2, 2, 2, 2, 2, 2, 2, 2, 2, 2, 2, 2, 2, 2, 2, 2, 2, 2, 2, 2, 2, 2, 2, 2, 2, 2, 2, 2, 2, 2, 2, 2, 2, 2, 2, 2, 2, 2, 2, 2, 2, 2, 2, 2, 2, 2, 2, 2, 2, 2, 2, 2, 2, 2, 2, 2, 2, 2, 2, 2, 3 ),
 ( 0.6881378855240343206, 0.6916666666666666519, 0.6958333333333333037, 0.6999999999999999556, 0.7041666666666667185, 0.7083333333333333703, 0.7125000000000000222, 0.7166666666666666741, 0.7208333333333333259, 0.7249999999999999778, 0.7291666666666666297, 0.7333333333333332815, 0.7375000000000000444, 0.7416666666666666963, 0.7458333333333333481, 0.7500000000000000000, 0.7541666666666666519, 0.7583333333333333037, 0.7624999999999999556, 0.7666666666666667185, 0.7708333333333333703, 0.7750000000000000222, 0.7791666666666666741, 0.7833333333333333259, 0.7874999999999999778, 0.7916666666666666297, 0.7958333333333332815, 0.8000000000000000444, 0.8041666666666666963, 0.8083333333333333481, 0.8125000000000000000, 0.8166666666666666519, 0.8208333333333333037, 0.8249999999999999556, 0.8291666666666667185, 0.8333333333333333703, 0.8375000000000000222, 0.8416666666666666741, 0.8458333333333333259, 0.8499999999999999778, 0.8541666666666666297, 0.8583333333333332815, 0.8625000000000000444, 0.8666666666666666963, 0.8708333333333333481, 0.8750000000000000000, 0.8791666666666666519, 0.8833333333333333037, 0.8874999999999999556, 0.8916666666666667185, 0.8958333333333333703, 0.9000000000000000222, 0.9041666666666666741, 0.9083333333333333259, 0.9124999999999999778, 0.9166666666666666297, 0.9208333333333332815, 0.9250000000000000444, 0.9291666666666666963, 0.9333333333333333481, 0.9375000000000000000, 0.9416666666666666519, 0.9458333333333333037, 0.9499999999999999556, 0.9506378855240344983 ),
 .UNSPECIFIED. ) 
 CURVE ( )  GEOMETRIC_REPRESENTATION_ITEM ( )  RATIONAL_B_SPLINE_CURVE ( ( 0.9911642120908021880, 0.9711423276059405474, 1.000000000000000000, 0.9659258262890683122, 1.000000000000000000, 0.9659258262890683122, 1.000000000000000000, 0.9659258262890683122, 1.000000000000000000, 0.9659258262890683122, 1.000000000000000000, 0.9659258262890683122, 1.000000000000000000, 0.9659258262890683122, 1.000000000000000000, 0.9659258262890683122, 1.000000000000000000, 0.9659258262890683122, 1.000000000000000000, 0.9659258262890683122, 1.000000000000000000, 0.9659258262890683122, 1.000000000000000000, 0.9659258262890683122, 1.000000000000000000, 0.9659258262890683122, 1.000000000000000000, 0.9659258262890683122, 1.000000000000000000, 0.9659258262890683122, 1.000000000000000000, 0.9659258262890683122, 1.000000000000000000, 0.9659258262890683122, 1.000000000000000000, 0.9659258262890683122, 1.000000000000000000, 0.9659258262890683122, 1.000000000000000000, 0.9659258262890683122, 1.000000000000000000, 0.9659258262890683122, 1.000000000000000000, 0.9659258262890683122, 1.000000000000000000, 0.9659258262890683122, 1.000000000000000000, 0.9659258262890683122, 1.000000000000000000, 0.9659258262890683122, 1.000000000000000000, 0.9659258262890683122, 1.000000000000000000, 0.9659258262890683122, 1.000000000000000000, 0.9659258262890683122, 1.000000000000000000, 0.9659258262890683122, 1.000000000000000000, 0.9659258262890683122, 1.000000000000000000, 0.9659258262890683122, 1.000000000000000000, 0.9659258262890683122, 1.000000000000000000, 0.9659258262890683122, 1.000000000000000000, 0.9659258262890683122, 1.000000000000000000, 0.9659258262890683122, 1.000000000000000000, 0.9659258262890683122, 1.000000000000000000, 0.9659258262890683122, 1.000000000000000000, 0.9659258262890683122, 1.000000000000000000, 0.9659258262890683122, 1.000000000000000000, 0.9659258262890683122, 1.000000000000000000, 0.9659258262890683122, 1.000000000000000000, 0.9659258262890683122, 1.000000000000000000, 0.9659258262890683122, 1.000000000000000000, 0.9659258262890683122, 1.000000000000000000, 0.9659258262890683122, 1.000000000000000000, 0.9659258262890683122, 1.000000000000000000, 0.9659258262890683122, 1.000000000000000000, 0.9659258262890683122, 1.000000000000000000, 0.9659258262890683122, 1.000000000000000000, 0.9659258262890683122, 1.000000000000000000, 0.9659258262890683122, 1.000000000000000000, 0.9659258262890683122, 1.000000000000000000, 0.9659258262890683122, 1.000000000000000000, 0.9659258262890683122, 1.000000000000000000, 0.9659258262890683122, 1.000000000000000000, 0.9659258262890683122, 1.000000000000000000, 0.9659258262890683122, 1.000000000000000000, 0.9659258262890683122, 1.000000000000000000, 0.9659258262890683122, 1.000000000000000000, 0.9659258262890683122, 1.000000000000000000, 0.9659258262890683122, 1.000000000000000000, 0.9659258262890683122, 1.000000000000000000, 0.9659258262890683122, 1.000000000000000000, 0.9947834986831260995, 0.9911642120907998565 ) ) 
 REPRESENTATION_ITEM ( '' )  );
#59732 = CARTESIAN_POINT ( 'NONE',  ( 0.1049643490035304938, -0.3917322834645669549, -2.217191601049868677 ) ) ;
#59733 = CARTESIAN_POINT ( 'NONE',  ( 1.640419947506562393, -0.4281496062992124485, 0.4176697321401328655 ) ) ;
#59734 = CARTESIAN_POINT ( 'NONE',  ( 0.7480314960629927956, -0.6692913385826771977, 8.415575281601705876E-17 ) ) ;
#59735 = CARTESIAN_POINT ( 'NONE',  ( 1.141732283464567788, -0.6692913385826771977, 8.415575281601705876E-17 ) ) ;
#59736 = CARTESIAN_POINT ( 'NONE',  ( -0.2821522309711278487, -0.5511811023622048555, -0.09757992244046775898 ) ) ;
#59737 = CARTESIAN_POINT ( 'NONE',  ( 0.4986876640419954376, 0.2306618581243848609, 0.2411417322834645549 ) ) ;
#59738 = CARTESIAN_POINT ( 'NONE',  ( 0.4091458600556404646, -0.2362204724409448231, -1.756561679790026309 ) ) ;
#59739 = CARTESIAN_POINT ( 'NONE',  ( -0.05249343832020911260, 0.1283753931104748280, 0.1820866141732283561 ) ) ;
#59740 = CARTESIAN_POINT ( 'NONE',  ( -0.2230971128608915943, -0.4281496062992127816, -0.4176697321401328100 ) ) ;
#59741 = CARTESIAN_POINT ( 'NONE',  ( -0.3949938075777411073, 0.1058382717557497660, -1.211942257217847763 ) ) ;
#59742 = CARTESIAN_POINT ( 'NONE',  ( -1.548556430446193399, 0.2306618581243848609, 0.2411417322834645549 ) ) ;
#59743 = CARTESIAN_POINT ( 'NONE',  ( -0.03280839895013062252, -0.5511811023622046335, 0.09757992244046803654 ) ) ;
#59744 = CARTESIAN_POINT ( 'NONE',  ( 1.646981627296588035, -0.2845877964562159024, 0.3641732283464567677 ) ) ;
#59745 = CARTESIAN_POINT ( 'NONE',  ( -0.8595800524934373854, -0.3162353388693409650, -0.4822834645669289433 ) ) ;
#59746 = CARTESIAN_POINT ( 'NONE',  ( -0.7545931758530176614, -0.5511811023622048555, -0.09757992244046775898 ) ) ;
#59747 = CARTESIAN_POINT ( 'NONE',  ( 1.600415083108465142, 1.509172534626478823, -0.1324231768467331039 ) ) ;
#59748 = CARTESIAN_POINT ( 'NONE',  ( -0.8792650918635160906, 0.05413385826771626580, -0.4176697321401330321 ) ) ;
#59749 = CARTESIAN_POINT ( 'NONE',  ( -0.5577427821522301654, -0.3162353388693405765, 0.4822834645669290543 ) ) ;
#59750 = CARTESIAN_POINT ( 'NONE',  ( 0.03937007874015833325, -0.6692913385826771977, 8.415575281601705876E-17 ) ) ;
#59751 = CARTESIAN_POINT ( 'NONE',  ( 0.2925321140481932369, 0.2925321140481932369, -2.576771653543307394 ) ) ;
#59752 = CARTESIAN_POINT ( 'NONE',  ( 0.3392501089628018329, -0.1958661417322834497, -2.074783833824459744 ) ) ;
#59753 = CARTESIAN_POINT ( 'NONE',  ( -2.114058874202352278, 1.379859446982304894, -0.4477348144951664444 ) ) ;
#59754 = CARTESIAN_POINT ( 'NONE',  ( 0.9251968503937015864, 0.07958543189024071263, -0.2665933059059888421 ) ) ;
#59755 = CARTESIAN_POINT ( 'NONE',  ( 1.548556430446194954, -0.6046776061558807314, 0.2411417322834647770 ) ) ;
#59756 = CARTESIAN_POINT ( 'NONE',  ( -1.417322834645668772, -0.1870078740157479769, 0.3641732283464567677 ) ) ;
#59757 = CARTESIAN_POINT ( 'NONE',  ( 1.069553805774278832, 0.2952755905511810774, -0.1292274648535930714 ) ) ;
#59758 = CARTESIAN_POINT ( 'NONE',  ( -1.122047244094487306, -0.4536011799217367080, 0.2665933059059888421 ) ) ;
#59759 = CARTESIAN_POINT ( 'NONE',  ( -0.6496062992125976043, -0.5400638737290844871, 0.3530559997133364547 ) ) ;
#59760 = CARTESIAN_POINT ( 'NONE',  ( 0.1509186351706045259, -0.08942795157528024563, -0.3641732283464568787 ) ) ;
#59761 = CARTESIAN_POINT ( 'NONE',  ( 1.614173228346457378, 0.2753471884572478157, 0.1372047244094478646 ) ) ;
#59762 = CARTESIAN_POINT ( 'NONE',  ( 1.259842519685040019, -0.1870078740157479769, 0.3641732283464567677 ) ) ;
#59763 = AXIS2_PLACEMENT_3D ( 'NONE', #19569, #45228, #6942 ) ;
#59764 = CARTESIAN_POINT ( 'NONE',  ( 0.4002624671916016896, -0.05778040916215522460, 0.4822834645669289988 ) ) ;
#59765 = CARTESIAN_POINT ( 'NONE',  ( -0.3460692066303957537, -0.1998031496062994405, -0.4442257217847768724 ) ) ;
#59766 = CARTESIAN_POINT ( 'NONE',  ( -0.7480314960629914633, 0.2952755905511811885, 0.000000000000000000 ) ) ;
#59767 = CARTESIAN_POINT ( 'NONE',  ( -9.594673741351313045E-17, 0.3917322834645670104, -1.501968503937008093 ) ) ;
#59768 = CARTESIAN_POINT ( 'NONE',  ( 0.8267716535433077274, 0.1771653543307087630, 0.000000000000000000 ) ) ;
#59769 = CARTESIAN_POINT ( 'NONE',  ( 0.3280839895013130669, -0.4281496062992127816, -0.4176697321401328100 ) ) ;
#59770 = CARTESIAN_POINT ( 'NONE',  ( -0.09186351706036663400, -0.4281496062992124485, 0.4176697321401328655 ) ) ;
#59771 = CARTESIAN_POINT ( 'NONE',  ( -0.1706036745406816491, -0.004921259842519870586, -0.3153832671262229437 ) ) ;
#59772 = DIRECTION ( 'NONE',  ( 0.000000000000000000, 0.000000000000000000, -1.000000000000000000 ) ) ;
#59773 = CARTESIAN_POINT ( 'NONE',  ( 0.1246719160104994284, 0.1771653543307087075, -0.09757992244046823083 ) ) ;
#59774 = CARTESIAN_POINT ( 'NONE',  ( 0.6561679790026253567, -0.6046776061558809534, -0.2411417322834644161 ) ) ;
#59775 = CARTESIAN_POINT ( 'NONE',  ( -0.6955380577427815458, -0.3690944881889765550, -0.3153832671262227771 ) ) ;
#59777 = CARTESIAN_POINT ( 'NONE',  ( -0.1070741851644051862, -0.3996062992125986590, -0.7788713910761155823 ) ) ;
#59776 = CIRCLE ( 'NONE', #8726, 3.937007874015748143 ) ;
#59778 = CARTESIAN_POINT ( 'NONE',  ( -0.9448818897637790704, -0.1870078740157480879, -0.4822834645669291653 ) ) ;
#59779 = DIRECTION ( 'NONE',  ( 0.5773502691896306160, -0.5773502691896320593, 0.5773502691896146288 ) ) ;
#59780 = ORIENTED_EDGE ( 'NONE', *, *, #12082, .T. ) ;
#59781 = CARTESIAN_POINT ( 'NONE',  ( -0.9908136482939626788, -0.5511811023622048555, -0.09757992244046775898 ) ) ;
#59782 = CARTESIAN_POINT ( 'NONE',  ( -0.1902887139107604098, -0.6692913385826771977, 0.1292274648535927661 ) ) ;
#59783 = CARTESIAN_POINT ( 'NONE',  ( -1.313877454013331780, 0.2929341459200028863, 0.7983292792091805090 ) ) ;
#59784 = CARTESIAN_POINT ( 'NONE',  ( -0.7086614173228339419, -0.1870078740157479769, 0.4822834645669291653 ) ) ;
#59785 = DIRECTION ( 'NONE',  ( -0.000000000000000000, 1.000000000000000000, -0.000000000000000000 ) ) ;
#59787 = CARTESIAN_POINT ( 'NONE',  ( 1.010498687664042716, 0.05413385826771626580, -0.4176697321401330321 ) ) ;
#59786 = CARTESIAN_POINT ( 'NONE',  ( 1.092353285368624860, -4.408777212815537393E-16, -0.4445507791589063395 ) ) ;
#59788 = CARTESIAN_POINT ( 'NONE',  ( 0.9514435695538062676, -0.3162353388693409650, -0.4822834645669289433 ) ) ;
#59789 = CARTESIAN_POINT ( 'NONE',  ( -0.2867679344610366554, 0.2867679344610365444, -2.688976377952755570 ) ) ;
#59790 = DIRECTION ( 'NONE',  ( 0.000000000000000000, 0.000000000000000000, -1.000000000000000000 ) ) ;
#59791 = CARTESIAN_POINT ( 'NONE',  ( -1.404199475065615932, 0.05413385826771666132, 0.4176697321401328100 ) ) ;
#59792 = B_SPLINE_CURVE_WITH_KNOTS ( 'NONE', 3,
 ( #66656, #14896, #27925, #66237, #59492, #15311, #26677, #27089, #40974, #78460, #27507, #20785, #33416, #53164, #52332, #53583, #64985, #39722, #34245, #65414, #58657, #21200, #20368, #46020, #7751, #40556 ),
 .UNSPECIFIED., .F., .F.,
 ( 4, 2, 2, 2, 2, 2, 2, 2, 2, 2, 2, 2, 4 ),
 ( 0.000000000000000000, 0.002383993240623330772, 0.003575989860934996808, 0.004767986481246663279, 0.007151979721869992750, 0.008343976342181655750, 0.009535972962493319618, 0.01072796958280498696, 0.01191996620311664215, 0.01430395944373995254, 0.01549595606405161120, 0.01668795268436326987, 0.01907194592498655597 ),
 .UNSPECIFIED. ) ;
#59793 = CARTESIAN_POINT ( 'NONE',  ( 0.3460692066303959757, -0.1998031496062991907, -0.5774278215223097588 ) ) ;
#59794 = ORIENTED_EDGE ( 'NONE', *, *, #21401, .T. ) ;
#59795 = CARTESIAN_POINT ( 'NONE',  ( -0.7152230971128602510, -0.2845877964562159024, 0.3641732283464567677 ) ) ;
#59796 = CARTESIAN_POINT ( 'NONE',  ( 0.3917322834645670104, 2.398668435337828261E-17, -2.157480314960630086 ) ) ;
#59797 = VERTEX_POINT ( 'NONE', #34683 ) ;
#59798 = CARTESIAN_POINT ( 'NONE',  ( 0.7677165354330716118, -0.5400638737290844871, 0.3530559997133364547 ) ) ;
#59799 = CARTESIAN_POINT ( 'NONE',  ( 0.02624671916010564918, 0.2306618581243848609, 0.2411417322834645549 ) ) ;
#59800 = CARTESIAN_POINT ( 'NONE',  ( -0.4855643044619415427, 0.05413385826771626580, -0.4176697321401330321 ) ) ;
#59801 = CARTESIAN_POINT ( 'NONE',  ( 1.351706036745407680, 0.05413385826771666132, 0.4176697321401328100 ) ) ;
#59802 = CARTESIAN_POINT ( 'NONE',  ( -0.8792650918635160906, -0.3690944881889763329, 0.3153832671262228327 ) ) ;
#59803 = CARTESIAN_POINT ( 'NONE',  ( -0.4724409448818898682, -8.678599364036362592E-17, -2.005905511811023612 ) ) ;
#59804 = CARTESIAN_POINT ( 'NONE',  ( 0.8858267716535438430, 0.1660481256975885056, 0.3530559997133364547 ) ) ;
#59805 = CARTESIAN_POINT ( 'NONE',  ( 0.3805774278215230400, -0.004921259842519870586, -0.3153832671262229437 ) ) ;
#59806 = CARTESIAN_POINT ( 'NONE',  ( -0.5446194225721777693, -0.05778040916215522460, 0.4822834645669289988 ) ) ;
#59807 = CARTESIAN_POINT ( 'NONE',  ( 0.2867679344610365999, -0.2867679344610365999, -1.438300894191914425 ) ) ;
#59808 = CARTESIAN_POINT ( 'NONE',  ( -1.292650918635170010, 0.2952755905511810774, -0.1292274648535930714 ) ) ;
#59809 = DIRECTION ( 'NONE',  ( -3.491481338843132961E-15, -0.000000000000000000, 1.000000000000000000 ) ) ;
#59810 = CARTESIAN_POINT ( 'NONE',  ( 1.456692913385827515, -0.6692913385826771977, 8.415575281601705876E-17 ) ) ;
#59811 = CARTESIAN_POINT ( 'NONE',  ( 1.233595800524935227, 0.1283753931104746893, -0.1820866141732285504 ) ) ;
#59812 = ORIENTED_EDGE ( 'NONE', *, *, #36661, .F. ) ;
#59813 = CARTESIAN_POINT ( 'NONE',  ( 4.797336870675656522E-17, -0.3917322834645670659, -2.910124302658479767 ) ) ;
#59814 = CARTESIAN_POINT ( 'NONE',  ( -0.09842519685039295696, -0.5400638737290844871, 0.3530559997133364547 ) ) ;
#59815 = EDGE_LOOP ( 'NONE', ( #31927, #13414, #12184, #4519 ) ) ;
#59816 = CARTESIAN_POINT ( 'NONE',  ( 1.017060367454068581, -0.08942795157528024563, -0.3641732283464568787 ) ) ;
#59817 = CARTESIAN_POINT ( 'NONE',  ( -1.095800524934382292, -0.05778040916215522460, 0.4822834645669289988 ) ) ;
#59818 = CARTESIAN_POINT ( 'NONE',  ( 1.062992125984252745, -0.6692913385826771977, 8.415575281601705876E-17 ) ) ;
#59819 = CARTESIAN_POINT ( 'NONE',  ( 0.7020997375328090762, -0.05778040916215560624, -0.4822834645669293319 ) ) ;
#59820 = CARTESIAN_POINT ( 'NONE',  ( 0.2624671916010504757, -0.6046776061558809534, -0.2411417322834644161 ) ) ;
#59821 = CARTESIAN_POINT ( 'NONE',  ( -0.5249343832020990641, 0.2306618581243848609, 0.2411417322834645549 ) ) ;
#59822 = CARTESIAN_POINT ( 'NONE',  ( -0.3917322834645671215, 0.1049643490035301469, -1.849737532808399143 ) ) ;
#59823 = CARTESIAN_POINT ( 'NONE',  ( -1.384514435695537005, 0.2952755905511811885, 0.1292274648535926551 ) ) ;
#59824 = CARTESIAN_POINT ( 'NONE',  ( -0.4527559055118102749, -0.5400638737290845981, -0.3530559997133363437 ) ) ;
#59825 = CARTESIAN_POINT ( 'NONE',  ( -0.5118110236220466680, -0.6692913385826771977, 8.415575281601705876E-17 ) ) ;
#59826 = CARTESIAN_POINT ( 'NONE',  ( -0.5839895013123351797, -0.5511811023622046335, 0.09757992244046803654 ) ) ;
#59827 = DIRECTION ( 'NONE',  ( 0.000000000000000000, 0.000000000000000000, 1.000000000000000000 ) ) ;
#59828 = LINE ( 'NONE', #2182, #61209 ) ;
#59829 = EDGE_CURVE ( 'NONE', #13254, #29189, #47704, .T. ) ;
#59830 = CARTESIAN_POINT ( 'NONE',  ( -0.3608923884514428360, -0.6692913385826773087, -0.1292274648535924053 ) ) ;
#59831 = DIRECTION ( 'NONE',  ( 0.000000000000000000, 0.000000000000000000, 1.000000000000000000 ) ) ;
#59832 = CARTESIAN_POINT ( 'NONE',  ( 0.6430446194225728496, 0.05413385826771666132, 0.4176697321401328100 ) ) ;
#59833 = CARTESIAN_POINT ( 'NONE',  ( -0.3996062992125986035, -0.1070741851644056997, -1.935695538057742526 ) ) ;
#59834 = CARTESIAN_POINT ( 'NONE',  ( 0.000000000000000000, 1.724409448818897905, 0.000000000000000000 ) ) ;
#59835 = EDGE_CURVE ( 'NONE', #56483, #14101, #5278, .T. ) ;
#59836 = CARTESIAN_POINT ( 'NONE',  ( -0.06561679790026180015, 0.05413385826771666132, 0.4176697321401328100 ) ) ;
#59838 = CARTESIAN_POINT ( 'NONE',  ( 0.6962418744208975774, 2.409604939980833412E-17, -0.3464511005275205946 ) ) ;
#59837 = CARTESIAN_POINT ( 'NONE',  ( 1.069553805774278832, 0.1771653543307087075, -0.09757992244046823083 ) ) ;
#59839 = CARTESIAN_POINT ( 'NONE',  ( 0.1265901696524989462, 0.4724409448818897572, -0.7001312335958002064 ) ) ;
#59840 = CARTESIAN_POINT ( 'NONE',  ( 1.332020997375329197, -0.2845877964562159024, 0.3641732283464567677 ) ) ;
#59841 = CARTESIAN_POINT ( 'NONE',  ( 1.128608923884514947, 0.2306618581243848609, 0.2411417322834645549 ) ) ;
#59842 = AXIS2_PLACEMENT_3D ( 'NONE', #52859, #46548, #72246 ) ;
#59843 = CARTESIAN_POINT ( 'NONE',  ( -0.3949938075777411073, 0.1058382717557497660, -0.1095800524934383707 ) ) ;
#59844 = CARTESIAN_POINT ( 'NONE',  ( -0.2887139107611542133, 0.2306618581243848609, 0.2411417322834645549 ) ) ;
#59845 = CARTESIAN_POINT ( 'NONE',  ( -1.528871391076114250, -0.6692913385826771977, 0.1292274648535927661 ) ) ;
#59846 = CARTESIAN_POINT ( 'NONE',  ( -1.660104986876639543, -0.05778040916215560624, -0.4822834645669293319 ) ) ;
#59847 = CARTESIAN_POINT ( 'NONE',  ( 0.01968503937007930540, 0.1660481256975885056, 0.3530559997133364547 ) ) ;
#59848 = CARTESIAN_POINT ( 'NONE',  ( 0.1974969037888704704, 0.3420746716998660508, -0.3786089238845145033 ) ) ;
#59849 = CARTESIAN_POINT ( 'NONE',  ( 1.410761154855643795, -0.05778040916215560624, -0.4822834645669293319 ) ) ;
#59850 = CARTESIAN_POINT ( 'NONE',  ( 0.4199475065616803948, -0.6046776061558809534, -0.2411417322834644161 ) ) ;
#59851 = CARTESIAN_POINT ( 'NONE',  ( 0.7152230971128616943, -0.08942795157527998196, 0.3641732283464567121 ) ) ;
#59852 = CARTESIAN_POINT ( 'NONE',  ( -0.4705509983644061700, 1.475022898150550654, -1.018614094479749932 ) ) ;
#59853 = CARTESIAN_POINT ( 'NONE',  ( 0.4658792650918641698, -0.08942795157528024563, -0.3641732283464568787 ) ) ;
#59854 = CARTESIAN_POINT ( 'NONE',  ( -1.043307086614172929, 0.1012011053420775880, -0.2882089793578257453 ) ) ;
#59855 = CARTESIAN_POINT ( 'NONE',  ( 4.893765752498283308E-17, -0.3996062992125985480, -1.257874015748031482 ) ) ;
#59856 = CARTESIAN_POINT ( 'NONE',  ( 0.8661417322834653598, -0.1870078740157479769, 0.4822834645669291653 ) ) ;
#59857 = ADVANCED_FACE ( 'NONE', ( #12313 ), #75472, .F. ) ;
#59858 = CARTESIAN_POINT ( 'NONE',  ( 0.1958661417322836440, -0.3392501089628017219, -0.8713910761154854967 ) ) ;
#59859 = CARTESIAN_POINT ( 'NONE',  ( -0.2362204724409447953, -0.4091458600556404646, -0.4573490813648293796 ) ) ;
#59860 = DIRECTION ( 'NONE',  ( 0.000000000000000000, 0.000000000000000000, 1.000000000000000000 ) ) ;
#59861 = CARTESIAN_POINT ( 'NONE',  ( -0.1115485564304456306, 0.1771653543307087075, -0.09757992244046823083 ) ) ;
#59862 = CARTESIAN_POINT ( 'NONE',  ( 0.3280839895013130669, -0.4281496062992127816, -0.4176697321401328100 ) ) ;
#59863 = CARTESIAN_POINT ( 'NONE',  ( 1.325459317585302665, -0.3690944881889763329, 0.3153832671262228327 ) ) ;
#59864 = CARTESIAN_POINT ( 'NONE',  ( -0.9711286089238838626, -0.5023911411419708095, 0.1820866141732285504 ) ) ;
#59865 = CARTESIAN_POINT ( 'NONE',  ( -0.9186351706036736120, 0.2306618581243848609, 0.2411417322834645549 ) ) ;
#59866 = CARTESIAN_POINT ( 'NONE',  ( -1.660104986876639543, -0.05778040916215560624, -0.4822834645669293319 ) ) ;
#59867 = CARTESIAN_POINT ( 'NONE',  ( 0.3280839895013130669, -0.4281496062992127816, -0.4176697321401328100 ) ) ;
#59868 = CARTESIAN_POINT ( 'NONE',  ( 1.410761154855643795, -0.05778040916215560624, -0.4822834645669293319 ) ) ;
#59869 = CARTESIAN_POINT ( 'NONE',  ( 0.1938976377952755792, 0.1938976377952755792, -0.3740157480314971750 ) ) ;
#59870 = CARTESIAN_POINT ( 'NONE',  ( 0.3871391076115492380, -0.05778040916215560624, -0.4822834645669293319 ) ) ;
#59871 = CARTESIAN_POINT ( 'NONE',  ( 5.785732909357575061E-17, -0.4724409448818898682, -2.832677165354331006 ) ) ;
#59872 = CARTESIAN_POINT ( 'NONE',  ( 1.660104986876641320, -0.05778040916215522460, 0.4822834645669289988 ) ) ;
#59873 = CARTESIAN_POINT ( 'NONE',  ( 1.312335958005250269, -0.6046776061558807314, 0.2411417322834647770 ) ) ;
#59874 = CARTESIAN_POINT ( 'NONE',  ( -1.581364829396324945, -0.2845877964562159024, 0.3641732283464567677 ) ) ;
#59875 = CARTESIAN_POINT ( 'NONE',  ( 1.338582677165355062, -0.1870078740157479769, 0.3641732283464567677 ) ) ;
#59876 = CARTESIAN_POINT ( 'NONE',  ( -1.200787401574802349, -0.4536011799217367080, 0.2665933059059888421 ) ) ;
#59877 = CARTESIAN_POINT ( 'NONE',  ( -0.8398950131233585692, 0.1283753931104748280, 0.1820866141732283561 ) ) ;
#59878 = CARTESIAN_POINT ( 'NONE',  ( -1.313877454013331780, 0.2755905511811023723, 0.9174237673981568975 ) ) ;
#59879 = CARTESIAN_POINT ( 'NONE',  ( 0.6036745406824153282, -0.5023911411419708095, 0.1820866141732285504 ) ) ;
#59880 = CARTESIAN_POINT ( 'NONE',  ( -0.08530183727034056085, -0.3162353388693405765, 0.4822834645669290543 ) ) ;
#59881 = CARTESIAN_POINT ( 'NONE',  ( 1.102362204724410155, -0.1870078740157479769, 0.4822834645669291653 ) ) ;
#59882 = CARTESIAN_POINT ( 'NONE',  ( 0.06561679790026316017, -0.4281496062992124485, 0.4176697321401328655 ) ) ;
#59883 = CARTESIAN_POINT ( 'NONE',  ( 0.2624671916010504757, -0.5023911411419708095, -0.1820866141732282451 ) ) ;
#59884 = CARTESIAN_POINT ( 'NONE',  ( 1.227034120734908917, -0.6692913385826771977, 0.1292274648535927661 ) ) ;
#59885 = LINE ( 'NONE', #14469, #7039 ) ;
#59886 = CARTESIAN_POINT ( 'NONE',  ( -1.036745406824146176, 0.05413385826771626580, -0.4176697321401330321 ) ) ;
#59887 = CARTESIAN_POINT ( 'NONE',  ( 0.2925321140481932369, 0.2925321140481932369, -0.6102362204724408601 ) ) ;
#59888 = CARTESIAN_POINT ( 'NONE',  ( 0.000000000000000000, 1.724409448818897461, 0.000000000000000000 ) ) ;
#59890 = VECTOR ( 'NONE', #67032, 39.37007874015748854 ) ;
#59889 = CARTESIAN_POINT ( 'NONE',  ( -1.023622047244093558, -0.1870078740157479769, 0.4822834645669291653 ) ) ;
#59891 = EDGE_CURVE ( 'NONE', #6920, #2295, #51973, .T. ) ;
#59892 = CARTESIAN_POINT ( 'NONE',  ( -0.1771653543307080136, -0.5400638737290844871, 0.3530559997133364547 ) ) ;
#59893 = CARTESIAN_POINT ( 'NONE',  ( 0.1998031496062994405, -0.3460692066303958092, -2.454068241469816058 ) ) ;
#59894 = CARTESIAN_POINT ( 'NONE',  ( -0.3420746716998661618, 0.1974969037888702206, -2.388451443569553856 ) ) ;
#59895 = ORIENTED_EDGE ( 'NONE', *, *, #57575, .T. ) ;
#59896 = CARTESIAN_POINT ( 'NONE',  ( -0.3392501089628019995, 0.1958661417322832277, -1.120734908136482799 ) ) ;
#59897 = DIRECTION ( 'NONE',  ( -1.000000000000000000, 0.000000000000000000, 0.000000000000000000 ) ) ;
#59898 = CARTESIAN_POINT ( 'NONE',  ( -1.272965879265091305, -0.3690944881889763329, 0.3153832671262228327 ) ) ;
#59899 = CARTESIAN_POINT ( 'NONE',  ( 0.1049643490035304938, -0.3917322834645669549, -1.022309711286088829 ) ) ;
#59900 = CARTESIAN_POINT ( 'NONE',  ( -1.594488188976377563, -0.5400638737290844871, 0.3530559997133364547 ) ) ;
#59901 = CARTESIAN_POINT ( 'NONE',  ( 0.1974969037888706092, -0.3420746716998660508, -2.845800524934383624 ) ) ;
#59902 = EDGE_CURVE ( 'NONE', #34982, #53393, #29942, .T. ) ;
#59903 = CARTESIAN_POINT ( 'NONE',  ( -0.1181102362204717315, -0.6692913385826771977, 8.415575281601705876E-17 ) ) ;
#59904 = CARTESIAN_POINT ( 'NONE',  ( -0.5052493438320203589, -0.5511811023622046335, 0.09757992244046803654 ) ) ;
#59905 = CARTESIAN_POINT ( 'NONE',  ( 1.049868766404200127, -0.6046776061558809534, -0.2411417322834644161 ) ) ;
#59906 = CARTESIAN_POINT ( 'NONE',  ( 0.2493438320209980519, -0.4281496062992127816, -0.4176697321401328100 ) ) ;
#59907 = CARTESIAN_POINT ( 'NONE',  ( -0.3049517105654738214, -2.191421614605370878E-15, 0.4445507791589071167 ) ) ;
#59908 = CARTESIAN_POINT ( 'NONE',  ( 0.1998031496062992740, 0.3460692066303959757, -2.506561679790026087 ) ) ;
#59909 = CARTESIAN_POINT ( 'NONE',  ( 0.1049643490035304799, -0.3917322834645670104, -1.341882832842206774 ) ) ;
#59910 = CARTESIAN_POINT ( 'NONE',  ( 1.069553805774278832, 0.2952755905511810774, -0.1292274648535930714 ) ) ;
#59911 = CARTESIAN_POINT ( 'NONE',  ( 0.1574803149606306130, -0.1870078740157479769, 0.4822834645669291653 ) ) ;
#59912 = CARTESIAN_POINT ( 'NONE',  ( -1.220472440944881054, -0.6692913385826771977, 8.415575281601705876E-17 ) ) ;
#59913 = CARTESIAN_POINT ( 'NONE',  ( 1.601049868766404982, 0.2306618581243848609, 0.2411417322834645549 ) ) ;
#59914 = CARTESIAN_POINT ( 'NONE',  ( 0.9776902887139113929, -0.6692913385826773087, -0.1292274648535924053 ) ) ;
#59915 = CARTESIAN_POINT ( 'NONE',  ( -0.1049643490035307020, 0.3917322834645669549, -0.5636482939632546652 ) ) ;
#59916 = CARTESIAN_POINT ( 'NONE',  ( 0.01968503937007930540, 0.1660481256975885056, 0.3530559997133364547 ) ) ;
#59917 = CARTESIAN_POINT ( 'NONE',  ( 0.6561679790026253567, -0.6046776061558809534, -0.2411417322834644161 ) ) ;
#59918 = CARTESIAN_POINT ( 'NONE',  ( -0.1640419947506553400, -0.05778040916215560624, -0.4822834645669293319 ) ) ;
#59919 = CARTESIAN_POINT ( 'NONE',  ( 0.6758530183727039509, -0.5511811023622046335, 0.09757992244046803654 ) ) ;
#59920 = CARTESIAN_POINT ( 'NONE',  ( -1.135170603674539924, -0.6692913385826771977, 0.1292274648535927661 ) ) ;
#59921 = CARTESIAN_POINT ( 'NONE',  ( -1.614173228346456268, -0.6692913385826771977, 8.415575281601705876E-17 ) ) ;
#59922 = CARTESIAN_POINT ( 'NONE',  ( 0.7217847769028878924, -0.4281496062992127816, -0.4176697321401328100 ) ) ;
#59923 = DIRECTION ( 'NONE',  ( 0.000000000000000000, 0.000000000000000000, 1.000000000000000000 ) ) ;
#59924 = CARTESIAN_POINT ( 'NONE',  ( -9.594673741351313045E-17, 0.3917322834645670104, -2.039370078740157410 ) ) ;
#59925 = ORIENTED_EDGE ( 'NONE', *, *, #34284, .F. ) ;
#59926 = CARTESIAN_POINT ( 'NONE',  ( 0.3996062992125986035, 2.446882876249141962E-17, -0.2755905511811024278 ) ) ;
#59927 = VERTEX_POINT ( 'NONE', #11494 ) ;
#59928 = CARTESIAN_POINT ( 'NONE',  ( 0.9383202099737538715, -0.05778040916215560624, -0.4822834645669293319 ) ) ;
#59929 = CARTESIAN_POINT ( 'NONE',  ( 0.3477690288713918276, 0.1771653543307087630, 0.09757992244046791164 ) ) ;
#59930 = AXIS2_PLACEMENT_3D ( 'NONE', #43556, #54540, #73928 ) ;
#59931 = AXIS2_PLACEMENT_3D ( 'NONE', #47736, #16194, #28386 ) ;
#59932 = CYLINDRICAL_SURFACE ( 'NONE', #31702, 0.07874015748031495954 ) ;
#59933 = CARTESIAN_POINT ( 'NONE',  ( 0.5314960629920920665, 2.729657717072965450, 3.237502119437994264 ) ) ;
#59934 = CARTESIAN_POINT ( 'NONE',  ( 0.3983403474834781299, 0.03178304480585100733, -1.929133858267716661 ) ) ;
#59935 = CARTESIAN_POINT ( 'NONE',  ( 0.3392501089628018329, 0.1958661417322835607, -1.160761154855643129 ) ) ;
#59936 = CARTESIAN_POINT ( 'NONE',  ( -0.3948464311378463432, -0.01987007963522063533, -1.929133858267717994 ) ) ;
#59937 = CARTESIAN_POINT ( 'NONE',  ( -0.4199475065616791736, 0.2306618581243847221, -0.2411417322834647770 ) ) ;
#59938 = CARTESIAN_POINT ( 'NONE',  ( 1.220472440944882386, -0.6692913385826771977, 8.415575281601705876E-17 ) ) ;
#59939 = ORIENTED_EDGE ( 'NONE', *, *, #61021, .T. ) ;
#59940 = CARTESIAN_POINT ( 'NONE',  ( -1.384514435695537005, 0.2952755905511811885, 0.1292274648535926551 ) ) ;
#59941 = CARTESIAN_POINT ( 'NONE',  ( -1.111574668186677162, 1.088302645458066875, -0.1536776283199748350 ) ) ;
#59942 = LENGTH_MEASURE_WITH_UNIT ( LENGTH_MEASURE( 0.02539999999999999897 ), #634 );
#59943 = CARTESIAN_POINT ( 'NONE',  ( 1.561679790026247350, -0.004921259842519870586, -0.3153832671262229437 ) ) ;
#59944 = CARTESIAN_POINT ( 'NONE',  ( 0.1070741851644054637, -0.3996062992125984925, -2.051837270341207109 ) ) ;
#59945 = CARTESIAN_POINT ( 'NONE',  ( -1.515748031496062076, -0.4536011799217367080, 0.2665933059059888421 ) ) ;
#59946 = CARTESIAN_POINT ( 'NONE',  ( -1.410761154855641575, -0.3162353388693409650, -0.4822834645669289433 ) ) ;
#59947 = CARTESIAN_POINT ( 'NONE',  ( 0.1968503937007881344, -0.6692913385826771977, 8.415575281601705876E-17 ) ) ;
#59948 = VECTOR ( 'NONE', #38812, 39.37007874015748143 ) ;
#59949 = VERTEX_POINT ( 'NONE', #43855 ) ;
#59951 = CARTESIAN_POINT ( 'NONE',  ( -2.362204724409448620, 1.724409448818897461, -2.474278114140802984E-14 ) ) ;
#59950 = CARTESIAN_POINT ( 'NONE',  ( 1.601049868766404982, -0.6046776061558809534, -0.2411417322834644161 ) ) ;
#59952 = CARTESIAN_POINT ( 'NONE',  ( -0.5839895013123351797, 0.1771653543307087075, -0.09757992244046823083 ) ) ;
#59953 = CARTESIAN_POINT ( 'NONE',  ( 0.9514435695538062676, -0.3162353388693409650, -0.4822834645669289433 ) ) ;
#59954 = CARTESIAN_POINT ( 'NONE',  ( -1.515748031496062076, 0.1660481256975883668, -0.3530559997133364547 ) ) ;
#59955 = CARTESIAN_POINT ( 'NONE',  ( -0.1049643490035306742, 0.3917322834645668994, -1.346437377131546764 ) ) ;
#59956 = CARTESIAN_POINT ( 'NONE',  ( -0.9908136482939626788, -0.5511811023622048555, -0.09757992244046775898 ) ) ;
#59957 = CARTESIAN_POINT ( 'NONE',  ( -1.509186351706035767, -0.3690944881889763329, 0.3153832671262228327 ) ) ;
#59958 = CARTESIAN_POINT ( 'NONE',  ( 0.3392501089628018884, -0.1958661417322834220, -1.134514435695538115 ) ) ;
#59959 = CARTESIAN_POINT ( 'NONE',  ( 0.5905511811023629321, -0.6692913385826771977, 8.415575281601705876E-17 ) ) ;
#59960 = CARTESIAN_POINT ( 'NONE',  ( -0.9973753280839886548, 0.1283753931104748280, 0.1820866141732283561 ) ) ;
#59961 = CARTESIAN_POINT ( 'NONE',  ( -0.2296587926509179312, -0.2845877964562161244, -0.3641732283464567121 ) ) ;
#59962 = CARTESIAN_POINT ( 'NONE',  ( -0.1509186351706028884, -0.05778040916215522460, 0.4822834645669289988 ) ) ;
#59963 = CARTESIAN_POINT ( 'NONE',  ( -1.548556430446193399, -0.5023911411419708095, -0.1820866141732282451 ) ) ;
#59964 = CARTESIAN_POINT ( 'NONE',  ( 0.1049643490035303967, 0.3917322834645670659, 0.009823203903200209905 ) ) ;
#59965 = CARTESIAN_POINT ( 'NONE',  ( 0.5511811023622054106, -0.1870078740157480879, -0.4822834645669291653 ) ) ;
#59966 = CARTESIAN_POINT ( 'NONE',  ( 0.4056338187708066201, 5.789745203009502317E-16, 0.3627989612356145588 ) ) ;
#59967 = CARTESIAN_POINT ( 'NONE',  ( -0.1265901696524993347, 0.4724409448818895907, -1.658136482939632117 ) ) ;
#59968 = CARTESIAN_POINT ( 'NONE',  ( -0.7283464566929126471, 0.1660481256975883668, -0.3530559997133364547 ) ) ;
#59969 = CARTESIAN_POINT ( 'NONE',  ( -0.3346456692913377662, -0.4536011799217367080, 0.2665933059059888421 ) ) ;
#59970 = ADVANCED_FACE ( 'NONE', ( #70371 ), #60113, .F. ) ;
#59971 = CARTESIAN_POINT ( 'NONE',  ( -1.187664041994749731, -0.3162353388693405765, 0.4822834645669290543 ) ) ;
#59972 = CARTESIAN_POINT ( 'NONE',  ( 0.4921259842519691285, -0.4536011799217368745, -0.2665933059059886201 ) ) ;
#59973 = CARTESIAN_POINT ( 'NONE',  ( -0.8661417322834640276, -0.1870078740157480601, -0.3641732283464567677 ) ) ;
#59974 = CARTESIAN_POINT ( 'NONE',  ( -1.253280839895012377, -0.05778040916215522460, 0.4822834645669289988 ) ) ;
#59975 = CARTESIAN_POINT ( 'NONE',  ( -1.601049868766403650, -0.6046776061558807314, 0.2411417322834647770 ) ) ;
#59976 = CARTESIAN_POINT ( 'NONE',  ( 1.227034120734908917, 0.2952755905511810774, -0.1292274648535930714 ) ) ;
#59977 = LINE ( 'NONE', #15380, #9847 ) ;
#59978 = CARTESIAN_POINT ( 'NONE',  ( 0.6889763779527566800, -0.4536011799217367080, 0.2665933059059888421 ) ) ;
#59979 = CARTESIAN_POINT ( 'NONE',  ( 0.2821522309711292364, 0.2952755905511810774, -0.1292274648535930714 ) ) ;
#59980 = EDGE_CURVE ( 'NONE', #11477, #54726, #6842, .T. ) ;
#59981 = CARTESIAN_POINT ( 'NONE',  ( 0.5419760673063064305, 1.535433070866141447, -0.4915354330708657793 ) ) ;
#59982 = CARTESIAN_POINT ( 'NONE',  ( 1.528871391076116026, -0.5511811023622048555, -0.09757992244046775898 ) ) ;
#59983 = VERTEX_POINT ( 'NONE', #56087 ) ;
#59984 = CARTESIAN_POINT ( 'NONE',  ( -0.2891555358219909388, -0.2891555358219912164, 0.1791338582677165503 ) ) ;
#59985 = CARTESIAN_POINT ( 'NONE',  ( -1.325459317585300889, -0.004921259842519576551, 0.3153832671262227771 ) ) ;
#59986 = CARTESIAN_POINT ( 'NONE',  ( -0.2952755905511803003, -0.5400638737290845981, -0.3530559997133363437 ) ) ;
#59987 = CARTESIAN_POINT ( 'NONE',  ( 0.4658792650918640033, -0.3162353388693405765, 0.4822834645669290543 ) ) ;
#59988 = AXIS2_PLACEMENT_3D ( 'NONE', #79439, #41121, #65567 ) ;
#59989 = CARTESIAN_POINT ( 'NONE',  ( -1.561679790026246017, -0.004921259842519576551, 0.3153832671262227771 ) ) ;
#59990 = CARTESIAN_POINT ( 'NONE',  ( -9.787531504996566615E-17, 0.3996062992125985480, -1.651574803149606474 ) ) ;
#59991 = CARTESIAN_POINT ( 'NONE',  ( -1.246719160104986512, 0.05413385826771666132, 0.4176697321401328100 ) ) ;
#59992 = AXIS2_PLACEMENT_3D ( 'NONE', #51805, #82984, #50969 ) ;
#59993 = AXIS2_PLACEMENT_3D ( 'NONE', #56673, #44854, #51177 ) ;
#59994 = CARTESIAN_POINT ( 'NONE',  ( 0.3215223097112867578, -0.3162353388693409650, -0.4822834645669289433 ) ) ;
#59995 = CARTESIAN_POINT ( 'NONE',  ( 0.01312335958005323398, -0.4281496062992127816, -0.4176697321401328100 ) ) ;
#59996 = CARTESIAN_POINT ( 'NONE',  ( 1.115485564304462551, 0.05413385826771666132, 0.4176697321401328100 ) ) ;
#59997 = CARTESIAN_POINT ( 'NONE',  ( 0.1998031496062994128, -0.3460692066303957537, -0.9560367454068241511 ) ) ;
#59998 = CARTESIAN_POINT ( 'NONE',  ( 0.2925321140481932369, 0.2925321140481932369, -1.240157480314960647 ) ) ;
#59999 = CARTESIAN_POINT ( 'NONE',  ( -0.2891555358219908833, -0.2891555358219912164, -0.5314960629921261503 ) ) ;
#60000 =( REPRESENTATION_RELATIONSHIP ('NONE','NONE', #79348, #76132 ) REPRESENTATION_RELATIONSHIP_WITH_TRANSFORMATION ( #15770 )SHAPE_REPRESENTATION_RELATIONSHIP( ) );
#60001 = CARTESIAN_POINT ( 'NONE',  ( -0.1958661417322836718, 0.3392501089628017219, -0.005249343832020950465 ) ) ;
#60002 = CARTESIAN_POINT ( 'NONE',  ( 0.07874015748031558404, -0.1870078740157480601, -0.3641732283464567677 ) ) ;
#60003 = CARTESIAN_POINT ( 'NONE',  ( -0.1181102362204717315, 0.2952755905511811885, 0.000000000000000000 ) ) ;
#60004 = CARTESIAN_POINT ( 'NONE',  ( 0.8005249343832027131, 0.05413385826771666132, 0.4176697321401328100 ) ) ;
#60005 = CARTESIAN_POINT ( 'NONE',  ( 0.1974969037888704704, 0.3420746716998660508, -1.638451443569553634 ) ) ;
#60006 = CARTESIAN_POINT ( 'NONE',  ( -0.03937007874015669567, 0.1771653543307087630, 0.000000000000000000 ) ) ;
#60007 = CARTESIAN_POINT ( 'NONE',  ( -1.318897637795274802, 0.1660481256975885056, 0.3530559997133364547 ) ) ;
#60008 = CARTESIAN_POINT ( 'NONE',  ( 1.601049868766404982, 0.2306618581243848609, 0.2411417322834645549 ) ) ;
#60009 = CARTESIAN_POINT ( 'NONE',  ( 0.3458507752293908943, -0.3458507752293908943, -2.145669291338581974 ) ) ;
#60010 = CARTESIAN_POINT ( 'NONE',  ( 0.3857315817373125899, -0.06912221444358807032, -2.755905511811024056 ) ) ;
#60011 = AXIS2_PLACEMENT_3D ( 'NONE', #65133, #7469, #32293 ) ;
#60012 = EDGE_LOOP ( 'NONE', ( #7227, #72780 ) ) ;
#60013 = ORIENTED_EDGE ( 'NONE', *, *, #38729, .T. ) ;
#60014 = CARTESIAN_POINT ( 'NONE',  ( 1.535433070866142335, -0.6692913385826771977, 8.415575281601705876E-17 ) ) ;
#60015 = CARTESIAN_POINT ( 'NONE',  ( 1.594488188976378673, 0.07958543189024085140, 0.2665933059059887866 ) ) ;
#60017 = CARTESIAN_POINT ( 'NONE',  ( -0.9908136482939626788, 0.2952755905511811885, 0.1292274648535926551 ) ) ;
#60016 = CARTESIAN_POINT ( 'NONE',  ( -1.076115485564303809, -0.5023911411419708095, -0.1820866141732282451 ) ) ;
#60018 = CARTESIAN_POINT ( 'NONE',  ( 0.1958661417322834497, 0.3392501089628018329, -2.586594857446507412 ) ) ;
#60019 = CARTESIAN_POINT ( 'NONE',  ( -2.795275590551183686, 1.299212598425198095, -1.990688069879260956E-16 ) ) ;
#60020 = CARTESIAN_POINT ( 'NONE',  ( 1.417322834645670104, -0.1870078740157480879, -0.4822834645669291653 ) ) ;
#60021 = CARTESIAN_POINT ( 'NONE',  ( -1.699475065616797398, 0.2952755905511811885, 0.1292274648535926551 ) ) ;
#60022 = CARTESIAN_POINT ( 'NONE',  ( -0.2559055118110230564, 0.1660481256975883668, -0.3530559997133364547 ) ) ;
#60023 = CARTESIAN_POINT ( 'NONE',  ( -0.3346456692913377662, -0.5400638737290844871, 0.3530559997133364547 ) ) ;
#60024 = CARTESIAN_POINT ( 'NONE',  ( -1.233595800524933894, -0.6046776061558809534, -0.2411417322834644161 ) ) ;
#60025 = CARTESIAN_POINT ( 'NONE',  ( 0.1958661417322834497, 0.3392501089628018329, -2.744075172407137497 ) ) ;
#60026 = CARTESIAN_POINT ( 'NONE',  ( 0.7545931758530188826, -0.6692913385826771977, 0.1292274648535927661 ) ) ;
#60027 = CARTESIAN_POINT ( 'NONE',  ( -0.1049643490035307020, 0.3917322834645669549, -1.730971128608923992 ) ) ;
#60028 = CARTESIAN_POINT ( 'NONE',  ( -1.364829396325458521, -0.5023911411419708095, 0.1820866141732285504 ) ) ;
#60029 = ORIENTED_EDGE ( 'NONE', *, *, #46673, .T. ) ;
#60030 = CARTESIAN_POINT ( 'NONE',  ( -0.1058382717557503211, 0.3949938075777409408, -2.211286089238845065 ) ) ;
#60031 = ORIENTED_EDGE ( 'NONE', *, *, #28480, .T. ) ;
#60032 = LINE ( 'NONE', #8280, #30081 ) ;
#60033 = CARTESIAN_POINT ( 'NONE',  ( -1.587926509186350810, -0.4281496062992124485, 0.4176697321401328655 ) ) ;
#60034 = CARTESIAN_POINT ( 'NONE',  ( -1.345144356955379816, -0.3162353388693405765, 0.4822834645669290543 ) ) ;
#60035 = CARTESIAN_POINT ( 'NONE',  ( 0.3996062992125986590, -0.1070741851644053111, -0.5839895013123358458 ) ) ;
#60036 = CARTESIAN_POINT ( 'NONE',  ( -1.601049868766403650, -0.6046776061558807314, 0.2411417322834647770 ) ) ;
#60037 = CARTESIAN_POINT ( 'NONE',  ( 1.827151616986590010, 2.742788234388597868, -0.5314960629921260393 ) ) ;
#60038 = CARTESIAN_POINT ( 'NONE',  ( 0.4593175853018380828, 0.05413385826771626580, -0.4176697321401330321 ) ) ;
#60039 = CARTESIAN_POINT ( 'NONE',  ( -8.478666411000228475E-17, -0.3992723400743185547, -2.755905511811022723 ) ) ;
#60040 = CARTESIAN_POINT ( 'NONE',  ( 0.2867679344610365999, -0.2867679344610365444, 0.1318897637795274913 ) ) ;
#60041 = CARTESIAN_POINT ( 'NONE',  ( -0.08530183727034056085, -0.2845877964562159024, 0.3641732283464567677 ) ) ;
#60042 = CARTESIAN_POINT ( 'NONE',  ( -0.6561679790026240244, -0.5023911411419708095, 0.1820866141732285504 ) ) ;
#60043 = CARTESIAN_POINT ( 'NONE',  ( -1.246719160104985846, -0.4281496062992127816, -0.4176697321401328100 ) ) ;
#60044 = CARTESIAN_POINT ( 'NONE',  ( 0.8005249343832027131, 0.05413385826771666132, 0.4176697321401328100 ) ) ;
#60045 = CARTESIAN_POINT ( 'NONE',  ( -0.9317585301837263412, -0.4281496062992127816, -0.4176697321401328100 ) ) ;
#60046 = CARTESIAN_POINT ( 'NONE',  ( 0.3917322834645670104, -0.1049643490035303411, 0.05380577427821527092 ) ) ;
#60047 = VERTEX_POINT ( 'NONE', #64062 ) ;
#60048 = CARTESIAN_POINT ( 'NONE',  ( -1.305774278215222184, 0.2952755905511811885, 0.1292274648535926551 ) ) ;
#60049 = CARTESIAN_POINT ( 'NONE',  ( -1.607611548556429737, -0.5511811023622046335, 0.09757992244046803654 ) ) ;
#60050 =( NAMED_UNIT ( * ) PLANE_ANGLE_UNIT ( ) SI_UNIT ( $, .RADIAN. ) );
#60051 = CARTESIAN_POINT ( 'NONE',  ( 0.2362204724409451007, -0.4091458600556402980, -1.194225721784776928 ) ) ;
#60052 = FACE_OUTER_BOUND ( 'NONE', #69750, .T. ) ;
#60053 = CARTESIAN_POINT ( 'NONE',  ( -0.1049643490035302024, -0.3917322834645671215, -0.6942257217847765949 ) ) ;
#60054 = VECTOR ( 'NONE', #80491, 39.37007874015748143 ) ;
#60055 = CARTESIAN_POINT ( 'NONE',  ( -9.594673741351313045E-17, 0.3917322834645670104, -2.289370078740157410 ) ) ;
#60056 = CARTESIAN_POINT ( 'NONE',  ( -0.3740157480314953431, 0.1660481256975885056, 0.3530559997133364547 ) ) ;
#60057 = CARTESIAN_POINT ( 'NONE',  ( -1.305774278215222184, 0.1771653543307087630, 0.09757992244046791164 ) ) ;
#60058 = AXIS2_PLACEMENT_3D ( 'NONE', #61881, #67803, #47592 ) ;
#60059 = AXIS2_PLACEMENT_3D ( 'NONE', #21021, #7567, #33239 ) ;
#60060 = CARTESIAN_POINT ( 'NONE',  ( 0.3996062992125985480, 2.446882876249141654E-17, -0.03740157480314963701 ) ) ;
#60062 = DIRECTION ( 'NONE',  ( 1.000000000000000000, 0.000000000000000000, 0.000000000000000000 ) ) ;
#60061 = CARTESIAN_POINT ( 'NONE',  ( -0.7461015469959760837, 2.202998601756388730, -0.5309055118110235227 ) ) ;
#60063 = CARTESIAN_POINT ( 'NONE',  ( -1.555118110236219930, 0.1660481256975885056, 0.3530559997133364547 ) ) ;
#60064 = CARTESIAN_POINT ( 'NONE',  ( -0.3740157480314953431, -0.5400638737290845981, -0.3530559997133363437 ) ) ;
#60065 = CARTESIAN_POINT ( 'NONE',  ( -0.1958661417322836440, 0.3392501089628016664, 0.2218040926847262562 ) ) ;
#60066 = CARTESIAN_POINT ( 'NONE',  ( 0.5052493438320215802, 0.1771653543307087630, 0.09757992244046791164 ) ) ;
#60067 = DIRECTION ( 'NONE',  ( -1.000000000000000000, -2.312964634635742464E-16, 0.000000000000000000 ) ) ;
#60068 = CARTESIAN_POINT ( 'NONE',  ( 0.3280839895013130669, -0.3690944881889765550, -0.3153832671262227771 ) ) ;
#60069 = CARTESIAN_POINT ( 'NONE',  ( 1.128608923884514947, 0.1283753931104748280, 0.1820866141732283561 ) ) ;
#60070 = CARTESIAN_POINT ( 'NONE',  ( 1.154855643044620184, 0.2306618581243847221, -0.2411417322834647770 ) ) ;
#60071 = CARTESIAN_POINT ( 'NONE',  ( -0.3412073490813641308, 0.1283753931104746893, -0.1820866141732285504 ) ) ;
#60072 = CARTESIAN_POINT ( 'NONE',  ( -0.3917322834645669549, -0.1049643490035306603, -2.085301837270341352 ) ) ;
#60073 = CARTESIAN_POINT ( 'NONE',  ( -1.233595800524933894, -0.6046776061558809534, -0.2411417322834644161 ) ) ;
#60074 = CARTESIAN_POINT ( 'NONE',  ( -0.1246719160104980823, 0.1771653543307087630, 0.09757992244046791164 ) ) ;
#60075 = CARTESIAN_POINT ( 'NONE',  ( -1.187664041994749731, -0.2845877964562159024, 0.3641732283464567677 ) ) ;
#60076 = CARTESIAN_POINT ( 'NONE',  ( 0.4091458600556404646, -0.2362204724409448231, -0.4967191601049869010 ) ) ;
#60077 = CARTESIAN_POINT ( 'NONE',  ( -0.7283464566929126471, -0.4536011799217367080, 0.2665933059059888421 ) ) ;
#60078 = CARTESIAN_POINT ( 'NONE',  ( 0.1273213304869930951, 0.000000000000000000, -1.680969278250197707 ) ) ;
#60079 = EDGE_CURVE ( 'NONE', #24482, #31528, #49349, .T. ) ;
#60080 = CARTESIAN_POINT ( 'NONE',  ( -0.1049868766404193215, -0.6046776061558807314, 0.2411417322834647770 ) ) ;
#60081 = CARTESIAN_POINT ( 'NONE',  ( 1.653543307086614789, -0.1870078740157479769, 0.3641732283464567677 ) ) ;
#60082 = CARTESIAN_POINT ( 'NONE',  ( 0.3740157480314966754, 0.07958543189024071263, -0.2665933059059888421 ) ) ;
#60083 = CARTESIAN_POINT ( 'NONE',  ( -0.4133858267716528645, 0.07958543189024071263, -0.2665933059059888421 ) ) ;
#60084 = CARTESIAN_POINT ( 'NONE',  ( -0.3280839895013117347, 0.05413385826771626580, -0.4176697321401330321 ) ) ;
#60085 = CARTESIAN_POINT ( 'NONE',  ( -1.627296587926508442, -0.6046776061558809534, -0.2411417322834644161 ) ) ;
#60086 = CARTESIAN_POINT ( 'NONE',  ( -1.030183727034119867, -0.2845877964562159024, 0.3641732283464567677 ) ) ;
#60087 = DIRECTION ( 'NONE',  ( 1.000000000000000000, -0.000000000000000000, -0.000000000000000000 ) ) ;
#60088 = CARTESIAN_POINT ( 'NONE',  ( 0.4265091863517067594, 0.2952755905511811885, 0.1292274648535926551 ) ) ;
#60089 = ORIENTED_EDGE ( 'NONE', *, *, #59835, .F. ) ;
#60090 = CARTESIAN_POINT ( 'NONE',  ( -0.1070741851644051862, -0.3996062992125986590, -1.408792650918635259 ) ) ;
#60091 = CARTESIAN_POINT ( 'NONE',  ( 0.3503937007874015075, 0.000000000000000000, 0.000000000000000000 ) ) ;
#60092 = CARTESIAN_POINT ( 'NONE',  ( -0.2230971128608915943, -0.3690944881889765550, -0.3153832671262227771 ) ) ;
#60093 = CARTESIAN_POINT ( 'NONE',  ( -0.05249343832020938322, -0.6046776061558809534, -0.2411417322834644161 ) ) ;
#60094 = CARTESIAN_POINT ( 'NONE',  ( -1.607611548556429737, 0.2952755905511810774, -0.1292274648535930714 ) ) ;
#60095 = CARTESIAN_POINT ( 'NONE',  ( -1.535433070866141225, -0.5511811023622047445, 6.969142054262312111E-17 ) ) ;
#60096 = CARTESIAN_POINT ( 'NONE',  ( 1.351706036745407680, 0.05413385826771666132, 0.4176697321401328100 ) ) ;
#60097 =( BOUNDED_SURFACE ( )  B_SPLINE_SURFACE ( 1, 2, ( 
 ( #66133, #21508, #73700, #53482, #72858, #53892, #15206, #9713, #40043, #67379, #61049, #16040, #2574, #79192, #53060, #28651, #34972, #72029, #54311, #47166, #8882, #40867, #2155, #60635, #65729, #14385, #21922, #66549, #34140, #35384, #8062, #33723, #59385, #34558, #72448, #80022, #60224, #28233, #27822, #1743, #79606, #47584, #3399, #29062, #54733, #41283, #27400, #78772, #73278, #8470, #46755, #21096, #59801, #14797, #40454, #15626, #22341, #48001, #41686, #20684, #2986, #66969, #9302, #46336, #81251, #50060, #24389, #81671, #17285, #80438, #23982, #36605, #74108, #48408, #3812, #11787, #55958, #63114, #16454, #10133, #55132, #42099, #67796, #29474, #30292, #17688, #56377, #61464, #29879, #49649, #42913, #22748, #80842, #35797, #23155, #31113, #55541, #48824, #82076, #74525, #62707, #16871, #42508, #75341, #37440, #68210, #75755, #4621, #69434, #69016, #68608, #18097, #43730, #5045, #10547, #30714, #43318, #62283, #11368, #36205, #23566, #10948, #61874, #4215, #49237, #5452, #37025, #74940, #76576, #52122, #32360, #76987, #56781, #31532, #12190, #76168, #7538, #31947, #82480, #58448, #37847, #39089, #18904, #63525, #51702, #13855, #24796, #77830, #64353, #45810, #45393, #19316, #26471, #808, #64770, #57188, #7109, #58022, #13021, #38675, #82890, #83299, #44969, #50464, #70244, #18505, #32779, #70665, #63935, #44554, #20160, #386, #6271, #25621, #6690, #51284, #71508, #44148, #39513, #65202, #69840, #26042, #57608, #5855, #25210, #71090, #50876, #12599, #77404, #19739, #13433, #38258, #73169, #52542, #1233, #34452, #59695, #46654, #47889, #26882, #78251, #20582, #21407, #1640, #41178, #47061, #79089, #14695, #71930, #8368, #60121, #22234, #79917, #73597, #53786, #39941, #14279, #72753, #78671, #59283, #33620, #72347, #46233, #65627, #7958, #66868, #9198, #34871, #15939, #47477, #52956, #40351, #20992, #34034, #2882, #60532, #2472, #53382, #33211, #28131, #15102, #27298, #66030, #2051, #41586, #8779, #67276, #27715, #40758, #66442, #79498, #21813, #15520, #28545, #54201, #58875, #74003, #42402, #68507, #23881, #74836, #30190, #81149, #3291, #55441, #75241, #23464, #55853, #36508, #61354, #10847, #81562, #43217, #49131, #17180, #35689, #68915, #74418, #61773, #10446, #62184, #16763, #4521, #48306, #3708, #75655, #35278, #17585, #29779, #68100, #36102, #11265, #30611, #41994, #10023, #36923, #4114, #42813, #49546, #62600, #56275, #16350, #4942, #81971, #24286, #49958, #17995, #43629, #9609, #60941, #28956, #67688, #54621, #80332, #22647, #29371, #55032, #80739, #23053, #48721, #6585, #44448, #6166, #50366, #25516, #19628, #20052, #31010, #5351, #82380, #5754, #12086, #13329, #51595, #70140, #52017, #69741, #44049, #26357, #69333, #12913, #70985, #32672, #76063, #44858, #18406, #70557, #37743, #25936, #63417, #31424, #38570, #11683, #57086, #82782, #25103, #38982, #58338, #64251, #19210, #700, #32256, #77723, #37340, #76476, #12492, #63828, #83194, #57917, #63013, #77297, #64665, #51181, #56678, #76879, #50776, #281, #18803, #38155, #24697, #31841, #57503, #45289, #7004, #79297, #53588, #21615, #39406, #9407, #29176, #35077, #9820, #73810, #15316, #22452, #35491, #80547, #3095, #60743, #72965, #22859, #28343, #15739, #47693, #16147, #54004, #41794, #2267, #40979, #29583, #71401, #54842, #67075, #79716, #22032, #48520, #67905, #47275, #66661, #74220, #73387, #28759, #67485, #16565, #10242, #27930, #61155, #42210, #3507, #54421, #55246, #80132, #48112, #35913, #61579, #9000, #41393, #3922, #65089, #7427, #34250, #80953, #45705, #13749, #59912, #34672, #60335, #2683, #62822, #56896, #57303, #68321, #42624, #36313, #43026, #49352, #50577, #5564, #24091, #5974, #23678, #81365, #63636, #23268, #50171, #24909, #69948, #29992, #82188, #55655, #24505, #75049, #63224, #17395, #68720, #75867, #48937, #11062, #36720, #62396, #76284, #12303, #18210, #56485, #37959, #43845, #31644, #74638, #30407, #81781, #17799, #37137, #69548, #16981, #31228, #18615, #5156, #10658, #30820, #4734, #11896, #56075, #49761, #61989, #4326, #75461, #43434, #69131, #11482, #37549, #82589 ),
 ( #44258, #46351, #40058, #78369, #64890, #58139, #32062, #7662, #13977, #50986, #33333, #26161, #71208, #51823, #64469, #39634, #19017, #76684, #934, #77527, #13141, #14403, #44665, #70361, #12716, #13551, #51399, #58994, #39207, #45511, #6806, #38376, #508, #26592, #72047, #65745, #8078, #20277, #6392, #64051, #7229, #45086, #25738, #85, #38793, #57722, #77103, #19435, #1350, #27000, #52663, #33741, #65325, #70790, #32477, #19863, #32901, #20701, #83001, #52244, #58569, #25322, #77948, #45927, #71625, #27416, #66151, #74125, #34988, #42116, #53077, #72465, #34157, #78789, #21114, #8488, #9318, #80038, #35400, #40473, #8900, #60652, #79624, #59401, #59818, #14814, #46774, #10150, #34576, #1759, #61065, #2173, #41702, #79209, #27839, #54329, #16471, #53501, #54749, #66986, #48426, #48017, #21941, #29079, #3416, #67395, #21525, #9729, #3002, #15644, #41300, #47184, #2591, #47601, #72876, #15224, #40884, #80455, #66566, #60244, #73295, #28250, #53910, #28668, #22358, #73717, #16056, #22764, #67813, #11800, #69450, #24811, #50074, #55558, #49254, #81267, #36622, #5466, #63128, #37040, #55975, #35816, #62722, #75356, #29490, #3830, #42527, #50478, #11383, #18519, #55149, #48841, #10563, #80860, #23172, #68229, #69032, #56391, #37454, #16888, #68624, #5059, #81687, #61481, #36221, #74542, #61890, #69854, #10964, #4231, #31128, #29895, #18111, #23582, #74956, #30729, #76182, #17302, #56795, #43332, #44162, #24404, #23998, #82495, #42929, #43744, #62300, #4637, #82090, #17704, #75769, #30308, #49666, #32375, #63539, #25637, #46249, #45825, #26060, #19334, #31963, #7556, #71106, #44986, #64369, #45410, #6706, #1249, #31546, #58890, #52557, #33227, #77422, #70684, #44569, #20175, #26488, #5870, #71524, #38691, #403, #58039, #77003, #52139, #57203, #82904, #13449, #51719, #51300, #26898, #25225, #50890, #76590, #19756, #63951, #13870, #39105, #64787, #13038, #18919, #7125, #32797, #78266, #20597, #12205, #58466, #37863, #70260, #12615, #829, #77846, #38273, #39529, #65217, #6288, #57624, #62528, #60138, #15121, #53399, #28564, #7974, #39958, #73187, #40775, #2068, #3308, #65644, #33637, #59300, #2489, #40367, #79936, #28148, #34472, #79106, #27314, #47079, #15537, #60958, #35296, #28973, #9215, #78687, #52973, #53804, #34050, #14712, #72364, #27734, #1657, #21010, #46670, #22251, #47909, #73614, #54640, #2900, #8385, #21425, #59713, #72770, #41602, #15956, #41197, #8796, #71945, #66885, #79517, #66047, #66460, #21832, #80350, #47495, #22663, #34888, #60549, #54220, #67292, #9625, #14297, #81582, #68932, #24304, #29388, #81165, #23899, #68523, #48322, #23069, #3724, #67705, #82396, #23481, #74019, #49974, #55048, #30628, #68119, #80755, #43235, #5368, #16365, #43646, #55869, #37357, #36940, #10864, #18012, #75672, #56293, #48737, #81990, #49565, #4537, #30207, #74434, #74855, #36524, #42011, #61790, #10041, #69349, #62200, #55456, #10464, #11703, #75259, #49148, #17197, #17603, #42830, #63030, #35705, #31029, #61374, #16781, #42419, #36117, #4130, #29795, #56697, #11281, #62618, #4960, #25123, #82799, #65110, #24714, #51613, #26378, #71422, #31441, #299, #57104, #25955, #50793, #64684, #76494, #18821, #77318, #58788, #44468, #70159, #12512, #77742, #13769, #19648, #57935, #39426, #45309, #7448, #33118, #31863, #83213, #19228, #38591, #71004, #50382, #7023, #20073, #64269, #76080, #6603, #38173, #13347, #63847, #25535, #18424, #5772, #6185, #57522, #51200, #76898, #44878, #70577, #39001, #32275, #32691, #12931, #44065, #58358, #720, #52038, #45725, #69757, #12103, #37761, #63436, #34792, #40677, #46978, #27212, #60451, #65948, #53294, #1969, #28048, #8284, #79415, #39850, #52875, #67197, #26796, #66787, #21325, #33950, #59614, #2803, #22154, #33536, #1558, #9122, #27632, #66362, #21734, #28462, #47813, #65541, #8700, #41099, #34371, #79006, #59199, #54123, #15438, #52453, #79837, #72672, #15021, #60036, #2392, #73515, #20494, #78163, #53706, #47397, #14611, #15864, #46148, #71843, #7872, #14193, #41512, #9528, #35200, #1146, #78585, #20911, #40265, #46564 ) ),
 .UNSPECIFIED., .F., .F., .F. ) 
 B_SPLINE_SURFACE_WITH_KNOTS ( ( 2, 2 ),
 ( 3, 2, 2, 2, 2, 2, 2, 2, 2, 2, 2, 2, 2, 2, 2, 2, 2, 2, 2, 2, 2, 2, 2, 2, 2, 2, 2, 2, 2, 2, 2, 2, 2, 2, 2, 2, 2, 2, 2, 2, 2, 2, 2, 2, 2, 2, 2, 2, 2, 2, 2, 2, 2, 2, 2, 2, 2, 2, 2, 2, 2, 2, 2, 2, 2, 2, 2, 2, 2, 2, 2, 2, 2, 2, 2, 2, 2, 2, 2, 2, 2, 2, 2, 2, 2, 2, 2, 2, 2, 2, 2, 2, 2, 2, 2, 2, 2, 2, 2, 2, 2, 2, 2, 2, 2, 2, 2, 2, 2, 2, 2, 2, 2, 2, 2, 2, 2, 2, 2, 2, 2, 2, 2, 2, 2, 2, 2, 2, 2, 2, 2, 2, 2, 2, 2, 2, 2, 2, 2, 2, 2, 2, 2, 2, 2, 2, 2, 2, 2, 2, 2, 2, 2, 2, 2, 2, 2, 2, 2, 2, 2, 2, 2, 2, 2, 2, 2, 2, 2, 2, 2, 2, 2, 2, 2, 2, 2, 2, 2, 2, 2, 2, 2, 2, 2, 2, 2, 2, 2, 2, 2, 2, 2, 2, 2, 2, 2, 2, 2, 2, 2, 2, 2, 2, 2, 2, 2, 2, 2, 2, 2, 2, 2, 2, 2, 2, 2, 2, 2, 2, 2, 2, 2, 2, 2, 2, 2, 2, 2, 2, 2, 2, 2, 2, 2, 2, 2, 2, 2, 2, 2, 2, 2, 2, 2, 2, 2, 2, 2, 2, 2, 2, 2, 2, 2, 3 ),
 ( 0.000000000000000000, 1.000000000000000000 ),
 ( 0.000000000000000000, 0.003787878787878787984, 0.007575757575757575968, 0.01136363636363636395, 0.01515151515151515194, 0.01893939393939393992, 0.02272727272727272790, 0.02651515151515151589, 0.03030303030303030387, 0.03409090909090908839, 0.03787878787878787984, 0.04166666666666666435, 0.04545454545454545581, 0.04924242424242424032, 0.05303030303030303177, 0.05681818181818181629, 0.06060606060606060774, 0.06439393939393939226, 0.06818181818181817677, 0.07196969696969697516, 0.07575757575757575968, 0.07954545454545454419, 0.08333333333333332871, 0.08712121212121212710, 0.09090909090909091161, 0.09469696969696969613, 0.09848484848484848064, 0.1022727272727272790, 0.1060606060606060635, 0.1098484848484848481, 0.1136363636363636326, 0.1174242424242424310, 0.1212121212121212155, 0.1250000000000000000, 0.1287878787878787845, 0.1325757575757575690, 0.1363636363636363535, 0.1401515151515151381, 0.1439393939393939503, 0.1477272727272727348, 0.1515151515151515194, 0.1553030303030303039, 0.1590909090909090884, 0.1628787878787878729, 0.1666666666666666574, 0.1704545454545454419, 0.1742424242424242542, 0.1780303030303030387, 0.1818181818181818232, 0.1856060606060606077, 0.1893939393939393923, 0.1931818181818181768, 0.1969696969696969613, 0.2007575757575757458, 0.2045454545454545581, 0.2083333333333333426, 0.2121212121212121271, 0.2159090909090909116, 0.2196969696969696961, 0.2234848484848484806, 0.2272727272727272652, 0.2310606060606060497, 0.2348484848484848619, 0.2386363636363636465, 0.2424242424242424310, 0.2462121212121212155, 0.2500000000000000000, 0.2537878787878787845, 0.2575757575757575690, 0.2613636363636363535, 0.2651515151515151381, 0.2689393939393939226, 0.2727272727272727071, 0.2765151515151514916, 0.2803030303030302761, 0.2840909090909091161, 0.2878787878787879007, 0.2916666666666666852, 0.2954545454545454697, 0.2992424242424242542, 0.3030303030303030387, 0.3068181818181818232, 0.3106060606060606077, 0.3143939393939393923, 0.3181818181818181768, 0.3219696969696969613, 0.3257575757575757458, 0.3295454545454545303, 0.3333333333333333148, 0.3371212121212120993, 0.3409090909090908839, 0.3446969696969697239, 0.3484848484848485084, 0.3522727272727272929, 0.3560606060606060774, 0.3598484848484848619, 0.3636363636363636465, 0.3674242424242424310, 0.3712121212121212155, 0.3750000000000000000, 0.3787878787878787845, 0.3825757575757575690, 0.3863636363636363535, 0.3901515151515151381, 0.3939393939393939226, 0.3977272727272727071, 0.4015151515151514916, 0.4053030303030302761, 0.4090909090909091161, 0.4128787878787879007, 0.4166666666666666852, 0.4204545454545454697, 0.4242424242424242542, 0.4280303030303030387, 0.4318181818181818232, 0.4356060606060606077, 0.4393939393939393923, 0.4431818181818181768, 0.4469696969696969613, 0.4507575757575757458, 0.4545454545454545303, 0.4583333333333333148, 0.4621212121212120993, 0.4659090909090908839, 0.4696969696969697239, 0.4734848484848485084, 0.4772727272727272929, 0.4810606060606060774, 0.4848484848484848619, 0.4886363636363636465, 0.4924242424242424310, 0.4962121212121212155, 0.5000000000000000000, 0.5037878787878787845, 0.5075757575757575690, 0.5113636363636363535, 0.5151515151515151381, 0.5189393939393939226, 0.5227272727272727071, 0.5265151515151514916, 0.5303030303030302761, 0.5340909090909090606, 0.5378787878787878451, 0.5416666666666666297, 0.5454545454545454142, 0.5492424242424241987, 0.5530303030303029832, 0.5568181818181817677, 0.5606060606060605522, 0.5643939393939394478, 0.5681818181818182323, 0.5719696969696970168, 0.5757575757575758013, 0.5795454545454545858, 0.5833333333333333703, 0.5871212121212121549, 0.5909090909090909394, 0.5946969696969697239, 0.5984848484848485084, 0.6022727272727272929, 0.6060606060606060774, 0.6098484848484848619, 0.6136363636363636465, 0.6174242424242424310, 0.6212121212121212155, 0.6250000000000000000, 0.6287878787878787845, 0.6325757575757575690, 0.6363636363636363535, 0.6401515151515151381, 0.6439393939393939226, 0.6477272727272727071, 0.6515151515151514916, 0.6553030303030302761, 0.6590909090909090606, 0.6628787878787878451, 0.6666666666666666297, 0.6704545454545454142, 0.6742424242424241987, 0.6780303030303029832, 0.6818181818181817677, 0.6856060606060605522, 0.6893939393939394478, 0.6931818181818182323, 0.6969696969696970168, 0.7007575757575758013, 0.7045454545454545858, 0.7083333333333333703, 0.7121212121212121549, 0.7159090909090909394, 0.7196969696969697239, 0.7234848484848485084, 0.7272727272727272929, 0.7310606060606060774, 0.7348484848484848619, 0.7386363636363636465, 0.7424242424242424310, 0.7462121212121212155, 0.7500000000000000000, 0.7537878787878787845, 0.7575757575757575690, 0.7613636363636363535, 0.7651515151515151381, 0.7689393939393939226, 0.7727272727272727071, 0.7765151515151514916, 0.7803030303030302761, 0.7840909090909090606, 0.7878787878787878451, 0.7916666666666666297, 0.7954545454545454142, 0.7992424242424241987, 0.8030303030303029832, 0.8068181818181817677, 0.8106060606060605522, 0.8143939393939394478, 0.8181818181818182323, 0.8219696969696970168, 0.8257575757575758013, 0.8295454545454545858, 0.8333333333333333703, 0.8371212121212121549, 0.8409090909090909394, 0.8446969696969697239, 0.8484848484848485084, 0.8522727272727272929, 0.8560606060606060774, 0.8598484848484848619, 0.8636363636363636465, 0.8674242424242424310, 0.8712121212121212155, 0.8750000000000000000, 0.8787878787878787845, 0.8825757575757575690, 0.8863636363636363535, 0.8901515151515151381, 0.8939393939393939226, 0.8977272727272727071, 0.9015151515151514916, 0.9053030303030302761, 0.9090909090909090606, 0.9128787878787878451, 0.9166666666666666297, 0.9204545454545454142, 0.9242424242424241987, 0.9280303030303029832, 0.9318181818181817677, 0.9356060606060605522, 0.9393939393939394478, 0.9431818181818182323, 0.9469696969696970168, 0.9507575757575758013, 0.9545454545454545858, 0.9583333333333333703, 0.9621212121212121549, 0.9659090909090909394 ),
 .UNSPECIFIED. ) 
 GEOMETRIC_REPRESENTATION_ITEM ( )  RATIONAL_B_SPLINE_SURFACE ( (
 ( 1.000000000000000000, 0.9659258262890683122, 1.000000000000000000, 0.9659258262890683122, 1.000000000000000000, 0.9659258262890683122, 1.000000000000000000, 0.9659258262890683122, 1.000000000000000000, 0.9659258262890683122, 1.000000000000000000, 0.9659258262890683122, 1.000000000000000000, 0.9659258262890683122, 1.000000000000000000, 0.9659258262890683122, 1.000000000000000000, 0.9659258262890683122, 1.000000000000000000, 0.9659258262890683122, 1.000000000000000000, 0.9659258262890683122, 1.000000000000000000, 0.9659258262890683122, 1.000000000000000000, 0.9659258262890683122, 1.000000000000000000, 0.9659258262890683122, 1.000000000000000000, 0.9659258262890683122, 1.000000000000000000, 0.9659258262890683122, 1.000000000000000000, 0.9659258262890683122, 1.000000000000000000, 0.9659258262890683122, 1.000000000000000000, 0.9659258262890683122, 1.000000000000000000, 0.9659258262890683122, 1.000000000000000000, 0.9659258262890683122, 1.000000000000000000, 0.9659258262890683122, 1.000000000000000000, 0.9659258262890683122, 1.000000000000000000, 0.9659258262890683122, 1.000000000000000000, 0.9659258262890683122, 1.000000000000000000, 0.9659258262890683122, 1.000000000000000000, 0.9659258262890683122, 1.000000000000000000, 0.9659258262890683122, 1.000000000000000000, 0.9659258262890683122, 1.000000000000000000, 0.9659258262890683122, 1.000000000000000000, 0.9659258262890683122, 1.000000000000000000, 0.9659258262890683122, 1.000000000000000000, 0.9659258262890683122, 1.000000000000000000, 0.9659258262890683122, 1.000000000000000000, 0.9659258262890683122, 1.000000000000000000, 0.9659258262890683122, 1.000000000000000000, 0.9659258262890683122, 1.000000000000000000, 0.9659258262890683122, 1.000000000000000000, 0.9659258262890683122, 1.000000000000000000, 0.9659258262890683122, 1.000000000000000000, 0.9659258262890683122, 1.000000000000000000, 0.9659258262890683122, 1.000000000000000000, 0.9659258262890683122, 1.000000000000000000, 0.9659258262890683122, 1.000000000000000000, 0.9659258262890683122, 1.000000000000000000, 0.9659258262890683122, 1.000000000000000000, 0.9659258262890683122, 1.000000000000000000, 0.9659258262890683122, 1.000000000000000000, 0.9659258262890683122, 1.000000000000000000, 0.9659258262890683122, 1.000000000000000000, 0.9659258262890683122, 1.000000000000000000, 0.9659258262890683122, 1.000000000000000000, 0.9659258262890683122, 1.000000000000000000, 0.9659258262890683122, 1.000000000000000000, 0.9659258262890683122, 1.000000000000000000, 0.9659258262890683122, 1.000000000000000000, 0.9659258262890683122, 1.000000000000000000, 0.9659258262890683122, 1.000000000000000000, 0.9659258262890683122, 1.000000000000000000, 0.9659258262890683122, 1.000000000000000000, 0.9659258262890683122, 1.000000000000000000, 0.9659258262890683122, 1.000000000000000000, 0.9659258262890683122, 1.000000000000000000, 0.9659258262890683122, 1.000000000000000000, 0.9659258262890683122, 1.000000000000000000, 0.9659258262890683122, 1.000000000000000000, 0.9659258262890683122, 1.000000000000000000, 0.9659258262890683122, 1.000000000000000000, 0.9659258262890683122, 1.000000000000000000, 0.9659258262890683122, 1.000000000000000000, 0.9659258262890683122, 1.000000000000000000, 0.9659258262890683122, 1.000000000000000000, 0.9659258262890683122, 1.000000000000000000, 0.9659258262890683122, 1.000000000000000000, 0.9659258262890683122, 1.000000000000000000, 0.9659258262890683122, 1.000000000000000000, 0.9659258262890683122, 1.000000000000000000, 0.9659258262890683122, 1.000000000000000000, 0.9659258262890683122, 1.000000000000000000, 0.9659258262890683122, 1.000000000000000000, 0.9659258262890683122, 1.000000000000000000, 0.9659258262890683122, 1.000000000000000000, 0.9659258262890683122, 1.000000000000000000, 0.9659258262890683122, 1.000000000000000000, 0.9659258262890683122, 1.000000000000000000, 0.9659258262890683122, 1.000000000000000000, 0.9659258262890683122, 1.000000000000000000, 0.9659258262890683122, 1.000000000000000000, 0.9659258262890683122, 1.000000000000000000, 0.9659258262890683122, 1.000000000000000000, 0.9659258262890683122, 1.000000000000000000, 0.9659258262890683122, 1.000000000000000000, 0.9659258262890683122, 1.000000000000000000, 0.9659258262890683122, 1.000000000000000000, 0.9659258262890683122, 1.000000000000000000, 0.9659258262890683122, 1.000000000000000000, 0.9659258262890683122, 1.000000000000000000, 0.9659258262890683122, 1.000000000000000000, 0.9659258262890683122, 1.000000000000000000, 0.9659258262890683122, 1.000000000000000000, 0.9659258262890683122, 1.000000000000000000, 0.9659258262890683122, 1.000000000000000000, 0.9659258262890683122, 1.000000000000000000, 0.9659258262890683122, 1.000000000000000000, 0.9659258262890683122, 1.000000000000000000, 0.9659258262890683122, 1.000000000000000000, 0.9659258262890683122, 1.000000000000000000, 0.9659258262890683122, 1.000000000000000000, 0.9659258262890683122, 1.000000000000000000, 0.9659258262890683122, 1.000000000000000000, 0.9659258262890683122, 1.000000000000000000, 0.9659258262890683122, 1.000000000000000000, 0.9659258262890683122, 1.000000000000000000, 0.9659258262890683122, 1.000000000000000000, 0.9659258262890683122, 1.000000000000000000, 0.9659258262890683122, 1.000000000000000000, 0.9659258262890683122, 1.000000000000000000, 0.9659258262890683122, 1.000000000000000000, 0.9659258262890683122, 1.000000000000000000, 0.9659258262890683122, 1.000000000000000000, 0.9659258262890683122, 1.000000000000000000, 0.9659258262890683122, 1.000000000000000000, 0.9659258262890683122, 1.000000000000000000, 0.9659258262890683122, 1.000000000000000000, 0.9659258262890683122, 1.000000000000000000, 0.9659258262890683122, 1.000000000000000000, 0.9659258262890683122, 1.000000000000000000, 0.9659258262890683122, 1.000000000000000000, 0.9659258262890683122, 1.000000000000000000, 0.9659258262890683122, 1.000000000000000000, 0.9659258262890683122, 1.000000000000000000, 0.9659258262890683122, 1.000000000000000000, 0.9659258262890683122, 1.000000000000000000, 0.9659258262890683122, 1.000000000000000000, 0.9659258262890683122, 1.000000000000000000, 0.9659258262890683122, 1.000000000000000000, 0.9659258262890683122, 1.000000000000000000, 0.9659258262890683122, 1.000000000000000000, 0.9659258262890683122, 1.000000000000000000, 0.9659258262890683122, 1.000000000000000000, 0.9659258262890683122, 1.000000000000000000, 0.9659258262890683122, 1.000000000000000000, 0.9659258262890683122, 1.000000000000000000, 0.9659258262890683122, 1.000000000000000000, 0.9659258262890683122, 1.000000000000000000, 0.9659258262890683122, 1.000000000000000000, 0.9659258262890683122, 1.000000000000000000, 0.9659258262890683122, 1.000000000000000000, 0.9659258262890683122, 1.000000000000000000, 0.9659258262890683122, 1.000000000000000000, 0.9659258262890683122, 1.000000000000000000, 0.9659258262890683122, 1.000000000000000000, 0.9659258262890683122, 1.000000000000000000, 0.9659258262890683122, 1.000000000000000000, 0.9659258262890683122, 1.000000000000000000, 0.9659258262890683122, 1.000000000000000000, 0.9659258262890683122, 1.000000000000000000, 0.9659258262890683122, 1.000000000000000000, 0.9659258262890683122, 1.000000000000000000, 0.9659258262890683122, 1.000000000000000000, 0.9659258262890683122, 1.000000000000000000, 0.9659258262890683122, 1.000000000000000000, 0.9659258262890683122, 1.000000000000000000, 0.9659258262890683122, 1.000000000000000000, 0.9659258262890683122, 1.000000000000000000, 0.9659258262890683122, 1.000000000000000000, 0.9659258262890683122, 1.000000000000000000, 0.9659258262890683122, 1.000000000000000000, 0.9659258262890683122, 1.000000000000000000, 0.9659258262890683122, 1.000000000000000000, 0.9659258262890683122, 1.000000000000000000, 0.9659258262890683122, 1.000000000000000000, 0.9659258262890683122, 1.000000000000000000, 0.9659258262890683122, 1.000000000000000000, 0.9659258262890683122, 1.000000000000000000, 0.9659258262890683122, 1.000000000000000000, 0.9659258262890683122, 1.000000000000000000, 0.9659258262890683122, 1.000000000000000000, 0.9659258262890683122, 1.000000000000000000, 0.9659258262890683122, 1.000000000000000000, 0.9659258262890683122, 1.000000000000000000, 0.9659258262890683122, 1.000000000000000000, 0.9659258262890683122, 1.000000000000000000, 0.9659258262890683122, 1.000000000000000000, 0.9659258262890683122, 1.000000000000000000, 0.9659258262890683122, 1.000000000000000000, 0.9659258262890683122, 1.000000000000000000, 0.9659258262890683122, 1.000000000000000000, 0.9659258262890683122, 1.000000000000000000, 0.9659258262890683122, 1.000000000000000000, 0.9659258262890683122, 1.000000000000000000, 0.9659258262890683122, 1.000000000000000000, 0.9659258262890683122, 1.000000000000000000, 0.9659258262890683122, 1.000000000000000000, 0.9659258262890683122, 1.000000000000000000, 0.9659258262890683122, 1.000000000000000000, 0.9659258262890683122, 1.000000000000000000, 0.9659258262890683122, 1.000000000000000000, 0.9659258262890683122, 1.000000000000000000, 0.9659258262890683122, 1.000000000000000000, 0.9659258262890683122, 1.000000000000000000, 0.9659258262890683122, 1.000000000000000000, 0.9659258262890683122, 1.000000000000000000, 0.9659258262890683122, 1.000000000000000000, 0.9659258262890683122, 1.000000000000000000, 0.9659258262890683122, 1.000000000000000000, 0.9659258262890683122, 1.000000000000000000, 0.9659258262890683122, 1.000000000000000000, 0.9659258262890683122, 1.000000000000000000, 0.9659258262890683122, 1.000000000000000000, 0.9659258262890683122, 1.000000000000000000, 0.9659258262890683122, 1.000000000000000000, 0.9659258262890683122, 1.000000000000000000, 0.9659258262890683122, 1.000000000000000000, 0.9659258262890683122, 1.000000000000000000, 0.9659258262890683122, 1.000000000000000000, 0.9659258262890683122, 1.000000000000000000, 0.9659258262890683122, 1.000000000000000000, 0.9659258262890683122, 1.000000000000000000, 0.9659258262890683122, 1.000000000000000000, 0.9659258262890683122, 1.000000000000000000, 0.9659258262890683122, 1.000000000000000000, 0.9659258262890683122, 1.000000000000000000, 0.9659258262890683122, 1.000000000000000000, 0.9659258262890683122, 1.000000000000000000, 0.9659258262890683122, 1.000000000000000000, 0.9659258262890683122, 1.000000000000000000, 0.9659258262890683122, 1.000000000000000000, 0.9659258262890683122, 1.000000000000000000, 0.9659258262890683122, 1.000000000000000000, 0.9659258262890683122, 1.000000000000000000, 0.9659258262890683122, 1.000000000000000000, 0.9659258262890683122, 1.000000000000000000, 0.9659258262890683122, 1.000000000000000000, 0.9659258262890683122, 1.000000000000000000, 0.9659258262890683122, 1.000000000000000000, 0.9659258262890683122, 1.000000000000000000, 0.9659258262890683122, 1.000000000000000000, 0.9659258262890683122, 1.000000000000000000, 0.9659258262890683122, 1.000000000000000000, 0.9659258262890683122, 1.000000000000000000, 0.9659258262890683122, 1.000000000000000000, 0.9659258262890683122, 1.000000000000000000, 0.9659258262890683122, 1.000000000000000000, 0.9659258262890683122, 1.000000000000000000, 0.9659258262890683122, 1.000000000000000000, 0.9659258262890683122, 1.000000000000000000, 0.9659258262890683122, 1.000000000000000000, 0.9659258262890683122, 1.000000000000000000, 0.9659258262890683122, 1.000000000000000000, 0.9659258262890683122, 1.000000000000000000, 0.9659258262890683122, 1.000000000000000000, 0.9659258262890683122, 1.000000000000000000, 0.9659258262890683122, 1.000000000000000000, 0.9659258262890683122, 1.000000000000000000),
 ( 1.000000000000000000, 0.9659258262890683122, 1.000000000000000000, 0.9659258262890683122, 1.000000000000000000, 0.9659258262890683122, 1.000000000000000000, 0.9659258262890683122, 1.000000000000000000, 0.9659258262890683122, 1.000000000000000000, 0.9659258262890683122, 1.000000000000000000, 0.9659258262890683122, 1.000000000000000000, 0.9659258262890683122, 1.000000000000000000, 0.9659258262890683122, 1.000000000000000000, 0.9659258262890683122, 1.000000000000000000, 0.9659258262890683122, 1.000000000000000000, 0.9659258262890683122, 1.000000000000000000, 0.9659258262890683122, 1.000000000000000000, 0.9659258262890683122, 1.000000000000000000, 0.9659258262890683122, 1.000000000000000000, 0.9659258262890683122, 1.000000000000000000, 0.9659258262890683122, 1.000000000000000000, 0.9659258262890683122, 1.000000000000000000, 0.9659258262890683122, 1.000000000000000000, 0.9659258262890683122, 1.000000000000000000, 0.9659258262890683122, 1.000000000000000000, 0.9659258262890683122, 1.000000000000000000, 0.9659258262890683122, 1.000000000000000000, 0.9659258262890683122, 1.000000000000000000, 0.9659258262890683122, 1.000000000000000000, 0.9659258262890683122, 1.000000000000000000, 0.9659258262890683122, 1.000000000000000000, 0.9659258262890683122, 1.000000000000000000, 0.9659258262890683122, 1.000000000000000000, 0.9659258262890683122, 1.000000000000000000, 0.9659258262890683122, 1.000000000000000000, 0.9659258262890683122, 1.000000000000000000, 0.9659258262890683122, 1.000000000000000000, 0.9659258262890683122, 1.000000000000000000, 0.9659258262890683122, 1.000000000000000000, 0.9659258262890683122, 1.000000000000000000, 0.9659258262890683122, 1.000000000000000000, 0.9659258262890683122, 1.000000000000000000, 0.9659258262890683122, 1.000000000000000000, 0.9659258262890683122, 1.000000000000000000, 0.9659258262890683122, 1.000000000000000000, 0.9659258262890683122, 1.000000000000000000, 0.9659258262890683122, 1.000000000000000000, 0.9659258262890683122, 1.000000000000000000, 0.9659258262890683122, 1.000000000000000000, 0.9659258262890683122, 1.000000000000000000, 0.9659258262890683122, 1.000000000000000000, 0.9659258262890683122, 1.000000000000000000, 0.9659258262890683122, 1.000000000000000000, 0.9659258262890683122, 1.000000000000000000, 0.9659258262890683122, 1.000000000000000000, 0.9659258262890683122, 1.000000000000000000, 0.9659258262890683122, 1.000000000000000000, 0.9659258262890683122, 1.000000000000000000, 0.9659258262890683122, 1.000000000000000000, 0.9659258262890683122, 1.000000000000000000, 0.9659258262890683122, 1.000000000000000000, 0.9659258262890683122, 1.000000000000000000, 0.9659258262890683122, 1.000000000000000000, 0.9659258262890683122, 1.000000000000000000, 0.9659258262890683122, 1.000000000000000000, 0.9659258262890683122, 1.000000000000000000, 0.9659258262890683122, 1.000000000000000000, 0.9659258262890683122, 1.000000000000000000, 0.9659258262890683122, 1.000000000000000000, 0.9659258262890683122, 1.000000000000000000, 0.9659258262890683122, 1.000000000000000000, 0.9659258262890683122, 1.000000000000000000, 0.9659258262890683122, 1.000000000000000000, 0.9659258262890683122, 1.000000000000000000, 0.9659258262890683122, 1.000000000000000000, 0.9659258262890683122, 1.000000000000000000, 0.9659258262890683122, 1.000000000000000000, 0.9659258262890683122, 1.000000000000000000, 0.9659258262890683122, 1.000000000000000000, 0.9659258262890683122, 1.000000000000000000, 0.9659258262890683122, 1.000000000000000000, 0.9659258262890683122, 1.000000000000000000, 0.9659258262890683122, 1.000000000000000000, 0.9659258262890683122, 1.000000000000000000, 0.9659258262890683122, 1.000000000000000000, 0.9659258262890683122, 1.000000000000000000, 0.9659258262890683122, 1.000000000000000000, 0.9659258262890683122, 1.000000000000000000, 0.9659258262890683122, 1.000000000000000000, 0.9659258262890683122, 1.000000000000000000, 0.9659258262890683122, 1.000000000000000000, 0.9659258262890683122, 1.000000000000000000, 0.9659258262890683122, 1.000000000000000000, 0.9659258262890683122, 1.000000000000000000, 0.9659258262890683122, 1.000000000000000000, 0.9659258262890683122, 1.000000000000000000, 0.9659258262890683122, 1.000000000000000000, 0.9659258262890683122, 1.000000000000000000, 0.9659258262890683122, 1.000000000000000000, 0.9659258262890683122, 1.000000000000000000, 0.9659258262890683122, 1.000000000000000000, 0.9659258262890683122, 1.000000000000000000, 0.9659258262890683122, 1.000000000000000000, 0.9659258262890683122, 1.000000000000000000, 0.9659258262890683122, 1.000000000000000000, 0.9659258262890683122, 1.000000000000000000, 0.9659258262890683122, 1.000000000000000000, 0.9659258262890683122, 1.000000000000000000, 0.9659258262890683122, 1.000000000000000000, 0.9659258262890683122, 1.000000000000000000, 0.9659258262890683122, 1.000000000000000000, 0.9659258262890683122, 1.000000000000000000, 0.9659258262890683122, 1.000000000000000000, 0.9659258262890683122, 1.000000000000000000, 0.9659258262890683122, 1.000000000000000000, 0.9659258262890683122, 1.000000000000000000, 0.9659258262890683122, 1.000000000000000000, 0.9659258262890683122, 1.000000000000000000, 0.9659258262890683122, 1.000000000000000000, 0.9659258262890683122, 1.000000000000000000, 0.9659258262890683122, 1.000000000000000000, 0.9659258262890683122, 1.000000000000000000, 0.9659258262890683122, 1.000000000000000000, 0.9659258262890683122, 1.000000000000000000, 0.9659258262890683122, 1.000000000000000000, 0.9659258262890683122, 1.000000000000000000, 0.9659258262890683122, 1.000000000000000000, 0.9659258262890683122, 1.000000000000000000, 0.9659258262890683122, 1.000000000000000000, 0.9659258262890683122, 1.000000000000000000, 0.9659258262890683122, 1.000000000000000000, 0.9659258262890683122, 1.000000000000000000, 0.9659258262890683122, 1.000000000000000000, 0.9659258262890683122, 1.000000000000000000, 0.9659258262890683122, 1.000000000000000000, 0.9659258262890683122, 1.000000000000000000, 0.9659258262890683122, 1.000000000000000000, 0.9659258262890683122, 1.000000000000000000, 0.9659258262890683122, 1.000000000000000000, 0.9659258262890683122, 1.000000000000000000, 0.9659258262890683122, 1.000000000000000000, 0.9659258262890683122, 1.000000000000000000, 0.9659258262890683122, 1.000000000000000000, 0.9659258262890683122, 1.000000000000000000, 0.9659258262890683122, 1.000000000000000000, 0.9659258262890683122, 1.000000000000000000, 0.9659258262890683122, 1.000000000000000000, 0.9659258262890683122, 1.000000000000000000, 0.9659258262890683122, 1.000000000000000000, 0.9659258262890683122, 1.000000000000000000, 0.9659258262890683122, 1.000000000000000000, 0.9659258262890683122, 1.000000000000000000, 0.9659258262890683122, 1.000000000000000000, 0.9659258262890683122, 1.000000000000000000, 0.9659258262890683122, 1.000000000000000000, 0.9659258262890683122, 1.000000000000000000, 0.9659258262890683122, 1.000000000000000000, 0.9659258262890683122, 1.000000000000000000, 0.9659258262890683122, 1.000000000000000000, 0.9659258262890683122, 1.000000000000000000, 0.9659258262890683122, 1.000000000000000000, 0.9659258262890683122, 1.000000000000000000, 0.9659258262890683122, 1.000000000000000000, 0.9659258262890683122, 1.000000000000000000, 0.9659258262890683122, 1.000000000000000000, 0.9659258262890683122, 1.000000000000000000, 0.9659258262890683122, 1.000000000000000000, 0.9659258262890683122, 1.000000000000000000, 0.9659258262890683122, 1.000000000000000000, 0.9659258262890683122, 1.000000000000000000, 0.9659258262890683122, 1.000000000000000000, 0.9659258262890683122, 1.000000000000000000, 0.9659258262890683122, 1.000000000000000000, 0.9659258262890683122, 1.000000000000000000, 0.9659258262890683122, 1.000000000000000000, 0.9659258262890683122, 1.000000000000000000, 0.9659258262890683122, 1.000000000000000000, 0.9659258262890683122, 1.000000000000000000, 0.9659258262890683122, 1.000000000000000000, 0.9659258262890683122, 1.000000000000000000, 0.9659258262890683122, 1.000000000000000000, 0.9659258262890683122, 1.000000000000000000, 0.9659258262890683122, 1.000000000000000000, 0.9659258262890683122, 1.000000000000000000, 0.9659258262890683122, 1.000000000000000000, 0.9659258262890683122, 1.000000000000000000, 0.9659258262890683122, 1.000000000000000000, 0.9659258262890683122, 1.000000000000000000, 0.9659258262890683122, 1.000000000000000000, 0.9659258262890683122, 1.000000000000000000, 0.9659258262890683122, 1.000000000000000000, 0.9659258262890683122, 1.000000000000000000, 0.9659258262890683122, 1.000000000000000000, 0.9659258262890683122, 1.000000000000000000, 0.9659258262890683122, 1.000000000000000000, 0.9659258262890683122, 1.000000000000000000, 0.9659258262890683122, 1.000000000000000000, 0.9659258262890683122, 1.000000000000000000, 0.9659258262890683122, 1.000000000000000000, 0.9659258262890683122, 1.000000000000000000, 0.9659258262890683122, 1.000000000000000000, 0.9659258262890683122, 1.000000000000000000, 0.9659258262890683122, 1.000000000000000000, 0.9659258262890683122, 1.000000000000000000, 0.9659258262890683122, 1.000000000000000000, 0.9659258262890683122, 1.000000000000000000, 0.9659258262890683122, 1.000000000000000000, 0.9659258262890683122, 1.000000000000000000, 0.9659258262890683122, 1.000000000000000000, 0.9659258262890683122, 1.000000000000000000, 0.9659258262890683122, 1.000000000000000000, 0.9659258262890683122, 1.000000000000000000, 0.9659258262890683122, 1.000000000000000000, 0.9659258262890683122, 1.000000000000000000, 0.9659258262890683122, 1.000000000000000000, 0.9659258262890683122, 1.000000000000000000, 0.9659258262890683122, 1.000000000000000000, 0.9659258262890683122, 1.000000000000000000, 0.9659258262890683122, 1.000000000000000000, 0.9659258262890683122, 1.000000000000000000, 0.9659258262890683122, 1.000000000000000000, 0.9659258262890683122, 1.000000000000000000, 0.9659258262890683122, 1.000000000000000000, 0.9659258262890683122, 1.000000000000000000, 0.9659258262890683122, 1.000000000000000000, 0.9659258262890683122, 1.000000000000000000, 0.9659258262890683122, 1.000000000000000000, 0.9659258262890683122, 1.000000000000000000, 0.9659258262890683122, 1.000000000000000000, 0.9659258262890683122, 1.000000000000000000, 0.9659258262890683122, 1.000000000000000000, 0.9659258262890683122, 1.000000000000000000, 0.9659258262890683122, 1.000000000000000000, 0.9659258262890683122, 1.000000000000000000, 0.9659258262890683122, 1.000000000000000000, 0.9659258262890683122, 1.000000000000000000, 0.9659258262890683122, 1.000000000000000000, 0.9659258262890683122, 1.000000000000000000, 0.9659258262890683122, 1.000000000000000000, 0.9659258262890683122, 1.000000000000000000, 0.9659258262890683122, 1.000000000000000000, 0.9659258262890683122, 1.000000000000000000, 0.9659258262890683122, 1.000000000000000000, 0.9659258262890683122, 1.000000000000000000, 0.9659258262890683122, 1.000000000000000000, 0.9659258262890683122, 1.000000000000000000, 0.9659258262890683122, 1.000000000000000000, 0.9659258262890683122, 1.000000000000000000, 0.9659258262890683122, 1.000000000000000000, 0.9659258262890683122, 1.000000000000000000, 0.9659258262890683122, 1.000000000000000000, 0.9659258262890683122, 1.000000000000000000, 0.9659258262890683122, 1.000000000000000000, 0.9659258262890683122, 1.000000000000000000, 0.9659258262890683122, 1.000000000000000000, 0.9659258262890683122, 1.000000000000000000, 0.9659258262890683122, 1.000000000000000000, 0.9659258262890683122, 1.000000000000000000, 0.9659258262890683122, 1.000000000000000000) ) ) 
 REPRESENTATION_ITEM ( '' )  SURFACE ( )  );
#60098 = CARTESIAN_POINT ( 'NONE',  ( -0.5249343832020990641, -0.5023911411419708095, -0.1820866141732282451 ) ) ;
#60099 = CARTESIAN_POINT ( 'NONE',  ( 0.4623158380715545746, 0.02617651024168222984, 2.142213561789874543 ) ) ;
#60100 = CARTESIAN_POINT ( 'NONE',  ( 0.3996062992125986035, 0.1070741851644054776, -0.2821522309711286258 ) ) ;
#60101 = CARTESIAN_POINT ( 'NONE',  ( 0.1958661417322834775, 0.3392501089628018884, -2.660780470637482242 ) ) ;
#60102 = CARTESIAN_POINT ( 'NONE',  ( -3.873860110281697189, 2.736617272820978553, -0.5314960629921261503 ) ) ;
#60103 = CARTESIAN_POINT ( 'NONE',  ( 0.9776902887139113929, 0.1771653543307087630, 0.09757992244046791164 ) ) ;
#60104 = CARTESIAN_POINT ( 'NONE',  ( -1.725721784776902190, -0.05778040916215522460, 0.4822834645669289988 ) ) ;
#60105 = AXIS2_PLACEMENT_3D ( 'NONE', #58978, #37942, #12286 ) ;
#60106 = CARTESIAN_POINT ( 'NONE',  ( 1.266404199475066328, -0.05778040916215522460, 0.4822834645669289988 ) ) ;
#60107 = CARTESIAN_POINT ( 'NONE',  ( 0.3917322834645669549, 0.1049643490035304660, -2.414041994750655729 ) ) ;
#60108 = CARTESIAN_POINT ( 'NONE',  ( 1.148293963254593875, -0.5511811023622046335, 0.09757992244046803654 ) ) ;
#60109 = CARTESIAN_POINT ( 'NONE',  ( 0.1049868766404206816, 0.2306618581243848609, 0.2411417322834645549 ) ) ;
#60110 = CARTESIAN_POINT ( 'NONE',  ( -0.4658792650918627265, -0.3162353388693409650, -0.4822834645669289433 ) ) ;
#60111 = CARTESIAN_POINT ( 'NONE',  ( 1.581364829396326277, -0.3162353388693409650, -0.4822834645669289433 ) ) ;
#60112 = VECTOR ( 'NONE', #19789, 39.37007874015748143 ) ;
#60113 = CONICAL_SURFACE ( 'NONE', #30491, 0.1771653543307085410, 1.029744258676653645 ) ;
#60114 = CARTESIAN_POINT ( 'NONE',  ( 3.856579543051780856, 2.748002881374839390, 0.5314960629921259283 ) ) ;
#60115 = CARTESIAN_POINT ( 'NONE',  ( 0.3674540682414705883, 0.1283753931104746893, -0.1820866141732285504 ) ) ;
#60116 = ORIENTED_EDGE ( 'NONE', *, *, #17653, .F. ) ;
#60117 = CARTESIAN_POINT ( 'NONE',  ( -9.594673741351313045E-17, 0.3917322834645670659, -0.4691794207687158269 ) ) ;
#60118 = VERTEX_POINT ( 'NONE', #76294 ) ;
#60119 = CARTESIAN_POINT ( 'NONE',  ( -0.4068241469816267775, 0.05413385826771626580, -0.4176697321401330321 ) ) ;
#60120 = CARTESIAN_POINT ( 'NONE',  ( 1.509186351706037543, -0.4281496062992127816, -0.4176697321401328100 ) ) ;
#60121 = CARTESIAN_POINT ( 'NONE',  ( 0.3149606299212606708, -0.1870078740157480879, -0.4822834645669291653 ) ) ;
#60122 = CARTESIAN_POINT ( 'NONE',  ( -0.3937007874015740483, -0.1870078740157479769, 0.3641732283464567677 ) ) ;
#60123 = CARTESIAN_POINT ( 'NONE',  ( 0.6824146981627303710, -0.6046776061558807314, 0.2411417322834647770 ) ) ;
#60124 = CARTESIAN_POINT ( 'NONE',  ( -0.8202099737532799750, 0.2952755905511810774, -0.1292274648535930714 ) ) ;
#60125 = CARTESIAN_POINT ( 'NONE',  ( -0.3937007874015740483, -0.1870078740157480879, -0.4822834645669291653 ) ) ;
#60126 = CARTESIAN_POINT ( 'NONE',  ( -0.7086614173228339419, -0.1870078740157480879, -0.4822834645669291653 ) ) ;
#60127 = CARTESIAN_POINT ( 'NONE',  ( 1.115485564304462551, 0.05413385826771666132, 0.4176697321401328100 ) ) ;
#60128 = CARTESIAN_POINT ( 'NONE',  ( 0.7874015748031503170, -0.1870078740157479769, 0.4822834645669291653 ) ) ;
#60129 = CARTESIAN_POINT ( 'NONE',  ( 0.7480314960629927956, 0.2952755905511811885, 0.000000000000000000 ) ) ;
#60130 = CARTESIAN_POINT ( 'NONE',  ( -0.1049643490035302024, -0.3917322834645671215, -0.5367454068241469534 ) ) ;
#60131 = CARTESIAN_POINT ( 'NONE',  ( -0.1115485564304453947, -0.5511811023622046335, 0.09757992244046803654 ) ) ;
#60132 = EDGE_LOOP ( 'NONE', ( #74707, #35471, #70082, #23148, #72750, #35812 ) ) ;
#60133 = CARTESIAN_POINT ( 'NONE',  ( 0.1058382717557499880, 0.3949938075777411073, -1.095800524934383180 ) ) ;
#60134 = VERTEX_POINT ( 'NONE', #37560 ) ;
#60135 = CARTESIAN_POINT ( 'NONE',  ( -1.003937007874015297, -0.4536011799217368745, -0.2665933059059886201 ) ) ;
#60136 = CARTESIAN_POINT ( 'NONE',  ( -0.2296587926509179312, -0.05778040916215522460, 0.4822834645669289988 ) ) ;
#60137 = CARTESIAN_POINT ( 'NONE',  ( 2.873826567705914936, 1.063196196511239977, 0.01636564761923926109 ) ) ;
#60138 = CARTESIAN_POINT ( 'NONE',  ( -0.07217847769028813698, -0.3162353388693409650, -0.4822834645669289433 ) ) ;
#60139 = CARTESIAN_POINT ( 'NONE',  ( -0.5511811023622041894, -0.1870078740157480879, -0.4822834645669291653 ) ) ;
#60140 = CARTESIAN_POINT ( 'NONE',  ( -1.469816272965878357, 0.2306618581243848609, 0.2411417322834645549 ) ) ;
#60141 = CARTESIAN_POINT ( 'NONE',  ( -1.417322834645668772, -0.1870078740157479769, 0.4822834645669291653 ) ) ;
#60142 = CARTESIAN_POINT ( 'NONE',  ( 1.364829396325460076, 0.1283753931104748280, 0.1820866141732283561 ) ) ;
#60143 = CARTESIAN_POINT ( 'NONE',  ( -1.469816272965878357, 0.2306618581243848609, 0.2411417322834645549 ) ) ;
#60144 = CARTESIAN_POINT ( 'NONE',  ( 0.2445717520902165876, 0.1654678116698105328, 5.638396876410332048 ) ) ;
#60145 = CARTESIAN_POINT ( 'NONE',  ( 0.4396325459317590445, -0.5511811023622046335, 0.09757992244046803654 ) ) ;
#60146 = CARTESIAN_POINT ( 'NONE',  ( 0.1640419947506569498, -0.3162353388693409650, -0.4822834645669289433 ) ) ;
#60147 = CARTESIAN_POINT ( 'NONE',  ( 0.3280839895013130669, -0.4281496062992127816, -0.4176697321401328100 ) ) ;
#60148 = ORIENTED_EDGE ( 'NONE', *, *, #16394, .T. ) ;
#60149 = CARTESIAN_POINT ( 'NONE',  ( -9.787531504996567848E-17, 0.3996062992125986035, -1.732283464566929165 ) ) ;
#60150 = CARTESIAN_POINT ( 'NONE',  ( 1.403614904275686858E-14, 1.537401574803149984, -3.937007874015761910 ) ) ;
#60151 = CARTESIAN_POINT ( 'NONE',  ( -0.1070741851644051862, -0.3996062992125986590, -1.093832020997375087 ) ) ;
#60152 = CARTESIAN_POINT ( 'NONE',  ( 0.1070741851644054776, -0.3996062992125984925, -0.4770341207349080848 ) ) ;
#60153 = CARTESIAN_POINT ( 'NONE',  ( -0.6889763779527552368, -0.5400638737290845981, -0.3530559997133363437 ) ) ;
#60154 = CARTESIAN_POINT ( 'NONE',  ( 0.2925321140481932369, -0.2925321140481932369, -2.933070866141732402 ) ) ;
#60155 = CARTESIAN_POINT ( 'NONE',  ( -0.3917322834645671215, 0.1049643490035301469, -2.322178477690288734 ) ) ;
#60156 = CARTESIAN_POINT ( 'NONE',  ( -1.443569553805773564, 0.1283753931104746893, -0.1820866141732285504 ) ) ;
#60157 = CARTESIAN_POINT ( 'NONE',  ( 0.8530183727034126306, 0.05413385826771626580, -0.4176697321401330321 ) ) ;
#60158 = CARTESIAN_POINT ( 'NONE',  ( 1.043307086614173818, 0.1660481256975885056, 0.3530559997133364547 ) ) ;
#60159 = CARTESIAN_POINT ( 'NONE',  ( -0.1115485564304453947, -0.5511811023622046335, 0.09757992244046803654 ) ) ;
#60160 = CARTESIAN_POINT ( 'NONE',  ( 0.04593175853018440641, 0.2952755905511810774, -0.1292274648535930714 ) ) ;
#60161 = CARTESIAN_POINT ( 'NONE',  ( -1.157146581871515012E-16, 0.4724409448818898682, -2.124015748031495843 ) ) ;
#60162 = CARTESIAN_POINT ( 'NONE',  ( 0.1246719160104994284, 0.1771653543307087075, -0.09757992244046823083 ) ) ;
#60163 = CARTESIAN_POINT ( 'NONE',  ( -0.3805774278215216522, -0.4281496062992127816, -0.4176697321401328100 ) ) ;
#60164 = CARTESIAN_POINT ( 'NONE',  ( -0.2891555358219909388, -0.2891555358219912164, -2.025590551181102761 ) ) ;
#60165 = CARTESIAN_POINT ( 'NONE',  ( -1.686351706036744558, 0.2952755905511810774, -0.1292274648535930714 ) ) ;
#60166 = CARTESIAN_POINT ( 'NONE',  ( 0.2034120734908142214, 0.1771653543307087075, -0.09757992244046823083 ) ) ;
#60167 = CARTESIAN_POINT ( 'NONE',  ( -1.056430446194224881, 0.2952755905511810774, -0.1292274648535930714 ) ) ;
#60168 = CARTESIAN_POINT ( 'NONE',  ( -0.8792650918635160906, -0.3690944881889763329, 0.3153832671262228327 ) ) ;
#60169 = CARTESIAN_POINT ( 'NONE',  ( -0.6955380577427815458, -0.4281496062992127816, -0.4176697321401328100 ) ) ;
#60170 = CARTESIAN_POINT ( 'NONE',  ( -0.5380577427821514602, 0.05413385826771666132, 0.4176697321401328100 ) ) ;
#60171 = CARTESIAN_POINT ( 'NONE',  ( -0.05905511811023545637, 0.1660481256975885056, 0.3530559997133364547 ) ) ;
#60172 = CARTESIAN_POINT ( 'NONE',  ( -0.2925321140481932369, 0.2925321140481931259, -2.458661417322834719 ) ) ;
#60173 = ADVANCED_FACE ( 'NONE', ( #25748 ), #11906, .F. ) ;
#60175 = CARTESIAN_POINT ( 'NONE',  ( 0.3917322834645668994, -0.1049643490035303134, -2.238825828575116805 ) ) ;
#60174 = AXIS2_PLACEMENT_3D ( 'NONE', #17690, #69019, #23568 ) ;
#60176 = CARTESIAN_POINT ( 'NONE',  ( -2.170146923806555606, 1.528804020127598751, -0.4744094488188977388 ) ) ;
#60177 = CARTESIAN_POINT ( 'NONE',  ( 0.3280839895013130669, -0.3690944881889765550, -0.3153832671262227771 ) ) ;
#60178 = CARTESIAN_POINT ( 'NONE',  ( 1.122047244094488860, 0.1660481256975885056, 0.3530559997133364547 ) ) ;
#60179 = CARTESIAN_POINT ( 'NONE',  ( -1.338582677165353729, -0.1870078740157480601, -0.3641732283464567677 ) ) ;
#60180 = CARTESIAN_POINT ( 'NONE',  ( 1.318897637795276356, -0.5400638737290844871, 0.3530559997133364547 ) ) ;
#60181 = CARTESIAN_POINT ( 'NONE',  ( -1.194225721784776262, -0.004921259842519870586, -0.3153832671262229437 ) ) ;
#60182 = ADVANCED_FACE ( 'NONE', ( #31656 ), #49772, .F. ) ;
#60183 = CARTESIAN_POINT ( 'NONE',  ( -0.3215223097112853146, -0.3162353388693405765, 0.4822834645669290543 ) ) ;
#60184 = CARTESIAN_POINT ( 'NONE',  ( -0.006561679790025524116, -0.08942795157528024563, -0.3641732283464568787 ) ) ;
#60185 = CARTESIAN_POINT ( 'NONE',  ( 1.609563999208788898, 0.2869511693896439342, 0.09226456620623516014 ) ) ;
#60186 = CARTESIAN_POINT ( 'NONE',  ( 0.6102362204724416372, -0.4536011799217367080, 0.2665933059059888421 ) ) ;
#60187 = B_SPLINE_CURVE_WITH_KNOTS ( 'NONE', 3,
 ( #43271, #11317, #50010, #30665, #4165, #4574, #82431 ),
 .UNSPECIFIED., .F., .F.,
 ( 4, 3, 4 ),
 ( 1.734723475976807094E-18, 0.001246230184515552441, 0.002492489877932635954 ),
 .UNSPECIFIED. ) ;
#60188 = CARTESIAN_POINT ( 'NONE',  ( 0.3149606299212606708, -0.1870078740157480879, -0.4822834645669291653 ) ) ;
#60189 = CARTESIAN_POINT ( 'NONE',  ( -0.3996062992125986590, 0.1070741851644051723, -0.4245406824146981672 ) ) ;
#60190 = CARTESIAN_POINT ( 'NONE',  ( -0.5052493438320203589, -0.6692913385826771977, 0.1292274648535927661 ) ) ;
#60191 = CARTESIAN_POINT ( 'NONE',  ( -0.2867679344610365999, 0.2867679344610364889, -1.836614173228346747 ) ) ;
#60192 = CARTESIAN_POINT ( 'NONE',  ( 1.181102362204724976, -0.1870078740157480601, -0.3641732283464567677 ) ) ;
#60193 = CARTESIAN_POINT ( 'NONE',  ( -0.06561679790026180015, 0.05413385826771666132, 0.4176697321401328100 ) ) ;
#60194 = CARTESIAN_POINT ( 'NONE',  ( -0.3740157480314953431, 0.1660481256975885056, 0.3530559997133364547 ) ) ;
#60195 = CARTESIAN_POINT ( 'NONE',  ( -0.3215223097112853146, -0.08942795157528024563, -0.3641732283464568787 ) ) ;
#60196 = DIRECTION ( 'NONE',  ( -1.000000000000000000, 0.000000000000000000, 0.000000000000000000 ) ) ;
#60197 = CARTESIAN_POINT ( 'NONE',  ( 0.03937007874015833325, -0.5511811023622047445, 6.969142054262312111E-17 ) ) ;
#60198 = CARTESIAN_POINT ( 'NONE',  ( 0.2952755905511819101, 0.1660481256975883668, -0.3530559997133364547 ) ) ;
#60199 = CARTESIAN_POINT ( 'NONE',  ( -0.6430446194225716283, -0.3690944881889763329, 0.3153832671262228327 ) ) ;
#60200 = CARTESIAN_POINT ( 'NONE',  ( -0.3996062992125984925, -0.1070741851644056858, -0.7526246719160103460 ) ) ;
#60201 = CARTESIAN_POINT ( 'NONE',  ( -1.246719160104985846, -0.4281496062992127816, -0.4176697321401328100 ) ) ;
#60202 = LINE ( 'NONE', #34952, #58204 ) ;
#60203 = B_SPLINE_CURVE_WITH_KNOTS ( 'NONE', 3,
 ( #4962, #57106, #37763, #82801 ),
 .UNSPECIFIED., .F., .F.,
 ( 4, 4 ),
 ( 0.07469576999304877729, 0.07612553241189870534 ),
 .UNSPECIFIED. ) ;
#60204 = ORIENTED_EDGE ( 'NONE', *, *, #75249, .F. ) ;
#60205 = CARTESIAN_POINT ( 'NONE',  ( -0.9317585301837263412, -0.004921259842519576551, 0.3153832671262227771 ) ) ;
#60206 = CARTESIAN_POINT ( 'NONE',  ( -0.1968503937007867743, -0.6692913385826771977, 8.415575281601705876E-17 ) ) ;
#60207 = CARTESIAN_POINT ( 'NONE',  ( 0.3996062992125986035, 2.446882876249141962E-17, -1.220472440944881942 ) ) ;
#60208 = CARTESIAN_POINT ( 'NONE',  ( -0.6824146981627288167, 0.2306618581243848609, 0.2411417322834645549 ) ) ;
#60209 = CARTESIAN_POINT ( 'NONE',  ( -0.4724409448818914226, -0.1265901696524962816, -2.093175853018372834 ) ) ;
#60210 = CARTESIAN_POINT ( 'NONE',  ( 1.496062992125985147, -0.1870078740157479769, 0.4822834645669291653 ) ) ;
#60211 = CARTESIAN_POINT ( 'NONE',  ( 0.8267716535433078384, -0.6692913385826771977, 8.415575281601705876E-17 ) ) ;
#60212 = CARTESIAN_POINT ( 'NONE',  ( -2.362204724409448620, 0.000000000000000000, -2.474278114140802984E-14 ) ) ;
#60213 = CARTESIAN_POINT ( 'NONE',  ( 6.267877318470707138E-17, 0.03937007874015751446, 2.874015748031495843 ) ) ;
#60214 = CARTESIAN_POINT ( 'NONE',  ( 0.2489951994332677832, -0.1588014424199898911, 5.622579823899912732 ) ) ;
#60215 = CARTESIAN_POINT ( 'NONE',  ( -1.555118110236219930, 0.1660481256975885056, 0.3530559997133364547 ) ) ;
#60216 = CARTESIAN_POINT ( 'NONE',  ( -0.3996062992125986035, -7.340648628747425578E-17, -0.3543307086614173040 ) ) ;
#60217 = VERTEX_POINT ( 'NONE', #56906 ) ;
#60218 = CARTESIAN_POINT ( 'NONE',  ( -0.3215223097112853146, -0.08942795157528024563, -0.3641732283464568787 ) ) ;
#60219 = CARTESIAN_POINT ( 'NONE',  ( 4.797336870675656522E-17, -0.3917322834645670104, -2.118110236220472675 ) ) ;
#60220 = EDGE_LOOP ( 'NONE', ( #49162, #82201, #15014, #54302 ) ) ;
#60221 = CARTESIAN_POINT ( 'NONE',  ( 0.8595800524934390507, -0.05778040916215560624, -0.4822834645669293319 ) ) ;
#60222 = CARTESIAN_POINT ( 'NONE',  ( 0.1443569553805781891, -0.4281496062992124485, 0.4176697321401328655 ) ) ;
#60223 = CARTESIAN_POINT ( 'NONE',  ( -0.7874015748031489847, -0.1870078740157480879, -0.4822834645669291653 ) ) ;
#60224 = CARTESIAN_POINT ( 'NONE',  ( 1.456692913385827515, -0.6692913385826771977, 8.415575281601705876E-17 ) ) ;
#60225 = CARTESIAN_POINT ( 'NONE',  ( -0.7414698162729651543, -0.5511811023622046335, 0.09757992244046803654 ) ) ;
#60226 = CARTESIAN_POINT ( 'NONE',  ( -0.3458507752293906723, -0.3458507752293910609, -2.025590551181101873 ) ) ;
#60227 = CARTESIAN_POINT ( 'NONE',  ( 0.2821522309711292364, 0.2952755905511810774, -0.1292274648535930714 ) ) ;
#60228 = CARTESIAN_POINT ( 'NONE',  ( 0.5708661417322841158, -0.4536011799217368745, -0.2665933059059886201 ) ) ;
#60229 = CARTESIAN_POINT ( 'NONE',  ( -0.8333333333333323711, 0.2952755905511811885, 0.1292274648535926551 ) ) ;
#60230 = CARTESIAN_POINT ( 'NONE',  ( -0.1958661417322836440, 0.3392501089628016664, -1.510479371882202937 ) ) ;
#60231 = CARTESIAN_POINT ( 'NONE',  ( -1.062992125984250968, -0.6692913385826771977, 8.415575281601705876E-17 ) ) ;
#60232 = B_SPLINE_CURVE_WITH_KNOTS ( 'NONE', 3,
 ( #40579, #59933, #60354, #16585 ),
 .UNSPECIFIED., .F., .F.,
 ( 4, 4 ),
 ( 0.1818586053348001663, 0.1832800580269407509 ),
 .UNSPECIFIED. ) ;
#60233 = LINE ( 'NONE', #78780, #73470 ) ;
#60234 =( BOUNDED_CURVE ( )  B_SPLINE_CURVE ( 2, ( #6091, #19133, #57011, #58681, #57427, #622, #71321, #45208, #82707, #78062, #77644, #204, #51105 ),
 .UNSPECIFIED., .F., .F. ) 
 B_SPLINE_CURVE_WITH_KNOTS ( ( 3, 2, 2, 2, 2, 2, 3 ),
 ( 0.8375000000000000222, 0.8416666666666666741, 0.8458333333333333259, 0.8499999999999999778, 0.8541666666666666297, 0.8583333333333332815, 0.8625000000000000444 ),
 .UNSPECIFIED. ) 
 CURVE ( )  GEOMETRIC_REPRESENTATION_ITEM ( )  RATIONAL_B_SPLINE_CURVE ( ( 1.000000000000000000, 0.9659258262890683122, 1.000000000000000000, 0.9659258262890683122, 1.000000000000000000, 0.9659258262890683122, 1.000000000000000000, 0.9659258262890683122, 1.000000000000000000, 0.9659258262890683122, 1.000000000000000000, 0.9659258262890683122, 1.000000000000000000 ) ) 
 REPRESENTATION_ITEM ( '' )  );
#60235 = CARTESIAN_POINT ( 'NONE',  ( 1.069553805774278832, 0.2952755905511810774, -0.1292274648535930714 ) ) ;
#60236 = CARTESIAN_POINT ( 'NONE',  ( 1.161417322834646493, -0.4536011799217367080, 0.2665933059059888421 ) ) ;
#60237 = ORIENTED_EDGE ( 'NONE', *, *, #45798, .T. ) ;
#60238 = CARTESIAN_POINT ( 'NONE',  ( 0.1958661417322836718, -0.3392501089628017219, -2.923247662238532385 ) ) ;
#60239 = CARTESIAN_POINT ( 'NONE',  ( -0.5052493438320203589, 0.2952755905511810774, -0.1292274648535930714 ) ) ;
#60240 = ORIENTED_EDGE ( 'NONE', *, *, #34333, .F. ) ;
#60241 = AXIS2_PLACEMENT_3D ( 'NONE', #63592, #31599, #12671 ) ;
#60242 = CARTESIAN_POINT ( 'NONE',  ( 0.3149606299212603933, -0.1870078740157479769, 0.3641732283464567677 ) ) ;
#60243 = CARTESIAN_POINT ( 'NONE',  ( -1.253280839895012377, -0.05778040916215522460, 0.4822834645669289988 ) ) ;
#60244 = CARTESIAN_POINT ( 'NONE',  ( 0.8333333333333340365, 0.2952755905511810774, -0.1292274648535930714 ) ) ;
#60245 = CARTESIAN_POINT ( 'NONE',  ( 0.6758530183727039509, 0.2952755905511810774, -0.1292274648535930714 ) ) ;
#60246 = CARTESIAN_POINT ( 'NONE',  ( -0.2755905511811018171, 0.2952755905511811885, 0.000000000000000000 ) ) ;
#60247 = CARTESIAN_POINT ( 'NONE',  ( -0.3083989501312330295, -0.3162353388693409650, -0.4822834645669289433 ) ) ;
#60248 = CARTESIAN_POINT ( 'NONE',  ( -0.3392501089628019995, 0.1958661417322832277, -2.158136482939632561 ) ) ;
#60249 = CARTESIAN_POINT ( 'NONE',  ( -1.502624671916009680, -0.05778040916215560624, -0.4822834645669293319 ) ) ;
#60250 = CARTESIAN_POINT ( 'NONE',  ( -0.4986876640419939388, 0.2306618581243847221, -0.2411417322834647770 ) ) ;
#60251 = CARTESIAN_POINT ( 'NONE',  ( -0.6627296587926501115, 0.1771653543307087075, -0.09757992244046823083 ) ) ;
#60252 = CARTESIAN_POINT ( 'NONE',  ( 1.135170603674541256, -0.6692913385826773087, -0.1292274648535924053 ) ) ;
#60253 = CARTESIAN_POINT ( 'NONE',  ( 0.3917322834645670104, 2.398668435337828261E-17, -2.944881889763779181 ) ) ;
#60254 = CARTESIAN_POINT ( 'NONE',  ( -0.8595800524934373854, -0.3162353388693409650, -0.4822834645669289433 ) ) ;
#60255 = CARTESIAN_POINT ( 'NONE',  ( -0.5314960629921372526, 2.716535433070866645, 3.224202737261813834 ) ) ;
#60256 = CARTESIAN_POINT ( 'NONE',  ( 0.7677165354330716118, -0.5400638737290844871, 0.3530559997133364547 ) ) ;
#60257 = CARTESIAN_POINT ( 'NONE',  ( -0.1998031496062991907, -0.3460692066303959757, -1.955380577427821454 ) ) ;
#60258 = LINE ( 'NONE', #23908, #17396 ) ;
#60259 = CARTESIAN_POINT ( 'NONE',  ( 0.03937007874015833325, -0.6692913385826771977, 8.415575281601705876E-17 ) ) ;
#60260 = CARTESIAN_POINT ( 'NONE',  ( -1.338582677165353729, -0.1870078740157479769, 0.3641732283464567677 ) ) ;
#60262 = CARTESIAN_POINT ( 'NONE',  ( 0.000000000000000000, 2.755905511811024056, 0.000000000000000000 ) ) ;
#60261 = CARTESIAN_POINT ( 'NONE',  ( 0.9776902887139113929, -0.5511811023622048555, -0.09757992244046775898 ) ) ;
#60263 = CARTESIAN_POINT ( 'NONE',  ( 0.3458507752293908943, 0.3458507752293908943, -0.8444881889763780070 ) ) ;
#60264 = CARTESIAN_POINT ( 'NONE',  ( 1.266404199475066328, -0.2845877964562161244, -0.3641732283464567121 ) ) ;
#60265 = CARTESIAN_POINT ( 'NONE',  ( 1.377952755905512472, -0.6692913385826771977, 8.415575281601705876E-17 ) ) ;
#60266 = CARTESIAN_POINT ( 'NONE',  ( 0.3420746716998660508, 0.1974969037888705814, -0.5229658792650918597 ) ) ;
#60267 = CARTESIAN_POINT ( 'NONE',  ( -0.2624671916010490880, 0.2306618581243847221, -0.2411417322834647770 ) ) ;
#60268 = CARTESIAN_POINT ( 'NONE',  ( -0.9285414500055709786, 2.165354330708662012, -0.6299212598425202314 ) ) ;
#60269 = CARTESIAN_POINT ( 'NONE',  ( 1.509186351706037543, -0.3690944881889765550, -0.3153832671262227771 ) ) ;
#60270 = CARTESIAN_POINT ( 'NONE',  ( -0.2230971128608915943, -0.4281496062992127816, -0.4176697321401328100 ) ) ;
#60271 = CARTESIAN_POINT ( 'NONE',  ( -0.3949938075777411073, 0.1058382717557497660, -0.4245406824146981672 ) ) ;
#60272 = CARTESIAN_POINT ( 'NONE',  ( 1.076115485564305141, 0.2306618581243847221, -0.2411417322834647770 ) ) ;
#60273 = CARTESIAN_POINT ( 'NONE',  ( -0.01312335958005186876, -0.4281496062992124485, 0.4176697321401328655 ) ) ;
#60274 = CARTESIAN_POINT ( 'NONE',  ( 0.6692913385826778638, -0.5511811023622047445, 6.969142054262312111E-17 ) ) ;
#60275 = CARTESIAN_POINT ( 'NONE',  ( -0.4736394362785769641, 1.506176172253612000, -1.017181694652558699 ) ) ;
#60276 = CARTESIAN_POINT ( 'NONE',  ( 0.4330708661417329575, 0.1771653543307087630, 0.000000000000000000 ) ) ;
#60277 = CARTESIAN_POINT ( 'NONE',  ( -1.646981627296586703, -0.05778040916215522460, 0.4822834645669289988 ) ) ;
#60278 = CARTESIAN_POINT ( 'NONE',  ( 0.3996062992125984925, 0.1070741851644054637, -1.146325459317585116 ) ) ;
#60279 = CARTESIAN_POINT ( 'NONE',  ( 0.7020997375328090762, -0.3162353388693405765, 0.4822834645669290543 ) ) ;
#60280 = CARTESIAN_POINT ( 'NONE',  ( -0.3392501089628017219, -0.1958661417322836718, -0.9895013123359579499 ) ) ;
#60281 = CARTESIAN_POINT ( 'NONE',  ( -0.4724409448818891466, -0.1265901696525000564, -0.4376640419947506744 ) ) ;
#60282 = CARTESIAN_POINT ( 'NONE',  ( -0.3788256970788715927, 0.1002886991238273323, -1.587495037872346049E-17 ) ) ;
#60283 = CARTESIAN_POINT ( 'NONE',  ( -0.01968503937007793844, -0.4536011799217367080, 0.2665933059059888421 ) ) ;
#60284 = CARTESIAN_POINT ( 'NONE',  ( 0.2427821522309719648, -0.05778040916215522460, 0.4822834645669289988 ) ) ;
#60285 = CARTESIAN_POINT ( 'NONE',  ( 1.194225721784777594, -0.004921259842519576551, 0.3153832671262227771 ) ) ;
#60286 = CARTESIAN_POINT ( 'NONE',  ( -1.377952755905511140, 0.1771653543307087630, 0.000000000000000000 ) ) ;
#60287 = CARTESIAN_POINT ( 'NONE',  ( -1.266404199475064773, -0.3162353388693405765, 0.4822834645669290543 ) ) ;
#60288 = CARTESIAN_POINT ( 'NONE',  ( 0.6627296587926517768, -0.6692913385826773087, -0.1292274648535924053 ) ) ;
#60289 = CARTESIAN_POINT ( 'NONE',  ( 1.443569553805774897, -0.6046776061558809534, -0.2411417322834644161 ) ) ;
#60290 = CARTESIAN_POINT ( 'NONE',  ( 0.2362204724409449064, 0.4091458600556404646, -0.2211286089238845010 ) ) ;
#60291 = CARTESIAN_POINT ( 'NONE',  ( 0.4068241469816279987, -0.4281496062992127816, -0.4176697321401328100 ) ) ;
#60292 = CARTESIAN_POINT ( 'NONE',  ( -0.1998031496062991630, -0.3460692066303959202, 0.1725721784776902690 ) ) ;
#60293 = CARTESIAN_POINT ( 'NONE',  ( 1.535433070866142558, 0.2952755905511811885, 0.000000000000000000 ) ) ;
#60294 = CARTESIAN_POINT ( 'NONE',  ( 0.9055118110236227702, 0.2952755905511811885, 0.000000000000000000 ) ) ;
#60295 = CARTESIAN_POINT ( 'NONE',  ( -1.555118110236219930, 0.07958543189024085140, 0.2665933059059887866 ) ) ;
#60296 = CARTESIAN_POINT ( 'NONE',  ( 1.332020997375329197, -0.2845877964562159024, 0.3641732283464567677 ) ) ;
#60297 = CARTESIAN_POINT ( 'NONE',  ( 1.423884514435696413, -0.3162353388693409650, -0.4822834645669289433 ) ) ;
#60298 = CARTESIAN_POINT ( 'NONE',  ( -0.9251968503937002541, -0.4536011799217368745, -0.2665933059059886201 ) ) ;
#60299 = CARTESIAN_POINT ( 'NONE',  ( 1.587926509186352142, 0.05413385826771666132, 0.4176697321401328100 ) ) ;
#60300 = CARTESIAN_POINT ( 'NONE',  ( 0.4658792650918640033, -0.2845877964562159024, 0.3641732283464567677 ) ) ;
#60301 = CARTESIAN_POINT ( 'NONE',  ( 0.1640419947506569498, -0.3162353388693409650, -0.4822834645669289433 ) ) ;
#60302 = CARTESIAN_POINT ( 'NONE',  ( 1.227034120734908917, -0.6692913385826771977, 0.1292274648535927661 ) ) ;
#60303 = CARTESIAN_POINT ( 'NONE',  ( -0.3280839895013117347, 0.05413385826771626580, -0.4176697321401330321 ) ) ;
#60304 = ADVANCED_FACE ( 'NONE', ( #18625 ), #32072, .T. ) ;
#60305 = CARTESIAN_POINT ( 'NONE',  ( 0.1706036745406830368, -0.004921259842519576551, 0.3153832671262227771 ) ) ;
#60306 = CARTESIAN_POINT ( 'NONE',  ( 1.082677165354331228, -0.5400638737290844871, 0.3530559997133364547 ) ) ;
#60307 = CARTESIAN_POINT ( 'NONE',  ( -1.620734908136482577, 0.2952755905511811885, 0.1292274648535926551 ) ) ;
#60308 = CARTESIAN_POINT ( 'NONE',  ( -0.8989501312335946848, 0.2952755905511810774, -0.1292274648535930714 ) ) ;
#60310 = CARTESIAN_POINT ( 'NONE',  ( 0.1070741851644054915, -0.3996062992125985480, -0.8727034120734907807 ) ) ;
#60309 = CARTESIAN_POINT ( 'NONE',  ( -1.423884514435694859, -0.2845877964562159024, 0.3641732283464567677 ) ) ;
#60311 = CARTESIAN_POINT ( 'NONE',  ( -1.193521905106661674, 2.660739321503277841E-15, -0.3464511005275191513 ) ) ;
#60312 = CARTESIAN_POINT ( 'NONE',  ( -0.6233595800524928121, -0.3162353388693409650, -0.4822834645669289433 ) ) ;
#60313 = CARTESIAN_POINT ( 'NONE',  ( -0.02624671916010428221, -0.6046776061558807314, 0.2411417322834647770 ) ) ;
#60314 = CARTESIAN_POINT ( 'NONE',  ( -0.3460692066303960868, 0.1998031496062990242, -2.860892388451443669 ) ) ;
#60315 = CARTESIAN_POINT ( 'NONE',  ( 0.1974969037888704704, 0.3420746716998660508, -2.349081364829396446 ) ) ;
#60316 = ORIENTED_EDGE ( 'NONE', *, *, #68819, .T. ) ;
#60317 = CARTESIAN_POINT ( 'NONE',  ( 0.6824146981627303710, -0.5023911411419708095, 0.1820866141732285504 ) ) ;
#60318 = CARTESIAN_POINT ( 'NONE',  ( 0.3917322834645670104, -0.1049643490035303411, -0.8910761154855640909 ) ) ;
#60319 = CARTESIAN_POINT ( 'NONE',  ( 0.9120734908136489683, -0.6692913385826771977, 0.1292274648535927661 ) ) ;
#60320 = CARTESIAN_POINT ( 'NONE',  ( -0.2473181295769223131, 5.952911114587291371E-15, -0.3954985857520045833 ) ) ;
#60321 = CARTESIAN_POINT ( 'NONE',  ( -1.476377952755905110, -0.4536011799217368745, -0.2665933059059886201 ) ) ;
#60322 = CARTESIAN_POINT ( 'NONE',  ( 1.640419947506562393, -0.4281496062992124485, 0.4176697321401328655 ) ) ;
#60323 = CARTESIAN_POINT ( 'NONE',  ( -1.443569553805773564, -0.6046776061558807314, 0.2411417322834647770 ) ) ;
#60324 = CARTESIAN_POINT ( 'NONE',  ( -0.1958661417322834497, -0.3392501089628018884, -0.4606106054780034764 ) ) ;
#60325 = CARTESIAN_POINT ( 'NONE',  ( 0.1771653543307093182, -0.5400638737290845981, -0.3530559997133363437 ) ) ;
#60326 = CARTESIAN_POINT ( 'NONE',  ( -0.3083989501312330295, -0.08942795157527998196, 0.3641732283464567121 ) ) ;
#60327 = EDGE_CURVE ( 'NONE', #15966, #51592, #56014, .T. ) ;
#60328 = CARTESIAN_POINT ( 'NONE',  ( 0.9645669291338588858, 0.1660481256975885056, 0.3530559997133364547 ) ) ;
#60329 = CARTESIAN_POINT ( 'NONE',  ( -0.03280839895013062252, -0.6692913385826771977, 0.1292274648535927661 ) ) ;
#60330 = DIRECTION ( 'NONE',  ( -0.000000000000000000, -1.000000000000000000, 0.000000000000000000 ) ) ;
#60331 = DIRECTION ( 'NONE',  ( -1.000000000000000000, -3.412570772413389987E-16, 0.000000000000000000 ) ) ;
#60332 = CARTESIAN_POINT ( 'NONE',  ( -0.3392501089628017219, -0.1958661417322836995, -1.466554748852705092 ) ) ;
#60333 = CARTESIAN_POINT ( 'NONE',  ( 0.9973753280839902091, -0.6046776061558807314, 0.2411417322834647770 ) ) ;
#60334 = CARTESIAN_POINT ( 'NONE',  ( 0.08530183727034192087, -0.3162353388693409650, -0.4822834645669289433 ) ) ;
#60335 = CARTESIAN_POINT ( 'NONE',  ( -1.233595800524933894, -0.6046776061558809534, -0.2411417322834644161 ) ) ;
#60336 = CARTESIAN_POINT ( 'NONE',  ( -1.627296587926508442, 0.2306618581243848609, 0.2411417322834645549 ) ) ;
#60337 = CARTESIAN_POINT ( 'NONE',  ( 0.8923884514435703741, 0.2306618581243848609, 0.2411417322834645549 ) ) ;
#60338 = CARTESIAN_POINT ( 'NONE',  ( 0.2867679344610365999, 0.2867679344610365999, -0.3799212598425197318 ) ) ;
#60339 = CARTESIAN_POINT ( 'NONE',  ( -0.4265091863517051496, 0.2952755905511810774, -0.1292274648535930714 ) ) ;
#60340 = CARTESIAN_POINT ( 'NONE',  ( 0.6299212598425204535, -0.1870078740157480879, -0.4822834645669291653 ) ) ;
#60341 = CARTESIAN_POINT ( 'NONE',  ( -0.07874015748031421014, -0.1870078740157479769, 0.4822834645669291653 ) ) ;
#60342 = CARTESIAN_POINT ( 'NONE',  ( 0.5380577427821529035, -0.3690944881889763329, 0.3153832671262228327 ) ) ;
#60343 = CARTESIAN_POINT ( 'NONE',  ( -1.476377952755905110, -0.5400638737290845981, -0.3530559997133363437 ) ) ;
#60344 = CARTESIAN_POINT ( 'NONE',  ( 1.216659146022341931, 1.505269100445303598, 0.5216994034917036283 ) ) ;
#60345 = CARTESIAN_POINT ( 'NONE',  ( 0.6364829396325465405, -0.05778040916215522460, 0.4822834645669289988 ) ) ;
#60346 = CARTESIAN_POINT ( 'NONE',  ( -1.220472440944878834, 0.4405861044731111953, -0.5309055118110234117 ) ) ;
#60347 = EDGE_CURVE ( 'NONE', #36478, #63415, #23825, .T. ) ;
#60348 = CARTESIAN_POINT ( 'NONE',  ( -0.1049643490035302024, -0.3917322834645671215, -2.426509186351705427 ) ) ;
#60349 = VERTEX_POINT ( 'NONE', #24516 ) ;
#60350 = ORIENTED_EDGE ( 'NONE', *, *, #8023, .F. ) ;
#60351 = CARTESIAN_POINT ( 'NONE',  ( 1.148293963254593875, -0.6692913385826771977, 0.1292274648535927661 ) ) ;
#60352 = CARTESIAN_POINT ( 'NONE',  ( 0.4658792650918640033, -0.2845877964562159024, 0.3641732283464567677 ) ) ;
#60353 = DIRECTION ( 'NONE',  ( -3.491481338843132961E-15, -0.000000000000000000, 1.000000000000000000 ) ) ;
#60354 = CARTESIAN_POINT ( 'NONE',  ( 0.5314960629920919555, 2.742781089625999424, 3.250800428249180030 ) ) ;
#60355 = DIRECTION ( 'NONE',  ( -1.734723475976806848E-16, -1.000000000000000000, 0.000000000000000000 ) ) ;
#60356 = CARTESIAN_POINT ( 'NONE',  ( -0.3392501089628017219, -0.1958661417322836718, -1.082020997375328086 ) ) ;
#60357 = CARTESIAN_POINT ( 'NONE',  ( 0.3996062992125986035, -0.1070741851644052972, -1.920603674540682038 ) ) ;
#60358 = CARTESIAN_POINT ( 'NONE',  ( -0.8333333333333323711, 0.2952755905511811885, 0.1292274648535926551 ) ) ;
#60359 = CARTESIAN_POINT ( 'NONE',  ( -0.6430446194225716283, -0.4281496062992124485, 0.4176697321401328655 ) ) ;
#60360 = CARTESIAN_POINT ( 'NONE',  ( 1.187664041994751285, -0.3162353388693409650, -0.4822834645669289433 ) ) ;
#60361 = EDGE_LOOP ( 'NONE', ( #50804, #2304, #80328, #68884, #67375, #6596, #64065, #71103, #73493, #68430, #213, #58779, #14276, #77943 ) ) ;
#60362 = CARTESIAN_POINT ( 'NONE',  ( -1.594488188976377563, -0.5400638737290844871, 0.3530559997133364547 ) ) ;
#60363 = CARTESIAN_POINT ( 'NONE',  ( -1.057068326459881691, 1.248267542859002655, 0.3764357908784603524 ) ) ;
#60364 = CARTESIAN_POINT ( 'NONE',  ( 1.627296587926509996, -0.5023911411419708095, 0.1820866141732285504 ) ) ;
#60365 = CARTESIAN_POINT ( 'NONE',  ( 0.3996062992125985480, 2.446882876249141654E-17, -2.084645669291338876 ) ) ;
#60366 = CARTESIAN_POINT ( 'NONE',  ( -1.384514435695537005, -0.5511811023622048555, -0.09757992244046775898 ) ) ;
#60367 = CARTESIAN_POINT ( 'NONE',  ( 0.3917322834645669549, 0.1049643490035304660, 0.04068241469816277767 ) ) ;
#60368 = CARTESIAN_POINT ( 'NONE',  ( 0.3412073490813655186, -0.6046776061558809534, -0.2411417322834644161 ) ) ;
#60370 = CARTESIAN_POINT ( 'NONE',  ( 0.7773926554473647998, 8.471767977567108961E-16, -0.4445507791589058955 ) ) ;
#60369 = CARTESIAN_POINT ( 'NONE',  ( 1.404199475065617708, 0.05413385826771626580, -0.4176697321401330321 ) ) ;
#60371 = CARTESIAN_POINT ( 'NONE',  ( -0.8070866141732276899, -0.4536011799217367080, 0.2665933059059888421 ) ) ;
#60372 = CARTESIAN_POINT ( 'NONE',  ( 0.6167979002624679463, 0.05413385826771626580, -0.4176697321401330321 ) ) ;
#60373 = CARTESIAN_POINT ( 'NONE',  ( 1.489501312335958172, -0.08942795157528024563, -0.3641732283464568787 ) ) ;
#60374 = CARTESIAN_POINT ( 'NONE',  ( -0.1958661417322834497, -0.3392501089628018884, -1.090531865320523153 ) ) ;
#60375 = CARTESIAN_POINT ( 'NONE',  ( -0.7349081364829390672, 0.1283753931104746893, -0.1820866141732285504 ) ) ;
#60376 = CARTESIAN_POINT ( 'NONE',  ( 1.194225721784777594, 0.05413385826771666132, 0.4176697321401328100 ) ) ;
#60377 = CARTESIAN_POINT ( 'NONE',  ( 2.630268417803912406, 1.724409448818900570, -0.4359958488159719758 ) ) ;
#60378 = CARTESIAN_POINT ( 'NONE',  ( 0.3477690288713918276, 0.2952755905511811885, 0.1292274648535926551 ) ) ;
#60379 = CARTESIAN_POINT ( 'NONE',  ( -1.056430446194224881, -0.5511811023622046335, 0.09757992244046803654 ) ) ;
#60380 = CARTESIAN_POINT ( 'NONE',  ( -0.3018372703412066094, -0.004921259842519576551, 0.3153832671262227771 ) ) ;
#60381 = CARTESIAN_POINT ( 'NONE',  ( -0.3477690288713905509, -0.6692913385826771977, 0.1292274648535927661 ) ) ;
#60382 = CARTESIAN_POINT ( 'NONE',  ( -1.410761154855641575, -0.2845877964562161244, -0.3641732283464567121 ) ) ;
#60383 = CARTESIAN_POINT ( 'NONE',  ( 0.3917322834645670659, 2.398668435337828261E-17, -0.1148487121072984812 ) ) ;
#60384 = CARTESIAN_POINT ( 'NONE',  ( 0.2296587926509192634, -0.05778040916215560624, -0.4822834645669293319 ) ) ;
#60385 = CARTESIAN_POINT ( 'NONE',  ( 0.8768409086929784824, 4.512065407040659715E-16, 0.4118484887281966822 ) ) ;
#60386 = CARTESIAN_POINT ( 'NONE',  ( 0.4724409448818897572, -0.1265901696524988906, -1.605643044619422977 ) ) ;
#60387 = CARTESIAN_POINT ( 'NONE',  ( -0.8923884514435688198, 0.2306618581243847221, -0.2411417322834647770 ) ) ;
#60388 = AXIS2_PLACEMENT_3D ( 'NONE', #12106, #81585, #56700 ) ;
#60389 = CARTESIAN_POINT ( 'NONE',  ( -0.3871391076115479057, -0.2845877964562161244, -0.3641732283464567121 ) ) ;
#60390 = CARTESIAN_POINT ( 'NONE',  ( -1.213910761154854745, -0.6692913385826771977, 0.1292274648535927661 ) ) ;
#60391 = CARTESIAN_POINT ( 'NONE',  ( 0.2887139107611556010, 0.1283753931104746893, -0.1820866141732285504 ) ) ;
#60392 = CARTESIAN_POINT ( 'NONE',  ( -0.6561679790026240244, -0.5023911411419708095, 0.1820866141732285504 ) ) ;
#60393 = CARTESIAN_POINT ( 'NONE',  ( -1.089238845144356427, 0.05413385826771666132, 0.4176697321401328100 ) ) ;
#60394 = CARTESIAN_POINT ( 'NONE',  ( -1.548556430446193399, 0.2306618581243848609, 0.2411417322834645549 ) ) ;
#60395 = CARTESIAN_POINT ( 'NONE',  ( 1.548556430446194954, 0.2306618581243847221, -0.2411417322834647770 ) ) ;
#60396 = CARTESIAN_POINT ( 'NONE',  ( 0.4724409448818898682, 0.000000000000000000, -2.755905511811024056 ) ) ;
#60397 = CARTESIAN_POINT ( 'NONE',  ( 0.8136482939632553313, -0.5023911411419708095, -0.1820866141732282451 ) ) ;
#60398 = CARTESIAN_POINT ( 'NONE',  ( 0.5577427821522316087, -0.05778040916215522460, 0.4822834645669289988 ) ) ;
#60399 = EDGE_CURVE ( 'NONE', #2588, #58735, #20279, .T. ) ;
#60400 = CARTESIAN_POINT ( 'NONE',  ( 0.5288531115724313114, 1.522331584275864680, -0.5046369196611424357 ) ) ;
#60401 = CARTESIAN_POINT ( 'NONE',  ( 1.272965879265092637, -0.004921259842519576551, 0.3153832671262227771 ) ) ;
#60402 = VERTEX_POINT ( 'NONE', #45523 ) ;
#60403 = CARTESIAN_POINT ( 'NONE',  ( -0.3996062992125985480, -7.340648628747423112E-17, -2.635826771653543066 ) ) ;
#60404 = CARTESIAN_POINT ( 'NONE',  ( -1.122047244094487306, 0.07958543189024071263, -0.2665933059059888421 ) ) ;
#60405 = CARTESIAN_POINT ( 'NONE',  ( -0.4133858267716528645, -0.5400638737290844871, 0.3530559997133364547 ) ) ;
#60406 = CARTESIAN_POINT ( 'NONE',  ( 0.4461942257217855201, -0.6046776061558807314, 0.2411417322834647770 ) ) ;
#60407 = CARTESIAN_POINT ( 'NONE',  ( -1.666666666666665853, -0.004921259842519870586, -0.3153832671262229437 ) ) ;
#60408 = CARTESIAN_POINT ( 'NONE',  ( -0.3460692066303957537, -0.1998031496062994405, -2.019028871391076230 ) ) ;
#60409 = CARTESIAN_POINT ( 'NONE',  ( -1.515748031496062076, 0.1660481256975883668, -0.3530559997133364547 ) ) ;
#60410 = CARTESIAN_POINT ( 'NONE',  ( 0.5314960629921267055, -0.5400638737290844871, 0.3530559997133364547 ) ) ;
#60411 = CARTESIAN_POINT ( 'NONE',  ( -0.1049868766404193215, -0.6046776061558807314, 0.2411417322834647770 ) ) ;
#60412 = CARTESIAN_POINT ( 'NONE',  ( 1.312335958005249825, 0.2306618581243847221, -0.2411417322834647770 ) ) ;
#60413 = FACE_OUTER_BOUND ( 'NONE', #17410, .T. ) ;
#60414 = CARTESIAN_POINT ( 'NONE',  ( 4.893765752498283924E-17, -0.3996062992125986035, -1.968503937007873850 ) ) ;
#60415 = CARTESIAN_POINT ( 'NONE',  ( -0.3420746716998659953, -0.1974969037888706647, -0.9973753280839895430 ) ) ;
#60416 = CARTESIAN_POINT ( 'NONE',  ( -0.3996062992125986035, -7.340648628747425578E-17, -2.401574803149606474 ) ) ;
#60417 = DIRECTION ( 'NONE',  ( 0.000000000000000000, 0.000000000000000000, -1.000000000000000000 ) ) ;
#60418 = CARTESIAN_POINT ( 'NONE',  ( -0.3917322834645669549, -0.1049643490035306603, -0.1955380577427821009 ) ) ;
#60419 = CARTESIAN_POINT ( 'NONE',  ( -0.05249343832020938322, -0.5023911411419708095, -0.1820866141732282451 ) ) ;
#60420 = CARTESIAN_POINT ( 'NONE',  ( -0.5314960629921254842, -0.5400638737290845981, -0.3530559997133363437 ) ) ;
#60421 = CARTESIAN_POINT ( 'NONE',  ( 0.8595800524934390507, -0.05778040916215560624, -0.4822834645669293319 ) ) ;
#60422 = CARTESIAN_POINT ( 'NONE',  ( -9.674558042662122972E-17, 0.3949938075777409963, -2.124015748031495843 ) ) ;
#60423 = CARTESIAN_POINT ( 'NONE',  ( -0.2296587926509179312, -0.08942795157527998196, 0.3641732283464567121 ) ) ;
#60424 = CARTESIAN_POINT ( 'NONE',  ( -1.062992125984250968, -0.6692913385826771977, 8.415575281601705876E-17 ) ) ;
#60425 = CARTESIAN_POINT ( 'NONE',  ( -1.587926509186350810, 0.05413385826771626580, -0.4176697321401330321 ) ) ;
#60426 = CARTESIAN_POINT ( 'NONE',  ( -0.4724409448818895907, -0.1265901696524993070, -2.093175853018372834 ) ) ;
#60427 = CARTESIAN_POINT ( 'NONE',  ( 0.1716039559346060062, 0.3527845929029486682, -2.755905511811024056 ) ) ;
#60428 = EDGE_LOOP ( 'NONE', ( #16465, #75576, #1653, #75651, #48404, #60089, #21320, #40446, #75237, #81119, #35774, #73627, #18378, #24070, #45217, #19449, #62152, #75766, #63237, #77000 ) ) ;
#60429 = ORIENTED_EDGE ( 'NONE', *, *, #31514, .T. ) ;
#60430 = CARTESIAN_POINT ( 'NONE',  ( 0.9711286089238851948, 0.2306618581243848609, 0.2411417322834645549 ) ) ;
#60431 = CARTESIAN_POINT ( 'NONE',  ( -1.489501312335957062, -0.3162353388693409650, -0.4822834645669289433 ) ) ;
#60433 = CARTESIAN_POINT ( 'NONE',  ( -1.069553805774277722, -0.6692913385826773087, -0.1292274648535924053 ) ) ;
#60432 = CARTESIAN_POINT ( 'NONE',  ( -1.187664041994749731, -0.2845877964562159024, 0.3641732283464567677 ) ) ;
#60434 = CARTESIAN_POINT ( 'NONE',  ( 0.1958661417322836162, -0.3392501089628018329, -2.219140789205037656 ) ) ;
#60435 = CARTESIAN_POINT ( 'NONE',  ( 3.900966923095589678, 2.559055118110236560, -0.5314960629921260393 ) ) ;
#60436 = CARTESIAN_POINT ( 'NONE',  ( 1.240157480314961314, 0.1660481256975883668, -0.3530559997133364547 ) ) ;
#60437 = CARTESIAN_POINT ( 'NONE',  ( -1.496062992125983815, -0.1870078740157480879, -0.4822834645669291653 ) ) ;
#60438 = CARTESIAN_POINT ( 'NONE',  ( -0.01312335958005186876, -0.4281496062992124485, 0.4176697321401328655 ) ) ;
#60439 = CARTESIAN_POINT ( 'NONE',  ( -0.2690288713910754526, 0.2952755905511810774, -0.1292274648535930714 ) ) ;
#60440 = CARTESIAN_POINT ( 'NONE',  ( -1.391076115485563314, -0.6046776061558809534, -0.2411417322834644161 ) ) ;
#60441 = CARTESIAN_POINT ( 'NONE',  ( -0.1049643490035307020, 0.3917322834645669549, 0.2237532808398949025 ) ) ;
#60442 = CARTESIAN_POINT ( 'NONE',  ( 0.3937007874015754361, -0.1870078740157480879, -0.4822834645669291653 ) ) ;
#60443 = CARTESIAN_POINT ( 'NONE',  ( -0.1049643490035302024, -0.3917322834645671215, -1.796587926509185973 ) ) ;
#60444 = CARTESIAN_POINT ( 'NONE',  ( -1.351706036745406347, -0.3690944881889763329, 0.3153832671262228327 ) ) ;
#60445 = VERTEX_POINT ( 'NONE', #78381 ) ;
#60446 = CARTESIAN_POINT ( 'NONE',  ( 0.3949938075777411073, -0.1058382717557499464, -2.473753280839894764 ) ) ;
#60447 = ORIENTED_EDGE ( 'NONE', *, *, #3802, .F. ) ;
#60448 = CARTESIAN_POINT ( 'NONE',  ( -1.526728978123871538, 1.379587654853634326, 0.4473998187889915434 ) ) ;
#60449 = CARTESIAN_POINT ( 'NONE',  ( -1.541994750656167090, 0.2952755905511811885, 0.1292274648535926551 ) ) ;
#60450 = CARTESIAN_POINT ( 'NONE',  ( 0.1070741851644054915, -0.3996062992125986035, -0.5577427821522309426 ) ) ;
#60451 = CARTESIAN_POINT ( 'NONE',  ( -1.358267716535432434, 0.1660481256975883668, -0.3530559997133364547 ) ) ;
#60452 = CARTESIAN_POINT ( 'NONE',  ( 1.017199299814982805, 1.569430237215018176, -0.4736019971540504914 ) ) ;
#60453 = CARTESIAN_POINT ( 'NONE',  ( -1.013613127888308485, -2.191421614605370878E-15, 0.4445507791589071167 ) ) ;
#60454 = CARTESIAN_POINT ( 'NONE',  ( 0.0003067303408410983591, -0.3990339831394564274, -2.755905511811023612 ) ) ;
#60455 = EDGE_CURVE ( 'NONE', #50394, #23460, #22489, .T. ) ;
#60456 = CARTESIAN_POINT ( 'NONE',  ( 0.1958661417322836440, -0.3392501089628017219, -0.1765091863517061210 ) ) ;
#60457 = CARTESIAN_POINT ( 'NONE',  ( -0.4133858267716528645, -0.4536011799217367080, 0.2665933059059888421 ) ) ;
#60458 = CARTESIAN_POINT ( 'NONE',  ( -0.5774278215223089816, 0.1283753931104746893, -0.1820866141732285504 ) ) ;
#60459 = CARTESIAN_POINT ( 'NONE',  ( -1.410761154855641575, -0.3162353388693409650, -0.4822834645669289433 ) ) ;
#60460 = EDGE_CURVE ( 'NONE', #23246, #6583, #40484, .T. ) ;
#60461 = CARTESIAN_POINT ( 'NONE',  ( 1.056430446194226436, -0.6692913385826773087, -0.1292274648535924053 ) ) ;
#60462 = CARTESIAN_POINT ( 'NONE',  ( -0.8858267716535425107, -0.5400638737290844871, 0.3530559997133364547 ) ) ;
#60463 = EDGE_LOOP ( 'NONE', ( #72241, #1962, #19986, #44389 ) ) ;
#60464 = CARTESIAN_POINT ( 'NONE',  ( -1.410761154855641575, -0.3162353388693409650, -0.4822834645669289433 ) ) ;
#60465 = CARTESIAN_POINT ( 'NONE',  ( -1.606345848754414662, 0.2948621807332563738, 0.02311241260066472514 ) ) ;
#60466 =( NAMED_UNIT ( * ) SI_UNIT ( $, .STERADIAN. ) SOLID_ANGLE_UNIT ( ) );
#60467 = CARTESIAN_POINT ( 'NONE',  ( -0.4091458600556405756, 0.2362204724409446288, -1.128608923884514503 ) ) ;
#60468 = CARTESIAN_POINT ( 'NONE',  ( 2.113943251734093032, 1.379671404989100569, -0.4476723508032725563 ) ) ;
#60469 = CARTESIAN_POINT ( 'NONE',  ( 0.3392501089628018329, 0.1958661417322835607, -0.7532808398950130435 ) ) ;
#60470 = CARTESIAN_POINT ( 'NONE',  ( -0.1958661417322834220, -0.3392501089628018884, -2.512467191601049699 ) ) ;
#60471 = CARTESIAN_POINT ( 'NONE',  ( -0.6233595800524928121, -0.3162353388693409650, -0.4822834645669289433 ) ) ;
#60472 = CARTESIAN_POINT ( 'NONE',  ( 1.246719160104987623, 0.05413385826771626580, -0.4176697321401330321 ) ) ;
#60473 = CARTESIAN_POINT ( 'NONE',  ( 4.893765752498283308E-17, -0.3996062992125985480, 0.001968503937007844932 ) ) ;
#60475 = CARTESIAN_POINT ( 'NONE',  ( 0.2087913723976025926, 0.2087913723976026203, 0.1248231986745541033 ) ) ;
#60474 = CARTESIAN_POINT ( 'NONE',  ( -1.633858267716534529, -0.5400638737290845981, -0.3530559997133363437 ) ) ;
#60476 = CARTESIAN_POINT ( 'NONE',  ( -1.377952755905511140, 0.2952755905511811885, 0.000000000000000000 ) ) ;
#60477 = CARTESIAN_POINT ( 'NONE',  ( -0.8989501312335946848, 0.2952755905511810774, -0.1292274648535930714 ) ) ;
#60478 = CARTESIAN_POINT ( 'NONE',  ( -0.3392501089628019439, 0.1958661417322832554, -0.1062798968165861030 ) ) ;
#60479 = CARTESIAN_POINT ( 'NONE',  ( 0.4068241469816279987, -0.3690944881889765550, -0.3153832671262227771 ) ) ;
#60480 = CARTESIAN_POINT ( 'NONE',  ( -0.3917322834645669549, -0.1049643490035306603, -0.2880577427821522929 ) ) ;
#60481 = CARTESIAN_POINT ( 'NONE',  ( 0.4396325459317593221, 0.1771653543307087075, -0.09757992244046823083 ) ) ;
#60482 = CARTESIAN_POINT ( 'NONE',  ( 0.9842519685039375910, 0.1771653543307087630, 0.000000000000000000 ) ) ;
#60483 = CARTESIAN_POINT ( 'NONE',  ( 0.9973753280839902091, 0.2306618581243847221, -0.2411417322834647770 ) ) ;
#60484 = UNCERTAINTY_MEASURE_WITH_UNIT (LENGTH_MEASURE( 1.000000000000000082E-05 ), #6359, 'distance_accuracy_value', 'NONE');
#60485 = CARTESIAN_POINT ( 'NONE',  ( -0.4855643044619415427, -0.004921259842519870586, -0.3153832671262229437 ) ) ;
#60486 = CARTESIAN_POINT ( 'NONE',  ( 4.797336870675656522E-17, -0.3917322834645670104, -1.960629921259842368 ) ) ;
#60487 = CARTESIAN_POINT ( 'NONE',  ( -1.253280839895012377, -0.3162353388693409650, -0.4822834645669289433 ) ) ;
#60488 = EDGE_CURVE ( 'NONE', #66895, #77098, #35911, .T. ) ;
#60489 = CARTESIAN_POINT ( 'NONE',  ( -1.227034120734907141, -0.5511811023622048555, -0.09757992244046775898 ) ) ;
#60490 = CARTESIAN_POINT ( 'NONE',  ( -1.157146581871515012E-16, 0.4724409448818898682, -0.2342519685039370358 ) ) ;
#60491 = CARTESIAN_POINT ( 'NONE',  ( -0.9645669291338575535, 0.07958543189024071263, -0.2665933059059888421 ) ) ;
#60492 = CARTESIAN_POINT ( 'NONE',  ( -0.1246719160104980823, -0.6692913385826773087, -0.1292274648535924053 ) ) ;
#60493 = CARTESIAN_POINT ( 'NONE',  ( -0.7426113562967729953, 2.199547029020892275, -0.5309055118110235227 ) ) ;
#60494 = EDGE_CURVE ( 'NONE', #71941, #65199, #78940, .T. ) ;
#60495 = CARTESIAN_POINT ( 'NONE',  ( 0.5774278215223103139, -0.5023911411419708095, -0.1820866141732282451 ) ) ;
#60496 = CARTESIAN_POINT ( 'NONE',  ( -0.4593175853018366950, -0.004921259842519576551, 0.3153832671262227771 ) ) ;
#60497 = CARTESIAN_POINT ( 'NONE',  ( -0.8333333333333323711, 0.2952755905511811885, 0.1292274648535926551 ) ) ;
#60498 = DIRECTION ( 'NONE',  ( 0.000000000000000000, 0.000000000000000000, -1.000000000000000000 ) ) ;
#60499 = CARTESIAN_POINT ( 'NONE',  ( -1.157146581871515012E-16, 0.4724409448818898682, -1.966535433070865979 ) ) ;
#60500 = CARTESIAN_POINT ( 'NONE',  ( -0.02624671916010428221, 0.2306618581243847221, -0.2411417322834647770 ) ) ;
#60501 = ORIENTED_EDGE ( 'NONE', *, *, #56208, .T. ) ;
#60502 = ADVANCED_BREP_SHAPE_REPRESENTATION ( '', ( #59541, #22098 ), #14119 ) ;
#60503 = CARTESIAN_POINT ( 'NONE',  ( -0.3996062992125984925, -0.1070741851644056858, -1.697506561679789971 ) ) ;
#60504 = EDGE_CURVE ( 'NONE', #13567, #23658, #78800, .T. ) ;
#60505 = CARTESIAN_POINT ( 'NONE',  ( 1.404199475065617264, -0.4281496062992124485, 0.4176697321401328655 ) ) ;
#60506 = CARTESIAN_POINT ( 'NONE',  ( -0.1706036745406816491, -0.3690944881889763329, 0.3153832671262228327 ) ) ;
#60507 = CARTESIAN_POINT ( 'NONE',  ( 5.463695987328526437E-16, -0.1870078740157479769, 0.4822834645669291653 ) ) ;
#60508 = CARTESIAN_POINT ( 'NONE',  ( -1.594488188976377119, 0.1660481256975883668, -0.3530559997133364547 ) ) ;
#60509 = CARTESIAN_POINT ( 'NONE',  ( 1.646981627296588035, -0.3162353388693405765, 0.4822834645669290543 ) ) ;
#60510 = CARTESIAN_POINT ( 'NONE',  ( 1.220472440944882608, 0.2952755905511811885, 0.000000000000000000 ) ) ;
#60511 = CARTESIAN_POINT ( 'NONE',  ( -0.6824146981627291497, -0.5023911411419708095, -0.1820866141732282451 ) ) ;
#60512 = DIRECTION ( 'NONE',  ( 0.000000000000000000, 0.000000000000000000, 1.000000000000000000 ) ) ;
#60513 = CARTESIAN_POINT ( 'NONE',  ( -0.1998031496062991907, -0.3460692066303959757, -0.2230971128608923715 ) ) ;
#60514 = CARTESIAN_POINT ( 'NONE',  ( -0.2891555358219911054, 0.2891555358219909388, -0.01968503937007880233 ) ) ;
#60515 = CARTESIAN_POINT ( 'NONE',  ( -0.05073257145186574335, -0.3893108287682404134, -1.862014699505666341E-17 ) ) ;
#60516 = CARTESIAN_POINT ( 'NONE',  ( 1.351706036745407458, -0.3690944881889765550, -0.3153832671262227771 ) ) ;
#60517 = CARTESIAN_POINT ( 'NONE',  ( -1.607611548556429737, -0.6692913385826771977, 0.1292274648535927661 ) ) ;
#60518 = CARTESIAN_POINT ( 'NONE',  ( 1.010498687664042716, 0.05413385826771626580, -0.4176697321401330321 ) ) ;
#60519 = CARTESIAN_POINT ( 'NONE',  ( 0.1958661417322836440, -0.3392501089628017219, -2.381233595800524849 ) ) ;
#60520 = CARTESIAN_POINT ( 'NONE',  ( 1.122047244094488860, -0.4536011799217368745, -0.2665933059059886201 ) ) ;
#60521 = CARTESIAN_POINT ( 'NONE',  ( -0.04593175853018302557, 0.2952755905511811885, 0.1292274648535926551 ) ) ;
#60522 = CARTESIAN_POINT ( 'NONE',  ( -0.3477690288713902178, 0.2952755905511810774, -0.1292274648535930714 ) ) ;
#60523 = FACE_OUTER_BOUND ( 'NONE', #17701, .T. ) ;
#60524 = CARTESIAN_POINT ( 'NONE',  ( -0.4724409448818898682, -8.678599364036362592E-17, -0.8267716535433070613 ) ) ;
#60525 = CARTESIAN_POINT ( 'NONE',  ( 3.892840969167625786, 2.712230453466949687, 0.5314960629921260393 ) ) ;
#60526 = CARTESIAN_POINT ( 'NONE',  ( 0.4330708661417329575, -0.5511811023622047445, 6.969142054262312111E-17 ) ) ;
#60527 = EDGE_LOOP ( 'NONE', ( #4854, #62683, #34466, #55954, #27163, #523 ) ) ;
#60528 = CARTESIAN_POINT ( 'NONE',  ( 0.3917322834645670659, 2.398668435337828261E-17, -0.2723290270679284419 ) ) ;
#60529 = ORIENTED_EDGE ( 'NONE', *, *, #40891, .T. ) ;
#60530 = CARTESIAN_POINT ( 'NONE',  ( -0.5314960629921254842, -0.5400638737290845981, -0.3530559997133363437 ) ) ;
#60531 = CARTESIAN_POINT ( 'NONE',  ( 0.7349081364829402885, -0.6046776061558809534, -0.2411417322834644161 ) ) ;
#60532 = CARTESIAN_POINT ( 'NONE',  ( 0.1509186351706045259, -0.05778040916215560624, -0.4822834645669293319 ) ) ;
#60533 = CARTESIAN_POINT ( 'NONE',  ( -0.4724409448818890911, -0.1870078740157480601, -0.3641732283464567677 ) ) ;
#60534 = CARTESIAN_POINT ( 'NONE',  ( 0.8333333333333340365, -0.6692913385826771977, 0.1292274648535927661 ) ) ;
#60535 = CARTESIAN_POINT ( 'NONE',  ( -0.8792650918635160906, -0.4281496062992124485, 0.4176697321401328655 ) ) ;
#60536 = CARTESIAN_POINT ( 'NONE',  ( -0.5183727034120726440, -0.6692913385826773087, -0.1292274648535924053 ) ) ;
#60537 = CARTESIAN_POINT ( 'NONE',  ( -0.7742782152230965886, 0.05413385826771666132, 0.4176697321401328100 ) ) ;
#60538 = CARTESIAN_POINT ( 'NONE',  ( 1.017060367454068581, -0.05778040916215560624, -0.4822834645669293319 ) ) ;
#60539 = CARTESIAN_POINT ( 'NONE',  ( 0.7217847769028878924, -0.4281496062992127816, -0.4176697321401328100 ) ) ;
#60540 = CARTESIAN_POINT ( 'NONE',  ( 0.8792650918635177559, 0.05413385826771666132, 0.4176697321401328100 ) ) ;
#60541 = CARTESIAN_POINT ( 'NONE',  ( -0.1958661417322834220, -0.3392501089628018884, -0.6876640419947506189 ) ) ;
#60542 = CARTESIAN_POINT ( 'NONE',  ( 0.2034120734908144990, -0.5511811023622046335, 0.09757992244046803654 ) ) ;
#60543 = VERTEX_POINT ( 'NONE', #34168 ) ;
#60544 = CARTESIAN_POINT ( 'NONE',  ( -0.3949938075777409963, -7.255918531996591613E-17, -0.8267716535433070613 ) ) ;
#60545 = EDGE_LOOP ( 'NONE', ( #66642, #47580, #29470, #524 ) ) ;
#60546 = CARTESIAN_POINT ( 'NONE',  ( -0.9317585301837263412, -0.004921259842519576551, 0.3153832671262227771 ) ) ;
#60547 = CARTESIAN_POINT ( 'NONE',  ( -0.4133858267716528645, -0.5400638737290844871, 0.3530559997133364547 ) ) ;
#60548 = CARTESIAN_POINT ( 'NONE',  ( -1.510944988927603871, 1.132458528238634798, 0.2471620315916907840 ) ) ;
#60549 = CARTESIAN_POINT ( 'NONE',  ( -0.4593175853018366950, 0.05413385826771666132, 0.4176697321401328100 ) ) ;
#60550 = CARTESIAN_POINT ( 'NONE',  ( -0.2362204724409442680, -0.1870078740157480879, -0.4822834645669291653 ) ) ;
#60551 = CARTESIAN_POINT ( 'NONE',  ( -1.443569553805773564, 0.2306618581243847221, -0.2411417322834647770 ) ) ;
#60552 = ADVANCED_FACE ( 'NONE', ( #32488 ), #52673, .F. ) ;
#60553 = CARTESIAN_POINT ( 'NONE',  ( -1.522309711286088607, 0.2306618581243847221, -0.2411417322834647770 ) ) ;
#60554 = CARTESIAN_POINT ( 'NONE',  ( 1.095800524934383846, -0.08942795157528024563, -0.3641732283464568787 ) ) ;
#60555 = CARTESIAN_POINT ( 'NONE',  ( -0.4724409448818898682, -8.678599364036362592E-17, -0.4311023622047244208 ) ) ;
#60556 = CARTESIAN_POINT ( 'NONE',  ( 0.2407687881342162883, 0.1709459579824098019, 5.655073192166721441 ) ) ;
#60557 = CARTESIAN_POINT ( 'NONE',  ( 0.3608923884514443348, 0.1771653543307087075, -0.09757992244046823083 ) ) ;
#60558 = CARTESIAN_POINT ( 'NONE',  ( -0.01312335958005186876, 0.05413385826771626580, -0.4176697321401330321 ) ) ;
#60559 = CARTESIAN_POINT ( 'NONE',  ( 0.4002624671916016896, -0.05778040916215522460, 0.4822834645669289988 ) ) ;
#60560 = EDGE_LOOP ( 'NONE', ( #58801, #79914, #76983, #23913 ) ) ;
#60561 = CARTESIAN_POINT ( 'NONE',  ( -0.1998031496062994683, 0.3460692066303958092, -1.745406824146981561 ) ) ;
#60562 = CARTESIAN_POINT ( 'NONE',  ( -0.5839895013123352907, 0.2066929133858267098, -0.1054918080437494132 ) ) ;
#60563 = ORIENTED_EDGE ( 'NONE', *, *, #62867, .F. ) ;
#60564 = CARTESIAN_POINT ( 'NONE',  ( 0.1070741851644053388, 0.3996062992125986035, -1.330052493438320216 ) ) ;
#60565 = CARTESIAN_POINT ( 'NONE',  ( 4.893765752498283308E-17, -0.3996062992125985480, -0.4704724409448819422 ) ) ;
#60566 = CARTESIAN_POINT ( 'NONE',  ( -0.4265091863517051496, 0.1771653543307087075, -0.09757992244046823083 ) ) ;
#60567 = CARTESIAN_POINT ( 'NONE',  ( -0.5708661417322828946, 0.1660481256975883668, -0.3530559997133364547 ) ) ;
#60568 = CARTESIAN_POINT ( 'NONE',  ( 0.2362204724409451007, -0.4091458600556402980, 0.06561679790026246628 ) ) ;
#60569 = CARTESIAN_POINT ( 'NONE',  ( -0.3917322834645670104, -7.196005306013484475E-17, -2.643700787401574548 ) ) ;
#60570 = CARTESIAN_POINT ( 'NONE',  ( 1.614173228346457378, -0.6692913385826771977, 8.415575281601705876E-17 ) ) ;
#60571 = CARTESIAN_POINT ( 'NONE',  ( 0.7152230971128614723, -0.3162353388693409650, -0.4822834645669289433 ) ) ;
#60572 = CARTESIAN_POINT ( 'NONE',  ( 0.8530183727034128527, -0.4281496062992124485, 0.4176697321401328655 ) ) ;
#60573 = CARTESIAN_POINT ( 'NONE',  ( -0.7808398950131222316, -0.2845877964562161244, -0.3641732283464567121 ) ) ;
#60574 = CARTESIAN_POINT ( 'NONE',  ( 0.07217847769028949700, -0.05778040916215560624, -0.4822834645669293319 ) ) ;
#60575 = CARTESIAN_POINT ( 'NONE',  ( 0.4091458600556403535, 0.2362204724409449896, -1.940288713910761187 ) ) ;
#60576 = CARTESIAN_POINT ( 'NONE',  ( -0.01968503937007793844, 0.07958543189024071263, -0.2665933059059888421 ) ) ;
#60577 = CARTESIAN_POINT ( 'NONE',  ( -0.3871391076115479057, -0.3162353388693409650, -0.4822834645669289433 ) ) ;
#60578 = CARTESIAN_POINT ( 'NONE',  ( -0.1058382717557503072, 0.3949938075777408852, -1.815616797900262869 ) ) ;
#60579 = CARTESIAN_POINT ( 'NONE',  ( 1.535433070866142335, -0.5511811023622047445, 6.969142054262312111E-17 ) ) ;
#60580 = CARTESIAN_POINT ( 'NONE',  ( -0.01968503937007793844, -0.4536011799217367080, 0.2665933059059888421 ) ) ;
#60581 = CARTESIAN_POINT ( 'NONE',  ( -0.7426113562971995430, 1.972848275015057995, -0.5309055118110235227 ) ) ;
#60582 = CARTESIAN_POINT ( 'NONE',  ( -1.148293963254592542, -0.6692913385826773087, -0.1292274648535924053 ) ) ;
#60583 = CONICAL_SURFACE ( 'NONE', #64598, 0.1190944881889763746, 0.8726646259971648778 ) ;
#60584 = CARTESIAN_POINT ( 'NONE',  ( -0.8070866141732276899, 0.07958543189024071263, -0.2665933059059888421 ) ) ;
#60585 = CARTESIAN_POINT ( 'NONE',  ( 0.1181102362204724532, -0.04921259842519688094, 0.08523872084492505052 ) ) ;
#60586 = CARTESIAN_POINT ( 'NONE',  ( -1.082677165354329896, 0.1660481256975885056, 0.3530559997133364547 ) ) ;
#60587 = CARTESIAN_POINT ( 'NONE',  ( 0.1377952755905518800, 0.1660481256975883668, -0.3530559997133364547 ) ) ;
#60588 = CARTESIAN_POINT ( 'NONE',  ( -0.3996062992125986590, 0.1070741851644051723, -2.629265091863517423 ) ) ;
#60589 = CARTESIAN_POINT ( 'NONE',  ( 0.3917322834645668994, -0.1049643490035303134, -2.553786458496376088 ) ) ;
#60590 = CARTESIAN_POINT ( 'NONE',  ( 0.5314960629920854052, 2.712196231959916659, 3.892860353355080072 ) ) ;
#60591 = CARTESIAN_POINT ( 'NONE',  ( 0.5249343832021005074, -0.5023911411419708095, 0.1820866141732285504 ) ) ;
#60592 = CARTESIAN_POINT ( 'NONE',  ( 0.9186351706036751663, -0.6046776061558807314, 0.2411417322834647770 ) ) ;
#60593 = CARTESIAN_POINT ( 'NONE',  ( -1.240157480314959759, 0.07958543189024085140, 0.2665933059059887866 ) ) ;
#60594 =( BOUNDED_CURVE ( )  B_SPLINE_CURVE ( 2, ( #69801, #63074, #36985, #12557, #18865, #55916, #38216, #31073, #76124, #56741, #69394, #44514, #23940 ),
 .UNSPECIFIED., .F., .F. ) 
 B_SPLINE_CURVE_WITH_KNOTS ( ( 3, 2, 2, 2, 2, 2, 3 ),
 ( 0.2642401855438917813, 0.2651515151515151381, 0.2689393939393939226, 0.2727272727272727071, 0.2765151515151514916, 0.2803030303030302761, 0.2812143599106537439 ),
 .UNSPECIFIED. ) 
 CURVE ( )  GEOMETRIC_REPRESENTATION_ITEM ( )  RATIONAL_B_SPLINE_CURVE ( ( 0.9875488213027530104, 0.9918020599134685922, 1.000000000000000000, 0.9659258262890683122, 1.000000000000000000, 0.9659258262890683122, 1.000000000000000000, 0.9659258262890683122, 1.000000000000000000, 0.9659258262890683122, 1.000000000000000000, 0.9918020599134677040, 0.9875488213027521223 ) ) 
 REPRESENTATION_ITEM ( '' )  );
#60595 = CARTESIAN_POINT ( 'NONE',  ( 1.108923884514436686, -0.3162353388693409650, -0.4822834645669289433 ) ) ;
#60596 = CARTESIAN_POINT ( 'NONE',  ( -1.502624671916009680, -0.08942795157528024563, -0.3641732283464568787 ) ) ;
#60597 = CARTESIAN_POINT ( 'NONE',  ( -0.3149606299212590610, -0.1870078740157479769, 0.4822834645669291653 ) ) ;
#60598 = CARTESIAN_POINT ( 'NONE',  ( 0.2559055118110243332, 0.07958543189024085140, 0.2665933059059887866 ) ) ;
#60599 = CARTESIAN_POINT ( 'NONE',  ( 0.5314960629921264834, 0.07958543189024071263, -0.2665933059059888421 ) ) ;
#60600 = CIRCLE ( 'NONE', #51187, 0.1978346456692914035 ) ;
#60601 = CARTESIAN_POINT ( 'NONE',  ( 0.1181102362204730916, 0.2952755905511811885, 0.000000000000000000 ) ) ;
#60602 = CARTESIAN_POINT ( 'NONE',  ( 0.3996062992125986035, -0.1070741851644052972, -0.5032808398950130435 ) ) ;
#60603 = CARTESIAN_POINT ( 'NONE',  ( -0.5118110236220466680, -0.6692913385826771977, 8.415575281601705876E-17 ) ) ;
#60604 = CARTESIAN_POINT ( 'NONE',  ( 0.1049643490035303689, 0.3917322834645670104, -1.810367454068241511 ) ) ;
#60605 = CARTESIAN_POINT ( 'NONE',  ( 1.220472440944882386, -0.5511811023622047445, 6.969142054262312111E-17 ) ) ;
#60606 = CARTESIAN_POINT ( 'NONE',  ( -0.03937007874015669567, 0.2952755905511811885, 0.000000000000000000 ) ) ;
#60607 = CARTESIAN_POINT ( 'NONE',  ( -0.2230971128608915943, 0.05413385826771666132, 0.4176697321401328100 ) ) ;
#60608 = CARTESIAN_POINT ( 'NONE',  ( -0.2230971128608915943, -0.004921259842519576551, 0.3153832671262227771 ) ) ;
#60609 = CARTESIAN_POINT ( 'NONE',  ( 1.207349081364829990, 0.2306618581243848609, 0.2411417322834645549 ) ) ;
#60610 = CARTESIAN_POINT ( 'NONE',  ( -0.3543307086614165824, 0.1771653543307087630, 0.000000000000000000 ) ) ;
#60611 = CARTESIAN_POINT ( 'NONE',  ( 0.2230971128608932319, -0.4281496062992124485, 0.4176697321401328655 ) ) ;
#60612 = CARTESIAN_POINT ( 'NONE',  ( -0.9120734908136475250, 0.1771653543307087630, 0.09757992244046791164 ) ) ;
#60613 = CARTESIAN_POINT ( 'NONE',  ( 0.1998031496062992463, 0.3460692066303959202, -0.8510498687664042050 ) ) ;
#60614 = CARTESIAN_POINT ( 'NONE',  ( -1.076115485564303809, -0.6046776061558809534, -0.2411417322834644161 ) ) ;
#60615 = CARTESIAN_POINT ( 'NONE',  ( 0.000000000000000000, -0.04921259842519685318, -0.08523872084492505052 ) ) ;
#60616 = ORIENTED_EDGE ( 'NONE', *, *, #70755, .F. ) ;
#60617 = CARTESIAN_POINT ( 'NONE',  ( -1.213910761154854745, 0.1771653543307087075, -0.09757992244046823083 ) ) ;
#60618 = CARTESIAN_POINT ( 'NONE',  ( -0.4396325459317579898, 0.2952755905511811885, 0.1292274648535926551 ) ) ;
#60619 = CARTESIAN_POINT ( 'NONE',  ( 0.3900885325447117635, 0.05060072268091646286, -1.220472440944882164 ) ) ;
#60620 = CARTESIAN_POINT ( 'NONE',  ( -1.338582677165353729, -0.1870078740157479769, 0.4822834645669291653 ) ) ;
#60621 = CARTESIAN_POINT ( 'NONE',  ( 0.6299212598424790421, 2.755905511811024056, 3.886287458032468667 ) ) ;
#60622 = CARTESIAN_POINT ( 'NONE',  ( 1.502624671916010790, -0.05778040916215522460, 0.4822834645669289988 ) ) ;
#60623 = CARTESIAN_POINT ( 'NONE',  ( 0.6627296587926517768, -0.6692913385826773087, -0.1292274648535924053 ) ) ;
#60624 = CARTESIAN_POINT ( 'NONE',  ( 0.4177787735907000366, 0.3937007874015748254, -1.559171609364239375 ) ) ;
#60625 = CARTESIAN_POINT ( 'NONE',  ( 0.2896728340831398740, -0.05829427551933642759, 5.869670624399382142 ) ) ;
#60626 = CARTESIAN_POINT ( 'NONE',  ( -1.666666666666665853, 0.05413385826771626580, -0.4176697321401330321 ) ) ;
#60627 = CARTESIAN_POINT ( 'NONE',  ( -0.2925321140481930704, -0.2925321140481933480, -0.6889763779527556808 ) ) ;
#60628 = ORIENTED_EDGE ( 'NONE', *, *, #13591, .T. ) ;
#60629 = CARTESIAN_POINT ( 'NONE',  ( -0.6561679790026240244, 0.1283753931104746893, -0.1820866141732285504 ) ) ;
#60630 = CARTESIAN_POINT ( 'NONE',  ( -0.1958661417322834220, -0.3392501089628018884, -2.419947506561679784 ) ) ;
#60631 = VERTEX_POINT ( 'NONE', #2184 ) ;
#60632 = CARTESIAN_POINT ( 'NONE',  ( 0.9514435695538062676, -0.05778040916215522460, 0.4822834645669289988 ) ) ;
#60633 = CARTESIAN_POINT ( 'NONE',  ( 0.08530183727034192087, -0.3162353388693409650, -0.4822834645669289433 ) ) ;
#60634 = CARTESIAN_POINT ( 'NONE',  ( -0.6233595800524928121, -0.3162353388693409650, -0.4822834645669289433 ) ) ;
#60635 = CARTESIAN_POINT ( 'NONE',  ( 1.541994750656168645, 0.2952755905511810774, -0.1292274648535930714 ) ) ;
#60636 = CARTESIAN_POINT ( 'NONE',  ( -1.259842519685038686, -0.1870078740157480601, -0.3641732283464567677 ) ) ;
#60637 = DIRECTION ( 'NONE',  ( -1.000000000000000000, -3.096699300667737957E-16, 1.692413147294446216E-16 ) ) ;
#60638 = CARTESIAN_POINT ( 'NONE',  ( 0.2755905511811031494, 0.2952755905511811885, 0.000000000000000000 ) ) ;
#60639 = VECTOR ( 'NONE', #43972, 39.37007874015748143 ) ;
#60640 = CARTESIAN_POINT ( 'NONE',  ( -0.7808398950131222316, -0.3162353388693409650, -0.4822834645669289433 ) ) ;
#60641 = CARTESIAN_POINT ( 'NONE',  ( -0.2867679344610364334, -0.2867679344610368219, -1.556411130412386656 ) ) ;
#60642 = CARTESIAN_POINT ( 'NONE',  ( -1.371391076115484609, -0.6692913385826771977, 0.1292274648535927661 ) ) ;
#60643 = CARTESIAN_POINT ( 'NONE',  ( 0.1807970329289269873, 1.098498331261034133, -2.841281961169017656 ) ) ;
#60644 = CARTESIAN_POINT ( 'NONE',  ( 1.089238845144357759, 0.05413385826771626580, -0.4176697321401330321 ) ) ;
#60645 = CARTESIAN_POINT ( 'NONE',  ( 1.095800524934383846, -0.08942795157528024563, -0.3641732283464568787 ) ) ;
#60646 = ORIENTED_EDGE ( 'NONE', *, *, #45034, .T. ) ;
#60647 = CARTESIAN_POINT ( 'NONE',  ( -0.3949938075777409408, -0.1058382717557502933, 0.1115485564304461441 ) ) ;
#60648 = CARTESIAN_POINT ( 'NONE',  ( -0.6233595800524928121, -0.3162353388693409650, -0.4822834645669289433 ) ) ;
#60649 = ORIENTED_EDGE ( 'NONE', *, *, #48765, .T. ) ;
#60650 = CARTESIAN_POINT ( 'NONE',  ( 0.2230971128608929543, -0.004921259842519870586, -0.3153832671262229437 ) ) ;
#60651 = CARTESIAN_POINT ( 'NONE',  ( -1.135170603674539924, -0.6692913385826771977, 0.1292274648535927661 ) ) ;
#60652 = CARTESIAN_POINT ( 'NONE',  ( 1.082677165354331228, -0.5400638737290844871, 0.3530559997133364547 ) ) ;
#60653 = CARTESIAN_POINT ( 'NONE',  ( 1.017060367454068581, -0.05778040916215560624, -0.4822834645669293319 ) ) ;
#60654 = EDGE_CURVE ( 'NONE', #80968, #41294, #38803, .T. ) ;
#60655 = CARTESIAN_POINT ( 'NONE',  ( -0.2559055118110230564, 0.1660481256975883668, -0.3530559997133364547 ) ) ;
#60656 = CARTESIAN_POINT ( 'NONE',  ( -0.9973753280839886548, 0.2306618581243848609, 0.2411417322834645549 ) ) ;
#60657 = CARTESIAN_POINT ( 'NONE',  ( -0.3917322834645669549, -0.1049643490035306603, -2.335301837270341352 ) ) ;
#60658 = CARTESIAN_POINT ( 'NONE',  ( -1.528871391076114250, 0.2952755905511810774, -0.1292274648535930714 ) ) ;
#60659 = CARTESIAN_POINT ( 'NONE',  ( -0.5314960629921250401, 0.1660481256975885056, 0.3530559997133364547 ) ) ;
#60660 = CARTESIAN_POINT ( 'NONE',  ( -0.6758530183727028406, 0.1771653543307087630, 0.09757992244046791164 ) ) ;
#60661 = CARTESIAN_POINT ( 'NONE',  ( 1.417322834645670104, -0.1870078740157480879, -0.4822834645669291653 ) ) ;
#60662 = VECTOR ( 'NONE', #7946, 39.37007874015748143 ) ;
#60663 = CARTESIAN_POINT ( 'NONE',  ( 1.568241469816273659, -0.05778040916215560624, -0.4822834645669293319 ) ) ;
#60664 = CARTESIAN_POINT ( 'NONE',  ( -0.8464566929133852113, -0.5400638737290845981, -0.3530559997133363437 ) ) ;
#60665 = CARTESIAN_POINT ( 'NONE',  ( -0.2925321140481932369, 0.2925321140481931259, -0.09645669291338582196 ) ) ;
#60666 = CARTESIAN_POINT ( 'NONE',  ( 0.8989501312335963501, -0.6692913385826773087, -0.1292274648535924053 ) ) ;
#60667 = CARTESIAN_POINT ( 'NONE',  ( 0.1070741851644054915, -0.3996062992125986035, -1.660104986876640210 ) ) ;
#60668 = DIRECTION ( 'NONE',  ( -3.096699300667737957E-16, 1.000000000000000000, -0.000000000000000000 ) ) ;
#60669 = CARTESIAN_POINT ( 'NONE',  ( -0.006561679790025524116, -0.05778040916215560624, -0.4822834645669293319 ) ) ;
#60670 = CARTESIAN_POINT ( 'NONE',  ( -1.207349081364828436, -0.5023911411419708095, 0.1820866141732285504 ) ) ;
#60671 = CARTESIAN_POINT ( 'NONE',  ( 0.9645669291338591078, -0.4536011799217368745, -0.2665933059059886201 ) ) ;
#60672 = CARTESIAN_POINT ( 'NONE',  ( -0.1265901696524986964, -0.4724409448818899238, -0.6213910761154856077 ) ) ;
#60673 = CARTESIAN_POINT ( 'NONE',  ( 1.141732283464567788, -0.5511811023622047445, 6.969142054262312111E-17 ) ) ;
#60674 = CARTESIAN_POINT ( 'NONE',  ( 0.9645669291338588858, 0.1660481256975885056, 0.3530559997133364547 ) ) ;
#60675 = CARTESIAN_POINT ( 'NONE',  ( -0.1058382717557497660, -0.3949938075777411073, -0.6213910761154856077 ) ) ;
#60676 = CARTESIAN_POINT ( 'NONE',  ( -0.4593175853018366950, 0.05413385826771666132, 0.4176697321401328100 ) ) ;
#60677 = CARTESIAN_POINT ( 'NONE',  ( 0.4606732211681152100, 1.541615089183626441, 0.5309055118110234117 ) ) ;
#60678 = CARTESIAN_POINT ( 'NONE',  ( 1.397637795275591177, -0.4536011799217367080, 0.2665933059059888421 ) ) ;
#60679 = CARTESIAN_POINT ( 'NONE',  ( -0.4461942257217840213, 0.2306618581243848609, 0.2411417322834645549 ) ) ;
#60680 = CARTESIAN_POINT ( 'NONE',  ( 4.837279021331061486E-17, -0.3949938075777409963, -0.4704724409448818867 ) ) ;
#60681 = CARTESIAN_POINT ( 'NONE',  ( 1.358267716535433323, 0.1660481256975885056, 0.3530559997133364547 ) ) ;
#60682 = CARTESIAN_POINT ( 'NONE',  ( 0.2427821522309716595, -0.3162353388693409650, -0.4822834645669289433 ) ) ;
#60683 = CARTESIAN_POINT ( 'NONE',  ( 0.3805774278215230400, -0.3690944881889763329, 0.3153832671262228327 ) ) ;
#60684 = CARTESIAN_POINT ( 'NONE',  ( 2.362204724409448620, 0.03937007874015751446, 8.247593713802677664E-15 ) ) ;
#60685 = CARTESIAN_POINT ( 'NONE',  ( 0.3871391076115493490, -0.2845877964562159024, 0.3641732283464567677 ) ) ;
#60686 = DIRECTION ( 'NONE',  ( -1.000000000000000000, -0.000000000000000000, -0.000000000000000000 ) ) ;
#60687 = CARTESIAN_POINT ( 'NONE',  ( -0.3996062992125984925, -0.1070741851644056858, -1.382545931758530022 ) ) ;
#60688 = CARTESIAN_POINT ( 'NONE',  ( 0.6955380577427828781, -0.4281496062992124485, 0.4176697321401328655 ) ) ;
#60689 = CARTESIAN_POINT ( 'NONE',  ( -0.3917322834645670104, -7.196005306013484475E-17, -1.133858267716535195 ) ) ;
#60690 = CARTESIAN_POINT ( 'NONE',  ( 1.548556430446194954, 0.1283753931104746893, -0.1820866141732285504 ) ) ;
#60691 = CARTESIAN_POINT ( 'NONE',  ( -0.3622863298689263933, 0.1504864506494507925, -1.599317578742253179E-17 ) ) ;
#60692 = CARTESIAN_POINT ( 'NONE',  ( -0.02624671916010428221, -0.5023911411419708095, 0.1820866141732285504 ) ) ;
#60693 = CARTESIAN_POINT ( 'NONE',  ( 0.07874015748031558404, -0.1870078740157479769, 0.4822834645669291653 ) ) ;
#60694 = CARTESIAN_POINT ( 'NONE',  ( 1.482939632545932307, -0.3690944881889763329, 0.3153832671262228327 ) ) ;
#60695 = CARTESIAN_POINT ( 'NONE',  ( -1.482939632545930975, -0.3690944881889765550, -0.3153832671262227771 ) ) ;
#60696 = CARTESIAN_POINT ( 'NONE',  ( -1.272965879265091305, -0.4281496062992124485, 0.4176697321401328655 ) ) ;
#60697 = MECHANICAL_DESIGN_GEOMETRIC_PRESENTATION_REPRESENTATION (  '', ( #5590 ), #53956 ) ;
#60698 = CARTESIAN_POINT ( 'NONE',  ( 0.3937007874015754361, -0.1870078740157479769, 0.4822834645669291653 ) ) ;
#60699 = CARTESIAN_POINT ( 'NONE',  ( 1.240157480314961314, 0.1660481256975883668, -0.3530559997133364547 ) ) ;
#60700 = FACE_OUTER_BOUND ( 'NONE', #67788, .T. ) ;
#60701 = CARTESIAN_POINT ( 'NONE',  ( 0.6233595800524939223, -0.3162353388693405765, 0.4822834645669290543 ) ) ;
#60702 = CARTESIAN_POINT ( 'NONE',  ( 1.463254593175853824, -0.6692913385826771977, 0.1292274648535927661 ) ) ;
#60703 = CARTESIAN_POINT ( 'NONE',  ( 0.8202099737532814183, -0.6692913385826773087, -0.1292274648535924053 ) ) ;
#60704 = CARTESIAN_POINT ( 'NONE',  ( -1.699475065616797398, 0.1771653543307087630, 0.09757992244046791164 ) ) ;
#60705 = CARTESIAN_POINT ( 'NONE',  ( 0.6824146981627303710, -0.5023911411419708095, 0.1820866141732285504 ) ) ;
#60706 = CARTESIAN_POINT ( 'NONE',  ( 1.673228346456693494, 0.1660481256975885056, 0.3530559997133364547 ) ) ;
#60707 = CARTESIAN_POINT ( 'NONE',  ( -0.8858267716535425107, -0.4536011799217367080, 0.2665933059059888421 ) ) ;
#60708 = CARTESIAN_POINT ( 'NONE',  ( 0.3937007874015754361, -0.1870078740157480601, -0.3641732283464567677 ) ) ;
#60709 = CARTESIAN_POINT ( 'NONE',  ( 0.04593175853018440641, -0.6692913385826771977, 0.1292274648535927661 ) ) ;
#60710 = CARTESIAN_POINT ( 'NONE',  ( 0.8398950131233602345, 0.2306618581243847221, -0.2411417322834647770 ) ) ;
#60711 = CARTESIAN_POINT ( 'NONE',  ( -0.4461942257217840213, -0.6046776061558809534, -0.2411417322834644161 ) ) ;
#60712 = CARTESIAN_POINT ( 'NONE',  ( 0.07874015748031558404, -0.1870078740157480601, -0.3641732283464567677 ) ) ;
#60713 = CARTESIAN_POINT ( 'NONE',  ( 0.8989501312335963501, -0.6692913385826773087, -0.1292274648535924053 ) ) ;
#60714 =( BOUNDED_CURVE ( )  B_SPLINE_CURVE ( 2, ( #54441, #15758, #14918, #41000, #72158, #65441, #2286, #65850, #2700, #28360, #67095, #7774, #8183 ),
 .UNSPECIFIED., .F., .F. ) 
 B_SPLINE_CURVE_WITH_KNOTS ( ( 3, 2, 2, 2, 2, 2, 3 ),
 ( 0.3096947309984372509, 0.3106060606060606077, 0.3143939393939393923, 0.3181818181818181768, 0.3219696969696969613, 0.3257575757575757458, 0.3266689053651991581 ),
 .UNSPECIFIED. ) 
 CURVE ( )  GEOMETRIC_REPRESENTATION_ITEM ( )  RATIONAL_B_SPLINE_CURVE ( ( 0.9875488213027530104, 0.9918020599134685922, 1.000000000000000000, 0.9659258262890683122, 1.000000000000000000, 0.9659258262890683122, 1.000000000000000000, 0.9659258262890683122, 1.000000000000000000, 0.9659258262890683122, 1.000000000000000000, 0.9918020599134680371, 0.9875488213027523443 ) ) 
 REPRESENTATION_ITEM ( '' )  );
#60715 = CARTESIAN_POINT ( 'NONE',  ( -1.733288081962263139, 1.252173825773542637, 0.3800872639956032750 ) ) ;
#60716 = CARTESIAN_POINT ( 'NONE',  ( -0.8202099737532801971, -0.6692913385826771977, 0.1292274648535927661 ) ) ;
#60718 = CARTESIAN_POINT ( 'NONE',  ( -9.787531504996567848E-17, 0.3996062992125986035, -0.6299212598425196763 ) ) ;
#60717 = LINE ( 'NONE', #36690, #55396 ) ;
#60719 = CARTESIAN_POINT ( 'NONE',  ( 2.170146923806634653, 1.537401574803149984, -0.4744094488188970171 ) ) ;
#60720 = CARTESIAN_POINT ( 'NONE',  ( -0.6167979002624665030, -0.4281496062992127816, -0.4176697321401328100 ) ) ;
#60721 = CARTESIAN_POINT ( 'NONE',  ( -0.3674540682414692561, -0.6046776061558809534, -0.2411417322834644161 ) ) ;
#60722 = CARTESIAN_POINT ( 'NONE',  ( -0.4091458600556405756, 0.2362204724409446288, 0.1312335958005249326 ) ) ;
#60723 = CARTESIAN_POINT ( 'NONE',  ( 0.3420746716998659953, 0.1974969037888705536, -2.493438320209973469 ) ) ;
#60724 = EDGE_LOOP ( 'NONE', ( #13529, #39086, #50069, #2752, #1097, #16792, #57589, #40653, #74933, #15130, #15619, #64049, #8235, #39796, #25617, #71601, #67701, #76094, #22130, #12316 ) ) ;
#60725 = CARTESIAN_POINT ( 'NONE',  ( 0.7742782152230979209, -0.004921259842519870586, -0.3153832671262229437 ) ) ;
#60726 = CARTESIAN_POINT ( 'NONE',  ( -0.1958661417322834220, -0.3392501089628018884, -1.160104986876640210 ) ) ;
#60727 = CARTESIAN_POINT ( 'NONE',  ( 1.253280839895013710, -0.3162353388693405765, 0.4822834645669290543 ) ) ;
#60728 = CARTESIAN_POINT ( 'NONE',  ( 3.900966923095589678, 2.677165354330708791, -0.5314960629921260393 ) ) ;
#60729 = CARTESIAN_POINT ( 'NONE',  ( -1.266404199475064773, -0.2845877964562159024, 0.3641732283464567677 ) ) ;
#60730 = CARTESIAN_POINT ( 'NONE',  ( 1.561679790026247350, 0.05413385826771626580, -0.4176697321401330321 ) ) ;
#60731 = CARTESIAN_POINT ( 'NONE',  ( -1.489501312335957062, -0.3162353388693409650, -0.4822834645669289433 ) ) ;
#60732 = CARTESIAN_POINT ( 'NONE',  ( 0.3083989501312343062, -0.05778040916215560624, -0.4822834645669293319 ) ) ;
#60733 = CARTESIAN_POINT ( 'NONE',  ( -0.2867679344610364334, -0.2867679344610368219, -0.1390882957667173292 ) ) ;
#60734 = CARTESIAN_POINT ( 'NONE',  ( -0.1771653543307080136, 0.1660481256975883668, -0.3530559997133364547 ) ) ;
#60735 = CARTESIAN_POINT ( 'NONE',  ( -0.8202099737532801971, -0.5511811023622046335, 0.09757992244046803654 ) ) ;
#60737 = EDGE_CURVE ( 'NONE', #61368, #49776, #20861, .T. ) ;
#60736 = CARTESIAN_POINT ( 'NONE',  ( 0.9908136482939640111, 0.2952755905511810774, -0.1292274648535930714 ) ) ;
#60738 = CARTESIAN_POINT ( 'NONE',  ( 0.1049868766404206816, -0.6046776061558809534, -0.2411417322834644161 ) ) ;
#60739 = CARTESIAN_POINT ( 'NONE',  ( 0.4477876756950379122, 1.694898206223995007, 3.911462694204230317 ) ) ;
#60740 = CARTESIAN_POINT ( 'NONE',  ( -0.3392501089628019995, 0.1958661417322831999, -1.597788344653229720 ) ) ;
#60741 = CARTESIAN_POINT ( 'NONE',  ( 0.9514435695538062676, -0.3162353388693409650, -0.4822834645669289433 ) ) ;
#60742 = CARTESIAN_POINT ( 'NONE',  ( 0.04593175853018440641, 0.2952755905511810774, -0.1292274648535930714 ) ) ;
#60743 = CARTESIAN_POINT ( 'NONE',  ( -0.9186351706036736120, -0.6046776061558809534, -0.2411417322834644161 ) ) ;
#60744 = CARTESIAN_POINT ( 'NONE',  ( 1.122047244094488860, 0.1660481256975885056, 0.3530559997133364547 ) ) ;
#60745 = CARTESIAN_POINT ( 'NONE',  ( 0.9908136482939640111, -0.6692913385826771977, 0.1292274648535927661 ) ) ;
#60746 = CARTESIAN_POINT ( 'NONE',  ( -0.3392501089628019995, 0.1958661417322832277, -0.8982939632545933195 ) ) ;
#60747 = CARTESIAN_POINT ( 'NONE',  ( -0.4855643044619415427, -0.4281496062992124485, 0.4176697321401328655 ) ) ;
#60748 = CARTESIAN_POINT ( 'NONE',  ( 0.4461942257217856311, 0.2306618581243847221, -0.2411417322834647770 ) ) ;
#60749 = CARTESIAN_POINT ( 'NONE',  ( 0.06561679790026316017, -0.4281496062992124485, 0.4176697321401328655 ) ) ;
#60750 = CARTESIAN_POINT ( 'NONE',  ( 0.9251968503937015864, 0.07958543189024071263, -0.2665933059059888421 ) ) ;
#60751 = CARTESIAN_POINT ( 'NONE',  ( -1.213910761154854745, 0.2952755905511810774, -0.1292274648535930714 ) ) ;
#60752 = CARTESIAN_POINT ( 'NONE',  ( -0.1341320108093635721, 1.082050302230251448, -2.856397811438244005 ) ) ;
#60753 = CARTESIAN_POINT ( 'NONE',  ( 0.4986876640419954376, 0.2306618581243848609, 0.2411417322834645549 ) ) ;
#60754 = AXIS2_PLACEMENT_3D ( 'NONE', #11033, #53978, #79690 ) ;
#60755 = CARTESIAN_POINT ( 'NONE',  ( 0.4724409448818898682, 2.892866454678787531E-17, -0.3523622047244094335 ) ) ;
#60756 = CARTESIAN_POINT ( 'NONE',  ( 0.3392501089628018329, 0.1958661417322835607, -2.485564304461941987 ) ) ;
#60757 = ORIENTED_EDGE ( 'NONE', *, *, #5521, .T. ) ;
#60758 = ORIENTED_EDGE ( 'NONE', *, *, #36242, .T. ) ;
#60759 = CARTESIAN_POINT ( 'NONE',  ( 0.9448818897637802916, -0.1870078740157480879, -0.4822834645669291653 ) ) ;
#60760 = CARTESIAN_POINT ( 'NONE',  ( 0.5380577427821529035, -0.004921259842519870586, -0.3153832671262229437 ) ) ;
#60762 = DIRECTION ( 'NONE',  ( 8.805702923740139587E-17, -1.000000000000000000, 0.000000000000000000 ) ) ;
#60761 = CARTESIAN_POINT ( 'NONE',  ( -1.171093442848938793, -2.191421614605370878E-15, 0.4445507791589071167 ) ) ;
#60763 = CARTESIAN_POINT ( 'NONE',  ( 1.348312163386739426, 0.2929341459200028863, 0.7386866130305692613 ) ) ;
#60764 = DIRECTION ( 'NONE',  ( 0.000000000000000000, -1.000000000000000000, 0.000000000000000000 ) ) ;
#60765 = CARTESIAN_POINT ( 'NONE',  ( 0.2867679344610365999, 0.2867679344610365999, -1.167322834645669438 ) ) ;
#60766 = CARTESIAN_POINT ( 'NONE',  ( -0.3996062992125985480, -7.340648628747423112E-17, -2.320866141732283783 ) ) ;
#60767 = CARTESIAN_POINT ( 'NONE',  ( -0.8202099737532799750, 0.2952755905511810774, -0.1292274648535930714 ) ) ;
#60768 = CARTESIAN_POINT ( 'NONE',  ( -0.7152230971128602510, -0.05778040916215560624, -0.4822834645669293319 ) ) ;
#60769 = CARTESIAN_POINT ( 'NONE',  ( 0.5511811023622054106, -0.1870078740157480879, -0.4822834645669291653 ) ) ;
#60770 = ORIENTED_EDGE ( 'NONE', *, *, #37751, .T. ) ;
#60771 = CARTESIAN_POINT ( 'NONE',  ( 1.312335958005249825, 0.2306618581243847221, -0.2411417322834647770 ) ) ;
#60772 = CARTESIAN_POINT ( 'NONE',  ( 1.692913385826772421, 0.1771653543307087630, 0.000000000000000000 ) ) ;
#60773 = CONTEXT_DEPENDENT_SHAPE_REPRESENTATION ( #60000, #35277 ) ;
#60774 = CARTESIAN_POINT ( 'NONE',  ( -1.586052503253848389, 0.7480314960629931287, -0.1653254495020559933 ) ) ;
#60775 = CARTESIAN_POINT ( 'NONE',  ( -0.5314960629921294810, 2.755905511811024056, 0.9881811337016621621 ) ) ;
#60776 = CARTESIAN_POINT ( 'NONE',  ( -1.469816272965878357, 0.1283753931104748280, 0.1820866141732283561 ) ) ;
#60777 = CARTESIAN_POINT ( 'NONE',  ( -0.2867679344610365999, 0.2867679344610364889, 0.1456692913385827237 ) ) ;
#60778 = CARTESIAN_POINT ( 'NONE',  ( 0.2559055118110243332, 0.1660481256975885056, 0.3530559997133364547 ) ) ;
#60780 = FACE_OUTER_BOUND ( 'NONE', #55555, .T. ) ;
#60779 = DIRECTION ( 'NONE',  ( -0.000000000000000000, -1.000000000000000000, 0.000000000000000000 ) ) ;
#60781 = CARTESIAN_POINT ( 'NONE',  ( -1.095800524934382292, -0.08942795157527998196, 0.3641732283464567121 ) ) ;
#60782 = CARTESIAN_POINT ( 'NONE',  ( 0.6692913385826778638, -0.6692913385826771977, 8.415575281601705876E-17 ) ) ;
#60783 = CARTESIAN_POINT ( 'NONE',  ( 1.410761154855643795, -0.2845877964562159024, 0.3641732283464567677 ) ) ;
#60784 = CARTESIAN_POINT ( 'NONE',  ( -0.3917322834645669549, -7.196005306013483243E-17, -1.064285146160418360 ) ) ;
#60785 = CARTESIAN_POINT ( 'NONE',  ( -1.423884514435694859, -0.2845877964562159024, 0.3641732283464567677 ) ) ;
#60786 = CARTESIAN_POINT ( 'NONE',  ( 1.515748031496063408, 0.1660481256975885056, 0.3530559997133364547 ) ) ;
#60787 = CARTESIAN_POINT ( 'NONE',  ( 0.3129921259842520787, 1.496062992125984259, 0.000000000000000000 ) ) ;
#60788 = CARTESIAN_POINT ( 'NONE',  ( -0.2493438320209966919, 0.05413385826771626580, -0.4176697321401330321 ) ) ;
#60789 = CARTESIAN_POINT ( 'NONE',  ( -1.417322834645668772, -0.1870078740157480601, -0.3641732283464567677 ) ) ;
#60790 = CARTESIAN_POINT ( 'NONE',  ( -0.3674540682414692561, -0.5023911411419708095, -0.1820866141732282451 ) ) ;
#60791 = CARTESIAN_POINT ( 'NONE',  ( -0.4068241469816267775, 0.05413385826771626580, -0.4176697321401330321 ) ) ;
#60792 = CARTESIAN_POINT ( 'NONE',  ( -1.568241469816272105, -0.2845877964562161244, -0.3641732283464567121 ) ) ;
#60793 = CARTESIAN_POINT ( 'NONE',  ( 0.2867679344610366554, 0.2867679344610366554, -0.2920140664380071471 ) ) ;
#60794 = CARTESIAN_POINT ( 'NONE',  ( 0.2690288713910767848, -0.6692913385826773087, -0.1292274648535924053 ) ) ;
#60795 = CARTESIAN_POINT ( 'NONE',  ( 0.4091458600556403535, 0.2362204724409449896, -1.782808398950131101 ) ) ;
#60796 = CARTESIAN_POINT ( 'NONE',  ( -1.102362204724408601, -0.1870078740157479769, 0.4822834645669291653 ) ) ;
#60797 = CARTESIAN_POINT ( 'NONE',  ( -0.5971128608923877978, 0.1771653543307087630, 0.09757992244046791164 ) ) ;
#60798 = CARTESIAN_POINT ( 'NONE',  ( -1.561679790026246017, -0.4281496062992127816, -0.4176697321401328100 ) ) ;
#60799 = CARTESIAN_POINT ( 'NONE',  ( -0.08530183727034056085, -0.3162353388693405765, 0.4822834645669290543 ) ) ;
#60800 = CARTESIAN_POINT ( 'NONE',  ( 0.4461942257217856311, 0.1283753931104746893, -0.1820866141732285504 ) ) ;
#60801 = CARTESIAN_POINT ( 'NONE',  ( -0.8923884514435688198, 0.1283753931104746893, -0.1820866141732285504 ) ) ;
#60802 = CARTESIAN_POINT ( 'NONE',  ( -1.154855643044618851, -0.6046776061558809534, -0.2411417322834644161 ) ) ;
#60803 = CARTESIAN_POINT ( 'NONE',  ( -1.391076115485563758, 0.2306618581243848609, 0.2411417322834645549 ) ) ;
#60804 = CARTESIAN_POINT ( 'NONE',  ( 1.489501312335958172, -0.3162353388693405765, 0.4822834645669290543 ) ) ;
#60805 = CARTESIAN_POINT ( 'NONE',  ( 0.000000000000000000, 0.000000000000000000, 0.000000000000000000 ) ) ;
#60806 = CARTESIAN_POINT ( 'NONE',  ( 0.8005249343832028242, -0.3690944881889765550, -0.3153832671262227771 ) ) ;
#60807 = PRODUCT_DEFINITION_SHAPE ( 'NONE', 'NONE',  #32108 ) ;
#60808 = CARTESIAN_POINT ( 'NONE',  ( 0.9055118110236227702, 0.2952755905511811885, 0.000000000000000000 ) ) ;
#60809 = DIRECTION ( 'NONE',  ( 0.000000000000000000, -1.000000000000000000, 0.000000000000000000 ) ) ;
#60810 = CARTESIAN_POINT ( 'NONE',  ( 1.555118110236221041, -0.4536011799217367080, 0.2665933059059888421 ) ) ;
#60811 = AXIS2_PLACEMENT_3D ( 'NONE', #9790, #17367, #15708 ) ;
#60812 = VERTEX_POINT ( 'NONE', #52255 ) ;
#60813 = CARTESIAN_POINT ( 'NONE',  ( -0.9055118110236215490, -0.6692913385826771977, 8.415575281601705876E-17 ) ) ;
#60814 = CARTESIAN_POINT ( 'NONE',  ( -0.8005249343832011588, 0.05413385826771626580, -0.4176697321401330321 ) ) ;
#60815 = CARTESIAN_POINT ( 'NONE',  ( 0.4330708661417329575, -0.6692913385826771977, 8.415575281601705876E-17 ) ) ;
#60816 = CARTESIAN_POINT ( 'NONE',  ( -1.286089238845143479, -0.5023911411419708095, 0.1820866141732285504 ) ) ;
#60817 = CARTESIAN_POINT ( 'NONE',  ( 0.3460692066303959202, -0.1998031496062991630, -2.071522309711286258 ) ) ;
#60818 = CARTESIAN_POINT ( 'NONE',  ( -1.286089238845143479, -0.6046776061558807314, 0.2411417322834647770 ) ) ;
#60819 = CARTESIAN_POINT ( 'NONE',  ( 0.2887139107611556010, 0.2306618581243847221, -0.2411417322834647770 ) ) ;
#60820 = CARTESIAN_POINT ( 'NONE',  ( 0.05249343832021075018, -0.6046776061558807314, 0.2411417322834647770 ) ) ;
#60821 = CARTESIAN_POINT ( 'NONE',  ( 0.8398950131233602345, 0.2306618581243847221, -0.2411417322834647770 ) ) ;
#60822 = CARTESIAN_POINT ( 'NONE',  ( 1.614173228346457156, 1.496062992125984037, -0.5309055118110239668 ) ) ;
#60823 = CARTESIAN_POINT ( 'NONE',  ( -0.1070741851644051862, -0.3996062992125987146, -1.646981627296587591 ) ) ;
#60824 = CARTESIAN_POINT ( 'NONE',  ( -0.3420746716998661618, 0.1974969037888702206, -0.9711286089238846397 ) ) ;
#60825 = CARTESIAN_POINT ( 'NONE',  ( 0.1998031496062994405, -0.3460692066303958092, -2.611548556430446144 ) ) ;
#60826 = CARTESIAN_POINT ( 'NONE',  ( -1.559171609364246924, 0.3937007874015747699, 0.2199441279213821265 ) ) ;
#60827 = CARTESIAN_POINT ( 'NONE',  ( -0.3917322834645671215, 0.1049643490035301469, -0.1824146981627296216 ) ) ;
#60828 = CARTESIAN_POINT ( 'NONE',  ( -0.2427821522309703550, -0.08942795157528024563, -0.3641732283464568787 ) ) ;
#60829 = CARTESIAN_POINT ( 'NONE',  ( -0.2296587926509179312, -0.3162353388693409650, -0.4822834645669289433 ) ) ;
#60830 = CARTESIAN_POINT ( 'NONE',  ( 0.6955380577427828781, 0.05413385826771626580, -0.4176697321401330321 ) ) ;
#60831 = CARTESIAN_POINT ( 'NONE',  ( -0.2891555358219909388, -0.2891555358219912164, -2.025590551181102761 ) ) ;
#60832 = CARTESIAN_POINT ( 'NONE',  ( 0.1574803149606306130, -0.1870078740157480601, -0.3641732283464567677 ) ) ;
#60833 = CARTESIAN_POINT ( 'NONE',  ( -1.325459317585300889, 0.05413385826771666132, 0.4176697321401328100 ) ) ;
#60834 = CARTESIAN_POINT ( 'NONE',  ( 1.148293963254593653, 0.2952755905511810774, -0.1292274648535930714 ) ) ;
#60835 = CARTESIAN_POINT ( 'NONE',  ( 0.3458507752293908943, -0.3458507752293908943, -2.618110236220472675 ) ) ;
#60836 = CARTESIAN_POINT ( 'NONE',  ( -9.787531504996567848E-17, 0.3996062992125986035, -1.889763779527559251 ) ) ;
#60837 = CARTESIAN_POINT ( 'NONE',  ( 1.204164820379012069, 1.535433070866141447, -0.4915354330708657793 ) ) ;
#60838 = ORIENTED_EDGE ( 'NONE', *, *, #39775, .T. ) ;
#60839 = ORIENTED_EDGE ( 'NONE', *, *, #65705, .T. ) ;
#60840 = CARTESIAN_POINT ( 'NONE',  ( 1.036745406824147508, -0.4281496062992127816, -0.4176697321401328100 ) ) ;
#60841 = CARTESIAN_POINT ( 'NONE',  ( -1.627296587926508442, -0.6046776061558809534, -0.2411417322834644161 ) ) ;
#60843 = CARTESIAN_POINT ( 'NONE',  ( -1.233595800524933894, -0.6046776061558809534, -0.2411417322834644161 ) ) ;
#60842 = CARTESIAN_POINT ( 'NONE',  ( -1.207349081364828436, -0.5023911411419708095, 0.1820866141732285504 ) ) ;
#60844 = CARTESIAN_POINT ( 'NONE',  ( -0.1958661417322834497, -0.3392501089628018884, -2.665335014926823121 ) ) ;
#60845 = DIRECTION ( 'NONE',  ( 0.000000000000000000, 0.000000000000000000, 1.000000000000000000 ) ) ;
#60846 = CARTESIAN_POINT ( 'NONE',  ( 1.430446194225722500, -0.4281496062992127816, -0.4176697321401328100 ) ) ;
#60847 = CARTESIAN_POINT ( 'NONE',  ( -1.627296587926508442, -0.6046776061558809534, -0.2411417322834644161 ) ) ;
#60848 = CARTESIAN_POINT ( 'NONE',  ( -0.1771653543307080136, -0.5400638737290844871, 0.3530559997133364547 ) ) ;
#60849 = CARTESIAN_POINT ( 'NONE',  ( -0.4986876640419942164, -0.6046776061558807314, 0.2411417322834647770 ) ) ;
#60850 = CARTESIAN_POINT ( 'NONE',  ( -1.496062992125983815, -0.1870078740157479769, 0.4822834645669291653 ) ) ;
#60851 = CARTESIAN_POINT ( 'NONE',  ( -0.1958661417322834220, -0.3392501089628018884, -0.3077427821522311091 ) ) ;
#60852 = CARTESIAN_POINT ( 'NONE',  ( 0.3674540682414705883, 0.2306618581243847221, -0.2411417322834647770 ) ) ;
#60853 = CARTESIAN_POINT ( 'NONE',  ( 0.2867679344610365999, -0.2867679344610365444, -2.295275590551181022 ) ) ;
#60854 = CARTESIAN_POINT ( 'NONE',  ( -1.437007874015747477, 0.07958543189024071263, -0.2665933059059888421 ) ) ;
#60855 = VERTEX_POINT ( 'NONE', #20290 ) ;
#60856 = CARTESIAN_POINT ( 'NONE',  ( 0.2891555358219910499, 0.2891555358219910499, -2.342519685039370358 ) ) ;
#60857 = EDGE_LOOP ( 'NONE', ( #41696, #34447, #58529, #46577 ) ) ;
#60858 = CARTESIAN_POINT ( 'NONE',  ( -1.563876174483072035, 1.386417634015433942, 0.4497423439146382429 ) ) ;
#60859 = CARTESIAN_POINT ( 'NONE',  ( -1.535433070866141225, 0.2952755905511811885, 0.000000000000000000 ) ) ;
#60860 = CARTESIAN_POINT ( 'NONE',  ( -0.1998031496062994683, 0.3460692066303958092, -1.115485564304461885 ) ) ;
#60861 = CARTESIAN_POINT ( 'NONE',  ( 1.607611548556431069, -0.5511811023622048555, -0.09757992244046775898 ) ) ;
#60862 = CARTESIAN_POINT ( 'NONE',  ( -1.555118110236219930, 0.1660481256975885056, 0.3530559997133364547 ) ) ;
#60863 = DIRECTION ( 'NONE',  ( -0.000000000000000000, -1.000000000000000000, 0.000000000000000000 ) ) ;
#60864 = DIRECTION ( 'NONE',  ( 0.000000000000000000, 0.000000000000000000, 1.000000000000000000 ) ) ;
#60865 = CARTESIAN_POINT ( 'NONE',  ( 0.3392501089628018884, -0.1958661417322834220, -0.03215223097112869521 ) ) ;
#60866 = AXIS2_PLACEMENT_3D ( 'NONE', #54971, #67623, #47827 ) ;
#60867 = CARTESIAN_POINT ( 'NONE',  ( -0.4790026246719152336, -0.08942795157528024563, -0.3641732283464568787 ) ) ;
#60868 = CARTESIAN_POINT ( 'NONE',  ( -0.6036745406824141069, 0.1283753931104748280, 0.1820866141732283561 ) ) ;
#60869 = CARTESIAN_POINT ( 'NONE',  ( -1.286089238845143479, 0.2306618581243847221, -0.2411417322834647770 ) ) ;
#60870 = CARTESIAN_POINT ( 'NONE',  ( 0.6824146981627303710, 0.2306618581243847221, -0.2411417322834647770 ) ) ;
#60871 = CARTESIAN_POINT ( 'NONE',  ( -1.023622047244093558, -0.1870078740157479769, 0.4822834645669291653 ) ) ;
#60872 = CARTESIAN_POINT ( 'NONE',  ( 0.5314960629921394730, 2.712230453466948799, -3.892840969167623566 ) ) ;
#60873 = EDGE_LOOP ( 'NONE', ( #6918, #57946, #56556, #2403, #14936, #82202, #78175, #23384, #63840, #7849 ) ) ;
#60874 = EDGE_CURVE ( 'NONE', #81247, #21404, #45939, .T. ) ;
#60875 = CARTESIAN_POINT ( 'NONE',  ( -1.502624671916009680, -0.3162353388693405765, 0.4822834645669290543 ) ) ;
#60876 = CARTESIAN_POINT ( 'NONE',  ( 0.000000000000000000, 0.000000000000000000, 0.000000000000000000 ) ) ;
#60877 =( NAMED_UNIT ( * ) PLANE_ANGLE_UNIT ( ) SI_UNIT ( $, .RADIAN. ) );
#60878 = CARTESIAN_POINT ( 'NONE',  ( 0.3458507752293908943, 0.3458507752293908943, -1.870078740157480546 ) ) ;
#60879 = CARTESIAN_POINT ( 'NONE',  ( -1.604771003085130321, 1.044625174762916719, -0.1466069496707741726 ) ) ;
#60880 = EDGE_CURVE ( 'NONE', #20906, #75749, #50936, .T. ) ;
#60881 = CARTESIAN_POINT ( 'NONE',  ( 0.3917322834645670104, -0.1049643490035303411, -0.5761154855643042527 ) ) ;
#60882 = CARTESIAN_POINT ( 'NONE',  ( 0.3917322834645670104, -0.1049643490035303273, -2.715879265091862838 ) ) ;
#60883 = CARTESIAN_POINT ( 'NONE',  ( -0.6299212598425188991, -0.1870078740157480879, -0.4822834645669291653 ) ) ;
#60884 = CARTESIAN_POINT ( 'NONE',  ( 1.286089238845145033, -0.6046776061558809534, -0.2411417322834644161 ) ) ;
#60885 = CARTESIAN_POINT ( 'NONE',  ( 0.2925321140481932369, 0.2925321140481932369, -0.6870078740157479213 ) ) ;
#60887 = DIRECTION ( 'NONE',  ( 0.000000000000000000, 0.000000000000000000, -1.000000000000000000 ) ) ;
#60886 = CARTESIAN_POINT ( 'NONE',  ( -1.614173228346456268, -0.6692913385826771977, 8.415575281601705876E-17 ) ) ;
#60888 = CARTESIAN_POINT ( 'NONE',  ( -1.332020997375327642, -0.3162353388693409650, -0.4822834645669289433 ) ) ;
#60889 = CARTESIAN_POINT ( 'NONE',  ( -0.7020997375328076329, -0.3162353388693409650, -0.4822834645669289433 ) ) ;
#60890 = CARTESIAN_POINT ( 'NONE',  ( -0.1049643490035306742, 0.3917322834645668994, -0.08659485744650738392 ) ) ;
#60891 = CARTESIAN_POINT ( 'NONE',  ( 0.2952755905511816326, -0.4536011799217367080, 0.2665933059059888421 ) ) ;
#60892 = CARTESIAN_POINT ( 'NONE',  ( -0.2867679344610366554, 0.2867679344610365444, -0.2618110236220473341 ) ) ;
#60893 = CARTESIAN_POINT ( 'NONE',  ( 0.1181102362204730916, 0.1771653543307087630, 0.000000000000000000 ) ) ;
#60894 = CARTESIAN_POINT ( 'NONE',  ( 1.148293963254593653, 0.1771653543307087075, -0.09757992244046823083 ) ) ;
#60895 = CARTESIAN_POINT ( 'NONE',  ( 0.9251968503937015864, -0.5400638737290844871, 0.3530559997133364547 ) ) ;
#60896 = CARTESIAN_POINT ( 'NONE',  ( -0.1706036745406816491, -0.004921259842519870586, -0.3153832671262229437 ) ) ;
#60897 = CARTESIAN_POINT ( 'NONE',  ( 0.3917322834645669549, 0.1049643490035304660, -2.321522309711285814 ) ) ;
#60898 = CARTESIAN_POINT ( 'NONE',  ( 1.469816272965879911, 0.2306618581243847221, -0.2411417322834647770 ) ) ;
#60899 = EDGE_CURVE ( 'NONE', #31040, #42893, #43989, .T. ) ;
#60900 = CARTESIAN_POINT ( 'NONE',  ( -1.272965879265091305, -0.004921259842519870586, -0.3153832671262229437 ) ) ;
#60901 = CARTESIAN_POINT ( 'NONE',  ( 5.785732909357575061E-17, -0.4724409448818898682, -0.3129921259842520231 ) ) ;
#60902 = ADVANCED_FACE ( 'NONE', ( #79635 ), #11192, .T. ) ;
#60903 = CARTESIAN_POINT ( 'NONE',  ( -0.1706036745406816491, 0.05413385826771626580, -0.4176697321401330321 ) ) ;
#60904 = CARTESIAN_POINT ( 'NONE',  ( -0.3503937007874015630, -0.3733313776025731778, -0.01968503937007957602 ) ) ;
#60905 = CARTESIAN_POINT ( 'NONE',  ( 0.6627296587926515548, 0.1771653543307087630, 0.09757992244046791164 ) ) ;
#60906 = CARTESIAN_POINT ( 'NONE',  ( -0.09842519685039295696, 0.07958543189024071263, -0.2665933059059888421 ) ) ;
#60907 = CARTESIAN_POINT ( 'NONE',  ( -0.6102362204724400829, -0.5400638737290845981, -0.3530559997133363437 ) ) ;
#60908 = CARTESIAN_POINT ( 'NONE',  ( 0.6986524979670498681, 8.471767977567108961E-16, -0.4445507791589058955 ) ) ;
#60909 = DIRECTION ( 'NONE',  ( 0.000000000000000000, 1.000000000000000000, 0.000000000000000000 ) ) ;
#60910 = CARTESIAN_POINT ( 'NONE',  ( 0.09186351706036827158, 0.05413385826771666132, 0.4176697321401328100 ) ) ;
#60911 = ORIENTED_EDGE ( 'NONE', *, *, #11099, .T. ) ;
#60912 = CARTESIAN_POINT ( 'NONE',  ( -0.3460692066303960313, 0.1998031496062989965, -1.362860892388451539 ) ) ;
#60913 = CARTESIAN_POINT ( 'NONE',  ( 0.2262115530851599166, 8.471767977567108961E-16, -0.4445507791589058955 ) ) ;
#60914 = CARTESIAN_POINT ( 'NONE',  ( -0.4330708661417315697, 0.1771653543307087630, 0.000000000000000000 ) ) ;
#60915 = CARTESIAN_POINT ( 'NONE',  ( 0.05249343832021075018, 0.2306618581243847221, -0.2411417322834647770 ) ) ;
#60916 = CARTESIAN_POINT ( 'NONE',  ( -1.410761154855641575, -0.3162353388693409650, -0.4822834645669289433 ) ) ;
#60917 = CARTESIAN_POINT ( 'NONE',  ( -1.627296587926508442, 0.1283753931104748280, 0.1820866141732283561 ) ) ;
#60918 = CARTESIAN_POINT ( 'NONE',  ( 1.279527559055118724, -0.5400638737290845981, -0.3530559997133363437 ) ) ;
#60919 = CARTESIAN_POINT ( 'NONE',  ( -1.325459317585300889, 0.05413385826771666132, 0.4176697321401328100 ) ) ;
#60920 = CARTESIAN_POINT ( 'NONE',  ( -0.5905511811023615998, 0.1771653543307087630, 0.000000000000000000 ) ) ;
#60921 = CARTESIAN_POINT ( 'NONE',  ( 0.1998031496062992463, 0.3460692066303959202, -0.2211286089238845565 ) ) ;
#60922 = CARTESIAN_POINT ( 'NONE',  ( -0.1070741851644051862, -0.3996062992125987146, -0.5446194225721783244 ) ) ;
#60923 = AXIS2_PLACEMENT_3D ( 'NONE', #35523, #15769, #29614 ) ;
#60924 = CARTESIAN_POINT ( 'NONE',  ( -0.1049643490035307158, 0.3917322834645670104, -2.837945824968191477 ) ) ;
#60925 = CARTESIAN_POINT ( 'NONE',  ( 1.528871391076116026, 0.1771653543307087630, 0.09757992244046791164 ) ) ;
#60926 = CARTESIAN_POINT ( 'NONE',  ( 1.115485564304462551, -0.004921259842519576551, 0.3153832671262227771 ) ) ;
#60927 = CARTESIAN_POINT ( 'NONE',  ( -1.692913385826770645, 0.2952755905511811885, 0.000000000000000000 ) ) ;
#60928 = CARTESIAN_POINT ( 'NONE',  ( 0.7349081364829402885, -0.6046776061558809534, -0.2411417322834644161 ) ) ;
#60929 = CARTESIAN_POINT ( 'NONE',  ( -0.3949938075777411073, 0.1058382717557497660, -0.7395013123359579499 ) ) ;
#60930 = CARTESIAN_POINT ( 'NONE',  ( 1.325459317585302665, -0.3690944881889763329, 0.3153832671262228327 ) ) ;
#60931 = CARTESIAN_POINT ( 'NONE',  ( 0.2165354330708668673, -0.5400638737290844871, 0.3530559997133364547 ) ) ;
#60932 = CARTESIAN_POINT ( 'NONE',  ( -0.9251968503937002541, -0.5400638737290845981, -0.3530559997133363437 ) ) ;
#60933 = CARTESIAN_POINT ( 'NONE',  ( 0.1771653543307086798, 0.000000000000000000, 0.000000000000000000 ) ) ;
#60934 = CARTESIAN_POINT ( 'NONE',  ( 0.3458507752293908943, 0.3458507752293908943, -0.6102362204724409711 ) ) ;
#60935 = CARTESIAN_POINT ( 'NONE',  ( 0.1070741851644054915, -0.3996062992125985480, -2.132545931758530244 ) ) ;
#60936 = CARTESIAN_POINT ( 'NONE',  ( 0.4199475065616803948, -0.5023911411419708095, -0.1820866141732282451 ) ) ;
#60937 = VERTEX_POINT ( 'NONE', #4083 ) ;
#60938 = CARTESIAN_POINT ( 'NONE',  ( 0.3392501089628018884, -0.1958661417322833942, -0.2592056674878758793 ) ) ;
#60939 = ORIENTED_EDGE ( 'NONE', *, *, #68146, .T. ) ;
#60940 = CARTESIAN_POINT ( 'NONE',  ( -0.5839895013123351797, 0.2952755905511810774, -0.1292274648535930714 ) ) ;
#60941 = CARTESIAN_POINT ( 'NONE',  ( -0.3346456692913377662, 0.1660481256975883668, -0.3530559997133364547 ) ) ;
#60942 = CARTESIAN_POINT ( 'NONE',  ( -0.1837270341207340729, 0.1283753931104746893, -0.1820866141732285504 ) ) ;
#60943 = CARTESIAN_POINT ( 'NONE',  ( 0.6102362204724416372, 0.1660481256975883668, -0.3530559997133364547 ) ) ;
#60944 = CARTESIAN_POINT ( 'NONE',  ( -1.003937007874014853, 0.1660481256975885056, 0.3530559997133364547 ) ) ;
#60945 = CARTESIAN_POINT ( 'NONE',  ( -0.1968503937007867743, -0.6692913385826771977, 8.415575281601705876E-17 ) ) ;
#60946 = CARTESIAN_POINT ( 'NONE',  ( 1.069553805774278610, -0.6692913385826771977, 0.1292274648535927661 ) ) ;
#60947 = CARTESIAN_POINT ( 'NONE',  ( 1.036745406824147508, -0.4281496062992127816, -0.4176697321401328100 ) ) ;
#60948 = EDGE_CURVE ( 'NONE', #34118, #80835, #72151, .T. ) ;
#60949 = CARTESIAN_POINT ( 'NONE',  ( 0.8595800524934390507, -0.3162353388693405765, 0.4822834645669290543 ) ) ;
#60950 = CARTESIAN_POINT ( 'NONE',  ( -0.1958661417322834220, -0.3392501089628018884, -0.5301837270341206443 ) ) ;
#60951 = CARTESIAN_POINT ( 'NONE',  ( 0.1902887139107617975, -0.5511811023622048555, -0.09757992244046775898 ) ) ;
#60952 = ORIENTED_EDGE ( 'NONE', *, *, #50736, .T. ) ;
#60953 = CARTESIAN_POINT ( 'NONE',  ( -9.674558042662121740E-17, 0.3949938075777409963, -1.102362204724409711 ) ) ;
#60954 = ORIENTED_EDGE ( 'NONE', *, *, #80559, .F. ) ;
#60955 = CARTESIAN_POINT ( 'NONE',  ( -1.069553805774277722, 0.1771653543307087630, 0.09757992244046791164 ) ) ;
#60956 = CARTESIAN_POINT ( 'NONE',  ( -0.5971128608923877978, -0.6692913385826773087, -0.1292274648535924053 ) ) ;
#60957 = CARTESIAN_POINT ( 'NONE',  ( 0.3996062992125986035, 0.1070741851644054776, 0.03280839895013121926 ) ) ;
#60958 = CARTESIAN_POINT ( 'NONE',  ( -0.2165354330708654795, -0.5400638737290845981, -0.3530559997133363437 ) ) ;
#60959 = CARTESIAN_POINT ( 'NONE',  ( -0.6167979002624665030, 0.05413385826771666132, 0.4176697321401328100 ) ) ;
#60960 = CARTESIAN_POINT ( 'NONE',  ( -1.148293963254592542, 0.2952755905511811885, 0.1292274648535926551 ) ) ;
#60961 = CARTESIAN_POINT ( 'NONE',  ( -1.305774278215222184, -0.6692913385826773087, -0.1292274648535924053 ) ) ;
#60962 = CARTESIAN_POINT ( 'NONE',  ( 0.8661417322834653598, -0.1870078740157479769, 0.3641732283464567677 ) ) ;
#60963 = CARTESIAN_POINT ( 'NONE',  ( -0.3458507752293906723, -0.3458507752293910609, -1.003937007874015741 ) ) ;
#60964 = CARTESIAN_POINT ( 'NONE',  ( 0.2524666497344155158, 0.1533018367440332486, 5.791491733107224427 ) ) ;
#60965 = CARTESIAN_POINT ( 'NONE',  ( 0.3674540682414705883, 0.1283753931104746893, -0.1820866141732285504 ) ) ;
#60966 = CARTESIAN_POINT ( 'NONE',  ( 0.02624671916010564918, -0.6046776061558809534, -0.2411417322834644161 ) ) ;
#60967 = CARTESIAN_POINT ( 'NONE',  ( 0.3346456692913393205, -0.5400638737290845981, -0.3530559997133363437 ) ) ;
#60968 = ORIENTED_EDGE ( 'NONE', *, *, #63295, .F. ) ;
#60969 = CARTESIAN_POINT ( 'NONE',  ( -0.3460692066303958092, -0.1998031496062994683, -1.627296587926509330 ) ) ;
#60970 = CARTESIAN_POINT ( 'NONE',  ( 0.1208384647389237204, -0.3726288332213487653, -2.755905511811024056 ) ) ;
#60971 = EDGE_LOOP ( 'NONE', ( #53800, #48747, #40217, #19240 ) ) ;
#60972 = CARTESIAN_POINT ( 'NONE',  ( 0.1998031496062994128, -0.3460692066303957537, -0.9560367454068241511 ) ) ;
#60973 = CARTESIAN_POINT ( 'NONE',  ( -9.787531504996566615E-17, 0.3996062992125985480, -0.3917322834645669549 ) ) ;
#60974 = CARTESIAN_POINT ( 'NONE',  ( -0.7611548556430438595, 0.1283753931104748280, 0.1820866141732283561 ) ) ;
#60975 = CARTESIAN_POINT ( 'NONE',  ( -1.128608923884513837, -0.6046776061558807314, 0.2411417322834647770 ) ) ;
#60976 = CARTESIAN_POINT ( 'NONE',  ( -0.4724409448818895907, -0.1265901696524993070, 0.1115485564304461719 ) ) ;
#60977 = EDGE_CURVE ( 'NONE', #3487, #38656, #11759, .T. ) ;
#60978 = CARTESIAN_POINT ( 'NONE',  ( -0.1049643490035302024, -0.3917322834645671215, -2.361548556430446144 ) ) ;
#60979 = CARTESIAN_POINT ( 'NONE',  ( -1.574803149606298192, -0.1870078740157480601, -0.3641732283464567677 ) ) ;
#60980 = CARTESIAN_POINT ( 'NONE',  ( 0.8202099737532813073, 0.2952755905511811885, 0.1292274648535926551 ) ) ;
#60981 = CARTESIAN_POINT ( 'NONE',  ( 0.4986876640419954376, -0.6046776061558809534, -0.2411417322834644161 ) ) ;
#60982 = CARTESIAN_POINT ( 'NONE',  ( -0.5839895013123351797, -0.5511811023622046335, 0.09757992244046803654 ) ) ;
#60983 = CARTESIAN_POINT ( 'NONE',  ( 0.09842519685039434474, -0.5400638737290845981, -0.3530559997133363437 ) ) ;
#60984 = CARTESIAN_POINT ( 'NONE',  ( -0.4724409448818899238, 0.1265901696524986686, -1.999343832020997525 ) ) ;
#60985 = CARTESIAN_POINT ( 'NONE',  ( -0.2230971128608915943, -0.004921259842519576551, 0.3153832671262227771 ) ) ;
#60986 = CARTESIAN_POINT ( 'NONE',  ( -0.4461942257217840213, 0.2306618581243848609, 0.2411417322834645549 ) ) ;
#60987 = VECTOR ( 'NONE', #64786, 39.37007874015748143 ) ;
#60988 = CARTESIAN_POINT ( 'NONE',  ( -0.3420746716998660508, -0.1974969037888706924, -1.704068241469815836 ) ) ;
#60989 = CARTESIAN_POINT ( 'NONE',  ( 1.522309711286089939, -0.5023911411419708095, -0.1820866141732282451 ) ) ;
#60990 = CARTESIAN_POINT ( 'NONE',  ( -0.09186351706036689768, -0.004921259842519870586, -0.3153832671262229437 ) ) ;
#60991 = CARTESIAN_POINT ( 'NONE',  ( 1.574803149606299746, -0.1870078740157480601, -0.3641732283464567677 ) ) ;
#60992 = CARTESIAN_POINT ( 'NONE',  ( -0.9842519685039365918, -0.6692913385826771977, 8.415575281601705876E-17 ) ) ;
#60993 = CARTESIAN_POINT ( 'NONE',  ( -0.8923884514435688198, -0.5023911411419708095, 0.1820866141732285504 ) ) ;
#60994 = PLANE ( 'NONE',  #61429 ) ;
#60995 = CARTESIAN_POINT ( 'NONE',  ( -1.200787401574802349, 0.1660481256975883668, -0.3530559997133364547 ) ) ;
#60996 = CARTESIAN_POINT ( 'NONE',  ( -0.3543307086614165824, 0.2952755905511811885, 0.000000000000000000 ) ) ;
#60997 = EDGE_CURVE ( 'NONE', #19450, #82899, #83190, .T. ) ;
#60998 = CARTESIAN_POINT ( 'NONE',  ( 0.4396325459317593221, 0.2952755905511810774, -0.1292274648535930714 ) ) ;
#60999 = CARTESIAN_POINT ( 'NONE',  ( -0.3917322834645670659, 0.1049643490035301607, -2.632526615976691353 ) ) ;
#61000 = CARTESIAN_POINT ( 'NONE',  ( -1.923693779251843150, 1.143166703770554626, -0.2643333500026249783 ) ) ;
#61001 = CARTESIAN_POINT ( 'NONE',  ( 0.3477690288713918276, -0.5511811023622048555, -0.09757992244046775898 ) ) ;
#61002 = CARTESIAN_POINT ( 'NONE',  ( 1.003937007874016185, 0.1660481256975883668, -0.3530559997133364547 ) ) ;
#61003 = CARTESIAN_POINT ( 'NONE',  ( -1.364829396325458521, 0.1283753931104746893, -0.1820866141732285504 ) ) ;
#61004 = CARTESIAN_POINT ( 'NONE',  ( 1.082677165354331228, 0.1660481256975883668, -0.3530559997133364547 ) ) ;
#61005 = CARTESIAN_POINT ( 'NONE',  ( -1.430446194225721390, -0.3690944881889763329, 0.3153832671262228327 ) ) ;
#61006 = CARTESIAN_POINT ( 'NONE',  ( -0.4068241469816267775, 0.05413385826771626580, -0.4176697321401330321 ) ) ;
#61007 = CARTESIAN_POINT ( 'NONE',  ( 0.1640419947506569498, -0.2845877964562161244, -0.3641732283464567121 ) ) ;
#61008 = CARTESIAN_POINT ( 'NONE',  ( -0.8761506516392493227, -2.567464376874931580E-15, -0.4445507791589072832 ) ) ;
#61009 = CARTESIAN_POINT ( 'NONE',  ( 0.4790026246719167324, -0.08942795157527998196, 0.3641732283464567121 ) ) ;
#61010 = CARTESIAN_POINT ( 'NONE',  ( -0.1968503937007867743, 0.2952755905511811885, 0.000000000000000000 ) ) ;
#61011 = CARTESIAN_POINT ( 'NONE',  ( 0.1998031496062992463, 0.3460692066303959202, -0.2211286089238845010 ) ) ;
#61012 = CARTESIAN_POINT ( 'NONE',  ( -1.089238845144356427, 0.05413385826771666132, 0.4176697321401328100 ) ) ;
#61013 = CARTESIAN_POINT ( 'NONE',  ( -0.1049643490035302024, -0.3917322834645671215, -1.889107611548556109 ) ) ;
#61014 = CARTESIAN_POINT ( 'NONE',  ( 0.9514435695538062676, -0.08942795157527998196, 0.3641732283464567121 ) ) ;
#61015 = CARTESIAN_POINT ( 'NONE',  ( 0.006561679790026889343, -0.3162353388693409650, -0.4822834645669289433 ) ) ;
#61016 = CARTESIAN_POINT ( 'NONE',  ( -0.1049868766404193215, -0.6046776061558807314, 0.2411417322834647770 ) ) ;
#61017 = CARTESIAN_POINT ( 'NONE',  ( -0.2427821522309703550, -0.2845877964562159024, 0.3641732283464567677 ) ) ;
#61018 = PLANE ( 'NONE',  #50771 ) ;
#61019 = CARTESIAN_POINT ( 'NONE',  ( -0.3280839895013117347, -0.004921259842519870586, -0.3153832671262229437 ) ) ;
#61020 = CARTESIAN_POINT ( 'NONE',  ( 0.4855643044619430415, -0.4281496062992127816, -0.4176697321401328100 ) ) ;
#61021 = EDGE_CURVE ( 'NONE', #38373, #15637, #3701, .T. ) ;
#61022 = CARTESIAN_POINT ( 'NONE',  ( -1.240157480314959759, 0.07958543189024085140, 0.2665933059059887866 ) ) ;
#61023 = CARTESIAN_POINT ( 'NONE',  ( 0.3996062992125984925, 0.1070741851644054637, -0.8313648293963252778 ) ) ;
#61024 = CARTESIAN_POINT ( 'NONE',  ( -1.049868766404198794, -0.6046776061558807314, 0.2411417322834647770 ) ) ;
#61025 = CARTESIAN_POINT ( 'NONE',  ( -0.4724409448818898682, -8.678599364036362592E-17, -2.635826771653543066 ) ) ;
#61026 = ORIENTED_EDGE ( 'NONE', *, *, #28821, .F. ) ;
#61027 = AXIS2_PLACEMENT_3D ( 'NONE', #39178, #64862, #58540 ) ;
#61028 = ADVANCED_FACE ( 'NONE', ( #72727 ), #64194, .F. ) ;
#61029 = CARTESIAN_POINT ( 'NONE',  ( -1.646981627296586703, -0.2845877964562161244, -0.3641732283464567121 ) ) ;
#61030 = CARTESIAN_POINT ( 'NONE',  ( -0.5708661417322828946, 0.1660481256975883668, -0.3530559997133364547 ) ) ;
#61031 = CARTESIAN_POINT ( 'NONE',  ( 0.3118275472110223490, 1.179820887159493292, -1.417058425483740836 ) ) ;
#61032 = CARTESIAN_POINT ( 'NONE',  ( -1.325459317585300889, 0.05413385826771666132, 0.4176697321401328100 ) ) ;
#61033 = CARTESIAN_POINT ( 'NONE',  ( -0.1958661417322836718, 0.3392501089628017219, -1.672572178477690352 ) ) ;
#61034 = CARTESIAN_POINT ( 'NONE',  ( 0.2881610400590569054, 0.2661962643026990483, -1.220472440944881942 ) ) ;
#61035 = CARTESIAN_POINT ( 'NONE',  ( 1.541994750656168645, 0.2952755905511810774, -0.1292274648535930714 ) ) ;
#61036 = CARTESIAN_POINT ( 'NONE',  ( 0.9055118110236227702, 0.2952755905511811885, 0.000000000000000000 ) ) ;
#61037 = DIRECTION ( 'NONE',  ( 0.000000000000000000, -1.000000000000000000, 0.000000000000000000 ) ) ;
#61038 = CARTESIAN_POINT ( 'NONE',  ( 0.4744094488189011805, 1.537401574803149984, -1.016821367227981998 ) ) ;
#61039 = CARTESIAN_POINT ( 'NONE',  ( -1.620734908136482577, -0.6692913385826773087, -0.1292274648535924053 ) ) ;
#61040 = CARTESIAN_POINT ( 'NONE',  ( 0.3460692066303959202, 0.1998031496062993295, -0.4461942257217847430 ) ) ;
#61041 = ORIENTED_EDGE ( 'NONE', *, *, #34230, .T. ) ;
#61042 = CARTESIAN_POINT ( 'NONE',  ( -0.6496062992125976043, 0.07958543189024071263, -0.2665933059059888421 ) ) ;
#61044 = CARTESIAN_POINT ( 'NONE',  ( 0.3917322834645669549, 0.1049643490035304660, -2.164041994750655729 ) ) ;
#61043 = AXIS2_PLACEMENT_3D ( 'NONE', #60624, #67783, #2974 ) ;
#61045 = ORIENTED_EDGE ( 'NONE', *, *, #63677, .F. ) ;
#61046 = CARTESIAN_POINT ( 'NONE',  ( 0.8202099737532813073, 0.2952755905511811885, 0.1292274648535926551 ) ) ;
#61047 = CARTESIAN_POINT ( 'NONE',  ( -0.4461942257217840213, 0.2306618581243848609, 0.2411417322834645549 ) ) ;
#61048 = CARTESIAN_POINT ( 'NONE',  ( -1.167979002624671470, 0.05413385826771666132, 0.4176697321401328100 ) ) ;
#61049 = CARTESIAN_POINT ( 'NONE',  ( 1.627296587926509996, -0.6046776061558807314, 0.2411417322834647770 ) ) ;
#61050 = CARTESIAN_POINT ( 'NONE',  ( -1.220472440944881054, -0.5511811023622047445, 6.969142054262312111E-17 ) ) ;
#61051 = CARTESIAN_POINT ( 'NONE',  ( 0.03160120395398562099, 1.064035752752396258, -1.466227782781327926 ) ) ;
#61052 = CARTESIAN_POINT ( 'NONE',  ( 0.4330708661417329575, 0.2952755905511811885, 0.000000000000000000 ) ) ;
#61053 = CARTESIAN_POINT ( 'NONE',  ( -0.7677165354330699465, -0.5400638737290845981, -0.3530559997133363437 ) ) ;
#61054 = CARTESIAN_POINT ( 'NONE',  ( 0.3392501089628018329, -0.1958661417322834497, -1.602342888942570154 ) ) ;
#61055 = CARTESIAN_POINT ( 'NONE',  ( -1.384514435695537005, -0.6692913385826773087, -0.1292274648535924053 ) ) ;
#61056 = CARTESIAN_POINT ( 'NONE',  ( 0.08519462842576361328, 1.070400731138066552, -2.867154304459277991 ) ) ;
#61057 = CARTESIAN_POINT ( 'NONE',  ( 0.9186351706036752773, 0.2306618581243847221, -0.2411417322834647770 ) ) ;
#61058 = CARTESIAN_POINT ( 'NONE',  ( 1.443569553805774897, -0.5023911411419708095, -0.1820866141732282451 ) ) ;
#61059 = ORIENTED_EDGE ( 'NONE', *, *, #6668, .F. ) ;
#61060 = CARTESIAN_POINT ( 'NONE',  ( 0.1958661417322836718, -0.3392501089628017219, -2.765767347277902299 ) ) ;
#61061 = CARTESIAN_POINT ( 'NONE',  ( -0.3412073490813641308, 0.2306618581243847221, -0.2411417322834647770 ) ) ;
#61062 = EDGE_LOOP ( 'NONE', ( #46054, #222, #77737, #27188 ) ) ;
#61063 = CARTESIAN_POINT ( 'NONE',  ( 0.5708661417322841158, -0.4536011799217368745, -0.2665933059059886201 ) ) ;
#61064 = CARTESIAN_POINT ( 'NONE',  ( -1.299212598425196097, -0.6692913385826771977, 8.415575281601705876E-17 ) ) ;
#61065 = CARTESIAN_POINT ( 'NONE',  ( 1.023622047244095112, -0.1870078740157480879, -0.4822834645669291653 ) ) ;
#61066 = CARTESIAN_POINT ( 'NONE',  ( 0.8792650918635177559, -0.4281496062992127816, -0.4176697321401328100 ) ) ;
#61067 = CARTESIAN_POINT ( 'NONE',  ( -0.02624671916010428221, -0.6046776061558807314, 0.2411417322834647770 ) ) ;
#61068 = CARTESIAN_POINT ( 'NONE',  ( 0.1049643490035303967, 0.3917322834645670659, -1.092539000821209250 ) ) ;
#61069 = CARTESIAN_POINT ( 'NONE',  ( -0.5905511811023613777, -0.6692913385826771977, 8.415575281601705876E-17 ) ) ;
#61070 = CARTESIAN_POINT ( 'NONE',  ( 0.1049643490035304938, -0.3917322834645669549, -2.374671916010498762 ) ) ;
#61071 = CARTESIAN_POINT ( 'NONE',  ( -1.679790026246718693, 0.2306618581243847221, -0.2411417322834647770 ) ) ;
#61072 = CARTESIAN_POINT ( 'NONE',  ( -1.003937007874014853, 0.1660481256975885056, 0.3530559997133364547 ) ) ;
#61073 = CARTESIAN_POINT ( 'NONE',  ( 1.148293963254593875, -0.6692913385826771977, 0.1292274648535927661 ) ) ;
#61074 = CARTESIAN_POINT ( 'NONE',  ( 1.397637795275591177, 0.1660481256975883668, -0.3530559997133364547 ) ) ;
#61076 = B_SPLINE_CURVE_WITH_KNOTS ( 'NONE', 3,
 ( #21989, #23221, #48891, #47650 ),
 .UNSPECIFIED., .F., .F.,
 ( 4, 4 ),
 ( 3.210432057660995851E-07, 0.001287787053612144111 ),
 .UNSPECIFIED. ) ;
#61075 = CARTESIAN_POINT ( 'NONE',  ( -1.030183727034119867, -0.05778040916215560624, -0.4822834645669293319 ) ) ;
#61077 = CARTESIAN_POINT ( 'NONE',  ( -9.787531504996566615E-17, 0.3996062992125985480, 0.08070866141732283006 ) ) ;
#61078 = CARTESIAN_POINT ( 'NONE',  ( 0.2099737532808405305, 0.2306618581243847221, -0.2411417322834647770 ) ) ;
#61079 = CARTESIAN_POINT ( 'NONE',  ( -0.1998031496062991907, -0.3460692066303959757, -1.797900262467191590 ) ) ;
#61080 = CARTESIAN_POINT ( 'NONE',  ( -0.5446194225721777693, -0.05778040916215522460, 0.4822834645669289988 ) ) ;
#61081 = CARTESIAN_POINT ( 'NONE',  ( 1.594488188976378673, -0.5400638737290845981, -0.3530559997133363437 ) ) ;
#61082 = CARTESIAN_POINT ( 'NONE',  ( 0.5643044619422579178, -0.004921259842519576551, 0.3153832671262227771 ) ) ;
#61083 = CARTESIAN_POINT ( 'NONE',  ( 1.200787401574803681, -0.5400638737290845981, -0.3530559997133363437 ) ) ;
#61084 = CARTESIAN_POINT ( 'NONE',  ( 5.785732909357575061E-17, -0.4724409448818898682, -0.4704724409448819422 ) ) ;
#61085 = CARTESIAN_POINT ( 'NONE',  ( 1.017060367454068803, -0.2845877964562159024, 0.3641732283464567677 ) ) ;
#61086 = CARTESIAN_POINT ( 'NONE',  ( 0.8595800524934390507, -0.05778040916215560624, -0.4822834645669293319 ) ) ;
#61087 = CARTESIAN_POINT ( 'NONE',  ( -0.3949938075777411073, 0.1058382717557497660, -0.5820209973753280863 ) ) ;
#61088 = CARTESIAN_POINT ( 'NONE',  ( -0.5118110236220466680, -0.6692913385826771977, 8.415575281601705876E-17 ) ) ;
#61089 = CARTESIAN_POINT ( 'NONE',  ( 0.5314960629921373636, 2.742781085175769462, -3.250800423740331624 ) ) ;
#61090 = CARTESIAN_POINT ( 'NONE',  ( 1.272965879265092637, -0.004921259842519576551, 0.3153832671262227771 ) ) ;
#61091 = CARTESIAN_POINT ( 'NONE',  ( -0.5511811023622041894, -0.1870078740157480879, -0.4822834645669291653 ) ) ;
#61092 = CARTESIAN_POINT ( 'NONE',  ( -0.3949938075777408852, -0.1058382717557502933, -0.2801837270341207553 ) ) ;
#61093 = CARTESIAN_POINT ( 'NONE',  ( 1.272965879265092637, -0.4281496062992127816, -0.4176697321401328100 ) ) ;
#61094 = CARTESIAN_POINT ( 'NONE',  ( 0.2296587926509192634, -0.05778040916215560624, -0.4822834645669293319 ) ) ;
#61095 = CARTESIAN_POINT ( 'NONE',  ( 0.4002624671916016896, -0.08942795157527998196, 0.3641732283464567121 ) ) ;
#61096 = CARTESIAN_POINT ( 'NONE',  ( -0.2391728406892293379, 1.126541202442033152, -1.096574649324438155 ) ) ;
#61097 = CARTESIAN_POINT ( 'NONE',  ( -0.05249343832020911260, 0.1283753931104748280, 0.1820866141732283561 ) ) ;
#61098 = CARTESIAN_POINT ( 'NONE',  ( -1.555118110236219930, -0.5400638737290845981, -0.3530559997133363437 ) ) ;
#61099 = CARTESIAN_POINT ( 'NONE',  ( 0.1070741851644054776, -0.3996062992125984925, -1.264435695538057569 ) ) ;
#61100 = CARTESIAN_POINT ( 'NONE',  ( 0.7939632545931766261, -0.3162353388693409650, -0.4822834645669289433 ) ) ;
#61101 = CARTESIAN_POINT ( 'NONE',  ( 0.3392501089628018884, -0.1958661417322834220, -1.041994750656167756 ) ) ;
#61102 = CARTESIAN_POINT ( 'NONE',  ( 1.437007874015748810, -0.4536011799217368745, -0.2665933059059886201 ) ) ;
#61103 = CARTESIAN_POINT ( 'NONE',  ( 2.795275590551181466, 1.023622047244095556, -2.156651478620225655E-16 ) ) ;
#61104 = CARTESIAN_POINT ( 'NONE',  ( -0.1312335958005241554, 0.1283753931104748280, 0.1820866141732283561 ) ) ;
#61105 = AXIS2_PLACEMENT_3D ( 'NONE', #29988, #80543, #67481 ) ;
#61106 = CARTESIAN_POINT ( 'NONE',  ( 0.3149606299212606708, -0.1870078740157480879, -0.4822834645669291653 ) ) ;
#61107 = CARTESIAN_POINT ( 'NONE',  ( 1.469816272965879911, -0.5023911411419708095, 0.1820866141732285504 ) ) ;
#61108 = CARTESIAN_POINT ( 'NONE',  ( -1.233595800524933894, 0.1283753931104748280, 0.1820866141732283561 ) ) ;
#61109 = CARTESIAN_POINT ( 'NONE',  ( -1.417322834645668772, -0.1870078740157479769, 0.4822834645669291653 ) ) ;
#61110 = CARTESIAN_POINT ( 'NONE',  ( 0.6955380577427828781, -0.4281496062992124485, 0.4176697321401328655 ) ) ;
#61111 = CARTESIAN_POINT ( 'NONE',  ( 1.253280839895013710, -0.05778040916215560624, -0.4822834645669293319 ) ) ;
#61112 = LINE ( 'NONE', #41351, #14189 ) ;
#61113 = CARTESIAN_POINT ( 'NONE',  ( 0.1312335958005255154, -0.6046776061558807314, 0.2411417322834647770 ) ) ;
#61114 = CARTESIAN_POINT ( 'NONE',  ( 1.312335958005250269, -0.6046776061558807314, 0.2411417322834647770 ) ) ;
#61115 = CARTESIAN_POINT ( 'NONE',  ( 0.8398950131233602345, -0.6046776061558807314, 0.2411417322834647770 ) ) ;
#61116 = CARTESIAN_POINT ( 'NONE',  ( -1.686351706036744558, 0.1771653543307087075, -0.09757992244046823083 ) ) ;
#61117 = CARTESIAN_POINT ( 'NONE',  ( 0.9120734908136490793, 0.1771653543307087075, -0.09757992244046823083 ) ) ;
#61118 = CARTESIAN_POINT ( 'NONE',  ( 1.489501312335958172, -0.3162353388693405765, 0.4822834645669290543 ) ) ;
#61119 = EDGE_CURVE ( 'NONE', #33739, #72166, #25181, .T. ) ;
#61120 = CARTESIAN_POINT ( 'NONE',  ( 0.3543307086614179147, 0.1771653543307087630, 0.000000000000000000 ) ) ;
#61121 = CARTESIAN_POINT ( 'NONE',  ( 0.2034120734908144990, -0.6692913385826771977, 0.1292274648535927661 ) ) ;
#61122 = CARTESIAN_POINT ( 'NONE',  ( 0.5774278215223103139, -0.6046776061558809534, -0.2411417322834644161 ) ) ;
#61123 = CARTESIAN_POINT ( 'NONE',  ( -0.3083989501312330295, -0.3162353388693409650, -0.4822834645669289433 ) ) ;
#61124 = CARTESIAN_POINT ( 'NONE',  ( -0.01312335958005186876, -0.3690944881889763329, 0.3153832671262228327 ) ) ;
#61125 = CARTESIAN_POINT ( 'NONE',  ( 0.8136482939632553313, 0.2306618581243848609, 0.2411417322834645549 ) ) ;
#61126 = DIRECTION ( 'NONE',  ( -1.000000000000000000, -0.000000000000000000, -0.000000000000000000 ) ) ;
#61127 = CARTESIAN_POINT ( 'NONE',  ( -1.128608923884513837, -0.6046776061558807314, 0.2411417322834647770 ) ) ;
#61129 = CARTESIAN_POINT ( 'NONE',  ( 1.586052503253845281, 1.299212598425198095, -0.1653254495020587411 ) ) ;
#61128 = DIRECTION ( 'NONE',  ( -3.491481338843132961E-15, -0.000000000000000000, 1.000000000000000000 ) ) ;
#61130 = CARTESIAN_POINT ( 'NONE',  ( -0.1565620680560287081, 1.056197359954963222, 0.2713048536997808569 ) ) ;
#61131 = CARTESIAN_POINT ( 'NONE',  ( -1.036745406824146176, -0.4281496062992124485, 0.4176697321401328655 ) ) ;
#61132 = CARTESIAN_POINT ( 'NONE',  ( -0.3280839895013117347, -0.4281496062992124485, 0.4176697321401328655 ) ) ;
#61133 = CARTESIAN_POINT ( 'NONE',  ( 0.3996062992125986035, 2.446882876249141962E-17, -2.952755905511811108 ) ) ;
#61134 = CARTESIAN_POINT ( 'NONE',  ( -0.1974969037888706647, 0.3420746716998658843, -2.532808398950130879 ) ) ;
#61135 = ORIENTED_EDGE ( 'NONE', *, *, #12124, .T. ) ;
#61136 = CARTESIAN_POINT ( 'NONE',  ( 0.8005249343832028242, -0.3690944881889765550, -0.3153832671262227771 ) ) ;
#61137 = CARTESIAN_POINT ( 'NONE',  ( 0.3392501089628018329, 0.1958661417322835607, -0.9107611548556429071 ) ) ;
#61138 = CARTESIAN_POINT ( 'NONE',  ( 1.240157480314961314, -0.5400638737290844871, 0.3530559997133364547 ) ) ;
#61139 = CARTESIAN_POINT ( 'NONE',  ( 0.3458507752293908943, 0.3458507752293908943, -2.500000000000000444 ) ) ;
#61140 = CARTESIAN_POINT ( 'NONE',  ( -0.2469196488504575571, 5.952911114587291371E-15, -0.4118484887281962381 ) ) ;
#61141 = CARTESIAN_POINT ( 'NONE',  ( -1.548556430446193399, 0.1283753931104748280, 0.1820866141732283561 ) ) ;
#61142 = CARTESIAN_POINT ( 'NONE',  ( 1.601049868766404982, -0.6046776061558809534, -0.2411417322834644161 ) ) ;
#61143 = CARTESIAN_POINT ( 'NONE',  ( -1.568241469816272105, -0.05778040916215522460, 0.4822834645669289988 ) ) ;
#61144 = CARTESIAN_POINT ( 'NONE',  ( 0.5511811023622055217, -0.1870078740157479769, 0.4822834645669291653 ) ) ;
#61145 = CARTESIAN_POINT ( 'NONE',  ( -0.3392501089628019439, 0.1958661417322832554, -0.1062798968165861030 ) ) ;
#61146 = CARTESIAN_POINT ( 'NONE',  ( -0.01968503937007793844, 0.1660481256975883668, -0.3530559997133364547 ) ) ;
#61147 = CARTESIAN_POINT ( 'NONE',  ( -0.7545931758530177724, 0.1771653543307087630, 0.09757992244046791164 ) ) ;
#61148 = CARTESIAN_POINT ( 'NONE',  ( 1.030183727034121421, -0.3162353388693409650, -0.4822834645669289433 ) ) ;
#61149 = CARTESIAN_POINT ( 'NONE',  ( -0.2034120734908131112, -0.6692913385826773087, -0.1292274648535924053 ) ) ;
#61150 = CARTESIAN_POINT ( 'NONE',  ( 0.5249343832021003964, 0.2306618581243847221, -0.2411417322834647770 ) ) ;
#61151 = CARTESIAN_POINT ( 'NONE',  ( -0.4091458600556405756, 0.2362204724409446288, -1.128608923884514503 ) ) ;
#61152 = CARTESIAN_POINT ( 'NONE',  ( -0.3392501089628017219, -0.1958661417322836995, -1.781515378773965042 ) ) ;
#61153 = CARTESIAN_POINT ( 'NONE',  ( 0.9908136482939640111, -0.6692913385826771977, 0.1292274648535927661 ) ) ;
#61154 = CARTESIAN_POINT ( 'NONE',  ( -0.01312335958005186876, -0.4281496062992124485, 0.4176697321401328655 ) ) ;
#61155 = CARTESIAN_POINT ( 'NONE',  ( -1.102362204724408601, -0.1870078740157480879, -0.4822834645669291653 ) ) ;
#61157 = CARTESIAN_POINT ( 'NONE',  ( 1.017060367454068581, -0.05778040916215560624, -0.4822834645669293319 ) ) ;
#61156 = CIRCLE ( 'NONE', #40981, 0.1978346456692914035 ) ;
#61158 = CARTESIAN_POINT ( 'NONE',  ( 0.2690288713910767848, 0.2952755905511811885, 0.1292274648535926551 ) ) ;
#61159 = CARTESIAN_POINT ( 'NONE',  ( 0.3917322834645670104, -0.1049643490035303411, -0.8261154855643043637 ) ) ;
#61160 = CARTESIAN_POINT ( 'NONE',  ( -0.2296587926509179312, -0.3162353388693409650, -0.4822834645669289433 ) ) ;
#61161 = CARTESIAN_POINT ( 'NONE',  ( 0.5839895013123367340, 0.2952755905511811885, 0.1292274648535926551 ) ) ;
#61162 = CARTESIAN_POINT ( 'NONE',  ( -0.1246719160104980823, -0.6692913385826773087, -0.1292274648535924053 ) ) ;
#61163 = CARTESIAN_POINT ( 'NONE',  ( 0.5971128608923891301, 0.1771653543307087075, -0.09757992244046823083 ) ) ;
#61164 = CARTESIAN_POINT ( 'NONE',  ( -1.692913385826770645, 0.2952755905511811885, 0.000000000000000000 ) ) ;
#61165 = CARTESIAN_POINT ( 'NONE',  ( -0.4725434569952416397, 1.494547573005089447, -2.558822519881354118 ) ) ;
#61166 = CARTESIAN_POINT ( 'NONE',  ( 0.1574803149606306130, -0.1870078740157479769, 0.4822834645669291653 ) ) ;
#61167 = CARTESIAN_POINT ( 'NONE',  ( -0.4091458600556402980, -0.2362204724409451284, -0.9166666666666666297 ) ) ;
#61168 = CARTESIAN_POINT ( 'NONE',  ( 0.1958661417322834775, 0.3392501089628018884, -2.341207349081364963 ) ) ;
#61169 = ORIENTED_EDGE ( 'NONE', *, *, #2754, .T. ) ;
#61170 = ORIENTED_EDGE ( 'NONE', *, *, #13485, .T. ) ;
#61171 = CARTESIAN_POINT ( 'NONE',  ( 1.207349081364829990, 0.2306618581243848609, 0.2411417322834645549 ) ) ;
#61172 = CARTESIAN_POINT ( 'NONE',  ( 0.6167979002624678353, -0.3690944881889763329, 0.3153832671262228327 ) ) ;
#61174 = CARTESIAN_POINT ( 'NONE',  ( 0.4724409448818898682, 2.892866454678787531E-17, -2.165354330708661568 ) ) ;
#61173 = CARTESIAN_POINT ( 'NONE',  ( 0.9563780557770535928, -8.614921172258640174E-17, 0.3791475997938231202 ) ) ;
#61175 = CARTESIAN_POINT ( 'NONE',  ( -0.3917322834645671215, 0.1049643490035301469, -0.5898950131233595684 ) ) ;
#61176 = CARTESIAN_POINT ( 'NONE',  ( 0.4556365110581300226, 1.773775493389249114, -0.5309055118110237448 ) ) ;
#61177 = DIRECTION ( 'NONE',  ( -0.000000000000000000, 1.000000000000000000, -0.000000000000000000 ) ) ;
#61178 = CARTESIAN_POINT ( 'NONE',  ( 0.3392501089628018329, 0.1958661417322835607, -1.475721784776902856 ) ) ;
#61179 = CARTESIAN_POINT ( 'NONE',  ( 0.2925321140481932369, 0.2925321140481932369, -2.576771653543307394 ) ) ;
#61180 = CARTESIAN_POINT ( 'NONE',  ( 0.9251968503937015864, -0.5400638737290844871, 0.3530559997133364547 ) ) ;
#61181 = CARTESIAN_POINT ( 'NONE',  ( -0.9580052493438311334, 0.05413385826771626580, -0.4176697321401330321 ) ) ;
#61182 = CARTESIAN_POINT ( 'NONE',  ( -0.7611548556430438595, 0.2306618581243848609, 0.2411417322834645549 ) ) ;
#61183 = CARTESIAN_POINT ( 'NONE',  ( 0.8267716535433077274, 0.2952755905511811885, 0.000000000000000000 ) ) ;
#61184 = CARTESIAN_POINT ( 'NONE',  ( 1.482939632545932307, 0.05413385826771626580, -0.4176697321401330321 ) ) ;
#61185 = CARTESIAN_POINT ( 'NONE',  ( 1.686351706036745890, 0.1771653543307087630, 0.09757992244046791164 ) ) ;
#61186 = CARTESIAN_POINT ( 'NONE',  ( 1.410761154855643795, -0.08942795157528024563, -0.3641732283464568787 ) ) ;
#61187 = CARTESIAN_POINT ( 'NONE',  ( -0.3996062992125984925, -0.1070741851644056719, -2.169947506561679784 ) ) ;
#61188 = CARTESIAN_POINT ( 'NONE',  ( -1.404199475065615932, -0.3690944881889765550, -0.3153832671262227771 ) ) ;
#61189 = CARTESIAN_POINT ( 'NONE',  ( -0.1958661417322834220, -0.3392501089628018884, 0.09973753280839897650 ) ) ;
#61190 = CARTESIAN_POINT ( 'NONE',  ( 0.02624671916010564918, -0.6046776061558809534, -0.2411417322834644161 ) ) ;
#61192 = DIRECTION ( 'NONE',  ( 0.000000000000000000, 0.000000000000000000, -1.000000000000000000 ) ) ;
#61191 = CARTESIAN_POINT ( 'NONE',  ( 1.627296587926509996, -0.6046776061558807314, 0.2411417322834647770 ) ) ;
#61193 = CARTESIAN_POINT ( 'NONE',  ( -1.115485564304461219, -0.3690944881889763329, 0.3153832671262228327 ) ) ;
#61194 = CARTESIAN_POINT ( 'NONE',  ( 0.2821522309711292364, 0.2952755905511810774, -0.1292274648535930714 ) ) ;
#61195 = CARTESIAN_POINT ( 'NONE',  ( 1.469816272965879911, 0.1283753931104746893, -0.1820866141732285504 ) ) ;
#61196 = CARTESIAN_POINT ( 'NONE',  ( 4.797336870675655290E-17, -0.3917322834645669549, -1.418615854821835276 ) ) ;
#61197 = CARTESIAN_POINT ( 'NONE',  ( -1.135170603674539924, -0.5511811023622046335, 0.09757992244046803654 ) ) ;
#61198 = CARTESIAN_POINT ( 'NONE',  ( 1.220472440944882608, 0.2952755905511811885, 0.000000000000000000 ) ) ;
#61199 = CARTESIAN_POINT ( 'NONE',  ( 0.2607642859107343059, 1.870951849707525927, 0.1732250691923664654 ) ) ;
#61200 = CARTESIAN_POINT ( 'NONE',  ( -0.006561679790025524116, -0.3162353388693405765, 0.4822834645669290543 ) ) ;
#61201 = CARTESIAN_POINT ( 'NONE',  ( -1.358267716535432434, -0.4536011799217367080, 0.2665933059059888421 ) ) ;
#61202 = CARTESIAN_POINT ( 'NONE',  ( -0.6167979002624665030, 0.05413385826771666132, 0.4176697321401328100 ) ) ;
#61203 = CARTESIAN_POINT ( 'NONE',  ( -1.614173228346455824, 0.1771653543307087630, 0.000000000000000000 ) ) ;
#61204 = CARTESIAN_POINT ( 'NONE',  ( -0.3917322834645670659, -7.196005306013484475E-17, -0.6660298144695031564 ) ) ;
#61205 = CARTESIAN_POINT ( 'NONE',  ( 0.4593175853018379162, -0.4281496062992124485, 0.4176697321401328655 ) ) ;
#61206 = EDGE_CURVE ( 'NONE', #5989, #26718, #70927, .T. ) ;
#61207 = CARTESIAN_POINT ( 'NONE',  ( 1.581364829396326277, -0.05778040916215522460, 0.4822834645669289988 ) ) ;
#61208 = CARTESIAN_POINT ( 'NONE',  ( 0.4091458600556403535, 0.2362204724409449896, -1.940288713910761187 ) ) ;
#61209 = VECTOR ( 'NONE', #16480, 39.37007874015748143 ) ;
#61210 = CARTESIAN_POINT ( 'NONE',  ( -1.233595800524933894, 0.2306618581243848609, 0.2411417322834645549 ) ) ;
#61211 = CARTESIAN_POINT ( 'NONE',  ( -0.4593175853018366950, -0.004921259842519576551, 0.3153832671262227771 ) ) ;
#61212 = CARTESIAN_POINT ( 'NONE',  ( -1.646051170424378096, 0.4405861044731112508, 0.3149606299212598381 ) ) ;
#61213 = CARTESIAN_POINT ( 'NONE',  ( 0.1574803149606306130, -0.1870078740157480879, -0.4822834645669291653 ) ) ;
#61214 = CARTESIAN_POINT ( 'NONE',  ( 0.5183727034120741983, -0.5511811023622046335, 0.09757992244046803654 ) ) ;
#61215 = CARTESIAN_POINT ( 'NONE',  ( -0.9448818897637790704, -0.1870078740157479769, 0.3641732283464567677 ) ) ;
#61216 = CARTESIAN_POINT ( 'NONE',  ( -1.502624671916009680, -0.05778040916215560624, -0.4822834645669293319 ) ) ;
#61217 = CARTESIAN_POINT ( 'NONE',  ( -1.404199475065615932, 0.05413385826771666132, 0.4176697321401328100 ) ) ;
#61218 = ADVANCED_FACE ( 'NONE', ( #73142 ), #26163, .F. ) ;
#61219 = CARTESIAN_POINT ( 'NONE',  ( 1.476377952755906442, -0.5400638737290844871, 0.3530559997133364547 ) ) ;
#61220 = CARTESIAN_POINT ( 'NONE',  ( -1.586052503253849055, 0.4724409448818907564, -0.1653254495020551051 ) ) ;
#61221 = CARTESIAN_POINT ( 'NONE',  ( 0.4527559055118117182, 0.07958543189024071263, -0.2665933059059888421 ) ) ;
#61222 = CARTESIAN_POINT ( 'NONE',  ( 0.7874015748031503170, -0.1870078740157480879, -0.4822834645669291653 ) ) ;
#61223 = LINE ( 'NONE', #10314, #429 ) ;
#61224 = CARTESIAN_POINT ( 'NONE',  ( 1.535433070866142335, -0.5511811023622047445, 6.969142054262312111E-17 ) ) ;
#61225 = B_SPLINE_CURVE_WITH_KNOTS ( 'NONE', 3,
 ( #47814, #28878, #60452, #28049, #1559, #73929, #2804, #79838 ),
 .UNSPECIFIED., .F., .F.,
 ( 4, 2, 2, 4 ),
 ( 0.03812540793793221805, 0.03934516121038392905, 0.04056491448283564699, 0.04300442102773906899 ),
 .UNSPECIFIED. ) ;
#61226 = EDGE_LOOP ( 'NONE', ( #77238, #51535, #29153, #19733 ) ) ;
#61227 = CARTESIAN_POINT ( 'NONE',  ( -1.148293963254592542, 0.2952755905511811885, 0.1292274648535926551 ) ) ;
#61228 = CARTESIAN_POINT ( 'NONE',  ( -0.8661417322834640276, -0.1870078740157479769, 0.4822834645669291653 ) ) ;
#61229 = CARTESIAN_POINT ( 'NONE',  ( 0.4002624671916016896, -0.3162353388693409650, -0.4822834645669289433 ) ) ;
#61230 = CARTESIAN_POINT ( 'NONE',  ( -1.719160104986876103, -0.004921259842519576551, 0.3153832671262227771 ) ) ;
#61231 = CARTESIAN_POINT ( 'NONE',  ( 0.3460692066303958092, 0.1998031496062993018, -2.097769028871391050 ) ) ;
#61232 = CARTESIAN_POINT ( 'NONE',  ( 1.056430446194226436, -0.6692913385826773087, -0.1292274648535924053 ) ) ;
#61233 = CARTESIAN_POINT ( 'NONE',  ( -1.699475065616797398, 0.2952755905511811885, 0.1292274648535926551 ) ) ;
#61234 = CARTESIAN_POINT ( 'NONE',  ( 0.3740157480314966754, -0.5400638737290844871, 0.3530559997133364547 ) ) ;
#61235 = CARTESIAN_POINT ( 'NONE',  ( 0.6496062992125991586, 0.1660481256975885056, 0.3530559997133364547 ) ) ;
#61236 = CARTESIAN_POINT ( 'NONE',  ( 0.1998031496062994405, -0.3460692066303958092, -1.824146981627296604 ) ) ;
#61237 = CARTESIAN_POINT ( 'NONE',  ( 0.1058382717557499880, 0.3949938075777411073, -1.253280839895013488 ) ) ;
#61238 = B_SPLINE_CURVE_WITH_KNOTS ( 'NONE', 3,
 ( #22941, #35577, #48196, #28427 ),
 .UNSPECIFIED., .F., .F.,
 ( 4, 4 ),
 ( 0.09384283614957933395, 0.09527263441391617405 ),
 .UNSPECIFIED. ) ;
#61239 = CARTESIAN_POINT ( 'NONE',  ( -0.3996062992125986035, -0.1070741851644056997, -2.565616797900262647 ) ) ;
#61240 = CARTESIAN_POINT ( 'NONE',  ( -0.1500752278769512948, -0.2544983382031791308, 0.1555222293686583102 ) ) ;
#61241 = CARTESIAN_POINT ( 'NONE',  ( 0.1049643490035304799, -0.3917322834645669549, -0.3923884514435694859 ) ) ;
#61242 = CARTESIAN_POINT ( 'NONE',  ( -0.1968503937007867743, -0.5511811023622047445, 6.969142054262312111E-17 ) ) ;
#61243 = CARTESIAN_POINT ( 'NONE',  ( -0.2952755905511804668, 0.1660481256975885056, 0.3530559997133364547 ) ) ;
#61244 = CARTESIAN_POINT ( 'NONE',  ( 0.7677165354330716118, -0.5400638737290844871, 0.3530559997133364547 ) ) ;
#61245 = CARTESIAN_POINT ( 'NONE',  ( -9.674558042662122972E-17, 0.3949938075777409963, -2.281496062992126372 ) ) ;
#61246 = CARTESIAN_POINT ( 'NONE',  ( -0.07874015748031421014, -0.1870078740157479769, 0.3641732283464567677 ) ) ;
#61247 = CARTESIAN_POINT ( 'NONE',  ( -1.305774278215222184, 0.2952755905511811885, 0.1292274648535926551 ) ) ;
#61248 = CARTESIAN_POINT ( 'NONE',  ( 1.010498687664042716, 0.05413385826771626580, -0.4176697321401330321 ) ) ;
#61249 = CARTESIAN_POINT ( 'NONE',  ( 0.4724409448818898682, 2.892866454678787531E-17, -2.480314960629921295 ) ) ;
#61250 = CARTESIAN_POINT ( 'NONE',  ( -0.3996062992125986035, -7.340648628747425578E-17, -1.929133858267716439 ) ) ;
#61251 = DIRECTION ( 'NONE',  ( -3.096699300667737957E-16, 1.000000000000000000, -0.000000000000000000 ) ) ;
#61252 = ORIENTED_EDGE ( 'NONE', *, *, #24864, .T. ) ;
#61253 = CARTESIAN_POINT ( 'NONE',  ( 0.8202099737532813073, 0.2952755905511811885, 0.1292274648535926551 ) ) ;
#61254 = CARTESIAN_POINT ( 'NONE',  ( 1.312335958005249825, 0.1283753931104746893, -0.1820866141732285504 ) ) ;
#61256 = CARTESIAN_POINT ( 'NONE',  ( 1.535433070866142335, -0.6692913385826771977, 8.415575281601705876E-17 ) ) ;
#61255 = CARTESIAN_POINT ( 'NONE',  ( -1.522309711286088607, -0.5023911411419708095, 0.1820866141732285504 ) ) ;
#61257 = CARTESIAN_POINT ( 'NONE',  ( -0.3392501089628019439, 0.1958661417322832554, -2.625964936186665266 ) ) ;
#61258 = LINE ( 'NONE', #66345, #47752 ) ;
#61259 = CARTESIAN_POINT ( 'NONE',  ( 1.384514435695538559, 0.2952755905511810774, -0.1292274648535930714 ) ) ;
#61260 = CARTESIAN_POINT ( 'NONE',  ( -1.732283464566928277, -0.1870078740157479769, 0.4822834645669291653 ) ) ;
#61261 = CARTESIAN_POINT ( 'NONE',  ( 0.03280839895013198948, 0.2952755905511811885, 0.1292274648535926551 ) ) ;
#61262 = CARTESIAN_POINT ( 'NONE',  ( -0.7742782152230965886, 0.05413385826771666132, 0.4176697321401328100 ) ) ;
#61263 = CARTESIAN_POINT ( 'NONE',  ( 1.437007874015748810, 0.1660481256975885056, 0.3530559997133364547 ) ) ;
#61264 = CARTESIAN_POINT ( 'NONE',  ( -0.3392501089628019995, 0.1958661417322832277, 0.04658792650918625738 ) ) ;
#61265 = CARTESIAN_POINT ( 'NONE',  ( 0.01968503937007930540, 0.1660481256975885056, 0.3530559997133364547 ) ) ;
#61266 = CARTESIAN_POINT ( 'NONE',  ( -0.3917322834645669549, -0.1049643490035306603, -2.242782152230970993 ) ) ;
#61267 = CARTESIAN_POINT ( 'NONE',  ( 1.515748031496063408, 0.1660481256975885056, 0.3530559997133364547 ) ) ;
#61268 = VERTEX_POINT ( 'NONE', #75852 ) ;
#61269 = CARTESIAN_POINT ( 'NONE',  ( -0.2891555358219908833, -0.2891555358219912164, -2.736220472440944462 ) ) ;
#61270 = ORIENTED_EDGE ( 'NONE', *, *, #37699, .F. ) ;
#61271 = CARTESIAN_POINT ( 'NONE',  ( 0.000000000000000000, 1.724409448818897905, 0.000000000000000000 ) ) ;
#61272 = CONICAL_SURFACE ( 'NONE', #77441, 0.1771653543307085410, 1.029744258676653645 ) ;
#61273 = CARTESIAN_POINT ( 'NONE',  ( -1.712598425196849572, 0.1660481256975885056, 0.3530559997133364547 ) ) ;
#61274 = CARTESIAN_POINT ( 'NONE',  ( 0.3996062992125986590, -0.1070741851644053111, -0.8989501312335956840 ) ) ;
#61275 = CARTESIAN_POINT ( 'NONE',  ( 0.5631141337314363726, 7.053449127088339072E-16, 0.3627989612356146698 ) ) ;
#61276 = LINE ( 'NONE', #3629, #18208 ) ;
#61277 = CARTESIAN_POINT ( 'NONE',  ( -0.9973753280839886548, 0.2306618581243848609, 0.2411417322834645549 ) ) ;
#61278 = CARTESIAN_POINT ( 'NONE',  ( 0.01987007963503858304, -0.3948464311378711011, -2.755905511811022279 ) ) ;
#61279 = CARTESIAN_POINT ( 'NONE',  ( 0.3917322834645669549, 0.1049643490035304660, -0.2093175853018373611 ) ) ;
#61280 = CARTESIAN_POINT ( 'NONE',  ( -0.1115485564304453947, -0.5511811023622046335, 0.09757992244046803654 ) ) ;
#61281 = EDGE_CURVE ( 'NONE', #47808, #1757, #8976, .T. ) ;
#61282 = CARTESIAN_POINT ( 'NONE',  ( -0.8989501312335946848, 0.1771653543307087075, -0.09757992244046823083 ) ) ;
#61283 = CARTESIAN_POINT ( 'NONE',  ( -1.345144356955379816, -0.3162353388693405765, 0.4822834645669290543 ) ) ;
#61284 = CARTESIAN_POINT ( 'NONE',  ( 0.5708661417322841158, -0.5400638737290845981, -0.3530559997133363437 ) ) ;
#61285 = CARTESIAN_POINT ( 'NONE',  ( -1.240157480314959759, -0.5400638737290845981, -0.3530559997133363437 ) ) ;
#61286 = CARTESIAN_POINT ( 'NONE',  ( 0.2867679344610365999, 0.2867679344610365999, 0.02755905511811028441 ) ) ;
#61287 = EDGE_LOOP ( 'NONE', ( #4341, #43639, #26297, #31206, #64464, #45101, #47981, #76258, #45922, #61350, #67918, #75337, #75626, #32453, #40862, #68206, #69267, #54323, #5578, #81147, #1363 ) ) ;
#61288 = CARTESIAN_POINT ( 'NONE',  ( -1.469816272965878357, 0.2306618581243848609, 0.2411417322834645549 ) ) ;
#61289 = CARTESIAN_POINT ( 'NONE',  ( -1.604771003085129211, 2.104981124449682550, -0.1466069496707751996 ) ) ;
#61290 = CARTESIAN_POINT ( 'NONE',  ( 0.3458507752293908943, 0.3458507752293908943, -1.555118110236220597 ) ) ;
#61291 = DIRECTION ( 'NONE',  ( 0.000000000000000000, 0.000000000000000000, -1.000000000000000000 ) ) ;
#61292 = CARTESIAN_POINT ( 'NONE',  ( 0.3917322834645670104, 2.398668435337828261E-17, -0.5826771653543306728 ) ) ;
#61293 = LINE ( 'NONE', #62539, #72132 ) ;
#61294 = CARTESIAN_POINT ( 'NONE',  ( -0.9120734908136475250, -0.6692913385826773087, -0.1292274648535924053 ) ) ;
#61295 = CARTESIAN_POINT ( 'NONE',  ( 1.581364829396326277, -0.3162353388693409650, -0.4822834645669289433 ) ) ;
#61297 = CARTESIAN_POINT ( 'NONE',  ( -0.4724409448818898682, -8.678599364036362592E-17, -1.929133858267716439 ) ) ;
#61296 = CARTESIAN_POINT ( 'NONE',  ( -1.719160104986876103, 0.05413385826771666132, 0.4176697321401328100 ) ) ;
#61298 = CARTESIAN_POINT ( 'NONE',  ( 1.522309711286089939, 0.2306618581243848609, 0.2411417322834645549 ) ) ;
#61299 = CARTESIAN_POINT ( 'NONE',  ( -1.017060367454067249, -0.3162353388693409650, -0.4822834645669289433 ) ) ;
#61300 = CARTESIAN_POINT ( 'NONE',  ( -0.3917322834645668994, -0.1049643490035306742, 0.1889956937345949883 ) ) ;
#61301 = CARTESIAN_POINT ( 'NONE',  ( -0.09186351706036689768, -0.004921259842519870586, -0.3153832671262229437 ) ) ;
#61302 = CARTESIAN_POINT ( 'NONE',  ( -0.1049643490035307020, 0.3917322834645669549, -0.4061679790026246906 ) ) ;
#61303 = CARTESIAN_POINT ( 'NONE',  ( -0.05905511811023545637, 0.07958543189024085140, 0.2665933059059887866 ) ) ;
#61304 = CARTESIAN_POINT ( 'NONE',  ( 0.9514435695538062676, -0.08942795157527998196, 0.3641732283464567121 ) ) ;
#61305 = CARTESIAN_POINT ( 'NONE',  ( 0.3674540682414705883, 0.2306618581243847221, -0.2411417322834647770 ) ) ;
#61306 = PRODUCT_DEFINITION_CONTEXT ( 'detailed design', #67026, 'design' ) ;
#61307 = CARTESIAN_POINT ( 'NONE',  ( -0.2362204724409440182, -0.1870078740157479769, 0.3641732283464567677 ) ) ;
#61308 = CARTESIAN_POINT ( 'NONE',  ( -0.3917322834645671215, 0.1049643490035301469, -2.387139107611548905 ) ) ;
#61309 = CARTESIAN_POINT ( 'NONE',  ( -1.515748031496062076, -0.5400638737290844871, 0.3530559997133364547 ) ) ;
#61310 = VECTOR ( 'NONE', #26825, 39.37007874015748143 ) ;
#61311 = CARTESIAN_POINT ( 'NONE',  ( -1.318897637795274802, 0.07958543189024085140, 0.2665933059059887866 ) ) ;
#61312 = CARTESIAN_POINT ( 'NONE',  ( -0.2362204724409451284, 0.4091458600556402425, -0.8772965879265091083 ) ) ;
#61313 = VECTOR ( 'NONE', #33784, 39.37007874015748143 ) ;
#61314 = CARTESIAN_POINT ( 'NONE',  ( 0.1706036745406830368, 0.05413385826771666132, 0.4176697321401328100 ) ) ;
#61315 = CARTESIAN_POINT ( 'NONE',  ( -0.4658792650918627265, -0.3162353388693409650, -0.4822834645669289433 ) ) ;
#61316 = CARTESIAN_POINT ( 'NONE',  ( -0.3372635250547070807, -0.3676148930005934123, -0.006554863637384360751 ) ) ;
#61317 = CARTESIAN_POINT ( 'NONE',  ( 0.4921259842519691285, 0.07958543189024085140, 0.2665933059059887866 ) ) ;
#61318 = CARTESIAN_POINT ( 'NONE',  ( -0.06561679790026180015, -0.4281496062992127816, -0.4176697321401328100 ) ) ;
#61319 = CARTESIAN_POINT ( 'NONE',  ( -0.7414698162729651543, -0.6692913385826771977, 0.1292274648535927661 ) ) ;
#61320 = DIRECTION ( 'NONE',  ( 0.000000000000000000, 1.000000000000000000, 0.000000000000000000 ) ) ;
#61321 = CYLINDRICAL_SURFACE ( 'NONE', #12600, 0.2165354330708660069 ) ;
#61322 = CARTESIAN_POINT ( 'NONE',  ( 0.07874015748031558404, -0.1870078740157479769, 0.4822834645669291653 ) ) ;
#61323 = CARTESIAN_POINT ( 'NONE',  ( 0.2925321140481932369, 0.2925321140481932369, -1.631889763779527325 ) ) ;
#61324 = CARTESIAN_POINT ( 'NONE',  ( -1.586052503253847501, 1.299212598425198095, -0.1653254495020571035 ) ) ;
#61325 = CARTESIAN_POINT ( 'NONE',  ( -0.2099737532808391705, -0.5023911411419708095, -0.1820866141732282451 ) ) ;
#61326 = CIRCLE ( 'NONE', #77499, 0.1771653543307085410 ) ;
#61327 = CARTESIAN_POINT ( 'NONE',  ( -0.3871391076115479057, -0.3162353388693409650, -0.4822834645669289433 ) ) ;
#61328 = CARTESIAN_POINT ( 'NONE',  ( -1.509186351706035767, -0.3690944881889763329, 0.3153832671262228327 ) ) ;
#61329 = CARTESIAN_POINT ( 'NONE',  ( 1.502624671916010790, -0.05778040916215522460, 0.4822834645669289988 ) ) ;
#61330 = CARTESIAN_POINT ( 'NONE',  ( -1.476377952755905110, 0.1660481256975885056, 0.3530559997133364547 ) ) ;
#61331 = CARTESIAN_POINT ( 'NONE',  ( -0.8136482939632537770, -0.5023911411419708095, 0.1820866141732285504 ) ) ;
#61332 = CARTESIAN_POINT ( 'NONE',  ( -0.2925321140481932369, 0.2925321140481930704, -0.09645669291338584972 ) ) ;
#61333 = CARTESIAN_POINT ( 'NONE',  ( 0.1998031496062994405, -0.3460692066303958092, -0.7217847769028871152 ) ) ;
#61334 = CARTESIAN_POINT ( 'NONE',  ( 0.2867679344610366554, 0.2867679344610366554, -2.811699105808085797 ) ) ;
#61335 = CARTESIAN_POINT ( 'NONE',  ( 1.404199475065617708, -0.004921259842519870586, -0.3153832671262229437 ) ) ;
#61336 = ADVANCED_FACE ( 'NONE', ( #62379 ), #44243, .F. ) ;
#61337 = CARTESIAN_POINT ( 'NONE',  ( 1.259842519685040019, -0.1870078740157479769, 0.3641732283464567677 ) ) ;
#61338 = CARTESIAN_POINT ( 'NONE',  ( 1.043307086614173818, -0.5400638737290845981, -0.3530559997133363437 ) ) ;
#61339 = CARTESIAN_POINT ( 'NONE',  ( -1.712598425196849572, 0.1660481256975885056, 0.3530559997133364547 ) ) ;
#61340 = CARTESIAN_POINT ( 'NONE',  ( 0.8858267716535438430, -0.5400638737290845981, -0.3530559997133363437 ) ) ;
#61341 = CARTESIAN_POINT ( 'NONE',  ( 0.1974969037888704704, 0.3420746716998660508, -0.6935695538057742304 ) ) ;
#61342 = CARTESIAN_POINT ( 'NONE',  ( 1.187664041994751285, -0.08942795157527998196, 0.3641732283464567121 ) ) ;
#61343 = EDGE_CURVE ( 'NONE', #33736, #16379, #68245, .T. ) ;
#61344 = CARTESIAN_POINT ( 'NONE',  ( 0.09842519685039434474, 0.1660481256975885056, 0.3530559997133364547 ) ) ;
#61345 = CARTESIAN_POINT ( 'NONE',  ( -0.6824146981627288167, 0.2306618581243848609, 0.2411417322834645549 ) ) ;
#61346 = CARTESIAN_POINT ( 'NONE',  ( -2.503252890251015828, 2.755905511811024056, -0.5314960629921260393 ) ) ;
#61347 = CARTESIAN_POINT ( 'NONE',  ( 0.3458507752293908943, 0.3458507752293908943, -1.240157480314960647 ) ) ;
#61348 = CARTESIAN_POINT ( 'NONE',  ( -0.2925321140481932369, 0.2925321140481931814, -2.381889763779527769 ) ) ;
#61349 = CARTESIAN_POINT ( 'NONE',  ( 0.4855643044619428750, -0.004921259842519576551, 0.3153832671262227771 ) ) ;
#61350 = ORIENTED_EDGE ( 'NONE', *, *, #2281, .F. ) ;
#61351 = CARTESIAN_POINT ( 'NONE',  ( 0.3917322834645670104, 0.1049643490035304660, -0.5938513367792144226 ) ) ;
#61352 = EDGE_LOOP ( 'NONE', ( #82587, #71016, #46332, #57829 ) ) ;
#61353 = CARTESIAN_POINT ( 'NONE',  ( -0.5643044619422565855, 0.05413385826771626580, -0.4176697321401330321 ) ) ;
#61354 = CARTESIAN_POINT ( 'NONE',  ( -0.07217847769028787330, -0.05778040916215522460, 0.4822834645669289988 ) ) ;
#61355 = CARTESIAN_POINT ( 'NONE',  ( -0.1574803149606292529, -0.1870078740157480879, -0.4822834645669291653 ) ) ;
#61356 = CARTESIAN_POINT ( 'NONE',  ( 0.6167979002624679463, 0.05413385826771626580, -0.4176697321401330321 ) ) ;
#61357 = CARTESIAN_POINT ( 'NONE',  ( -0.8070866141732276899, 0.1660481256975883668, -0.3530559997133364547 ) ) ;
#61358 = CARTESIAN_POINT ( 'NONE',  ( -0.4527559055118102749, 0.1660481256975885056, 0.3530559997133364547 ) ) ;
#61359 = CARTESIAN_POINT ( 'NONE',  ( 0.9776902887139113929, 0.2952755905511811885, 0.1292274648535926551 ) ) ;
#61360 = EDGE_CURVE ( 'NONE', #45388, #37563, #49335, .T. ) ;
#61361 = CARTESIAN_POINT ( 'NONE',  ( 0.2952755905511816326, -0.5400638737290844871, 0.3530559997133364547 ) ) ;
#61362 = CARTESIAN_POINT ( 'NONE',  ( 0.9514435695538062676, -0.3162353388693409650, -0.4822834645669289433 ) ) ;
#61363 = EDGE_CURVE ( 'NONE', #55851, #7036, #21902, .T. ) ;
#61364 = CARTESIAN_POINT ( 'NONE',  ( 0.3392501089628018884, -0.1958661417322834220, -1.199475065616797842 ) ) ;
#61365 = CARTESIAN_POINT ( 'NONE',  ( -0.1902887139107604098, 0.1771653543307087075, -0.09757992244046823083 ) ) ;
#61366 = ORIENTED_EDGE ( 'NONE', *, *, #74915, .F. ) ;
#61367 = CARTESIAN_POINT ( 'NONE',  ( -0.1058382717557503211, 0.3949938075777409408, -0.9514435695538059345 ) ) ;
#61368 = VERTEX_POINT ( 'NONE', #35895 ) ;
#61369 = CARTESIAN_POINT ( 'NONE',  ( -0.8661417322834640276, -0.1870078740157480601, -0.3641732283464567677 ) ) ;
#61370 = VECTOR ( 'NONE', #10140, 39.37007874015748143 ) ;
#61371 = AXIS2_PLACEMENT_3D ( 'NONE', #77396, #58438, #19730 ) ;
#61372 = CARTESIAN_POINT ( 'NONE',  ( -0.5643044619422565855, -0.4281496062992124485, 0.4176697321401328655 ) ) ;
#61373 = CARTESIAN_POINT ( 'NONE',  ( 0.7759054087898769048, 2.575861430505332611E-15, -0.3791475997938230091 ) ) ;
#61374 = CARTESIAN_POINT ( 'NONE',  ( -0.8464566929133852113, -0.5400638737290845981, -0.3530559997133363437 ) ) ;
#61375 = CARTESIAN_POINT ( 'NONE',  ( -0.5183727034120726440, -0.6692913385826773087, -0.1292274648535924053 ) ) ;
#61376 = MANIFOLD_SOLID_BREP ( 'Chamfer1', #20538 ) ;
#61377 = CARTESIAN_POINT ( 'NONE',  ( -1.095800524934382292, -0.3162353388693409650, -0.4822834645669289433 ) ) ;
#61378 = CARTESIAN_POINT ( 'NONE',  ( -1.423884514435694859, -0.3162353388693405765, 0.4822834645669290543 ) ) ;
#61379 = CARTESIAN_POINT ( 'NONE',  ( 0.7677165354330716118, 0.07958543189024071263, -0.2665933059059888421 ) ) ;
#61380 = CARTESIAN_POINT ( 'NONE',  ( -0.5314960629921395840, 2.755905511811024056, 3.900966923095588346 ) ) ;
#61381 = CARTESIAN_POINT ( 'NONE',  ( 0.2945219335573386332, 0.02405856270293458068, 5.877884953661865808 ) ) ;
#61382 = CARTESIAN_POINT ( 'NONE',  ( 0.6299212598425204535, -0.1870078740157479769, 0.3641732283464567677 ) ) ;
#61383 = CARTESIAN_POINT ( 'NONE',  ( -0.03937007874015669567, 0.2952755905511811885, 0.000000000000000000 ) ) ;
#61384 = CARTESIAN_POINT ( 'NONE',  ( -0.2165354330708654795, 0.1660481256975885056, 0.3530559997133364547 ) ) ;
#61385 = VERTEX_POINT ( 'NONE', #37944 ) ;
#61386 = CARTESIAN_POINT ( 'NONE',  ( 4.893765752498283924E-17, -0.3996062992125986035, -1.496062992125984259 ) ) ;
#61387 = FACE_OUTER_BOUND ( 'NONE', #61062, .T. ) ;
#61388 = ORIENTED_EDGE ( 'NONE', *, *, #20062, .F. ) ;
#61389 = CARTESIAN_POINT ( 'NONE',  ( 0.1998031496062994128, -0.3460692066303957537, -1.113517060367454015 ) ) ;
#61390 = CARTESIAN_POINT ( 'NONE',  ( -0.7874015748031492068, 2.204724409448818978, 0.000000000000000000 ) ) ;
#61391 = CARTESIAN_POINT ( 'NONE',  ( -0.5643044619422565855, -0.004921259842519870586, -0.3153832671262229437 ) ) ;
#61392 = CARTESIAN_POINT ( 'NONE',  ( -0.8923884514435688198, 0.2306618581243847221, -0.2411417322834647770 ) ) ;
#61393 = CARTESIAN_POINT ( 'NONE',  ( 0.2362204724409451007, -0.4091458600556402980, -0.4068241469816273326 ) ) ;
#61394 = CARTESIAN_POINT ( 'NONE',  ( 0.3917322834645669549, 0.1049643490035304660, -2.729002624671915900 ) ) ;
#61395 = CARTESIAN_POINT ( 'NONE',  ( 1.594488188976378673, -0.5400638737290845981, -0.3530559997133363437 ) ) ;
#61396 = CARTESIAN_POINT ( 'NONE',  ( 0.4593175853018379162, -0.4281496062992124485, 0.4176697321401328655 ) ) ;
#61397 = CARTESIAN_POINT ( 'NONE',  ( 0.5774278215223104249, 0.2306618581243848609, 0.2411417322834645549 ) ) ;
#61398 = CARTESIAN_POINT ( 'NONE',  ( -0.7349081364829387342, -0.5023911411419708095, 0.1820866141732285504 ) ) ;
#61399 = CARTESIAN_POINT ( 'NONE',  ( -0.03937007874015669567, -0.6692913385826771977, 8.415575281601705876E-17 ) ) ;
#61400 = CARTESIAN_POINT ( 'NONE',  ( -0.3458507752293906723, -0.3458507752293910609, -2.340551181102362488 ) ) ;
#61401 = CARTESIAN_POINT ( 'NONE',  ( -0.5774278215223089816, 0.2306618581243847221, -0.2411417322834647770 ) ) ;
#61402 = CARTESIAN_POINT ( 'NONE',  ( 0.1058382717557499880, 0.3949938075777409408, -1.802493438320210251 ) ) ;
#61403 = CARTESIAN_POINT ( 'NONE',  ( 1.095800524934383846, -0.2845877964562159024, 0.3641732283464567677 ) ) ;
#61404 = CARTESIAN_POINT ( 'NONE',  ( 0.2690288713910767848, -0.5511811023622048555, -0.09757992244046775898 ) ) ;
#61405 = CARTESIAN_POINT ( 'NONE',  ( 1.305774278215223960, -0.5511811023622046335, 0.09757992244046803654 ) ) ;
#61406 = CARTESIAN_POINT ( 'NONE',  ( -1.338582677165353729, -0.1870078740157480879, -0.4822834645669291653 ) ) ;
#61407 = CARTESIAN_POINT ( 'NONE',  ( -0.5643044619422565855, -0.3690944881889763329, 0.3153832671262228327 ) ) ;
#61408 = LINE ( 'NONE', #15572, #57380 ) ;
#61409 = CARTESIAN_POINT ( 'NONE',  ( -1.148293963254592542, -0.6692913385826773087, -0.1292274648535924053 ) ) ;
#61410 = CARTESIAN_POINT ( 'NONE',  ( -0.6036745406824141069, -0.6046776061558809534, -0.2411417322834644161 ) ) ;
#61411 = CARTESIAN_POINT ( 'NONE',  ( 0.4593175853018380828, 0.05413385826771626580, -0.4176697321401330321 ) ) ;
#61412 = CARTESIAN_POINT ( 'NONE',  ( -0.3917322834645668994, -0.1049643490035306742, -2.488169660596113886 ) ) ;
#61413 = CARTESIAN_POINT ( 'NONE',  ( 1.948818897637795367, 0.000000000000000000, 5.879133660591329580 ) ) ;
#61414 = CARTESIAN_POINT ( 'NONE',  ( 0.5183727034120741983, -0.5511811023622046335, 0.09757992244046803654 ) ) ;
#61415 = CARTESIAN_POINT ( 'NONE',  ( 0.8661417322834652488, -0.1870078740157480879, -0.4822834645669291653 ) ) ;
#61416 = CARTESIAN_POINT ( 'NONE',  ( -1.154855643044618851, -0.5023911411419708095, -0.1820866141732282451 ) ) ;
#61417 = CARTESIAN_POINT ( 'NONE',  ( 1.233595800524935227, 0.2306618581243847221, -0.2411417322834647770 ) ) ;
#61418 = CARTESIAN_POINT ( 'NONE',  ( -1.404199475065615932, -0.004921259842519576551, 0.3153832671262227771 ) ) ;
#61419 = CARTESIAN_POINT ( 'NONE',  ( -1.469816272965878357, -0.6046776061558809534, -0.2411417322834644161 ) ) ;
#61420 = CARTESIAN_POINT ( 'NONE',  ( -0.7808398950131225646, -0.05778040916215522460, 0.4822834645669289988 ) ) ;
#61421 = CARTESIAN_POINT ( 'NONE',  ( 8.195543980992789655E-16, -0.1870078740157480601, -0.3641732283464567677 ) ) ;
#61422 = LINE ( 'NONE', #8843, #21923 ) ;
#61423 = CARTESIAN_POINT ( 'NONE',  ( 0.5249343832021003964, 0.1283753931104746893, -0.1820866141732285504 ) ) ;
#61424 = AXIS2_PLACEMENT_3D ( 'NONE', #78426, #39688, #15277 ) ;
#61425 = EDGE_CURVE ( 'NONE', #39595, #41210, #15794, .T. ) ;
#61426 = CARTESIAN_POINT ( 'NONE',  ( 0.02624671916010564918, -0.6046776061558809534, -0.2411417322834644161 ) ) ;
#61427 = CARTESIAN_POINT ( 'NONE',  ( -9.787531504996566615E-17, 0.3996062992125985480, -0.2342519685039370358 ) ) ;
#61428 = CARTESIAN_POINT ( 'NONE',  ( -1.115485564304461219, -0.4281496062992124485, 0.4176697321401328655 ) ) ;
#61429 = AXIS2_PLACEMENT_3D ( 'NONE', #3343, #54673, #80385 ) ;
#61430 = CARTESIAN_POINT ( 'NONE',  ( 0.2867679344610365999, 0.2867679344610365999, -1.797244094488188892 ) ) ;
#61431 = CARTESIAN_POINT ( 'NONE',  ( 0.8923884514435701520, -0.5023911411419708095, -0.1820866141732282451 ) ) ;
#61433 = MECHANICAL_DESIGN_GEOMETRIC_PRESENTATION_REPRESENTATION (  '', ( #72196 ), #64135 ) ;
#61432 = CARTESIAN_POINT ( 'NONE',  ( -0.1509186351706028884, -0.3162353388693409650, -0.4822834645669289433 ) ) ;
#61434 = VECTOR ( 'NONE', #36954, 39.37007874015748143 ) ;
#61435 = CARTESIAN_POINT ( 'NONE',  ( -0.2887139107611542133, -0.6046776061558809534, -0.2411417322834644161 ) ) ;
#61436 = CARTESIAN_POINT ( 'NONE',  ( -0.5774278215223089816, -0.5023911411419708095, 0.1820866141732285504 ) ) ;
#61437 = CARTESIAN_POINT ( 'NONE',  ( 0.9842519685039375910, 0.2066929133858268208, 0.000000000000000000 ) ) ;
#61438 = CARTESIAN_POINT ( 'NONE',  ( -0.5511811023622038563, -0.1870078740157479769, 0.3641732283464567677 ) ) ;
#61439 = CARTESIAN_POINT ( 'NONE',  ( 0.3937007874015754361, -0.1870078740157479769, 0.4822834645669291653 ) ) ;
#61440 = CARTESIAN_POINT ( 'NONE',  ( -1.286089238845143479, -0.5023911411419708095, 0.1820866141732285504 ) ) ;
#61441 = CARTESIAN_POINT ( 'NONE',  ( 0.1998031496062994128, -0.3460692066303957537, -0.9560367454068241511 ) ) ;
#61442 = CARTESIAN_POINT ( 'NONE',  ( -1.417322834645668772, -0.1870078740157480879, -0.4822834645669291653 ) ) ;
#61443 = CARTESIAN_POINT ( 'NONE',  ( 0.4724409448818880919, 0.1265901696525020825, -2.563648293963254776 ) ) ;
#61444 = ORIENTED_EDGE ( 'NONE', *, *, #25507, .T. ) ;
#61445 = CARTESIAN_POINT ( 'NONE',  ( -1.437007874015747477, -0.4536011799217367080, 0.2665933059059888421 ) ) ;
#61446 = CARTESIAN_POINT ( 'NONE',  ( -0.6430446194225716283, -0.4281496062992124485, 0.4176697321401328655 ) ) ;
#61447 = CARTESIAN_POINT ( 'NONE',  ( -1.358267716535432434, -0.5400638737290844871, 0.3530559997133364547 ) ) ;
#61448 = CARTESIAN_POINT ( 'NONE',  ( 0.1049643490035304938, -0.3917322834645669549, -1.587270341207349222 ) ) ;
#61449 = LINE ( 'NONE', #41269, #12234 ) ;
#61450 = CARTESIAN_POINT ( 'NONE',  ( 1.325459317585302665, -0.4281496062992124485, 0.4176697321401328655 ) ) ;
#61451 = CARTESIAN_POINT ( 'NONE',  ( 0.2690288713910767848, 0.2952755905511811885, 0.1292274648535926551 ) ) ;
#61452 = DIRECTION ( 'NONE',  ( 0.000000000000000000, 0.000000000000000000, 1.000000000000000000 ) ) ;
#61453 = CARTESIAN_POINT ( 'NONE',  ( 4.893765752498283308E-17, -0.3996062992125985480, -2.360236220472441193 ) ) ;
#61454 = B_SPLINE_CURVE_WITH_KNOTS ( 'NONE', 3,
 ( #67084, #80556, #49361, #16156, #61165, #16574, #68731, #17405, #61998, #29185, #10668, #54853, #23277, #15748, #48529, #29592, #74229, #55665, #79725, #55255, #9416, #48947, #35086, #60752, #28769, #80141, #22463, #48121, #30417, #25330 ),
 .UNSPECIFIED., .F., .F.,
 ( 4, 2, 2, 2, 2, 2, 2, 2, 2, 2, 2, 2, 2, 2, 4 ),
 ( 0.005313729678161549161, 0.005969797177608808514, 0.006625864677056067867, 0.007937999675950588307, 0.009250134674845107013, 0.01056226967373962572, 0.01318653967152868742, 0.01581080966931774912, 0.01712294466821228170, 0.01843507966710681428, 0.02105934966489587251, 0.02237148466379040163, 0.02368361966268493074, 0.02499575466157945985, 0.02630788966047398897 ),
 .UNSPECIFIED. ) ;
#61455 = CARTESIAN_POINT ( 'NONE',  ( 1.541994750656168645, -0.5511811023622046335, 0.09757992244046803654 ) ) ;
#61456 = CARTESIAN_POINT ( 'NONE',  ( 0.1070741851644054915, -0.3996062992125986035, -0.5577427821522309426 ) ) ;
#61457 = ORIENTED_EDGE ( 'NONE', *, *, #22925, .F. ) ;
#61458 = CARTESIAN_POINT ( 'NONE',  ( -1.062992125984250968, -0.5511811023622047445, 6.969142054262312111E-17 ) ) ;
#61459 = CARTESIAN_POINT ( 'NONE',  ( -0.3392501089628019995, 0.1958661417322832277, -2.223097112860892288 ) ) ;
#61460 = ORIENTED_EDGE ( 'NONE', *, *, #60948, .F. ) ;
#61461 = CARTESIAN_POINT ( 'NONE',  ( 0.8530183727034126306, 0.05413385826771626580, -0.4176697321401330321 ) ) ;
#61462 = CARTESIAN_POINT ( 'NONE',  ( -0.2034120734908131112, -0.6692913385826773087, -0.1292274648535924053 ) ) ;
#61463 = CARTESIAN_POINT ( 'NONE',  ( -1.279527559055116948, 0.1660481256975883668, -0.3530559997133364547 ) ) ;
#61464 = CARTESIAN_POINT ( 'NONE',  ( 1.122047244094488860, -0.5400638737290845981, -0.3530559997133363437 ) ) ;
#61465 = CARTESIAN_POINT ( 'NONE',  ( -1.174540682414697335, -0.08942795157527998196, 0.3641732283464567121 ) ) ;
#61466 = CARTESIAN_POINT ( 'NONE',  ( 0.08907927694007038155, -1.094630224652485432E-15, 0.4281993546915535687 ) ) ;
#61467 = CARTESIAN_POINT ( 'NONE',  ( 0.2165354330708668673, -0.5400638737290844871, 0.3530559997133364547 ) ) ;
#61468 = CARTESIAN_POINT ( 'NONE',  ( -0.7611548556430438595, -0.6046776061558809534, -0.2411417322834644161 ) ) ;
#61469 = CARTESIAN_POINT ( 'NONE',  ( 0.1049643490035303689, 0.3917322834645668994, -1.648274647472754095 ) ) ;
#61470 = CARTESIAN_POINT ( 'NONE',  ( -1.167979002624671470, 0.05413385826771666132, 0.4176697321401328100 ) ) ;
#61471 = CARTESIAN_POINT ( 'NONE',  ( 0.4359958488159859646, 1.724409448818897905, -3.937007874015760578 ) ) ;
#61472 = CARTESIAN_POINT ( 'NONE',  ( 1.076115485564305141, 0.2306618581243847221, -0.2411417322834647770 ) ) ;
#61473 = CARTESIAN_POINT ( 'NONE',  ( 0.1958661417322836440, -0.3392501089628017219, 0.07349081364829400387 ) ) ;
#61474 = CARTESIAN_POINT ( 'NONE',  ( 1.286089238845145033, -0.5023911411419708095, -0.1820866141732282451 ) ) ;
#61475 = ORIENTED_EDGE ( 'NONE', *, *, #46438, .F. ) ;
#61476 = CARTESIAN_POINT ( 'NONE',  ( 0.2867679344610366554, 0.2867679344610366554, -2.811699105808085797 ) ) ;
#61477 = CARTESIAN_POINT ( 'NONE',  ( -0.4921259842519677963, 0.1660481256975883668, -0.3530559997133364547 ) ) ;
#61478 = ORIENTED_EDGE ( 'NONE', *, *, #53988, .T. ) ;
#61479 = CARTESIAN_POINT ( 'NONE',  ( 0.4593175853018379162, -0.3690944881889763329, 0.3153832671262228327 ) ) ;
#61480 = CARTESIAN_POINT ( 'NONE',  ( -1.496062992125983815, -0.1870078740157480879, -0.4822834645669291653 ) ) ;
#61481 = CARTESIAN_POINT ( 'NONE',  ( 0.5446194225721792126, -0.05778040916215560624, -0.4822834645669293319 ) ) ;
#61482 = CARTESIAN_POINT ( 'NONE',  ( 0.8727034120734912248, -0.3162353388693409650, -0.4822834645669289433 ) ) ;
#61483 = CARTESIAN_POINT ( 'NONE',  ( -0.1837270341207343505, -0.6046776061558807314, 0.2411417322834647770 ) ) ;
#61484 = CARTESIAN_POINT ( 'NONE',  ( -9.594673741351313045E-17, 0.3917322834645670659, -1.256580995571865200 ) ) ;
#61485 = CARTESIAN_POINT ( 'NONE',  ( -0.9317585301837263412, -0.4281496062992127816, -0.4176697321401328100 ) ) ;
#61486 = EDGE_CURVE ( 'NONE', #23692, #64172, #10882, .T. ) ;
#61487 = CARTESIAN_POINT ( 'NONE',  ( -0.3917322834645670104, -7.196005306013484475E-17, -2.171259842519685179 ) ) ;
#61488 = CARTESIAN_POINT ( 'NONE',  ( -1.437007874015747477, -0.5400638737290844871, 0.3530559997133364547 ) ) ;
#61489 = CARTESIAN_POINT ( 'NONE',  ( -0.9120734908136475250, -0.6692913385826773087, -0.1292274648535924053 ) ) ;
#61490 = CARTESIAN_POINT ( 'NONE',  ( 1.122047244094488860, -0.5400638737290845981, -0.3530559997133363437 ) ) ;
#61491 = CARTESIAN_POINT ( 'NONE',  ( 1.594488188976378673, -0.5400638737290845981, -0.3530559997133363437 ) ) ;
#61492 = CARTESIAN_POINT ( 'NONE',  ( -9.787531504996567848E-17, 0.3996062992125986035, -0.3149606299212598381 ) ) ;
#61493 = CARTESIAN_POINT ( 'NONE',  ( -1.056430446194224881, 0.2952755905511810774, -0.1292274648535930714 ) ) ;
#61494 = CARTESIAN_POINT ( 'NONE',  ( -1.948818897637795367, 0.000000000000000000, 5.701968306260621233 ) ) ;
#61495 = CARTESIAN_POINT ( 'NONE',  ( 0.4724409448818904789, -0.1870078740157479769, 0.4822834645669291653 ) ) ;
#61496 = CARTESIAN_POINT ( 'NONE',  ( 0.3460692066303959202, 0.1998031496062993295, -2.493438320209973469 ) ) ;
#61497 = CARTESIAN_POINT ( 'NONE',  ( -0.5708661417322825615, -0.5400638737290844871, 0.3530559997133364547 ) ) ;
#61498 = CONICAL_SURFACE ( 'NONE', #38646, 0.1978346456692914035, 0.8726646259971685415 ) ;
#61499 = CARTESIAN_POINT ( 'NONE',  ( -1.627296587926508442, 0.1283753931104748280, 0.1820866141732283561 ) ) ;
#61500 = CARTESIAN_POINT ( 'NONE',  ( 0.6758530183727039509, -0.5511811023622046335, 0.09757992244046803654 ) ) ;
#61501 = CARTESIAN_POINT ( 'NONE',  ( 1.233595800524935227, -0.6046776061558807314, 0.2411417322834647770 ) ) ;
#61502 = CARTESIAN_POINT ( 'NONE',  ( -0.3458507752293909498, 0.3458507752293907833, -1.198818897637795367 ) ) ;
#61503 = CARTESIAN_POINT ( 'NONE',  ( 0.7086614173228353852, -0.1870078740157479769, 0.3641732283464567677 ) ) ;
#61504 = ADVANCED_FACE ( 'NONE', ( #50971 ), #61498, .F. ) ;
#61505 = CARTESIAN_POINT ( 'NONE',  ( 0.6496062992125991586, 0.1660481256975885056, 0.3530559997133364547 ) ) ;
#61506 = CARTESIAN_POINT ( 'NONE',  ( 0.1974969037888706092, -0.3420746716998660508, -0.6410761154855643129 ) ) ;
#61507 = CARTESIAN_POINT ( 'NONE',  ( -0.5774278215223089816, 0.2306618581243847221, -0.2411417322834647770 ) ) ;
#61508 = DIRECTION ( 'NONE',  ( -0.000000000000000000, -0.000000000000000000, -1.000000000000000000 ) ) ;
#61509 = CARTESIAN_POINT ( 'NONE',  ( 1.299212598425197429, 0.1771653543307087630, 0.000000000000000000 ) ) ;
#61510 = CARTESIAN_POINT ( 'NONE',  ( -0.7086614173228339419, -0.1870078740157480879, -0.4822834645669291653 ) ) ;
#61511 = EDGE_CURVE ( 'NONE', #5038, #65535, #27908, .T. ) ;
#61512 = CARTESIAN_POINT ( 'NONE',  ( 0.1312335958005255154, -0.6046776061558807314, 0.2411417322834647770 ) ) ;
#61513 = CARTESIAN_POINT ( 'NONE',  ( -1.135170603674539924, 0.2952755905511810219, -0.1292274648535930437 ) ) ;
#61514 = CARTESIAN_POINT ( 'NONE',  ( -0.02624671916010428221, -0.6046776061558807314, 0.2411417322834647770 ) ) ;
#61515 = CARTESIAN_POINT ( 'NONE',  ( 0.4199475065616805614, 0.1283753931104748280, 0.1820866141732283561 ) ) ;
#61516 = CARTESIAN_POINT ( 'NONE',  ( -0.4319747415000730895, 1.340679305999893600, -1.035581624764630115 ) ) ;
#61517 = CARTESIAN_POINT ( 'NONE',  ( 0.1377952755905518800, 0.07958543189024071263, -0.2665933059059888421 ) ) ;
#61518 = CARTESIAN_POINT ( 'NONE',  ( 0.8398950131233602345, 0.1283753931104746893, -0.1820866141732285504 ) ) ;
#61519 = CARTESIAN_POINT ( 'NONE',  ( -1.049868766404198794, 0.1539470093639521697, -0.1968503937007875793 ) ) ;
#61520 = CARTESIAN_POINT ( 'NONE',  ( 0.2925321140481932369, -0.2925321140481931814, -1.120078740157480324 ) ) ;
#61521 = CARTESIAN_POINT ( 'NONE',  ( 0.6889763779527566800, -0.5400638737290844871, 0.3530559997133364547 ) ) ;
#61522 = CARTESIAN_POINT ( 'NONE',  ( 0.3392501089628018884, -0.1958661417322834220, -1.199475065616797842 ) ) ;
#61523 = CARTESIAN_POINT ( 'NONE',  ( 1.633858267716535639, -0.4536011799217367080, 0.2665933059059888421 ) ) ;
#61524 = CARTESIAN_POINT ( 'NONE',  ( 0.1115485564304470184, 0.2952755905511811885, 0.1292274648535926551 ) ) ;
#61525 = CARTESIAN_POINT ( 'NONE',  ( 0.1771653543307093182, 0.07958543189024085140, 0.2665933059059887866 ) ) ;
#61526 = CARTESIAN_POINT ( 'NONE',  ( 0.2230971128608932319, -0.4281496062992124485, 0.4176697321401328655 ) ) ;
#61527 = CARTESIAN_POINT ( 'NONE',  ( 1.299212598425197429, -0.5511811023622047445, 6.969142054262312111E-17 ) ) ;
#61528 = CARTESIAN_POINT ( 'NONE',  ( -1.227034120734907585, 0.1771653543307087630, 0.09757992244046791164 ) ) ;
#61529 = CARTESIAN_POINT ( 'NONE',  ( -1.364829396325458521, 0.2306618581243847221, -0.2411417322834647770 ) ) ;
#61530 = CARTESIAN_POINT ( 'NONE',  ( 0.2690288713910767848, 0.2952755905511811885, 0.1292274648535926551 ) ) ;
#61531 = EDGE_CURVE ( 'NONE', #46748, #21089, #76668, .T. ) ;
#61532 = CARTESIAN_POINT ( 'NONE',  ( 1.148293963254593875, -0.6692913385826771977, 0.1292274648535927661 ) ) ;
#61533 = DIRECTION ( 'NONE',  ( 0.000000000000000000, 0.000000000000000000, -1.000000000000000000 ) ) ;
#61534 = CARTESIAN_POINT ( 'NONE',  ( 0.1115485564304467270, -0.6692913385826773087, -0.1292274648535924053 ) ) ;
#61535 = CARTESIAN_POINT ( 'NONE',  ( 1.377952755905512472, 0.2952755905511811885, 0.000000000000000000 ) ) ;
#61536 = CARTESIAN_POINT ( 'NONE',  ( 0.8858267716535438430, 0.1660481256975885056, 0.3530559997133364547 ) ) ;
#61537 = CARTESIAN_POINT ( 'NONE',  ( -0.2362204724409447953, -0.4091458600556404646, -0.2998687664041995160 ) ) ;
#61538 = CARTESIAN_POINT ( 'NONE',  ( 0.9973753280839902091, -0.5023911411419708095, 0.1820866141732285504 ) ) ;
#61539 = CARTESIAN_POINT ( 'NONE',  ( 1.607611548556431069, -0.6692913385826773087, -0.1292274648535924053 ) ) ;
#61540 = EDGE_CURVE ( 'NONE', #25753, #65725, #79173, .T. ) ;
#61541 = CARTESIAN_POINT ( 'NONE',  ( 0.1837270341207354329, 0.1283753931104748280, 0.1820866141732283561 ) ) ;
#61542 = CARTESIAN_POINT ( 'NONE',  ( 0.1115485564304470323, 0.2952755905511811885, 0.1292274648535926551 ) ) ;
#61543 = CARTESIAN_POINT ( 'NONE',  ( 0.6430446194225728496, 0.05413385826771666132, 0.4176697321401328100 ) ) ;
#61544 = CARTESIAN_POINT ( 'NONE',  ( -0.4855643044619415427, 0.05413385826771626580, -0.4176697321401330321 ) ) ;
#61545 = CARTESIAN_POINT ( 'NONE',  ( 0.1958661417322834775, 0.3392501089628018884, -2.188339525755591986 ) ) ;
#61546 = CARTESIAN_POINT ( 'NONE',  ( -0.4396325459317579898, 0.1771653543307087630, 0.09757992244046791164 ) ) ;
#61547 = CARTESIAN_POINT ( 'NONE',  ( 0.6496062992125991586, 0.1660481256975885056, 0.3530559997133364547 ) ) ;
#61549 = CARTESIAN_POINT ( 'NONE',  ( 1.043307086614173818, 0.07958543189024085140, 0.2665933059059887866 ) ) ;
#61548 = B_SPLINE_CURVE_WITH_KNOTS ( 'NONE', 3,
 ( #31237, #12311, #56904, #76292, #25746, #63644, #70369, #5983, #31654, #83009, #12724, #38383, #64060, #6399, #8499, #71216, #47192, #21533 ),
 .UNSPECIFIED., .F., .F.,
 ( 4, 2, 2, 2, 2, 2, 2, 2, 4 ),
 ( 0.000000000000000000, 2.503579457911093929E-05, 5.007158915822187858E-05, 0.0001001431783164417514, 0.0002002863566328814428, 0.0004005727132657608798, 0.0008011454265315193744, 0.001602290853063036364, 0.003204581706126070559 ),
 .UNSPECIFIED. ) ;
#61550 = FACE_BOUND ( 'NONE', #15385, .T. ) ;
#61552 = CARTESIAN_POINT ( 'NONE',  ( -0.2925321140481930704, -0.2925321140481933480, -1.003937007874015741 ) ) ;
#61551 = CARTESIAN_POINT ( 'NONE',  ( -1.092353285368623750, -2.191421614605370878E-15, 0.4445507791589071167 ) ) ;
#61553 = CARTESIAN_POINT ( 'NONE',  ( -1.220472440944882830, 0.2066929133858268208, 2.389277853677468338E-14 ) ) ;
#61554 = VECTOR ( 'NONE', #46308, 39.37007874015748143 ) ;
#61555 = CARTESIAN_POINT ( 'NONE',  ( -1.194225721784776262, -0.4281496062992124485, 0.4176697321401328655 ) ) ;
#61556 = CARTESIAN_POINT ( 'NONE',  ( -0.4790026246719154557, -0.3162353388693405765, 0.4822834645669290543 ) ) ;
#61557 = CARTESIAN_POINT ( 'NONE',  ( -0.2362204724409447953, -0.4091458600556404646, -0.06561679790026246628 ) ) ;
#61558 = CARTESIAN_POINT ( 'NONE',  ( -0.3420746716998659953, -0.1974969037888706647, -2.414698162729658648 ) ) ;
#61559 = ORIENTED_EDGE ( 'NONE', *, *, #15443, .T. ) ;
#61560 = CARTESIAN_POINT ( 'NONE',  ( 0.2755905511811031494, 0.1771653543307087630, 0.000000000000000000 ) ) ;
#61561 = CARTESIAN_POINT ( 'NONE',  ( -0.1049643490035307020, 0.3917322834645669549, -1.101049868766403872 ) ) ;
#61562 = CARTESIAN_POINT ( 'NONE',  ( 0.8989501312335963501, -0.6692913385826773087, -0.1292274648535924053 ) ) ;
#61563 = CARTESIAN_POINT ( 'NONE',  ( 0.2362204724409449064, 0.4091458600556404646, -2.506561679790026087 ) ) ;
#61564 = CARTESIAN_POINT ( 'NONE',  ( 1.013613127888309595, -4.408777212815537393E-16, -0.4445507791589063395 ) ) ;
#61565 = CARTESIAN_POINT ( 'NONE',  ( 0.000000000000000000, 0.000000000000000000, 0.000000000000000000 ) ) ;
#61566 = DIRECTION ( 'NONE',  ( 0.000000000000000000, 0.000000000000000000, 1.000000000000000000 ) ) ;
#61567 = CARTESIAN_POINT ( 'NONE',  ( 1.384514435695538337, -0.5511811023622046335, 0.09757992244046803654 ) ) ;
#61568 = CARTESIAN_POINT ( 'NONE',  ( 0.4790026246719168435, -0.3162353388693409650, -0.4822834645669289433 ) ) ;
#61569 = CARTESIAN_POINT ( 'NONE',  ( 0.3392501089628018329, 0.1958661417322835052, -0.2112667734570061184 ) ) ;
#61570 = CARTESIAN_POINT ( 'NONE',  ( 0.04593175853018440641, -0.6692913385826771977, 0.1292274648535927661 ) ) ;
#61571 = CARTESIAN_POINT ( 'NONE',  ( -1.089238845144356427, -0.004921259842519576551, 0.3153832671262227771 ) ) ;
#61572 = CARTESIAN_POINT ( 'NONE',  ( 0.4461942257217855201, -0.6046776061558807314, 0.2411417322834647770 ) ) ;
#61573 = CARTESIAN_POINT ( 'NONE',  ( 0.04593175853018440641, 0.2952755905511810774, -0.1292274648535930714 ) ) ;
#61574 = CARTESIAN_POINT ( 'NONE',  ( 0.4744094488188839720, 1.537401574803149984, 3.908320185825793658 ) ) ;
#61575 = CARTESIAN_POINT ( 'NONE',  ( -0.4724409448818908119, 0.1265901696524971698, -1.135170603674540590 ) ) ;
#61576 = CARTESIAN_POINT ( 'NONE',  ( -0.3917322834645670659, -7.196005306013484475E-17, -1.610911704233282560 ) ) ;
#61577 = CARTESIAN_POINT ( 'NONE',  ( 0.9711286089238851948, -0.6046776061558809534, -0.2411417322834644161 ) ) ;
#61578 = CARTESIAN_POINT ( 'NONE',  ( -0.1443569553805768291, 0.05413385826771666132, 0.4176697321401328100 ) ) ;
#61579 = CARTESIAN_POINT ( 'NONE',  ( -1.154855643044618851, 0.2306618581243848609, 0.2411417322834645549 ) ) ;
#61580 = CARTESIAN_POINT ( 'NONE',  ( 1.108923884514436242, -0.05778040916215522460, 0.4822834645669289988 ) ) ;
#61581 = CARTESIAN_POINT ( 'NONE',  ( 0.4790026246719168435, -0.3162353388693409650, -0.4822834645669289433 ) ) ;
#61582 = CARTESIAN_POINT ( 'NONE',  ( 0.1958661417322836440, -0.3392501089628017219, -0.9639107611548557442 ) ) ;
#61583 = CARTESIAN_POINT ( 'NONE',  ( -0.3543307086614165824, -0.6692913385826771977, 8.415575281601705876E-17 ) ) ;
#61584 = CARTESIAN_POINT ( 'NONE',  ( 0.2690288713910767848, 0.2952755905511811885, 0.1292274648535926551 ) ) ;
#61585 = CARTESIAN_POINT ( 'NONE',  ( -0.3674540682414689785, 0.2306618581243848609, 0.2411417322834645549 ) ) ;
#61586 = CARTESIAN_POINT ( 'NONE',  ( 0.1902887139107617975, -0.5511811023622048555, -0.09757992244046775898 ) ) ;
#61587 = CARTESIAN_POINT ( 'NONE',  ( -1.633858267716534529, -0.5400638737290845981, -0.3530559997133363437 ) ) ;
#61588 = LINE ( 'NONE', #68330, #78594 ) ;
#61589 = CARTESIAN_POINT ( 'NONE',  ( 0.2887139107611556010, -0.6046776061558807314, 0.2411417322834647770 ) ) ;
#61590 = LINE ( 'NONE', #9011, #65476 ) ;
#61591 = CARTESIAN_POINT ( 'NONE',  ( 1.371391076115485719, -0.6692913385826773087, -0.1292274648535924053 ) ) ;
#61592 = CARTESIAN_POINT ( 'NONE',  ( -0.1958661417322834220, -0.3392501089628018884, -2.419947506561679784 ) ) ;
#61593 = ORIENTED_EDGE ( 'NONE', *, *, #47818, .F. ) ;
#61594 = EDGE_LOOP ( 'NONE', ( #53053, #47595, #6406, #9640 ) ) ;
#61595 = CARTESIAN_POINT ( 'NONE',  ( 0.5446194225721792126, -0.3162353388693405765, 0.4822834645669290543 ) ) ;
#61596 = CARTESIAN_POINT ( 'NONE',  ( 0.6233595800524939223, -0.2845877964562159024, 0.3641732283464567677 ) ) ;
#61598 = CARTESIAN_POINT ( 'NONE',  ( 2.795275590551181466, 2.165354330708662012, 0.000000000000000000 ) ) ;
#61597 = CARTESIAN_POINT ( 'NONE',  ( 0.5314960629921070545, 2.755905511811024056, 1.813482582612299110 ) ) ;
#61599 = CARTESIAN_POINT ( 'NONE',  ( -0.3392501089628017219, -0.1958661417322836718, -0.7670603674540683592 ) ) ;
#61600 = CARTESIAN_POINT ( 'NONE',  ( 5.785732909357575061E-17, -0.4724409448818898682, 0.001968503937007862279 ) ) ;
#61601 = CARTESIAN_POINT ( 'NONE',  ( 0.7190005367825900162, -6.840088175765282460E-16, 0.4281993546915531246 ) ) ;
#61602 = ADVANCED_FACE ( 'NONE', ( #920 ), #26577, .F. ) ;
#61603 = CARTESIAN_POINT ( 'NONE',  ( -0.3996062992125986590, 0.1070741851644051723, -2.629265091863517423 ) ) ;
#61604 = APPLICATION_CONTEXT ( 'automotive_design' ) ;
#61605 = CARTESIAN_POINT ( 'NONE',  ( 0.8202099737532813073, 0.2952755905511811885, 0.1292274648535926551 ) ) ;
#61606 = CARTESIAN_POINT ( 'NONE',  ( -0.6167979002624665030, -0.4281496062992127816, -0.4176697321401328100 ) ) ;
#61607 = CARTESIAN_POINT ( 'NONE',  ( -0.5314960629921254842, -0.5400638737290845981, -0.3530559997133363437 ) ) ;
#61608 = CARTESIAN_POINT ( 'NONE',  ( 0.7545931758530188826, -0.6692913385826771977, 0.1292274648535927661 ) ) ;
#61609 = CARTESIAN_POINT ( 'NONE',  ( 1.443569553805774897, 0.2306618581243848609, 0.2411417322834645549 ) ) ;
#61610 = CARTESIAN_POINT ( 'NONE',  ( -1.016821367227983997, 1.537401574803149984, 0.4744094488188970171 ) ) ;
#61611 = CONTEXT_DEPENDENT_SHAPE_REPRESENTATION ( #18095, #32501 ) ;
#61612 = CARTESIAN_POINT ( 'NONE',  ( 1.417322834645670104, -0.1870078740157480601, -0.3641732283464567677 ) ) ;
#61613 = CARTESIAN_POINT ( 'NONE',  ( -0.1070741851644057135, 0.3996062992125984925, -1.973097112860892510 ) ) ;
#61614 = CARTESIAN_POINT ( 'NONE',  ( -1.410761154855641575, -0.2845877964562161244, -0.3641732283464567121 ) ) ;
#61615 = CARTESIAN_POINT ( 'NONE',  ( -0.3392501089628019995, 0.1958661417322832277, -0.01837270341207344546 ) ) ;
#61616 = CARTESIAN_POINT ( 'NONE',  ( 0.2952755905511819101, 0.1660481256975883668, -0.3530559997133364547 ) ) ;
#61618 = DIRECTION ( 'NONE',  ( 0.000000000000000000, -1.000000000000000000, 0.000000000000000000 ) ) ;
#61617 = CARTESIAN_POINT ( 'NONE',  ( 1.200787401574803681, 0.1660481256975885056, 0.3530559997133364547 ) ) ;
#61619 = CARTESIAN_POINT ( 'NONE',  ( -1.227034120734907585, 0.1771653543307087630, 0.09757992244046791164 ) ) ;
#61620 = CARTESIAN_POINT ( 'NONE',  ( 0.3608923884514443348, -0.6692913385826771977, 0.1292274648535927661 ) ) ;
#61621 = CARTESIAN_POINT ( 'NONE',  ( 1.095800524934383846, -0.2845877964562159024, 0.3641732283464567677 ) ) ;
#61622 = CARTESIAN_POINT ( 'NONE',  ( -0.2867679344610366554, 0.2867679344610365444, -1.674521366632859110 ) ) ;
#61623 = CARTESIAN_POINT ( 'NONE',  ( -1.305774278215222184, -0.5511811023622048555, -0.09757992244046775898 ) ) ;
#61624 = CARTESIAN_POINT ( 'NONE',  ( 1.312335958005250269, -0.6046776061558807314, 0.2411417322834647770 ) ) ;
#61625 = CARTESIAN_POINT ( 'NONE',  ( 0.3072681130597426091, 1.737353037853611948, 0.06208766824286577474 ) ) ;
#61626 = CARTESIAN_POINT ( 'NONE',  ( -0.2690288713910754526, 0.1771653543307087075, -0.09757992244046823083 ) ) ;
#61627 = CARTESIAN_POINT ( 'NONE',  ( -0.2624671916010490880, 0.2306618581243847221, -0.2411417322834647770 ) ) ;
#61628 = CARTESIAN_POINT ( 'NONE',  ( -1.437007874015747477, 0.07958543189024071263, -0.2665933059059888421 ) ) ;
#61629 = CARTESIAN_POINT ( 'NONE',  ( -0.6299212598425188991, -0.1870078740157479769, 0.4822834645669291653 ) ) ;
#61630 = CARTESIAN_POINT ( 'NONE',  ( -1.404199475065615932, -0.3690944881889765550, -0.3153832671262227771 ) ) ;
#61631 = CARTESIAN_POINT ( 'NONE',  ( 0.2867679344610366554, 0.2867679344610366554, -0.4494943813986370107 ) ) ;
#61632 = SHAPE_REPRESENTATION ( 'Chuck Key Tool', ( #22098 ), #65183 ) ;
#61633 = CARTESIAN_POINT ( 'NONE',  ( -1.646051170424378096, 0.000000000000000000, -0.3464511005275205946 ) ) ;
#61634 = CARTESIAN_POINT ( 'NONE',  ( 1.463254593175853824, 0.2952755905511810774, -0.1292274648535930714 ) ) ;
#61635 = CARTESIAN_POINT ( 'NONE',  ( -0.1265901696524986964, -0.4724409448818899238, -2.038713910761154491 ) ) ;
#61636 = CARTESIAN_POINT ( 'NONE',  ( -1.345144356955379816, -0.05778040916215560624, -0.4822834645669293319 ) ) ;
#61637 = CARTESIAN_POINT ( 'NONE',  ( -1.069553805774277722, -0.5511811023622048555, -0.09757992244046775898 ) ) ;
#61638 = CARTESIAN_POINT ( 'NONE',  ( -0.7808398950131225646, -0.08942795157527998196, 0.3641732283464567121 ) ) ;
#61639 = CARTESIAN_POINT ( 'NONE',  ( 0.2087913723976025926, -0.2087913723976025926, 0.1248231986745540617 ) ) ;
#61640 = CARTESIAN_POINT ( 'NONE',  ( 0.1968503937007881344, -0.6692913385826771977, 8.415575281601705876E-17 ) ) ;
#61641 = CARTESIAN_POINT ( 'NONE',  ( 0.6036745406824154392, 0.1283753931104746893, -0.1820866141732285504 ) ) ;
#61642 = CARTESIAN_POINT ( 'NONE',  ( -1.227034120734907585, 0.1771653543307087630, 0.09757992244046791164 ) ) ;
#61643 = CARTESIAN_POINT ( 'NONE',  ( -1.561679790026246017, 0.05413385826771666132, 0.4176697321401328100 ) ) ;
#61644 = CARTESIAN_POINT ( 'NONE',  ( 1.220472440944882386, -0.5511811023622047445, 6.969142054262312111E-17 ) ) ;
#61645 = CARTESIAN_POINT ( 'NONE',  ( 1.351706036745407680, 0.05413385826771666132, 0.4176697321401328100 ) ) ;
#61646 = CARTESIAN_POINT ( 'NONE',  ( -0.3458507752293909498, 0.3458507752293908388, -2.143700787401574104 ) ) ;
#61647 = CARTESIAN_POINT ( 'NONE',  ( 0.2821522309711292364, 0.1771653543307087075, -0.09757992244046823083 ) ) ;
#61648 = CARTESIAN_POINT ( 'NONE',  ( 1.062992125984252745, 0.2952755905511811885, 0.000000000000000000 ) ) ;
#61649 = DIRECTION ( 'NONE',  ( 1.049727191138617093E-16, -0.5150380749100561539, 0.8571673007021108903 ) ) ;
#61650 = CARTESIAN_POINT ( 'NONE',  ( 1.076115485564305141, -0.5023911411419708095, 0.1820866141732285504 ) ) ;
#61651 = ORIENTED_EDGE ( 'NONE', *, *, #24144, .F. ) ;
#61652 = CARTESIAN_POINT ( 'NONE',  ( -1.371391076115484609, -0.6692913385826771977, 0.1292274648535927661 ) ) ;
#61653 = CARTESIAN_POINT ( 'NONE',  ( -0.7086614173228339419, -0.1870078740157479769, 0.4822834645669291653 ) ) ;
#61654 = CARTESIAN_POINT ( 'NONE',  ( 0.01968503937007930540, 0.1660481256975885056, 0.3530559997133364547 ) ) ;
#61655 = CARTESIAN_POINT ( 'NONE',  ( -0.2925321140481930704, -0.2925321140481933480, -0.05905511811023624047 ) ) ;
#61656 = CARTESIAN_POINT ( 'NONE',  ( -9.787531504996566615E-17, 0.3996062992125985480, -2.124015748031496287 ) ) ;
#61657 = CARTESIAN_POINT ( 'NONE',  ( 0.9251968503937015864, -0.5400638737290844871, 0.3530559997133364547 ) ) ;
#61658 = CARTESIAN_POINT ( 'NONE',  ( 1.371391076115485719, -0.5511811023622048555, -0.09757992244046775898 ) ) ;
#61659 = CARTESIAN_POINT ( 'NONE',  ( -0.07874015748031421014, -0.1870078740157479769, 0.4822834645669291653 ) ) ;
#61660 = CARTESIAN_POINT ( 'NONE',  ( 0.7020997375328090762, -0.05778040916215560624, -0.4822834645669293319 ) ) ;
#61661 = CARTESIAN_POINT ( 'NONE',  ( 0.3460692066303959757, -0.1998031496062991907, -1.679790026246719137 ) ) ;
#61662 = CARTESIAN_POINT ( 'NONE',  ( -0.2891555358219908833, -0.2891555358219912164, -1.003937007874015741 ) ) ;
#61663 = CARTESIAN_POINT ( 'NONE',  ( -0.1998031496062991907, -0.3460692066303959757, -2.270341207349081181 ) ) ;
#61664 = CARTESIAN_POINT ( 'NONE',  ( -0.2362204724409451284, 0.4091458600556402425, -0.6430446194225721834 ) ) ;
#61665 = CARTESIAN_POINT ( 'NONE',  ( 0.1958661417322834775, 0.3392501089628018884, -0.1364829396325459021 ) ) ;
#61666 = CARTESIAN_POINT ( 'NONE',  ( -0.2821522309711278487, 0.1771653543307087630, 0.09757992244046791164 ) ) ;
#61667 = CARTESIAN_POINT ( 'NONE',  ( -0.5643044619422565855, 0.05413385826771626580, -0.4176697321401330321 ) ) ;
#61668 = CARTESIAN_POINT ( 'NONE',  ( 0.8398950131233602345, 0.2306618581243847221, -0.2411417322834647770 ) ) ;
#61669 = CARTESIAN_POINT ( 'NONE',  ( -0.3420746716998660508, -0.1974969037888706924, -2.333989501312335957 ) ) ;
#61670 = CARTESIAN_POINT ( 'NONE',  ( -0.5839895013123351797, -0.5511811023622046335, 0.09757992244046803654 ) ) ;
#61671 = CARTESIAN_POINT ( 'NONE',  ( -1.443569553805773564, 0.2306618581243847221, -0.2411417322834647770 ) ) ;
#61672 = CARTESIAN_POINT ( 'NONE',  ( 1.246719160104987623, -0.4281496062992124485, 0.4176697321401328655 ) ) ;
#61673 = CARTESIAN_POINT ( 'NONE',  ( 5.785732909357575061E-17, -0.4724409448818898682, -2.440944881889763884 ) ) ;
#61674 = CARTESIAN_POINT ( 'NONE',  ( 0.2925321140481932369, 0.2925321140481932369, -1.555118110236220597 ) ) ;
#61675 = CARTESIAN_POINT ( 'NONE',  ( 2.787279214012418738, 0.000000000000000000, 0.000000000000000000 ) ) ;
#61676 = EDGE_LOOP ( 'NONE', ( #13327, #12489, #21519, #36933 ) ) ;
#61677 = CARTESIAN_POINT ( 'NONE',  ( 0.9514435695538062676, -0.05778040916215522460, 0.4822834645669289988 ) ) ;
#61678 = CARTESIAN_POINT ( 'NONE',  ( 1.279527559055118724, 0.07958543189024085140, 0.2665933059059887866 ) ) ;
#61680 = CARTESIAN_POINT ( 'NONE',  ( -1.581364829396324945, -0.05778040916215560624, -0.4822834645669293319 ) ) ;
#61679 = CARTESIAN_POINT ( 'NONE',  ( -1.653543307086613234, -0.1870078740157479769, 0.3641732283464567677 ) ) ;
#61681 = CARTESIAN_POINT ( 'NONE',  ( 0.1958661417322834775, 0.3392501089628018884, 0.08595800524934374409 ) ) ;
#61682 = DIRECTION ( 'NONE',  ( 1.000000000000000000, 0.000000000000000000, -0.000000000000000000 ) ) ;
#61683 = CARTESIAN_POINT ( 'NONE',  ( 0.6299212598425204535, -0.1870078740157480879, -0.4822834645669291653 ) ) ;
#61684 = CARTESIAN_POINT ( 'NONE',  ( -1.528871391076114250, 0.2952755905511810774, -0.1292274648535930714 ) ) ;
#61685 = CARTESIAN_POINT ( 'NONE',  ( -0.6102362204724400829, 0.1660481256975885056, 0.3530559997133364547 ) ) ;
#61686 = CARTESIAN_POINT ( 'NONE',  ( -0.6299212598425188991, -0.1870078740157479769, 0.4822834645669291653 ) ) ;
#61687 = CARTESIAN_POINT ( 'NONE',  ( 1.469816272965879911, 0.2306618581243847221, -0.2411417322834647770 ) ) ;
#61688 = CARTESIAN_POINT ( 'NONE',  ( 0.3917322834645670104, -0.1049643490035303411, -0.03871391076115493490 ) ) ;
#61689 = EDGE_CURVE ( 'NONE', #56464, #24808, #74614, .T. ) ;
#61690 = CARTESIAN_POINT ( 'NONE',  ( 0.2821522309711292364, -0.6692913385826771977, 0.1292274648535927661 ) ) ;
#61691 = CARTESIAN_POINT ( 'NONE',  ( 0.3392501089628018884, -0.1958661417322834220, -2.459317585301837195 ) ) ;
#61692 = CARTESIAN_POINT ( 'NONE',  ( -1.607611548556429737, 0.1771653543307087075, -0.09757992244046823083 ) ) ;
#61693 = ORIENTED_EDGE ( 'NONE', *, *, #78869, .F. ) ;
#61694 = CARTESIAN_POINT ( 'NONE',  ( -0.3420746716998661618, 0.1974969037888702206, -2.860892388451444113 ) ) ;
#61695 = ORIENTED_EDGE ( 'NONE', *, *, #53188, .F. ) ;
#61696 = CARTESIAN_POINT ( 'NONE',  ( -0.4709442531824371558, -0.03757601356356778805, -1.220472440944882164 ) ) ;
#61697 = CARTESIAN_POINT ( 'NONE',  ( -1.522309711286088607, 0.2306618581243847221, -0.2411417322834647770 ) ) ;
#61698 = CARTESIAN_POINT ( 'NONE',  ( -0.1998031496062991907, -0.3460692066303959757, -1.010498687664042050 ) ) ;
#61699 = CARTESIAN_POINT ( 'NONE',  ( 0.5615202218219601527, -1.094630224652485432E-15, 0.4281993546915535687 ) ) ;
#61700 = CARTESIAN_POINT ( 'NONE',  ( -0.3492006680983059108, -0.3045572308828553565, -0.01849200668098333403 ) ) ;
#61701 = CARTESIAN_POINT ( 'NONE',  ( 0.4068241469816281097, 0.05413385826771666132, 0.4176697321401328100 ) ) ;
#61702 = CARTESIAN_POINT ( 'NONE',  ( 0.04037479286079570517, -0.3917864676224462328, -2.755905511810075481 ) ) ;
#61703 = CARTESIAN_POINT ( 'NONE',  ( 0.2867679344610365999, 0.2867679344610365999, -0.3799212598425197318 ) ) ;
#61704 = CARTESIAN_POINT ( 'NONE',  ( -0.1640419947506553400, -0.08942795157528024563, -0.3641732283464568787 ) ) ;
#61705 = CARTESIAN_POINT ( 'NONE',  ( -1.233595800524933894, 0.1283753931104748280, 0.1820866141732283561 ) ) ;
#61706 = CARTESIAN_POINT ( 'NONE',  ( -1.594488188976377119, 0.1660481256975883668, -0.3530559997133364547 ) ) ;
#61707 = CARTESIAN_POINT ( 'NONE',  ( 0.3215223097112867578, -0.05778040916215522460, 0.4822834645669289988 ) ) ;
#61708 = CARTESIAN_POINT ( 'NONE',  ( -1.515748031496062076, -0.5400638737290844871, 0.3530559997133364547 ) ) ;
#61709 = CARTESIAN_POINT ( 'NONE',  ( 0.3917322834645670104, 2.398668435337828261E-17, -0.2677165354330708347 ) ) ;
#61710 = ORIENTED_EDGE ( 'NONE', *, *, #73965, .F. ) ;
#61711 = CARTESIAN_POINT ( 'NONE',  ( -1.509186351706035767, -0.4281496062992124485, 0.4176697321401328655 ) ) ;
#61712 = DIRECTION ( 'NONE',  ( -0.000000000000000000, -1.000000000000000000, -0.000000000000000000 ) ) ;
#61713 = CARTESIAN_POINT ( 'NONE',  ( -0.4091458600556405756, 0.2362204724409446288, -1.758530183727034180 ) ) ;
#61714 = CARTESIAN_POINT ( 'NONE',  ( 2.167227123902291108, 1.572090529166659367, 0.4732185887570802829 ) ) ;
#61715 =( BOUNDED_CURVE ( )  B_SPLINE_CURVE ( 2, ( #62365, #35051, #67877, #68691, #36286, #74191, #4703, #22424, #67458, #55217, #28733, #35464, #61551 ),
 .UNSPECIFIED., .F., .F. ) 
 B_SPLINE_CURVE_WITH_KNOTS ( ( 3, 2, 2, 2, 2, 2, 3 ),
 ( 0.7642401855438917258, 0.7651515151515151381, 0.7689393939393939226, 0.7727272727272727071, 0.7765151515151514916, 0.7803030303030302761, 0.7812143599106537994 ),
 .UNSPECIFIED. ) 
 CURVE ( )  GEOMETRIC_REPRESENTATION_ITEM ( )  RATIONAL_B_SPLINE_CURVE ( ( 0.9875488213027523443, 0.9918020599134680371, 1.000000000000000000, 0.9659258262890683122, 1.000000000000000000, 0.9659258262890683122, 1.000000000000000000, 0.9659258262890683122, 1.000000000000000000, 0.9659258262890683122, 1.000000000000000000, 0.9918020599134671489, 0.9875488213027514561 ) ) 
 REPRESENTATION_ITEM ( '' )  );
#61716 = DIRECTION ( 'NONE',  ( 0.000000000000000000, 1.000000000000000000, 0.000000000000000000 ) ) ;
#61717 = CARTESIAN_POINT ( 'NONE',  ( -0.8923884514435688198, -0.6046776061558807314, 0.2411417322834647770 ) ) ;
#61718 = CARTESIAN_POINT ( 'NONE',  ( 1.391076115485564868, 0.2306618581243847221, -0.2411417322834647770 ) ) ;
#61720 = CARTESIAN_POINT ( 'NONE',  ( 1.141392835773559211, 0.000000000000000000, 0.8264322058523028147 ) ) ;
#61719 = CARTESIAN_POINT ( 'NONE',  ( -1.515748031496062076, 0.1660481256975883668, -0.3530559997133364547 ) ) ;
#61721 = AXIS2_PLACEMENT_3D ( 'NONE', #6188, #50796, #44471 ) ;
#61722 = CARTESIAN_POINT ( 'NONE',  ( -1.732283464566928277, -0.1870078740157479769, 0.4822834645669291653 ) ) ;
#61723 = CARTESIAN_POINT ( 'NONE',  ( -0.6561679790026240244, -0.6046776061558807314, 0.2411417322834647770 ) ) ;
#61724 = CARTESIAN_POINT ( 'NONE',  ( 0.3392501089628018329, -0.1958661417322834497, -0.1850200542969010764 ) ) ;
#61725 = CARTESIAN_POINT ( 'NONE',  ( 0.07874015748031558404, -0.1870078740157480601, -0.3641732283464567677 ) ) ;
#61726 = CARTESIAN_POINT ( 'NONE',  ( -0.3917322834645669549, -0.1049643490035306603, -0.6030183727034120755 ) ) ;
#61727 = CARTESIAN_POINT ( 'NONE',  ( -0.06561679790026180015, -0.004921259842519576551, 0.3153832671262227771 ) ) ;
#61728 = CARTESIAN_POINT ( 'NONE',  ( 0.6167979002624678353, -0.3690944881889763329, 0.3153832671262228327 ) ) ;
#61729 = CARTESIAN_POINT ( 'NONE',  ( 0.5774278215223103139, -0.6046776061558809534, -0.2411417322834644161 ) ) ;
#61730 = CARTESIAN_POINT ( 'NONE',  ( -0.1968503937007867743, 0.1771653543307087630, 0.000000000000000000 ) ) ;
#61731 = CARTESIAN_POINT ( 'NONE',  ( 0.3392501089628018329, 0.1958661417322835607, -2.328083989501312345 ) ) ;
#61732 = CARTESIAN_POINT ( 'NONE',  ( -1.587926509186350810, 0.05413385826771626580, -0.4176697321401330321 ) ) ;
#61733 = CARTESIAN_POINT ( 'NONE',  ( -1.102362204724408601, -0.1870078740157480879, -0.4822834645669291653 ) ) ;
#61734 = CARTESIAN_POINT ( 'NONE',  ( 0.1265901696524990294, -0.4724409448818896462, -0.7919947506561679784 ) ) ;
#61735 = CARTESIAN_POINT ( 'NONE',  ( -0.06561679790026180015, -0.4281496062992127816, -0.4176697321401328100 ) ) ;
#61736 = CARTESIAN_POINT ( 'NONE',  ( -0.3871391076115476282, -0.05778040916215522460, 0.4822834645669289988 ) ) ;
#61737 = CARTESIAN_POINT ( 'NONE',  ( 1.561679790026247350, -0.004921259842519870586, -0.3153832671262229437 ) ) ;
#61738 = CARTESIAN_POINT ( 'NONE',  ( -0.01968503937007793844, -0.4536011799217367080, 0.2665933059059888421 ) ) ;
#61739 = CARTESIAN_POINT ( 'NONE',  ( -0.1443569553805768291, 0.05413385826771666132, 0.4176697321401328100 ) ) ;
#61740 = CARTESIAN_POINT ( 'NONE',  ( -0.5314960629921250401, 0.1660481256975885056, 0.3530559997133364547 ) ) ;
#61741 = FACE_OUTER_BOUND ( 'NONE', #25044, .T. ) ;
#61742 = CARTESIAN_POINT ( 'NONE',  ( 0.1265901696524989184, 0.4724409448818898127, -0.3083989501312335846 ) ) ;
#61743 = CARTESIAN_POINT ( 'NONE',  ( 0.1115485564304470323, 0.2952755905511811885, 0.1292274648535926551 ) ) ;
#61744 = ORIENTED_EDGE ( 'NONE', *, *, #1251, .T. ) ;
#61745 = CARTESIAN_POINT ( 'NONE',  ( -0.2925321140481930149, -0.2925321140481933480, -1.868110236220472453 ) ) ;
#61746 = CARTESIAN_POINT ( 'NONE',  ( 1.548556430446194954, -0.6046776061558807314, 0.2411417322834647770 ) ) ;
#61747 = CARTESIAN_POINT ( 'NONE',  ( -0.6167979002624665030, -0.004921259842519576551, 0.3153832671262227771 ) ) ;
#61748 = CARTESIAN_POINT ( 'NONE',  ( -0.7349081364829390672, 0.2306618581243847221, -0.2411417322834647770 ) ) ;
#61749 = CARTESIAN_POINT ( 'NONE',  ( 1.305774278215223960, -0.6692913385826771977, 0.1292274648535927661 ) ) ;
#61750 = CARTESIAN_POINT ( 'NONE',  ( 1.377952755905512472, 0.2952755905511811885, 0.000000000000000000 ) ) ;
#61751 = CARTESIAN_POINT ( 'NONE',  ( -1.587926509186350810, 0.05413385826771626580, -0.4176697321401330321 ) ) ;
#61752 = CARTESIAN_POINT ( 'NONE',  ( -1.062992125984250968, 0.1771653543307087630, 0.000000000000000000 ) ) ;
#61753 = CARTESIAN_POINT ( 'NONE',  ( -0.3996062992125986035, 0.1070741851644051584, -0.4245406824146982228 ) ) ;
#61754 = CARTESIAN_POINT ( 'NONE',  ( 0.2925321140481932369, 0.2925321140481932369, -0.4527559055118109965 ) ) ;
#61755 = CARTESIAN_POINT ( 'NONE',  ( 0.1958661417322834775, 0.3392501089628018884, -2.818260785598111884 ) ) ;
#61756 = CARTESIAN_POINT ( 'NONE',  ( 1.601049868766404982, -0.5023911411419708095, -0.1820866141732282451 ) ) ;
#61757 = CARTESIAN_POINT ( 'NONE',  ( 1.108923884514436242, -0.08942795157527998196, 0.3641732283464567121 ) ) ;
#61758 = CARTESIAN_POINT ( 'NONE',  ( 0.5446194225721792126, -0.05778040916215560624, -0.4822834645669293319 ) ) ;
#61759 = CARTESIAN_POINT ( 'NONE',  ( -1.673228346456691717, 0.1660481256975883668, -0.3530559997133364547 ) ) ;
#61760 = CARTESIAN_POINT ( 'NONE',  ( 0.9711286089238851948, 0.2306618581243848609, 0.2411417322834645549 ) ) ;
#61761 = CARTESIAN_POINT ( 'NONE',  ( 0.1058382717557499880, 0.3949938075777409408, -0.7001312335958006505 ) ) ;
#61762 = CARTESIAN_POINT ( 'NONE',  ( 1.384514435695538559, 0.1771653543307087075, -0.09757992244046823083 ) ) ;
#61763 = CARTESIAN_POINT ( 'NONE',  ( 0.1312335958005257930, 0.2306618581243847221, -0.2411417322834647770 ) ) ;
#61764 = CARTESIAN_POINT ( 'NONE',  ( -0.8792650918635160906, -0.4281496062992124485, 0.4176697321401328655 ) ) ;
#61765 = CARTESIAN_POINT ( 'NONE',  ( 1.207349081364829990, 0.2306618581243848609, 0.2411417322834645549 ) ) ;
#61766 = CARTESIAN_POINT ( 'NONE',  ( 0.3458507752293908943, -0.3458507752293908943, -1.200787401574803015 ) ) ;
#61767 = CARTESIAN_POINT ( 'NONE',  ( -0.2925321140481932369, 0.2925321140481931814, -2.224409448818897683 ) ) ;
#61768 = CARTESIAN_POINT ( 'NONE',  ( 0.3937007874015754361, -0.1870078740157480601, -0.3641732283464567677 ) ) ;
#61769 = ORIENTED_EDGE ( 'NONE', *, *, #36314, .F. ) ;
#61770 = CARTESIAN_POINT ( 'NONE',  ( -0.2867679344610365444, -0.2867679344610367664, -0.6857148538395820836 ) ) ;
#61771 = ORIENTED_EDGE ( 'NONE', *, *, #48287, .T. ) ;
#61772 = CARTESIAN_POINT ( 'NONE',  ( -0.8530183727034112984, -0.4281496062992127816, -0.4176697321401328100 ) ) ;
#61773 = CARTESIAN_POINT ( 'NONE',  ( -0.1312335958005241554, -0.6046776061558809534, -0.2411417322834644161 ) ) ;
#61774 = CARTESIAN_POINT ( 'NONE',  ( -0.2493438320209966919, -0.4281496062992124485, 0.4176697321401328655 ) ) ;
#61775 = CARTESIAN_POINT ( 'NONE',  ( 0.7874015748031503170, -0.1870078740157480879, -0.4822834645669291653 ) ) ;
#61776 = CARTESIAN_POINT ( 'NONE',  ( -1.345144356955379816, -0.3162353388693405765, 0.4822834645669290543 ) ) ;
#61777 = CARTESIAN_POINT ( 'NONE',  ( -0.4986876640419942164, -0.6046776061558807314, 0.2411417322834647770 ) ) ;
#61778 = CARTESIAN_POINT ( 'NONE',  ( 0.7414698162729663755, -0.6692913385826773087, -0.1292274648535924053 ) ) ;
#61779 = CARTESIAN_POINT ( 'NONE',  ( 0.3149606299212603933, -0.1870078740157479769, 0.4822834645669291653 ) ) ;
#61780 = CARTESIAN_POINT ( 'NONE',  ( 0.8005249343832028242, -0.4281496062992127816, -0.4176697321401328100 ) ) ;
#61781 = EDGE_CURVE ( 'NONE', #73035, #27965, #74972, .T. ) ;
#61782 = CARTESIAN_POINT ( 'NONE',  ( 0.3917322834645669549, 0.1049643490035304660, -0.9041994750656167090 ) ) ;
#61783 = CARTESIAN_POINT ( 'NONE',  ( -0.4265091863517051496, -0.5511811023622046335, 0.09757992244046803654 ) ) ;
#61784 = ORIENTED_EDGE ( 'NONE', *, *, #33853, .F. ) ;
#61785 = CARTESIAN_POINT ( 'NONE',  ( -0.1058382717557503211, 0.3949938075777409408, -1.266404199475065440 ) ) ;
#61786 = ORIENTED_EDGE ( 'NONE', *, *, #33602, .F. ) ;
#61787 = CARTESIAN_POINT ( 'NONE',  ( -1.200787401574802349, 0.07958543189024071263, -0.2665933059059888421 ) ) ;
#61788 = CARTESIAN_POINT ( 'NONE',  ( -0.5118110236220466680, 0.2952755905511811885, 0.000000000000000000 ) ) ;
#61789 = DIRECTION ( 'NONE',  ( 0.000000000000000000, 0.000000000000000000, 1.000000000000000000 ) ) ;
#61790 = CARTESIAN_POINT ( 'NONE',  ( -0.7480314960629914633, 0.2952755905511811885, 0.000000000000000000 ) ) ;
#61791 = CARTESIAN_POINT ( 'NONE',  ( -0.6758530183727028406, -0.6692913385826773087, -0.1292274648535924053 ) ) ;
#61792 = CARTESIAN_POINT ( 'NONE',  ( -1.397637795275589623, -0.5400638737290845981, -0.3530559997133363437 ) ) ;
#61793 = CARTESIAN_POINT ( 'NONE',  ( -1.509186351706035767, 0.05413385826771626580, -0.4176697321401330321 ) ) ;
#61794 = CARTESIAN_POINT ( 'NONE',  ( 0.9383202099737538715, -0.08942795157528024563, -0.3641732283464568787 ) ) ;
#61795 = DIRECTION ( 'NONE',  ( 0.000000000000000000, 0.000000000000000000, -1.000000000000000000 ) ) ;
#61796 = DIRECTION ( 'NONE',  ( 1.047444401652940007E-14, 0.000000000000000000, -1.000000000000000000 ) ) ;
#61797 = CARTESIAN_POINT ( 'NONE',  ( 0.2296587926509192634, -0.08942795157528024563, -0.3641732283464568787 ) ) ;
#61798 = CARTESIAN_POINT ( 'NONE',  ( -0.2559055118110227234, -0.5400638737290844871, 0.3530559997133364547 ) ) ;
#61799 = CARTESIAN_POINT ( 'NONE',  ( 0.1246719160104994284, 0.2952755905511810774, -0.1292274648535930714 ) ) ;
#61800 = ORIENTED_EDGE ( 'NONE', *, *, #47629, .T. ) ;
#61801 = CARTESIAN_POINT ( 'NONE',  ( 0.3996062992125986035, 2.446882876249141962E-17, -1.850393700787401619 ) ) ;
#61802 = PLANE ( 'NONE',  #45247 ) ;
#61803 = ORIENTED_EDGE ( 'NONE', *, *, #48095, .F. ) ;
#61804 = CARTESIAN_POINT ( 'NONE',  ( 4.893765752498283308E-17, -0.3996062992125985480, -1.415354330708661346 ) ) ;
#61805 = CARTESIAN_POINT ( 'NONE',  ( 1.614173228346457378, 0.4410134679336836783, -0.1372047244094476148 ) ) ;
#61806 = CARTESIAN_POINT ( 'NONE',  ( -0.7480314960629914633, 0.1771653543307087630, 0.000000000000000000 ) ) ;
#61807 = CARTESIAN_POINT ( 'NONE',  ( -0.8202099737532801971, -0.6692913385826771977, 0.1292274648535927661 ) ) ;
#61808 = CARTESIAN_POINT ( 'NONE',  ( -0.3458507752293906723, -0.3458507752293910609, -0.5314960629921260393 ) ) ;
#61809 = CARTESIAN_POINT ( 'NONE',  ( -0.2101607493002635163, 1.111797321395157967, 3.931418615208038148 ) ) ;
#61810 = CARTESIAN_POINT ( 'NONE',  ( 0.1049643490035304938, -0.3917322834645669549, -2.689632545931758489 ) ) ;
#61811 = CARTESIAN_POINT ( 'NONE',  ( 1.417322834645670104, -0.1870078740157480879, -0.4822834645669291653 ) ) ;
#61812 = CARTESIAN_POINT ( 'NONE',  ( 0.3543307086614179147, 0.2952755905511811885, 0.000000000000000000 ) ) ;
#61813 = CARTESIAN_POINT ( 'NONE',  ( 0.5643044619422579178, 0.05413385826771666132, 0.4176697321401328100 ) ) ;
#61814 = CARTESIAN_POINT ( 'NONE',  ( -0.8333333333333323711, 0.1771653543307087630, 0.09757992244046791164 ) ) ;
#61815 = CARTESIAN_POINT ( 'NONE',  ( -0.1049868766404193215, 0.2306618581243847221, -0.2411417322834647770 ) ) ;
#61816 = CARTESIAN_POINT ( 'NONE',  ( -0.4724409448818895907, -0.1265901696524993070, -2.169947506561679340 ) ) ;
#61817 = CARTESIAN_POINT ( 'NONE',  ( -0.4527559055118102749, 0.1660481256975885056, 0.3530559997133364547 ) ) ;
#61818 = CARTESIAN_POINT ( 'NONE',  ( 4.837279021331061486E-17, -0.3949938075777409963, -1.730314960629921295 ) ) ;
#61819 = CARTESIAN_POINT ( 'NONE',  ( 1.456692913385827515, 0.1771653543307087630, 0.000000000000000000 ) ) ;
#61820 = CARTESIAN_POINT ( 'NONE',  ( -0.1312335958005241554, 0.1283753931104748280, 0.1820866141732283561 ) ) ;
#61821 = CARTESIAN_POINT ( 'NONE',  ( 1.069553805774278832, 0.1771653543307087075, -0.09757992244046823083 ) ) ;
#61823 = EDGE_CURVE ( 'NONE', #59927, #42372, #41867, .T. ) ;
#61822 = CARTESIAN_POINT ( 'NONE',  ( -1.240157480314959759, 0.1660481256975885056, 0.3530559997133364547 ) ) ;
#61824 = CARTESIAN_POINT ( 'NONE',  ( -0.9908136482939626788, 0.1771653543307087630, 0.09757992244046791164 ) ) ;
#61825 = CARTESIAN_POINT ( 'NONE',  ( -2.795275590551184131, 1.023622047244095556, -2.654250759839014936E-16 ) ) ;
#61826 = CARTESIAN_POINT ( 'NONE',  ( -1.181102362204723644, -0.1870078740157480879, -0.4822834645669291653 ) ) ;
#61827 = CARTESIAN_POINT ( 'NONE',  ( -0.2559055118110227234, -0.5400638737290844871, 0.3530559997133364547 ) ) ;
#61828 = CARTESIAN_POINT ( 'NONE',  ( 0.3937007874015754361, -0.1870078740157479769, 0.4822834645669291653 ) ) ;
#61829 = CARTESIAN_POINT ( 'NONE',  ( 4.797336870675655290E-17, -0.3917322834645669549, -2.363497744585615123 ) ) ;
#61830 = CARTESIAN_POINT ( 'NONE',  ( -1.877461585981332171, 1.092324130688954176, 0.1650676745532031753 ) ) ;
#61831 = CARTESIAN_POINT ( 'NONE',  ( 0.3543307086614181922, -0.5511811023622047445, 6.969142054262312111E-17 ) ) ;
#61832 = CARTESIAN_POINT ( 'NONE',  ( -1.568241469816272105, -0.08942795157527998196, 0.3641732283464567121 ) ) ;
#61833 = CARTESIAN_POINT ( 'NONE',  ( 0.6889763779527566800, -0.5400638737290844871, 0.3530559997133364547 ) ) ;
#61834 = CARTESIAN_POINT ( 'NONE',  ( -1.607611548556429737, -0.5511811023622046335, 0.09757992244046803654 ) ) ;
#61835 = CARTESIAN_POINT ( 'NONE',  ( 1.233595800524935227, -0.5023911411419708095, 0.1820866141732285504 ) ) ;
#61836 = CARTESIAN_POINT ( 'NONE',  ( -0.8464566929133852113, -0.5400638737290845981, -0.3530559997133363437 ) ) ;
#61837 = CARTESIAN_POINT ( 'NONE',  ( -0.09186351706036663400, -0.3690944881889763329, 0.3153832671262228327 ) ) ;
#61838 = DIRECTION ( 'NONE',  ( 1.000000000000000000, 3.083952846180989294E-16, 0.000000000000000000 ) ) ;
#61839 = CARTESIAN_POINT ( 'NONE',  ( 0.6758530183727039509, 0.1771653543307087075, -0.09757992244046823083 ) ) ;
#61840 = CARTESIAN_POINT ( 'NONE',  ( -0.07217847769028787330, -0.05778040916215522460, 0.4822834645669289988 ) ) ;
#61841 = EDGE_CURVE ( 'NONE', #62412, #50709, #11771, .T. ) ;
#61842 = CARTESIAN_POINT ( 'NONE',  ( 0.1998031496062992463, 0.3460692066303959202, -0.5360892388451443669 ) ) ;
#61843 = CARTESIAN_POINT ( 'NONE',  ( -0.3917322834645670104, -7.196005306013484475E-17, -1.856299212598425230 ) ) ;
#61844 = CARTESIAN_POINT ( 'NONE',  ( 0.7152230971128614723, -0.2845877964562161244, -0.3641732283464567121 ) ) ;
#61845 = CARTESIAN_POINT ( 'NONE',  ( 0.2427821522309719648, -0.05778040916215522460, 0.4822834645669289988 ) ) ;
#61846 = CARTESIAN_POINT ( 'NONE',  ( -0.8136482939632537770, 0.2306618581243847221, -0.2411417322834647770 ) ) ;
#61847 = CARTESIAN_POINT ( 'NONE',  ( -0.4790026246719152336, -0.08942795157528024563, -0.3641732283464568787 ) ) ;
#61848 = DIRECTION ( 'NONE',  ( 0.8660254037844362651, 0.000000000000000000, 0.5000000000000041078 ) ) ;
#61849 = CARTESIAN_POINT ( 'NONE',  ( -0.4002624671916004129, -0.2845877964562159024, 0.3641732283464567677 ) ) ;
#61850 = CARTESIAN_POINT ( 'NONE',  ( 0.4396325459317593221, 0.2952755905511810774, -0.1292274648535930714 ) ) ;
#61851 = CARTESIAN_POINT ( 'NONE',  ( -1.036745406824146176, -0.004921259842519870586, -0.3153832671262229437 ) ) ;
#61852 = CARTESIAN_POINT ( 'NONE',  ( 0.1070741851644054776, -0.3996062992125984925, -1.264435695538057569 ) ) ;
#61853 = CARTESIAN_POINT ( 'NONE',  ( 1.541994750656168645, -0.6692913385826771977, 0.1292274648535927661 ) ) ;
#61854 = CARTESIAN_POINT ( 'NONE',  ( -1.313877454013331780, 0.2755905511811023723, 0.7983292792091805090 ) ) ;
#61855 = VERTEX_POINT ( 'NONE', #47586 ) ;
#61856 = CARTESIAN_POINT ( 'NONE',  ( -1.332020997375327642, -0.2845877964562161244, -0.3641732283464567121 ) ) ;
#61857 = CARTESIAN_POINT ( 'NONE',  ( -0.6561679790026240244, -0.6046776061558807314, 0.2411417322834647770 ) ) ;
#61858 = CARTESIAN_POINT ( 'NONE',  ( -1.279527559055116948, 0.1660481256975883668, -0.3530559997133364547 ) ) ;
#61859 = CARTESIAN_POINT ( 'NONE',  ( -0.2867679344610364334, -0.2867679344610367109, -1.718503937007874072 ) ) ;
#61860 = DIRECTION ( 'NONE',  ( 0.000000000000000000, -0.000000000000000000, -1.000000000000000000 ) ) ;
#61861 = CARTESIAN_POINT ( 'NONE',  ( 1.548556430446194954, 0.2306618581243847221, -0.2411417322834647770 ) ) ;
#61862 = CARTESIAN_POINT ( 'NONE',  ( 0.3083989501312343062, -0.05778040916215560624, -0.4822834645669293319 ) ) ;
#61863 = CARTESIAN_POINT ( 'NONE',  ( -0.4724409448818898682, -8.678599364036362592E-17, -0.5118110236220472231 ) ) ;
#61864 = CARTESIAN_POINT ( 'NONE',  ( 0.3996062992125985480, 2.446882876249141654E-17, -2.242125984251968518 ) ) ;
#61865 = CARTESIAN_POINT ( 'NONE',  ( 1.476377952755906220, 0.07958543189024071263, -0.2665933059059888421 ) ) ;
#61866 = CARTESIAN_POINT ( 'NONE',  ( -0.2925321140481932924, 0.2925321140481931814, -0.8070866141732284671 ) ) ;
#61867 = ORIENTED_EDGE ( 'NONE', *, *, #37700, .T. ) ;
#61868 = CARTESIAN_POINT ( 'NONE',  ( -0.8792650918635160906, -0.3690944881889763329, 0.3153832671262228327 ) ) ;
#61869 = CARTESIAN_POINT ( 'NONE',  ( -0.1049643490035302024, -0.3917322834645671215, -2.741469816272964710 ) ) ;
#61870 = EDGE_LOOP ( 'NONE', ( #25019, #77662, #49425, #52537, #38669, #63447, #15032, #36218, #48497, #57318, #44479, #42638, #20272, #30639 ) ) ;
#61871 = CARTESIAN_POINT ( 'NONE',  ( 0.4724409448818904789, -0.1870078740157479769, 0.4822834645669291653 ) ) ;
#61872 = CARTESIAN_POINT ( 'NONE',  ( -0.5577427821522301654, -0.05778040916215560624, -0.4822834645669293319 ) ) ;
#61873 = CARTESIAN_POINT ( 'NONE',  ( -0.9514435695538050464, -0.05778040916215560624, -0.4822834645669293319 ) ) ;
#61874 = CARTESIAN_POINT ( 'NONE',  ( 0.8923884514435703741, 0.2306618581243848609, 0.2411417322834645549 ) ) ;
#61875 = CARTESIAN_POINT ( 'NONE',  ( -1.227034120734907141, -0.5511811023622048555, -0.09757992244046775898 ) ) ;
#61876 = DIRECTION ( 'NONE',  ( 0.000000000000000000, 0.000000000000000000, -1.000000000000000000 ) ) ;
#61877 = CARTESIAN_POINT ( 'NONE',  ( 0.2427821522309719648, -0.05778040916215522460, 0.4822834645669289988 ) ) ;
#61878 = CARTESIAN_POINT ( 'NONE',  ( -0.9711286089238838626, 0.2306618581243847221, -0.2411417322834647770 ) ) ;
#61879 = CARTESIAN_POINT ( 'NONE',  ( 0.3392501089628018329, -0.1958661417322834497, -2.074783833824459744 ) ) ;
#61880 = CARTESIAN_POINT ( 'NONE',  ( 1.548556430446194954, -0.6046776061558807314, 0.2411417322834647770 ) ) ;
#61881 = CARTESIAN_POINT ( 'NONE',  ( -1.313877454013331780, 1.062992125984252079, 0.7983292792091805090 ) ) ;
#61882 = CARTESIAN_POINT ( 'NONE',  ( -0.1049643490035302024, -0.3917322834645671215, -2.833989501312335957 ) ) ;
#61883 = CARTESIAN_POINT ( 'NONE',  ( 0.9383202099737538715, -0.08942795157528024563, -0.3641732283464568787 ) ) ;
#61884 = ORIENTED_EDGE ( 'NONE', *, *, #74342, .T. ) ;
#61885 = CARTESIAN_POINT ( 'NONE',  ( 0.1974969037888704704, 0.3420746716998660508, -0.1443569553805774675 ) ) ;
#61886 = CARTESIAN_POINT ( 'NONE',  ( -0.3805774278215216522, 0.05413385826771666132, 0.4176697321401328100 ) ) ;
#61887 = ORIENTED_EDGE ( 'NONE', *, *, #33217, .F. ) ;
#61888 = CARTESIAN_POINT ( 'NONE',  ( 0.5052493438320215802, 0.1771653543307087630, 0.09757992244046791164 ) ) ;
#61889 = CARTESIAN_POINT ( 'NONE',  ( -1.476377952755905110, -0.5400638737290845981, -0.3530559997133363437 ) ) ;
#61890 = CARTESIAN_POINT ( 'NONE',  ( 0.5249343832021003964, 0.2306618581243847221, -0.2411417322834647770 ) ) ;
#61891 = CARTESIAN_POINT ( 'NONE',  ( 0.5249343832021003964, 0.2306618581243847221, -0.2411417322834647770 ) ) ;
#61892 = CARTESIAN_POINT ( 'NONE',  ( -0.006561679790025524116, -0.3162353388693405765, 0.4822834645669290543 ) ) ;
#61893 = CARTESIAN_POINT ( 'NONE',  ( 0.2867679344610366554, -0.2867679344610365999, -1.197525877461629307 ) ) ;
#61894 = CARTESIAN_POINT ( 'NONE',  ( -0.6627296587926501115, 0.2952755905511810774, -0.1292274648535930714 ) ) ;
#61895 = CARTESIAN_POINT ( 'NONE',  ( -9.594673741351313045E-17, 0.3917322834645670104, -2.131889763779527769 ) ) ;
#61896 = CARTESIAN_POINT ( 'NONE',  ( 1.482939632545932307, -0.004921259842519870586, -0.3153832671262229437 ) ) ;
#61897 = CARTESIAN_POINT ( 'NONE',  ( -1.102362204724408601, -0.1870078740157480879, -0.4822834645669291653 ) ) ;
#61898 = CARTESIAN_POINT ( 'NONE',  ( 1.266404199475066328, -0.3162353388693409650, -0.4822834645669289433 ) ) ;
#61899 = CARTESIAN_POINT ( 'NONE',  ( 1.240157480314961314, 0.1660481256975883668, -0.3530559997133364547 ) ) ;
#61900 = CIRCLE ( 'NONE', #68634, 0.4724409448818898682 ) ;
#61901 = CARTESIAN_POINT ( 'NONE',  ( 4.893765752498283924E-17, -0.3996062992125986035, -0.2362204724409449341 ) ) ;
#61902 = CARTESIAN_POINT ( 'NONE',  ( -0.8136482939632537770, -0.6046776061558807314, 0.2411417322834647770 ) ) ;
#61903 = CARTESIAN_POINT ( 'NONE',  ( 0.3996062992125985480, 2.446882876249141654E-17, 0.1200787401574803098 ) ) ;
#61904 = CARTESIAN_POINT ( 'NONE',  ( 0.1312335958005255154, -0.6046776061558807314, 0.2411417322834647770 ) ) ;
#61905 = CARTESIAN_POINT ( 'NONE',  ( -0.3996062992125986035, -0.1070741851644056997, -2.093175853018372834 ) ) ;
#61906 = CARTESIAN_POINT ( 'NONE',  ( -0.6758530183727028406, 0.2952755905511811885, 0.1292274648535926551 ) ) ;
#61907 = CARTESIAN_POINT ( 'NONE',  ( 1.614173228346457378, -0.6692913385826771977, 8.415575281601705876E-17 ) ) ;
#61908 = CARTESIAN_POINT ( 'NONE',  ( 0.6364829396325465405, -0.2845877964562161244, -0.3641732283464567121 ) ) ;
#61909 = CARTESIAN_POINT ( 'NONE',  ( 1.167979002624672580, 0.05413385826771626580, -0.4176697321401330321 ) ) ;
#61910 = CARTESIAN_POINT ( 'NONE',  ( 0.2362204724409451007, -0.4091458600556402980, -1.113517060367454015 ) ) ;
#61911 = CARTESIAN_POINT ( 'NONE',  ( 0.9448818897637802916, -0.1870078740157480601, -0.3641732283464567677 ) ) ;
#61912 = CARTESIAN_POINT ( 'NONE',  ( 0.8727034120734912248, -0.3162353388693409650, -0.4822834645669289433 ) ) ;
#61913 = CARTESIAN_POINT ( 'NONE',  ( 0.3420746716998660508, 0.1974969037888705814, -0.6804461942257220564 ) ) ;
#61914 = CARTESIAN_POINT ( 'NONE',  ( -0.7086614173228339419, -0.1870078740157480879, -0.4822834645669291653 ) ) ;
#61915 = CARTESIAN_POINT ( 'NONE',  ( -3.937007874015748143, 2.755905511811024056, 0.5314960629921260393 ) ) ;
#61916 = CARTESIAN_POINT ( 'NONE',  ( 1.358267716535433323, -0.4536011799217368745, -0.2665933059059886201 ) ) ;
#61917 = CARTESIAN_POINT ( 'NONE',  ( -0.4068241469816267775, 0.05413385826771626580, -0.4176697321401330321 ) ) ;
#61918 = CARTESIAN_POINT ( 'NONE',  ( 0.2296587926509192634, -0.05778040916215560624, -0.4822834645669293319 ) ) ;
#61919 = DIRECTION ( 'NONE',  ( 1.000000000000000000, 0.000000000000000000, 0.000000000000000000 ) ) ;
#61921 = EDGE_CURVE ( 'NONE', #5694, #57471, #73036, .T. ) ;
#61920 = CARTESIAN_POINT ( 'NONE',  ( 0.2624671916010504757, -0.6046776061558809534, -0.2411417322834644161 ) ) ;
#61922 = CARTESIAN_POINT ( 'NONE',  ( -0.03937007874015669567, 0.1771653543307087630, 0.000000000000000000 ) ) ;
#61923 = CARTESIAN_POINT ( 'NONE',  ( -2.847313777101077026, 1.091897865355362152, 0.1662078246829769568 ) ) ;
#61924 = CARTESIAN_POINT ( 'NONE',  ( 0.09842519685039434474, 0.07958543189024085140, 0.2665933059059887866 ) ) ;
#61925 = CARTESIAN_POINT ( 'NONE',  ( 0.9383202099737536495, -0.2845877964562159024, 0.3641732283464567677 ) ) ;
#61926 = FACE_OUTER_BOUND ( 'NONE', #73904, .T. ) ;
#61927 = CARTESIAN_POINT ( 'NONE',  ( 0.3996062992125985480, 2.446882876249141654E-17, -1.612204724409448842 ) ) ;
#61928 = CARTESIAN_POINT ( 'NONE',  ( 0.4265091863517067594, 0.2952755905511811885, 0.1292274648535926551 ) ) ;
#61929 = CARTESIAN_POINT ( 'NONE',  ( 4.797336870675656522E-17, -0.3917322834645670104, -1.645669291338582640 ) ) ;
#61930 = CARTESIAN_POINT ( 'NONE',  ( 1.528871391076116026, 0.1771653543307087630, 0.09757992244046791164 ) ) ;
#61931 = CARTESIAN_POINT ( 'NONE',  ( -0.2432155562301253904, -0.3078094465263045976, 3.457013956890525812E-17 ) ) ;
#61932 = CARTESIAN_POINT ( 'NONE',  ( -0.2690288713910754526, 0.1771653543307087075, -0.09757992244046823083 ) ) ;
#61933 = CARTESIAN_POINT ( 'NONE',  ( 0.1902887139107617975, -0.6692913385826773087, -0.1292274648535924053 ) ) ;
#61934 = CARTESIAN_POINT ( 'NONE',  ( 0.9383202099737538715, -0.08942795157528024563, -0.3641732283464568787 ) ) ;
#61935 = CARTESIAN_POINT ( 'NONE',  ( -1.194225721784776262, -0.004921259842519870586, -0.3153832671262229437 ) ) ;
#61936 = CARTESIAN_POINT ( 'NONE',  ( -1.633858267716534529, -0.5400638737290845981, -0.3530559997133363437 ) ) ;
#61937 = CARTESIAN_POINT ( 'NONE',  ( 0.1377952755905518800, 0.1660481256975883668, -0.3530559997133364547 ) ) ;
#61938 = CARTESIAN_POINT ( 'NONE',  ( 1.089238845144357759, 0.05413385826771626580, -0.4176697321401330321 ) ) ;
#61939 =( BOUNDED_CURVE ( )  B_SPLINE_CURVE ( 2, ( #48553, #3123, #67105, #67515, #42652, #3953, #62019 ),
 .UNSPECIFIED., .F., .F. ) 
 B_SPLINE_CURVE_WITH_KNOTS ( ( 3, 2, 2, 3 ),
 ( 0.1363636363636364923, 0.1401515151515152213, 0.1439393939393939503, 0.1441485521566764350 ),
 .UNSPECIFIED. ) 
 CURVE ( )  GEOMETRIC_REPRESENTATION_ITEM ( )  RATIONAL_B_SPLINE_CURVE ( ( 0.9999999999999987788, 0.9659258262890695335, 1.000000000000000000, 0.9659258262890683122, 1.000000000000000000, 0.9981185001348095165, 0.9964447847208426357 ) ) 
 REPRESENTATION_ITEM ( '' )  );
#61940 = EDGE_CURVE ( 'NONE', #55671, #73693, #34142, .T. ) ;
#61941 = DIRECTION ( 'NONE',  ( 1.000000000000000000, 0.000000000000000000, 0.000000000000000000 ) ) ;
#61942 = CARTESIAN_POINT ( 'NONE',  ( 0.07217847769028949700, -0.05778040916215560624, -0.4822834645669293319 ) ) ;
#61943 = CARTESIAN_POINT ( 'NONE',  ( 1.220472440944882608, 0.2952755905511811885, 0.000000000000000000 ) ) ;
#61944 = CARTESIAN_POINT ( 'NONE',  ( 0.8923884514435703741, 0.2306618581243848609, 0.2411417322834645549 ) ) ;
#61945 = EDGE_CURVE ( 'NONE', #15221, #54535, #11679, .T. ) ;
#61946 = CARTESIAN_POINT ( 'NONE',  ( -0.5314960629921171575, 2.729661165926052124, -2.530077622625179767 ) ) ;
#61947 = CARTESIAN_POINT ( 'NONE',  ( 0.7217847769028878924, -0.004921259842519576551, 0.3153832671262227771 ) ) ;
#61948 = CARTESIAN_POINT ( 'NONE',  ( 1.548556430446194954, 0.2306618581243847221, -0.2411417322834647770 ) ) ;
#61949 = CARTESIAN_POINT ( 'NONE',  ( 0.2099737532808405305, 0.1283753931104746893, -0.1820866141732285504 ) ) ;
#61950 = CARTESIAN_POINT ( 'NONE',  ( -0.2427821522309703550, -0.3162353388693405765, 0.4822834645669290543 ) ) ;
#61951 = CARTESIAN_POINT ( 'NONE',  ( 0.5183727034120741983, 0.2952755905511810774, -0.1292274648535930714 ) ) ;
#61952 = CARTESIAN_POINT ( 'NONE',  ( -0.5708661417322825615, -0.5400638737290844871, 0.3530559997133364547 ) ) ;
#61953 = CARTESIAN_POINT ( 'NONE',  ( -0.3392501089628017219, -0.1958661417322836995, -1.938995693734595127 ) ) ;
#61954 = CARTESIAN_POINT ( 'NONE',  ( -0.2362204724409442680, -0.1870078740157480601, -0.3641732283464567677 ) ) ;
#61955 = AXIS2_PLACEMENT_3D ( 'NONE', #78166, #13350, #71846 ) ;
#61956 = CARTESIAN_POINT ( 'NONE',  ( 0.6889763779527563470, 0.1660481256975883668, -0.3530559997133364547 ) ) ;
#61957 = CARTESIAN_POINT ( 'NONE',  ( 0.8267716535433078384, -0.5511811023622047445, 6.969142054262312111E-17 ) ) ;
#61958 = CARTESIAN_POINT ( 'NONE',  ( -1.704584837829988819, 1.183873793530418661, 0.3164211518737862217 ) ) ;
#61960 = CARTESIAN_POINT ( 'NONE',  ( 0.3460692066303959202, 0.1998031496062993295, -1.076115485564304475 ) ) ;
#61959 = CARTESIAN_POINT ( 'NONE',  ( 0.4330708661417329575, 1.805669738366188382, 0.000000000000000000 ) ) ;
#61961 = CARTESIAN_POINT ( 'NONE',  ( 2.170146923806633765, 1.554943921348592273, -0.4744094488188969616 ) ) ;
#61962 = CARTESIAN_POINT ( 'NONE',  ( -1.404199475065615932, -0.4281496062992127816, -0.4176697321401328100 ) ) ;
#61963 = CARTESIAN_POINT ( 'NONE',  ( -0.4002624671916004129, -0.05778040916215560624, -0.4822834645669293319 ) ) ;
#61964 = EDGE_CURVE ( 'NONE', #41007, #32917, #68999, .T. ) ;
#61965 = CARTESIAN_POINT ( 'NONE',  ( 0.4724409448818896462, 0.1265901696524990294, 0.03280839895013123314 ) ) ;
#61966 = CARTESIAN_POINT ( 'NONE',  ( -0.1058382717557503211, 0.3949938075777409408, -2.683727034120735766 ) ) ;
#61967 = ORIENTED_EDGE ( 'NONE', *, *, #55092, .F. ) ;
#61968 = CARTESIAN_POINT ( 'NONE',  ( 0.2493438320209980519, -0.004921259842519576551, 0.3153832671262227771 ) ) ;
#61969 = CARTESIAN_POINT ( 'NONE',  ( -0.2867679344610365999, 0.2867679344610364889, -1.586614173228346747 ) ) ;
#61970 = CARTESIAN_POINT ( 'NONE',  ( 0.9514435695538062676, -0.05778040916215522460, 0.4822834645669289988 ) ) ;
#61971 = CARTESIAN_POINT ( 'NONE',  ( 0.1265901696524990294, -0.4724409448818896462, -2.604986876640420057 ) ) ;
#61972 = CARTESIAN_POINT ( 'NONE',  ( 0.4091458600556403535, 0.2362204724409449896, -0.8379265091863516979 ) ) ;
#61973 = EDGE_CURVE ( 'NONE', #68390, #7361, #81702, .T. ) ;
#61975 = AXIS2_PLACEMENT_3D ( 'NONE', #18082, #31517, #82466 ) ;
#61974 = CARTESIAN_POINT ( 'NONE',  ( -1.607611548556429737, -0.5511811023622046335, 0.09757992244046803654 ) ) ;
#61976 = CARTESIAN_POINT ( 'NONE',  ( -0.1540510737581029521, 1.087609530016003356, 1.111807356369383104 ) ) ;
#61977 = CARTESIAN_POINT ( 'NONE',  ( 1.233595800524935227, -0.5023911411419708095, 0.1820866141732285504 ) ) ;
#61978 = CARTESIAN_POINT ( 'NONE',  ( 0.6167979002624679463, 0.05413385826771626580, -0.4176697321401330321 ) ) ;
#61979 = CARTESIAN_POINT ( 'NONE',  ( -0.3392501089628018329, -0.1958661417322836440, -0.1325266159766911034 ) ) ;
#61980 = CARTESIAN_POINT ( 'NONE',  ( -0.2034120734908128059, 0.2952755905511811885, 0.1292274648535926551 ) ) ;
#61981 = CARTESIAN_POINT ( 'NONE',  ( -1.082677165354329896, 0.07958543189024085140, 0.2665933059059887866 ) ) ;
#61982 = CARTESIAN_POINT ( 'NONE',  ( 0.2887139107611556010, -0.6046776061558807314, 0.2411417322834647770 ) ) ;
#61983 = CARTESIAN_POINT ( 'NONE',  ( 0.09842519685039434474, -0.5400638737290845981, -0.3530559997133363437 ) ) ;
#61984 = FACE_OUTER_BOUND ( 'NONE', #71187, .T. ) ;
#61985 = CARTESIAN_POINT ( 'NONE',  ( 0.3460692066303959202, 0.1998031496062993295, -2.808398950131233640 ) ) ;
#61986 = CARTESIAN_POINT ( 'NONE',  ( 0.2867679344610366554, 0.2867679344610366554, -1.551856586123046888 ) ) ;
#61987 = CARTESIAN_POINT ( 'NONE',  ( 0.6430446194225729606, -0.4281496062992127816, -0.4176697321401328100 ) ) ;
#61988 = CARTESIAN_POINT ( 'NONE',  ( -0.2230971128608915943, -0.4281496062992127816, -0.4176697321401328100 ) ) ;
#61989 = CARTESIAN_POINT ( 'NONE',  ( -1.607611548556429737, 0.2952755905511810774, -0.1292274648535930714 ) ) ;
#61990 = CARTESIAN_POINT ( 'NONE',  ( 1.253280839895013710, -0.3162353388693405765, 0.4822834645669290543 ) ) ;
#61991 = CARTESIAN_POINT ( 'NONE',  ( 0.3937007874015754361, -0.1870078740157479769, 0.4822834645669291653 ) ) ;
#61992 = CARTESIAN_POINT ( 'NONE',  ( 0.1049643490035303689, 0.3917322834645670104, -1.180446194225722056 ) ) ;
#61993 = CARTESIAN_POINT ( 'NONE',  ( -0.3346456692913377662, -0.5400638737290844871, 0.3530559997133364547 ) ) ;
#61994 = CARTESIAN_POINT ( 'NONE',  ( 0.09842519685039434474, 0.1660481256975885056, 0.3530559997133364547 ) ) ;
#61995 = CARTESIAN_POINT ( 'NONE',  ( -0.3215223097112853146, -0.05778040916215560624, -0.4822834645669293319 ) ) ;
#61996 = CARTESIAN_POINT ( 'NONE',  ( 0.4986876640419954376, -0.5023911411419708095, -0.1820866141732282451 ) ) ;
#61997 = CARTESIAN_POINT ( 'NONE',  ( -1.574803149606298636, -0.1870078740157479769, 0.4822834645669291653 ) ) ;
#61998 = CARTESIAN_POINT ( 'NONE',  ( -0.4567115769095945188, 1.408171547189569939, -2.593413219429640204 ) ) ;
#61999 = CARTESIAN_POINT ( 'NONE',  ( 0.5380577427821529035, 0.05413385826771626580, -0.4176697321401330321 ) ) ;
#62000 = LINE ( 'NONE', #73400, #953 ) ;
#62001 = ADVANCED_FACE ( 'NONE', ( #53062 ), #2576, .T. ) ;
#62002 = CARTESIAN_POINT ( 'NONE',  ( 1.496062992125984703, -0.1870078740157480879, -0.4822834645669291653 ) ) ;
#62003 = CARTESIAN_POINT ( 'NONE',  ( -0.3392501089628019995, 0.1958661417322832277, -2.223097112860892288 ) ) ;
#62004 = ORIENTED_EDGE ( 'NONE', *, *, #78455, .T. ) ;
#62005 = ORIENTED_EDGE ( 'NONE', *, *, #10455, .T. ) ;
#62006 = CARTESIAN_POINT ( 'NONE',  ( 0.5774278215223104249, 0.2306618581243848609, 0.2411417322834645549 ) ) ;
#62007 = CARTESIAN_POINT ( 'NONE',  ( 0.09186351706036799403, -0.3690944881889765550, -0.3153832671262227771 ) ) ;
#62008 = LINE ( 'NONE', #67504, #14252 ) ;
#62009 = CARTESIAN_POINT ( 'NONE',  ( 0.1958661417322834775, 0.3392501089628018884, -0.7014435695538058235 ) ) ;
#62010 = CARTESIAN_POINT ( 'NONE',  ( 0.09156050430091122738, 0.3808816823641256732, -2.755905511811024056 ) ) ;
#62011 = ADVANCED_FACE ( 'NONE', ( #10135 ), #74527, .F. ) ;
#62012 = CARTESIAN_POINT ( 'NONE',  ( -0.2925321140481930149, -0.2925321140481933480, -2.498031496062992574 ) ) ;
#62013 = CARTESIAN_POINT ( 'NONE',  ( 0.5643044619422579178, -0.4281496062992127816, -0.4176697321401328100 ) ) ;
#62014 = CARTESIAN_POINT ( 'NONE',  ( -0.9120734908136475250, -0.6692913385826773087, -0.1292274648535924053 ) ) ;
#62015 = CARTESIAN_POINT ( 'NONE',  ( -0.8792650918635160906, 0.05413385826771626580, -0.4176697321401330321 ) ) ;
#62016 = CARTESIAN_POINT ( 'NONE',  ( 0.8398950131233602345, 0.2306618581243847221, -0.2411417322834647770 ) ) ;
#62017 = AXIS2_PLACEMENT_3D ( 'NONE', #68744, #18636, #75483 ) ;
#62018 = CARTESIAN_POINT ( 'NONE',  ( 1.181102362204724976, -0.1870078740157480879, -0.4822834645669291653 ) ) ;
#62019 = CARTESIAN_POINT ( 'NONE',  ( 1.193521905106662784, 3.421639014772782816E-16, 0.3464511005275203726 ) ) ;
#62020 = ITEM_DEFINED_TRANSFORMATION ( 'NONE', 'NONE', #69201,  #22098 ) ;
#62021 = CARTESIAN_POINT ( 'NONE',  ( 1.141732283464567788, -0.5511811023622047445, 6.969142054262312111E-17 ) ) ;
#62022 = CARTESIAN_POINT ( 'NONE',  ( -0.7414698162729651543, -0.6692913385826771977, 0.1292274648535927661 ) ) ;
#62023 = CARTESIAN_POINT ( 'NONE',  ( -1.646981627296586703, -0.08942795157527998196, 0.3641732283464567121 ) ) ;
#62024 = ADVANCED_FACE ( 'NONE', ( #55134 ), #30294, .F. ) ;
#62025 = CARTESIAN_POINT ( 'NONE',  ( 1.595398199321655497, 0.7585570207896586981, 0.1559797534342493297 ) ) ;
#62026 = CARTESIAN_POINT ( 'NONE',  ( -0.3543307086614165824, 0.2952755905511811885, 0.000000000000000000 ) ) ;
#62028 = CARTESIAN_POINT ( 'NONE',  ( -0.7213048234621840527, 1.923042554663772385, 0.5309055118110236338 ) ) ;
#62027 = CARTESIAN_POINT ( 'NONE',  ( 1.194225721784777594, 0.05413385826771666132, 0.4176697321401328100 ) ) ;
#62029 = CARTESIAN_POINT ( 'NONE',  ( -0.9776902887139098386, -0.5511811023622046335, 0.09757992244046803654 ) ) ;
#62030 = CARTESIAN_POINT ( 'NONE',  ( 0.2624671916010504757, 0.2306618581243848609, 0.2411417322834645549 ) ) ;
#62031 = CARTESIAN_POINT ( 'NONE',  ( 0.7414698162729663755, -0.5511811023622048555, -0.09757992244046775898 ) ) ;
#62032 = CARTESIAN_POINT ( 'NONE',  ( -0.1049643490035301746, -0.3917322834645670659, -1.727014804953068916 ) ) ;
#62033 = CARTESIAN_POINT ( 'NONE',  ( -1.062992125984250968, 0.1771653543307087630, 0.000000000000000000 ) ) ;
#62034 = CARTESIAN_POINT ( 'NONE',  ( 1.272965879265092637, -0.4281496062992127816, -0.4176697321401328100 ) ) ;
#62035 = CARTESIAN_POINT ( 'NONE',  ( 0.1890927523439494273, 1.924543803844427581, 0.2498735643778251525 ) ) ;
#62036 = CARTESIAN_POINT ( 'NONE',  ( -0.07217847769028813698, -0.2845877964562161244, -0.3641732283464567121 ) ) ;
#62037 = CARTESIAN_POINT ( 'NONE',  ( -0.1443569553805768291, 0.05413385826771666132, 0.4176697321401328100 ) ) ;
#62038 = CARTESIAN_POINT ( 'NONE',  ( -1.187664041994749731, -0.2845877964562159024, 0.3641732283464567677 ) ) ;
#62039 = CARTESIAN_POINT ( 'NONE',  ( -0.7283464566929126471, 0.1660481256975883668, -0.3530559997133364547 ) ) ;
#62040 = CARTESIAN_POINT ( 'NONE',  ( 1.423884514435696413, -0.3162353388693409650, -0.4822834645669289433 ) ) ;
#62041 = CARTESIAN_POINT ( 'NONE',  ( -0.1958661417322836995, 0.3392501089628017219, -0.3248224653881383595 ) ) ;
#62042 = CARTESIAN_POINT ( 'NONE',  ( -0.7217847769028863381, -0.3690944881889763329, 0.3153832671262228327 ) ) ;
#62043 = PLANE ( 'NONE',  #54763 ) ;
#62044 = CARTESIAN_POINT ( 'NONE',  ( 1.437007874015748810, 0.1660481256975885056, 0.3530559997133364547 ) ) ;
#62045 = CARTESIAN_POINT ( 'NONE',  ( 0.4724409448818896462, 0.1265901696524990294, -2.091207349081364519 ) ) ;
#62046 = CARTESIAN_POINT ( 'NONE',  ( -1.213910761154854745, 0.2952755905511810774, -0.1292274648535930714 ) ) ;
#62047 = CARTESIAN_POINT ( 'NONE',  ( -1.200787401574802349, -0.4536011799217367080, 0.2665933059059888421 ) ) ;
#62048 = CARTESIAN_POINT ( 'NONE',  ( -0.7349081364829390672, 0.1283753931104746893, -0.1820866141732285504 ) ) ;
#62049 = DIRECTION ( 'NONE',  ( 1.049727191138616477E-16, -0.5150380749100564870, 0.8571673007021107793 ) ) ;
#62050 = CARTESIAN_POINT ( 'NONE',  ( -0.1312335958005241554, -0.6046776061558809534, -0.2411417322834644161 ) ) ;
#62051 = CARTESIAN_POINT ( 'NONE',  ( -0.03937007874015669567, 0.1771653543307087630, 0.000000000000000000 ) ) ;
#62052 = CARTESIAN_POINT ( 'NONE',  ( -1.299212598425196097, -0.5511811023622047445, 6.969142054262312111E-17 ) ) ;
#62053 = CARTESIAN_POINT ( 'NONE',  ( -1.286089238845143479, -0.6046776061558807314, 0.2411417322834647770 ) ) ;
#62054 = CARTESIAN_POINT ( 'NONE',  ( 1.437007874015748810, 0.07958543189024085140, 0.2665933059059887866 ) ) ;
#62055 = CARTESIAN_POINT ( 'NONE',  ( 0.7677165354330716118, 0.1660481256975883668, -0.3530559997133364547 ) ) ;
#62056 = DIRECTION ( 'NONE',  ( 0.000000000000000000, 0.000000000000000000, -1.000000000000000000 ) ) ;
#62057 = CARTESIAN_POINT ( 'NONE',  ( 0.3805774278215230400, -0.3690944881889763329, 0.3153832671262228327 ) ) ;
#62058 = CARTESIAN_POINT ( 'NONE',  ( 0.8070866141732289112, -0.5400638737290845981, -0.3530559997133363437 ) ) ;
#62059 = CARTESIAN_POINT ( 'NONE',  ( 1.128608923884514947, 0.1283753931104748280, 0.1820866141732283561 ) ) ;
#62060 = ORIENTED_EDGE ( 'NONE', *, *, #13149, .F. ) ;
#62061 = CARTESIAN_POINT ( 'NONE',  ( -1.049868766404198794, -0.6046776061558807314, 0.2411417322834647770 ) ) ;
#62062 = CARTESIAN_POINT ( 'NONE',  ( -0.9448818897637790704, -0.1870078740157480879, -0.4822834645669291653 ) ) ;
#62063 = CARTESIAN_POINT ( 'NONE',  ( 0.01312335958005323398, 0.05413385826771666132, 0.4176697321401328100 ) ) ;
#62064 = CARTESIAN_POINT ( 'NONE',  ( 0.1998031496062994405, -0.3460692066303958092, -0.09186351706036746667 ) ) ;
#62065 = CARTESIAN_POINT ( 'NONE',  ( 0.3996062992125986035, -0.1070741851644052972, -2.393044619422572072 ) ) ;
#62066 = CARTESIAN_POINT ( 'NONE',  ( 0.7152230971128614723, -0.3162353388693409650, -0.4822834645669289433 ) ) ;
#62067 = CARTESIAN_POINT ( 'NONE',  ( 1.377952755905512472, -0.5511811023622047445, 6.969142054262312111E-17 ) ) ;
#62068 = CARTESIAN_POINT ( 'NONE',  ( 0.1771653543307093182, -0.5400638737290845981, -0.3530559997133363437 ) ) ;
#62069 = CARTESIAN_POINT ( 'NONE',  ( 0.6758530183727039509, 0.2952755905511810774, -0.1292274648535930714 ) ) ;
#62070 = EDGE_CURVE ( 'NONE', #47884, #66895, #17287, .T. ) ;
#62071 = CARTESIAN_POINT ( 'NONE',  ( 0.3996062992125986035, 2.446882876249141962E-17, -1.692913385826771533 ) ) ;
#62072 = CARTESIAN_POINT ( 'NONE',  ( -0.3420746716998661618, 0.1974969037888702206, -1.128608923884514503 ) ) ;
#62073 = CARTESIAN_POINT ( 'NONE',  ( 0.1998031496062994405, -0.3460692066303958092, -2.454068241469816058 ) ) ;
#62074 = CYLINDRICAL_SURFACE ( 'NONE', #64071, 0.1771653543307085410 ) ;
#62075 = CARTESIAN_POINT ( 'NONE',  ( 0.3917322834645670104, 2.398668435337828261E-17, -0.4251968503937007537 ) ) ;
#62076 = CARTESIAN_POINT ( 'NONE',  ( -0.4986876640419942164, -0.5023911411419708095, 0.1820866141732285504 ) ) ;
#62077 = CARTESIAN_POINT ( 'NONE',  ( -0.7152230971128602510, -0.05778040916215560624, -0.4822834645669293319 ) ) ;
#62078 = CARTESIAN_POINT ( 'NONE',  ( 0.3805774278215230400, 0.05413385826771626580, -0.4176697321401330321 ) ) ;
#62079 = CARTESIAN_POINT ( 'NONE',  ( -0.3949938075777408852, -0.1058382717557502933, -2.012467191601050143 ) ) ;
#62080 = CARTESIAN_POINT ( 'NONE',  ( -1.522309711286088607, -0.6046776061558807314, 0.2411417322834647770 ) ) ;
#62081 = CARTESIAN_POINT ( 'NONE',  ( 1.115485564304462551, 0.05413385826771666132, 0.4176697321401328100 ) ) ;
#62082 = CARTESIAN_POINT ( 'NONE',  ( -0.4091458600556405756, 0.2362204724409446288, -2.388451443569553856 ) ) ;
#62083 = CARTESIAN_POINT ( 'NONE',  ( 0.1998031496062992740, 0.3460692066303959757, -1.561679790026246684 ) ) ;
#62084 = CARTESIAN_POINT ( 'NONE',  ( 1.122047244094488860, 0.1660481256975885056, 0.3530559997133364547 ) ) ;
#62085 = CARTESIAN_POINT ( 'NONE',  ( 0.8202099737532813073, 0.2952755905511811885, 0.1292274648535926551 ) ) ;
#62086 = CARTESIAN_POINT ( 'NONE',  ( 0.6627296587926515548, 0.2952755905511811885, 0.1292274648535926551 ) ) ;
#62087 = CARTESIAN_POINT ( 'NONE',  ( 1.259842519685040019, -0.1870078740157479769, 0.3641732283464567677 ) ) ;
#62089 = CARTESIAN_POINT ( 'NONE',  ( -1.646981627296586703, -0.05778040916215522460, 0.4822834645669289988 ) ) ;
#62088 = CARTESIAN_POINT ( 'NONE',  ( -1.535433070866141225, -0.5511811023622047445, 6.969142054262312111E-17 ) ) ;
#62090 = CARTESIAN_POINT ( 'NONE',  ( -0.2867679344610364334, -0.2867679344610368219, -2.658773335136795701 ) ) ;
#62091 = CARTESIAN_POINT ( 'NONE',  ( -1.614173228346457378, 1.267785121476993293, 0.1372047244094476981 ) ) ;
#62092 = CARTESIAN_POINT ( 'NONE',  ( 0.8267716535433078384, -0.6692913385826771977, 8.415575281601705876E-17 ) ) ;
#62093 = FACE_OUTER_BOUND ( 'NONE', #60971, .T. ) ;
#62094 = CARTESIAN_POINT ( 'NONE',  ( -0.5774278215223089816, 0.2306618581243847221, -0.2411417322834647770 ) ) ;
#62095 = CARTESIAN_POINT ( 'NONE',  ( -0.6364829396325453192, -0.3162353388693405765, 0.4822834645669290543 ) ) ;
#62096 = CARTESIAN_POINT ( 'NONE',  ( 1.417322834645670104, -0.1870078740157479769, 0.4822834645669291653 ) ) ;
#62097 = CARTESIAN_POINT ( 'NONE',  ( 0.1958661417322834775, 0.3392501089628018884, -0.07152230971128617498 ) ) ;
#62098 = CARTESIAN_POINT ( 'NONE',  ( 0.3543307086614179147, 0.2952755905511811885, 0.000000000000000000 ) ) ;
#62099 = CARTESIAN_POINT ( 'NONE',  ( 0.3917322834645670104, -0.1049643490035303411, -2.308398950131233640 ) ) ;
#62100 = CARTESIAN_POINT ( 'NONE',  ( 1.568241469816273659, -0.05778040916215560624, -0.4822834645669293319 ) ) ;
#62101 = ORIENTED_EDGE ( 'NONE', *, *, #10568, .T. ) ;
#62102 = CARTESIAN_POINT ( 'NONE',  ( -0.3949938075777409963, -7.255918531996591613E-17, -2.874015748031495843 ) ) ;
#62103 = ORIENTED_EDGE ( 'NONE', *, *, #80969, .T. ) ;
#62104 = DIRECTION ( 'NONE',  ( 0.000000000000000000, -1.000000000000000000, 0.000000000000000000 ) ) ;
#62105 = CARTESIAN_POINT ( 'NONE',  ( 1.194225721784777594, -0.3690944881889765550, -0.3153832671262227771 ) ) ;
#62106 = CARTESIAN_POINT ( 'NONE',  ( -0.3460692066303958092, -0.1998031496062994683, -0.8398950131233595684 ) ) ;
#62107 = DIRECTION ( 'NONE',  ( 1.000000000000000000, -0.000000000000000000, -0.000000000000000000 ) ) ;
#62108 = CARTESIAN_POINT ( 'NONE',  ( 0.000000000000000000, 0.000000000000000000, 0.000000000000000000 ) ) ;
#62109 = LINE ( 'NONE', #62523, #4678 ) ;
#62110 = CARTESIAN_POINT ( 'NONE',  ( -0.3095605055124933114, 1.709780007968088489, 0.04771746845409036847 ) ) ;
#62111 = CARTESIAN_POINT ( 'NONE',  ( -0.3392501089628019995, 0.1958661417322832277, -0.4258530183727035068 ) ) ;
#62112 = CARTESIAN_POINT ( 'NONE',  ( -0.3149606299212590610, -0.1870078740157480601, -0.3641732283464567677 ) ) ;
#62113 = CARTESIAN_POINT ( 'NONE',  ( -1.036745406824146176, -0.004921259842519870586, -0.3153832671262229437 ) ) ;
#62114 = CARTESIAN_POINT ( 'NONE',  ( -1.528871391076114250, -0.6692913385826771977, 0.1292274648535927661 ) ) ;
#62115 = CARTESIAN_POINT ( 'NONE',  ( 0.6758530183727039509, 0.2952755905511810774, -0.1292274648535930714 ) ) ;
#62116 = CARTESIAN_POINT ( 'NONE',  ( -1.509186351706035767, -0.4281496062992124485, 0.4176697321401328655 ) ) ;
#62117 = CARTESIAN_POINT ( 'NONE',  ( 0.3917322834645670104, 2.398668435337828261E-17, -0.1102362204724409156 ) ) ;
#62118 = ORIENTED_EDGE ( 'NONE', *, *, #69225, .T. ) ;
#62119 = CARTESIAN_POINT ( 'NONE',  ( 1.502624671916010790, -0.3162353388693409650, -0.4822834645669289433 ) ) ;
#62120 = CARTESIAN_POINT ( 'NONE',  ( -0.1938976377952756625, -0.1938976377952756625, 0.07874015748031495954 ) ) ;
#62121 = CARTESIAN_POINT ( 'NONE',  ( 0.3458507752293908943, 0.3458507752293908943, -1.712598425196850460 ) ) ;
#62122 = DIRECTION ( 'NONE',  ( 0.8660254037844361541, 0.000000000000000000, 0.5000000000000043299 ) ) ;
#62123 =( BOUNDED_SURFACE ( )  B_SPLINE_SURFACE ( 1, 2, ( 
 ( #65005, #76798, #13255, #12832, #19129, #51101, #71319, #31761, #50696, #13668, #1454, #76393, #12414, #71736, #38904, #44368, #32592, #52353, #38072, #20390, #51937, #39320, #64584, #57423, #77642, #6921, #33439, #46042, #200, #83117, #26276, #25435, #44778, #70475, #58255, #6507, #38489, #14091, #39743, #19545, #26698, #58679, #7341, #25852, #620, #64173, #19974, #1044, #32177, #51512, #45203, #45625, #33009, #78060, #65439, #48128, #46875, #28358, #27946, #54020, #8181, #9423, #33847, #28775, #73825, #59513, #2698, #52774, #1867, #14916, #15333, #40998, #72981, #66678, #61171, #9015, #78899, #34688, #67501, #78482, #9836, #41809, #21220, #60351, #35507, #27111, #34268, #46462, #72569, #79313, #16163, #20806, #67092, #80148, #79731, #22048, #8596, #21632, #72156, #27529, #2284, #14511, #53184, #47708, #22468, #40164, #65848, #35092, #15755, #73404, #41408, #40576, #66257, #47292, #60759, #59928, #53605, #3110, #54437, #18225, #5172, #42639, #43451, #55672, #24108, #42225, #75064, #36737, #17412, #37154, #54858, #4751, #69149, #37565, #56501, #24521, #43862, #80563, #48954, #74236, #43042, #30836, #11500, #49777, #10258, #50187, #30425, #35928, #29600, #16997, #82203, #68336, #75884, #81797, #55261, #56092, #80971, #3523, #10675, #74655, #36331, #62838, #48536, #29191, #68738, #62413, #69563, #11080, #11911, #23284, #62006, #4342, #75477, #22874, #30009, #61595, #16580, #81381, #67920, #23695, #49368, #3941, #17818, #6824, #951, #57738, #63239, #45944, #70806, #18630, #38809, #44680, #26607, #50592, #7246, #32493, #31245, #5579, #56911, #51840, #45528, #19451, #71642, #13158, #71226, #38390, #32918, #13993, #26178, #100, #77545, #82607, #52259, #57320, #58584, #77965, #13570, #24925, #37976, #45102, #51001, #64068, #19879, #25754, #76301, #44274, #64486, #6407, #76700, #20295, #69964, #12318, #63651, #51416, #31661, #39224, #77118, #58157, #70376, #5990, #83016, #525, #25339, #19033, #12731, #32077, #64909, #65758, #2189, #1774, #8091, #40071, #60259, #20716, #39650, #2608, #73736, #48034, #59009, #60669, #27857, #65341, #21540, #41319, #1364, #9333, #40900, #28265, #59836, #7676, #66581, #79224, #80055, #35004, #72479, #33347, #15240, #22374, #27016, #52677, #33755, #78385, #14828, #66166, #72891, #53927, #15659, #46367, #21131, #54345, #53517, #8917, #47201, #73311, #72061, #34594, #79639, #14419, #3017, #28684, #59418, #27432, #53094, #78804, #21957, #67001, #47616, #46788, #40488, #8506, #34172, #48441, #42132, #29505, #44482, #55166, #18837, #12119, #67827, #69775, #10165, #51216, #80875, #3845, #23187, #50807, #55574, #48858, #9744, #38187, #12526, #42542, #76508, #25138, #37777, #74558, #36236, #80469, #81284, #70173, #16071, #61080, #35415, #29093, #35831, #61497, #63862, #6199, #16903, #17317, #68244, #42945, #22781, #82814, #74141, #31877, #57537, #16486, #74971, #41717, #10579, #61906, #4248, #29910, #23599, #49269, #67410, #63452, #5788, #31458, #83228, #3430, #25549, #54764, #57120, #26812, #33965, #1982, #737, #12946, #71018, #45740, #40278, #27645, #33550, #46579, #7463, #46162, #58374, #71436, #14624, #51628, #52052, #65961, #57948, #39440, #72277, #6617, #70592, #59212, #65555, #65128, #52470, #8297, #44893, #13783, #33133, #32708, #26394, #58803, #76912, #59627, #78600, #77757, #1573, #1161, #14208, #32288, #38604, #19242, #78178, #20508, #27227, #71858, #64282, #315, #39864, #25969, #20090, #7886, #52888, #77332, #19661, #20924, #45323, #13362, #39015, #64699, #7038, #41524, #3227, #67209, #3640, #21339, #54552, #9954, #4051, #22991, #74353, #10380, #46992, #15452, #40689, #9543, #80677, #35625, #16284, #60048, #16697, #80267, #2404, #79427, #66799, #48656, #9134, #54970, #48244, #21746, #22583, #47411, #53307, #34805, #41111, #60464, #29308, #35212, #2815, #72685, #42338, #68035, #79850, #36038, #61288, #73940, #28475, #73527, #34383, #60875, #61711, #79020, #15033, #66375, #8712, #73100, #54135, #28062, #53719, #22167, #41929, #47826, #67622, #15876, #28892, #68446, #75998, #12020, #10786, #17931, #55379, #36446, #23814 ),
 ( #43567, #24221, #63353, #69677, #43156, #57022, #69268, #5687, #81085, #17116, #4462, #49069, #68852, #36859, #75592, #37275, #50300, #62119, #75179, #31356, #42751, #56209, #11615, #81909, #24634, #23402, #62950, #30947, #29717, #74768, #30127, #55791, #49486, #49892, #11200, #18340, #81497, #17523, #62533, #5286, #4871, #30544, #37676, #56614, #82314, #43980, #35061, #23250, #16547, #47677, #74201, #73372, #55637, #3079, #9391, #60727, #55227, #61138, #28743, #15301, #42603, #16964, #48093, #80934, #29565, #42192, #80116, #41775, #2668, #3490, #48919, #21599, #66645, #40963, #34655, #41377, #15721, #74620, #68305, #67058, #22841, #22434, #48500, #28327, #3905, #53989, #10641, #36296, #79701, #80529, #47260, #22017, #54404, #9803, #35474, #67468, #29156, #72950, #54825, #73793, #67887, #61970, #8982, #4309, #29973, #16129, #10225, #60319, #35892, #61562, #17378, #75442, #50152, #44646, #6371, #37940, #50967, #11877, #50558, #62803, #75848, #18997, #56054, #56468, #70343, #62376, #43823, #76664, #11043, #75033, #63617, #69928, #69527, #56877, #64031, #4714, #18190, #12697, #37119, #5137, #37529, #32043, #38356, #82982, #30802, #5954, #63205, #18596, #43008, #31623, #12284, #5544, #82570, #81346, #30388, #31209, #23661, #82169, #24485, #24889, #49332, #68702, #25302, #76261, #57285, #44239, #36702, #81763, #24073, #49742, #17781, #43415, #69113, #11461, #14382, #8467, #27397, #78769, #14794, #25719, #19842, #45067, #71605, #1740, #40040, #20681, #64449, #21093, #58975, #6785, #486, #71188, #53057, #13530, #59382, #52645, #26141, #26980, #51802, #57702, #39186, #45491, #64870, #8059, #13958, #7210, #51379, #46752, #72445, #915, #33720, #65726, #78349, #32880, #77928, #38772, #39615, #40451, #65, #19416, #77084, #70770, #77507, #58549, #66130, #13120, #26572, #1331, #52225, #46333, #32457, #58119, #20259, #45908, #65304, #7643, #33313, #72026, #66774, #44978, #22141, #79825, #6279, #9107, #58457, #70252, #52129, #73075, #31955, #41085, #72657, #34357, #7117, #12607, #15007, #26479, #28450, #34780, #19747, #38265, #46965, #54109, #63942, #83307, #13030, #57616, #45402, #13441, #21312, #8687, #47384, #51292, #51711, #2790, #25629, #76995, #817, #38683, #79401, #78992, #32788, #77412, #19326, #70673, #40664, #64361, #6698, #60439, #71098, #2378, #32367, #66348, #58031, #394, #26052, #39097, #64779, #60023, #28035, #53693, #21720, #15424, #68828, #36015, #56183, #29691, #49460, #67185, #17500, #49044, #10762, #68010, #47799, #74741, #4027, #4846, #43130, #80652, #81886, #23376, #30521, #41500, #60849, #73916, #9515, #22965, #74326, #81060, #68422, #23789, #28865, #29282, #62508, #35188, #73503, #55354, #17089, #4437, #42726, #54946, #36422, #11175, #61686, #62095, #15851, #3616, #80242, #3201, #9928, #54527, #16256, #48631, #22558, #75155, #30103, #36835, #42312, #48220, #41903, #55765, #67597, #81472, #16673, #35599, #61262, #10355, #51092, #75567, #24197, #17908, #12824, #6498, #63740, #32584, #31753, #32168, #82695, #51504, #58247, #70467, #18718, #38481, #43544, #45194, #18315, #77208, #19537, #57824, #69243, #82291, #6079, #11997, #25014, #64165, #44360, #11591, #37251, #25427, #50687, #37651, #38896, #62926, #5260, #30924, #56590, #83108, #5666, #70897, #24610, #13247, #76789, #50277, #49867, #75975, #191, #25844, #57415, #43957, #19121, #64575, #76385, #6912, #69653, #63328, #70051, #31333, #56998, #12406, #38064, #44770, #53597, #8589, #51929, #58672, #40157, #71729, #1447, #14909, #78475, #19966, #77634, #1859, #27104, #14084, #15326, #45617, #71311, #13658, #72148, #52346, #34260, #14504, #46455, #65432, #39311, #34681, #65841, #78053, #64999, #21624, #7765, #40569, #26691, #8174, #46034, #20382, #1037, #39736, #33431, #79306, #59092, #612, #9009, #7334, #47284, #33839, #26268, #59506, #2276, #33002, #72974, #27521, #46868, #20799, #52766, #53177, #78892, #40991, #66670, #21213, #72562, #66250, #59921, #27939, #73398, #3104, #22042, #35501, #3516, #10251, #80962, #36324, #41402, #41803, #75058, #47702, #2692, #42219, #35922, #16990, #67915 ) ),
 .UNSPECIFIED., .F., .F., .F. ) 
 B_SPLINE_SURFACE_WITH_KNOTS ( ( 2, 2 ),
 ( 3, 2, 2, 2, 2, 2, 2, 2, 2, 2, 2, 2, 2, 2, 2, 2, 2, 2, 2, 2, 2, 2, 2, 2, 2, 2, 2, 2, 2, 2, 2, 2, 2, 2, 2, 2, 2, 2, 2, 2, 2, 2, 2, 2, 2, 2, 2, 2, 2, 2, 2, 2, 2, 2, 2, 2, 2, 2, 2, 2, 2, 2, 2, 2, 2, 2, 2, 2, 2, 2, 2, 2, 2, 2, 2, 2, 2, 2, 2, 2, 2, 2, 2, 2, 2, 2, 2, 2, 2, 2, 2, 2, 2, 2, 2, 2, 2, 2, 2, 2, 2, 2, 2, 2, 2, 2, 2, 2, 2, 2, 2, 2, 2, 2, 2, 2, 2, 2, 2, 2, 2, 2, 2, 2, 2, 2, 2, 2, 2, 2, 2, 2, 2, 2, 2, 2, 2, 2, 2, 2, 2, 2, 2, 2, 2, 2, 2, 2, 2, 2, 2, 2, 2, 2, 2, 2, 2, 2, 2, 2, 2, 2, 2, 2, 2, 2, 2, 2, 2, 2, 2, 2, 2, 2, 2, 2, 2, 2, 2, 2, 2, 2, 2, 2, 2, 2, 2, 2, 2, 2, 2, 2, 2, 2, 2, 2, 2, 2, 2, 2, 2, 2, 2, 2, 2, 2, 2, 2, 2, 2, 2, 2, 2, 2, 2, 2, 2, 2, 2, 2, 2, 2, 2, 2, 2, 2, 2, 2, 2, 2, 2, 2, 2, 2, 2, 2, 2, 2, 2, 2, 2, 2, 2, 2, 2, 2, 2, 2, 2, 2, 2, 2, 2, 2, 2, 3 ),
 ( 0.000000000000000000, 1.000000000000000000 ),
 ( 0.000000000000000000, 0.003787878787878787984, 0.007575757575757575968, 0.01136363636363636395, 0.01515151515151515194, 0.01893939393939393992, 0.02272727272727272790, 0.02651515151515151589, 0.03030303030303030387, 0.03409090909090908839, 0.03787878787878787984, 0.04166666666666666435, 0.04545454545454545581, 0.04924242424242424032, 0.05303030303030303177, 0.05681818181818181629, 0.06060606060606060774, 0.06439393939393939226, 0.06818181818181817677, 0.07196969696969697516, 0.07575757575757575968, 0.07954545454545454419, 0.08333333333333332871, 0.08712121212121212710, 0.09090909090909091161, 0.09469696969696969613, 0.09848484848484848064, 0.1022727272727272790, 0.1060606060606060635, 0.1098484848484848481, 0.1136363636363636326, 0.1174242424242424310, 0.1212121212121212155, 0.1250000000000000000, 0.1287878787878787845, 0.1325757575757575690, 0.1363636363636363535, 0.1401515151515151381, 0.1439393939393939503, 0.1477272727272727348, 0.1515151515151515194, 0.1553030303030303039, 0.1590909090909090884, 0.1628787878787878729, 0.1666666666666666574, 0.1704545454545454419, 0.1742424242424242542, 0.1780303030303030387, 0.1818181818181818232, 0.1856060606060606077, 0.1893939393939393923, 0.1931818181818181768, 0.1969696969696969613, 0.2007575757575757458, 0.2045454545454545581, 0.2083333333333333426, 0.2121212121212121271, 0.2159090909090909116, 0.2196969696969696961, 0.2234848484848484806, 0.2272727272727272652, 0.2310606060606060497, 0.2348484848484848619, 0.2386363636363636465, 0.2424242424242424310, 0.2462121212121212155, 0.2500000000000000000, 0.2537878787878787845, 0.2575757575757575690, 0.2613636363636363535, 0.2651515151515151381, 0.2689393939393939226, 0.2727272727272727071, 0.2765151515151514916, 0.2803030303030302761, 0.2840909090909091161, 0.2878787878787879007, 0.2916666666666666852, 0.2954545454545454697, 0.2992424242424242542, 0.3030303030303030387, 0.3068181818181818232, 0.3106060606060606077, 0.3143939393939393923, 0.3181818181818181768, 0.3219696969696969613, 0.3257575757575757458, 0.3295454545454545303, 0.3333333333333333148, 0.3371212121212120993, 0.3409090909090908839, 0.3446969696969697239, 0.3484848484848485084, 0.3522727272727272929, 0.3560606060606060774, 0.3598484848484848619, 0.3636363636363636465, 0.3674242424242424310, 0.3712121212121212155, 0.3750000000000000000, 0.3787878787878787845, 0.3825757575757575690, 0.3863636363636363535, 0.3901515151515151381, 0.3939393939393939226, 0.3977272727272727071, 0.4015151515151514916, 0.4053030303030302761, 0.4090909090909091161, 0.4128787878787879007, 0.4166666666666666852, 0.4204545454545454697, 0.4242424242424242542, 0.4280303030303030387, 0.4318181818181818232, 0.4356060606060606077, 0.4393939393939393923, 0.4431818181818181768, 0.4469696969696969613, 0.4507575757575757458, 0.4545454545454545303, 0.4583333333333333148, 0.4621212121212120993, 0.4659090909090908839, 0.4696969696969697239, 0.4734848484848485084, 0.4772727272727272929, 0.4810606060606060774, 0.4848484848484848619, 0.4886363636363636465, 0.4924242424242424310, 0.4962121212121212155, 0.5000000000000000000, 0.5037878787878787845, 0.5075757575757575690, 0.5113636363636363535, 0.5151515151515151381, 0.5189393939393939226, 0.5227272727272727071, 0.5265151515151514916, 0.5303030303030302761, 0.5340909090909090606, 0.5378787878787878451, 0.5416666666666666297, 0.5454545454545454142, 0.5492424242424241987, 0.5530303030303029832, 0.5568181818181817677, 0.5606060606060605522, 0.5643939393939394478, 0.5681818181818182323, 0.5719696969696970168, 0.5757575757575758013, 0.5795454545454545858, 0.5833333333333333703, 0.5871212121212121549, 0.5909090909090909394, 0.5946969696969697239, 0.5984848484848485084, 0.6022727272727272929, 0.6060606060606060774, 0.6098484848484848619, 0.6136363636363636465, 0.6174242424242424310, 0.6212121212121212155, 0.6250000000000000000, 0.6287878787878787845, 0.6325757575757575690, 0.6363636363636363535, 0.6401515151515151381, 0.6439393939393939226, 0.6477272727272727071, 0.6515151515151514916, 0.6553030303030302761, 0.6590909090909090606, 0.6628787878787878451, 0.6666666666666666297, 0.6704545454545454142, 0.6742424242424241987, 0.6780303030303029832, 0.6818181818181817677, 0.6856060606060605522, 0.6893939393939394478, 0.6931818181818182323, 0.6969696969696970168, 0.7007575757575758013, 0.7045454545454545858, 0.7083333333333333703, 0.7121212121212121549, 0.7159090909090909394, 0.7196969696969697239, 0.7234848484848485084, 0.7272727272727272929, 0.7310606060606060774, 0.7348484848484848619, 0.7386363636363636465, 0.7424242424242424310, 0.7462121212121212155, 0.7500000000000000000, 0.7537878787878787845, 0.7575757575757575690, 0.7613636363636363535, 0.7651515151515151381, 0.7689393939393939226, 0.7727272727272727071, 0.7765151515151514916, 0.7803030303030302761, 0.7840909090909090606, 0.7878787878787878451, 0.7916666666666666297, 0.7954545454545454142, 0.7992424242424241987, 0.8030303030303029832, 0.8068181818181817677, 0.8106060606060605522, 0.8143939393939394478, 0.8181818181818182323, 0.8219696969696970168, 0.8257575757575758013, 0.8295454545454545858, 0.8333333333333333703, 0.8371212121212121549, 0.8409090909090909394, 0.8446969696969697239, 0.8484848484848485084, 0.8522727272727272929, 0.8560606060606060774, 0.8598484848484848619, 0.8636363636363636465, 0.8674242424242424310, 0.8712121212121212155, 0.8750000000000000000, 0.8787878787878787845, 0.8825757575757575690, 0.8863636363636363535, 0.8901515151515151381, 0.8939393939393939226, 0.8977272727272727071, 0.9015151515151514916, 0.9053030303030302761, 0.9090909090909090606, 0.9128787878787878451, 0.9166666666666666297, 0.9204545454545454142, 0.9242424242424241987, 0.9280303030303029832, 0.9318181818181817677, 0.9356060606060605522, 0.9393939393939394478, 0.9431818181818182323, 0.9469696969696970168, 0.9507575757575758013, 0.9545454545454545858, 0.9583333333333333703, 0.9621212121212121549, 0.9659090909090909394 ),
 .UNSPECIFIED. ) 
 GEOMETRIC_REPRESENTATION_ITEM ( )  RATIONAL_B_SPLINE_SURFACE ( (
 ( 1.000000000000000000, 0.9659258262890683122, 1.000000000000000000, 0.9659258262890683122, 1.000000000000000000, 0.9659258262890683122, 1.000000000000000000, 0.9659258262890683122, 1.000000000000000000, 0.9659258262890683122, 1.000000000000000000, 0.9659258262890683122, 1.000000000000000000, 0.9659258262890683122, 1.000000000000000000, 0.9659258262890683122, 1.000000000000000000, 0.9659258262890683122, 1.000000000000000000, 0.9659258262890683122, 1.000000000000000000, 0.9659258262890683122, 1.000000000000000000, 0.9659258262890683122, 1.000000000000000000, 0.9659258262890683122, 1.000000000000000000, 0.9659258262890683122, 1.000000000000000000, 0.9659258262890683122, 1.000000000000000000, 0.9659258262890683122, 1.000000000000000000, 0.9659258262890683122, 1.000000000000000000, 0.9659258262890683122, 1.000000000000000000, 0.9659258262890683122, 1.000000000000000000, 0.9659258262890683122, 1.000000000000000000, 0.9659258262890683122, 1.000000000000000000, 0.9659258262890683122, 1.000000000000000000, 0.9659258262890683122, 1.000000000000000000, 0.9659258262890683122, 1.000000000000000000, 0.9659258262890683122, 1.000000000000000000, 0.9659258262890683122, 1.000000000000000000, 0.9659258262890683122, 1.000000000000000000, 0.9659258262890683122, 1.000000000000000000, 0.9659258262890683122, 1.000000000000000000, 0.9659258262890683122, 1.000000000000000000, 0.9659258262890683122, 1.000000000000000000, 0.9659258262890683122, 1.000000000000000000, 0.9659258262890683122, 1.000000000000000000, 0.9659258262890683122, 1.000000000000000000, 0.9659258262890683122, 1.000000000000000000, 0.9659258262890683122, 1.000000000000000000, 0.9659258262890683122, 1.000000000000000000, 0.9659258262890683122, 1.000000000000000000, 0.9659258262890683122, 1.000000000000000000, 0.9659258262890683122, 1.000000000000000000, 0.9659258262890683122, 1.000000000000000000, 0.9659258262890683122, 1.000000000000000000, 0.9659258262890683122, 1.000000000000000000, 0.9659258262890683122, 1.000000000000000000, 0.9659258262890683122, 1.000000000000000000, 0.9659258262890683122, 1.000000000000000000, 0.9659258262890683122, 1.000000000000000000, 0.9659258262890683122, 1.000000000000000000, 0.9659258262890683122, 1.000000000000000000, 0.9659258262890683122, 1.000000000000000000, 0.9659258262890683122, 1.000000000000000000, 0.9659258262890683122, 1.000000000000000000, 0.9659258262890683122, 1.000000000000000000, 0.9659258262890683122, 1.000000000000000000, 0.9659258262890683122, 1.000000000000000000, 0.9659258262890683122, 1.000000000000000000, 0.9659258262890683122, 1.000000000000000000, 0.9659258262890683122, 1.000000000000000000, 0.9659258262890683122, 1.000000000000000000, 0.9659258262890683122, 1.000000000000000000, 0.9659258262890683122, 1.000000000000000000, 0.9659258262890683122, 1.000000000000000000, 0.9659258262890683122, 1.000000000000000000, 0.9659258262890683122, 1.000000000000000000, 0.9659258262890683122, 1.000000000000000000, 0.9659258262890683122, 1.000000000000000000, 0.9659258262890683122, 1.000000000000000000, 0.9659258262890683122, 1.000000000000000000, 0.9659258262890683122, 1.000000000000000000, 0.9659258262890683122, 1.000000000000000000, 0.9659258262890683122, 1.000000000000000000, 0.9659258262890683122, 1.000000000000000000, 0.9659258262890683122, 1.000000000000000000, 0.9659258262890683122, 1.000000000000000000, 0.9659258262890683122, 1.000000000000000000, 0.9659258262890683122, 1.000000000000000000, 0.9659258262890683122, 1.000000000000000000, 0.9659258262890683122, 1.000000000000000000, 0.9659258262890683122, 1.000000000000000000, 0.9659258262890683122, 1.000000000000000000, 0.9659258262890683122, 1.000000000000000000, 0.9659258262890683122, 1.000000000000000000, 0.9659258262890683122, 1.000000000000000000, 0.9659258262890683122, 1.000000000000000000, 0.9659258262890683122, 1.000000000000000000, 0.9659258262890683122, 1.000000000000000000, 0.9659258262890683122, 1.000000000000000000, 0.9659258262890683122, 1.000000000000000000, 0.9659258262890683122, 1.000000000000000000, 0.9659258262890683122, 1.000000000000000000, 0.9659258262890683122, 1.000000000000000000, 0.9659258262890683122, 1.000000000000000000, 0.9659258262890683122, 1.000000000000000000, 0.9659258262890683122, 1.000000000000000000, 0.9659258262890683122, 1.000000000000000000, 0.9659258262890683122, 1.000000000000000000, 0.9659258262890683122, 1.000000000000000000, 0.9659258262890683122, 1.000000000000000000, 0.9659258262890683122, 1.000000000000000000, 0.9659258262890683122, 1.000000000000000000, 0.9659258262890683122, 1.000000000000000000, 0.9659258262890683122, 1.000000000000000000, 0.9659258262890683122, 1.000000000000000000, 0.9659258262890683122, 1.000000000000000000, 0.9659258262890683122, 1.000000000000000000, 0.9659258262890683122, 1.000000000000000000, 0.9659258262890683122, 1.000000000000000000, 0.9659258262890683122, 1.000000000000000000, 0.9659258262890683122, 1.000000000000000000, 0.9659258262890683122, 1.000000000000000000, 0.9659258262890683122, 1.000000000000000000, 0.9659258262890683122, 1.000000000000000000, 0.9659258262890683122, 1.000000000000000000, 0.9659258262890683122, 1.000000000000000000, 0.9659258262890683122, 1.000000000000000000, 0.9659258262890683122, 1.000000000000000000, 0.9659258262890683122, 1.000000000000000000, 0.9659258262890683122, 1.000000000000000000, 0.9659258262890683122, 1.000000000000000000, 0.9659258262890683122, 1.000000000000000000, 0.9659258262890683122, 1.000000000000000000, 0.9659258262890683122, 1.000000000000000000, 0.9659258262890683122, 1.000000000000000000, 0.9659258262890683122, 1.000000000000000000, 0.9659258262890683122, 1.000000000000000000, 0.9659258262890683122, 1.000000000000000000, 0.9659258262890683122, 1.000000000000000000, 0.9659258262890683122, 1.000000000000000000, 0.9659258262890683122, 1.000000000000000000, 0.9659258262890683122, 1.000000000000000000, 0.9659258262890683122, 1.000000000000000000, 0.9659258262890683122, 1.000000000000000000, 0.9659258262890683122, 1.000000000000000000, 0.9659258262890683122, 1.000000000000000000, 0.9659258262890683122, 1.000000000000000000, 0.9659258262890683122, 1.000000000000000000, 0.9659258262890683122, 1.000000000000000000, 0.9659258262890683122, 1.000000000000000000, 0.9659258262890683122, 1.000000000000000000, 0.9659258262890683122, 1.000000000000000000, 0.9659258262890683122, 1.000000000000000000, 0.9659258262890683122, 1.000000000000000000, 0.9659258262890683122, 1.000000000000000000, 0.9659258262890683122, 1.000000000000000000, 0.9659258262890683122, 1.000000000000000000, 0.9659258262890683122, 1.000000000000000000, 0.9659258262890683122, 1.000000000000000000, 0.9659258262890683122, 1.000000000000000000, 0.9659258262890683122, 1.000000000000000000, 0.9659258262890683122, 1.000000000000000000, 0.9659258262890683122, 1.000000000000000000, 0.9659258262890683122, 1.000000000000000000, 0.9659258262890683122, 1.000000000000000000, 0.9659258262890683122, 1.000000000000000000, 0.9659258262890683122, 1.000000000000000000, 0.9659258262890683122, 1.000000000000000000, 0.9659258262890683122, 1.000000000000000000, 0.9659258262890683122, 1.000000000000000000, 0.9659258262890683122, 1.000000000000000000, 0.9659258262890683122, 1.000000000000000000, 0.9659258262890683122, 1.000000000000000000, 0.9659258262890683122, 1.000000000000000000, 0.9659258262890683122, 1.000000000000000000, 0.9659258262890683122, 1.000000000000000000, 0.9659258262890683122, 1.000000000000000000, 0.9659258262890683122, 1.000000000000000000, 0.9659258262890683122, 1.000000000000000000, 0.9659258262890683122, 1.000000000000000000, 0.9659258262890683122, 1.000000000000000000, 0.9659258262890683122, 1.000000000000000000, 0.9659258262890683122, 1.000000000000000000, 0.9659258262890683122, 1.000000000000000000, 0.9659258262890683122, 1.000000000000000000, 0.9659258262890683122, 1.000000000000000000, 0.9659258262890683122, 1.000000000000000000, 0.9659258262890683122, 1.000000000000000000, 0.9659258262890683122, 1.000000000000000000, 0.9659258262890683122, 1.000000000000000000, 0.9659258262890683122, 1.000000000000000000, 0.9659258262890683122, 1.000000000000000000, 0.9659258262890683122, 1.000000000000000000, 0.9659258262890683122, 1.000000000000000000, 0.9659258262890683122, 1.000000000000000000, 0.9659258262890683122, 1.000000000000000000, 0.9659258262890683122, 1.000000000000000000, 0.9659258262890683122, 1.000000000000000000, 0.9659258262890683122, 1.000000000000000000, 0.9659258262890683122, 1.000000000000000000, 0.9659258262890683122, 1.000000000000000000, 0.9659258262890683122, 1.000000000000000000, 0.9659258262890683122, 1.000000000000000000, 0.9659258262890683122, 1.000000000000000000, 0.9659258262890683122, 1.000000000000000000, 0.9659258262890683122, 1.000000000000000000, 0.9659258262890683122, 1.000000000000000000, 0.9659258262890683122, 1.000000000000000000, 0.9659258262890683122, 1.000000000000000000, 0.9659258262890683122, 1.000000000000000000, 0.9659258262890683122, 1.000000000000000000, 0.9659258262890683122, 1.000000000000000000, 0.9659258262890683122, 1.000000000000000000, 0.9659258262890683122, 1.000000000000000000, 0.9659258262890683122, 1.000000000000000000, 0.9659258262890683122, 1.000000000000000000, 0.9659258262890683122, 1.000000000000000000, 0.9659258262890683122, 1.000000000000000000, 0.9659258262890683122, 1.000000000000000000, 0.9659258262890683122, 1.000000000000000000, 0.9659258262890683122, 1.000000000000000000, 0.9659258262890683122, 1.000000000000000000, 0.9659258262890683122, 1.000000000000000000, 0.9659258262890683122, 1.000000000000000000, 0.9659258262890683122, 1.000000000000000000, 0.9659258262890683122, 1.000000000000000000, 0.9659258262890683122, 1.000000000000000000, 0.9659258262890683122, 1.000000000000000000, 0.9659258262890683122, 1.000000000000000000, 0.9659258262890683122, 1.000000000000000000, 0.9659258262890683122, 1.000000000000000000, 0.9659258262890683122, 1.000000000000000000, 0.9659258262890683122, 1.000000000000000000, 0.9659258262890683122, 1.000000000000000000, 0.9659258262890683122, 1.000000000000000000, 0.9659258262890683122, 1.000000000000000000, 0.9659258262890683122, 1.000000000000000000, 0.9659258262890683122, 1.000000000000000000, 0.9659258262890683122, 1.000000000000000000, 0.9659258262890683122, 1.000000000000000000, 0.9659258262890683122, 1.000000000000000000, 0.9659258262890683122, 1.000000000000000000, 0.9659258262890683122, 1.000000000000000000, 0.9659258262890683122, 1.000000000000000000, 0.9659258262890683122, 1.000000000000000000, 0.9659258262890683122, 1.000000000000000000, 0.9659258262890683122, 1.000000000000000000, 0.9659258262890683122, 1.000000000000000000, 0.9659258262890683122, 1.000000000000000000, 0.9659258262890683122, 1.000000000000000000, 0.9659258262890683122, 1.000000000000000000, 0.9659258262890683122, 1.000000000000000000, 0.9659258262890683122, 1.000000000000000000, 0.9659258262890683122, 1.000000000000000000, 0.9659258262890683122, 1.000000000000000000, 0.9659258262890683122, 1.000000000000000000, 0.9659258262890683122, 1.000000000000000000, 0.9659258262890683122, 1.000000000000000000, 0.9659258262890683122, 1.000000000000000000, 0.9659258262890683122, 1.000000000000000000, 0.9659258262890683122, 1.000000000000000000, 0.9659258262890683122, 1.000000000000000000, 0.9659258262890683122, 1.000000000000000000, 0.9659258262890683122, 1.000000000000000000, 0.9659258262890683122, 1.000000000000000000, 0.9659258262890683122, 1.000000000000000000, 0.9659258262890683122, 1.000000000000000000),
 ( 1.000000000000000000, 0.9659258262890683122, 1.000000000000000000, 0.9659258262890683122, 1.000000000000000000, 0.9659258262890683122, 1.000000000000000000, 0.9659258262890683122, 1.000000000000000000, 0.9659258262890683122, 1.000000000000000000, 0.9659258262890683122, 1.000000000000000000, 0.9659258262890683122, 1.000000000000000000, 0.9659258262890683122, 1.000000000000000000, 0.9659258262890683122, 1.000000000000000000, 0.9659258262890683122, 1.000000000000000000, 0.9659258262890683122, 1.000000000000000000, 0.9659258262890683122, 1.000000000000000000, 0.9659258262890683122, 1.000000000000000000, 0.9659258262890683122, 1.000000000000000000, 0.9659258262890683122, 1.000000000000000000, 0.9659258262890683122, 1.000000000000000000, 0.9659258262890683122, 1.000000000000000000, 0.9659258262890683122, 1.000000000000000000, 0.9659258262890683122, 1.000000000000000000, 0.9659258262890683122, 1.000000000000000000, 0.9659258262890683122, 1.000000000000000000, 0.9659258262890683122, 1.000000000000000000, 0.9659258262890683122, 1.000000000000000000, 0.9659258262890683122, 1.000000000000000000, 0.9659258262890683122, 1.000000000000000000, 0.9659258262890683122, 1.000000000000000000, 0.9659258262890683122, 1.000000000000000000, 0.9659258262890683122, 1.000000000000000000, 0.9659258262890683122, 1.000000000000000000, 0.9659258262890683122, 1.000000000000000000, 0.9659258262890683122, 1.000000000000000000, 0.9659258262890683122, 1.000000000000000000, 0.9659258262890683122, 1.000000000000000000, 0.9659258262890683122, 1.000000000000000000, 0.9659258262890683122, 1.000000000000000000, 0.9659258262890683122, 1.000000000000000000, 0.9659258262890683122, 1.000000000000000000, 0.9659258262890683122, 1.000000000000000000, 0.9659258262890683122, 1.000000000000000000, 0.9659258262890683122, 1.000000000000000000, 0.9659258262890683122, 1.000000000000000000, 0.9659258262890683122, 1.000000000000000000, 0.9659258262890683122, 1.000000000000000000, 0.9659258262890683122, 1.000000000000000000, 0.9659258262890683122, 1.000000000000000000, 0.9659258262890683122, 1.000000000000000000, 0.9659258262890683122, 1.000000000000000000, 0.9659258262890683122, 1.000000000000000000, 0.9659258262890683122, 1.000000000000000000, 0.9659258262890683122, 1.000000000000000000, 0.9659258262890683122, 1.000000000000000000, 0.9659258262890683122, 1.000000000000000000, 0.9659258262890683122, 1.000000000000000000, 0.9659258262890683122, 1.000000000000000000, 0.9659258262890683122, 1.000000000000000000, 0.9659258262890683122, 1.000000000000000000, 0.9659258262890683122, 1.000000000000000000, 0.9659258262890683122, 1.000000000000000000, 0.9659258262890683122, 1.000000000000000000, 0.9659258262890683122, 1.000000000000000000, 0.9659258262890683122, 1.000000000000000000, 0.9659258262890683122, 1.000000000000000000, 0.9659258262890683122, 1.000000000000000000, 0.9659258262890683122, 1.000000000000000000, 0.9659258262890683122, 1.000000000000000000, 0.9659258262890683122, 1.000000000000000000, 0.9659258262890683122, 1.000000000000000000, 0.9659258262890683122, 1.000000000000000000, 0.9659258262890683122, 1.000000000000000000, 0.9659258262890683122, 1.000000000000000000, 0.9659258262890683122, 1.000000000000000000, 0.9659258262890683122, 1.000000000000000000, 0.9659258262890683122, 1.000000000000000000, 0.9659258262890683122, 1.000000000000000000, 0.9659258262890683122, 1.000000000000000000, 0.9659258262890683122, 1.000000000000000000, 0.9659258262890683122, 1.000000000000000000, 0.9659258262890683122, 1.000000000000000000, 0.9659258262890683122, 1.000000000000000000, 0.9659258262890683122, 1.000000000000000000, 0.9659258262890683122, 1.000000000000000000, 0.9659258262890683122, 1.000000000000000000, 0.9659258262890683122, 1.000000000000000000, 0.9659258262890683122, 1.000000000000000000, 0.9659258262890683122, 1.000000000000000000, 0.9659258262890683122, 1.000000000000000000, 0.9659258262890683122, 1.000000000000000000, 0.9659258262890683122, 1.000000000000000000, 0.9659258262890683122, 1.000000000000000000, 0.9659258262890683122, 1.000000000000000000, 0.9659258262890683122, 1.000000000000000000, 0.9659258262890683122, 1.000000000000000000, 0.9659258262890683122, 1.000000000000000000, 0.9659258262890683122, 1.000000000000000000, 0.9659258262890683122, 1.000000000000000000, 0.9659258262890683122, 1.000000000000000000, 0.9659258262890683122, 1.000000000000000000, 0.9659258262890683122, 1.000000000000000000, 0.9659258262890683122, 1.000000000000000000, 0.9659258262890683122, 1.000000000000000000, 0.9659258262890683122, 1.000000000000000000, 0.9659258262890683122, 1.000000000000000000, 0.9659258262890683122, 1.000000000000000000, 0.9659258262890683122, 1.000000000000000000, 0.9659258262890683122, 1.000000000000000000, 0.9659258262890683122, 1.000000000000000000, 0.9659258262890683122, 1.000000000000000000, 0.9659258262890683122, 1.000000000000000000, 0.9659258262890683122, 1.000000000000000000, 0.9659258262890683122, 1.000000000000000000, 0.9659258262890683122, 1.000000000000000000, 0.9659258262890683122, 1.000000000000000000, 0.9659258262890683122, 1.000000000000000000, 0.9659258262890683122, 1.000000000000000000, 0.9659258262890683122, 1.000000000000000000, 0.9659258262890683122, 1.000000000000000000, 0.9659258262890683122, 1.000000000000000000, 0.9659258262890683122, 1.000000000000000000, 0.9659258262890683122, 1.000000000000000000, 0.9659258262890683122, 1.000000000000000000, 0.9659258262890683122, 1.000000000000000000, 0.9659258262890683122, 1.000000000000000000, 0.9659258262890683122, 1.000000000000000000, 0.9659258262890683122, 1.000000000000000000, 0.9659258262890683122, 1.000000000000000000, 0.9659258262890683122, 1.000000000000000000, 0.9659258262890683122, 1.000000000000000000, 0.9659258262890683122, 1.000000000000000000, 0.9659258262890683122, 1.000000000000000000, 0.9659258262890683122, 1.000000000000000000, 0.9659258262890683122, 1.000000000000000000, 0.9659258262890683122, 1.000000000000000000, 0.9659258262890683122, 1.000000000000000000, 0.9659258262890683122, 1.000000000000000000, 0.9659258262890683122, 1.000000000000000000, 0.9659258262890683122, 1.000000000000000000, 0.9659258262890683122, 1.000000000000000000, 0.9659258262890683122, 1.000000000000000000, 0.9659258262890683122, 1.000000000000000000, 0.9659258262890683122, 1.000000000000000000, 0.9659258262890683122, 1.000000000000000000, 0.9659258262890683122, 1.000000000000000000, 0.9659258262890683122, 1.000000000000000000, 0.9659258262890683122, 1.000000000000000000, 0.9659258262890683122, 1.000000000000000000, 0.9659258262890683122, 1.000000000000000000, 0.9659258262890683122, 1.000000000000000000, 0.9659258262890683122, 1.000000000000000000, 0.9659258262890683122, 1.000000000000000000, 0.9659258262890683122, 1.000000000000000000, 0.9659258262890683122, 1.000000000000000000, 0.9659258262890683122, 1.000000000000000000, 0.9659258262890683122, 1.000000000000000000, 0.9659258262890683122, 1.000000000000000000, 0.9659258262890683122, 1.000000000000000000, 0.9659258262890683122, 1.000000000000000000, 0.9659258262890683122, 1.000000000000000000, 0.9659258262890683122, 1.000000000000000000, 0.9659258262890683122, 1.000000000000000000, 0.9659258262890683122, 1.000000000000000000, 0.9659258262890683122, 1.000000000000000000, 0.9659258262890683122, 1.000000000000000000, 0.9659258262890683122, 1.000000000000000000, 0.9659258262890683122, 1.000000000000000000, 0.9659258262890683122, 1.000000000000000000, 0.9659258262890683122, 1.000000000000000000, 0.9659258262890683122, 1.000000000000000000, 0.9659258262890683122, 1.000000000000000000, 0.9659258262890683122, 1.000000000000000000, 0.9659258262890683122, 1.000000000000000000, 0.9659258262890683122, 1.000000000000000000, 0.9659258262890683122, 1.000000000000000000, 0.9659258262890683122, 1.000000000000000000, 0.9659258262890683122, 1.000000000000000000, 0.9659258262890683122, 1.000000000000000000, 0.9659258262890683122, 1.000000000000000000, 0.9659258262890683122, 1.000000000000000000, 0.9659258262890683122, 1.000000000000000000, 0.9659258262890683122, 1.000000000000000000, 0.9659258262890683122, 1.000000000000000000, 0.9659258262890683122, 1.000000000000000000, 0.9659258262890683122, 1.000000000000000000, 0.9659258262890683122, 1.000000000000000000, 0.9659258262890683122, 1.000000000000000000, 0.9659258262890683122, 1.000000000000000000, 0.9659258262890683122, 1.000000000000000000, 0.9659258262890683122, 1.000000000000000000, 0.9659258262890683122, 1.000000000000000000, 0.9659258262890683122, 1.000000000000000000, 0.9659258262890683122, 1.000000000000000000, 0.9659258262890683122, 1.000000000000000000, 0.9659258262890683122, 1.000000000000000000, 0.9659258262890683122, 1.000000000000000000, 0.9659258262890683122, 1.000000000000000000, 0.9659258262890683122, 1.000000000000000000, 0.9659258262890683122, 1.000000000000000000, 0.9659258262890683122, 1.000000000000000000, 0.9659258262890683122, 1.000000000000000000, 0.9659258262890683122, 1.000000000000000000, 0.9659258262890683122, 1.000000000000000000, 0.9659258262890683122, 1.000000000000000000, 0.9659258262890683122, 1.000000000000000000, 0.9659258262890683122, 1.000000000000000000, 0.9659258262890683122, 1.000000000000000000, 0.9659258262890683122, 1.000000000000000000, 0.9659258262890683122, 1.000000000000000000, 0.9659258262890683122, 1.000000000000000000, 0.9659258262890683122, 1.000000000000000000, 0.9659258262890683122, 1.000000000000000000, 0.9659258262890683122, 1.000000000000000000, 0.9659258262890683122, 1.000000000000000000, 0.9659258262890683122, 1.000000000000000000, 0.9659258262890683122, 1.000000000000000000, 0.9659258262890683122, 1.000000000000000000, 0.9659258262890683122, 1.000000000000000000, 0.9659258262890683122, 1.000000000000000000, 0.9659258262890683122, 1.000000000000000000, 0.9659258262890683122, 1.000000000000000000, 0.9659258262890683122, 1.000000000000000000, 0.9659258262890683122, 1.000000000000000000, 0.9659258262890683122, 1.000000000000000000, 0.9659258262890683122, 1.000000000000000000, 0.9659258262890683122, 1.000000000000000000, 0.9659258262890683122, 1.000000000000000000, 0.9659258262890683122, 1.000000000000000000, 0.9659258262890683122, 1.000000000000000000, 0.9659258262890683122, 1.000000000000000000, 0.9659258262890683122, 1.000000000000000000, 0.9659258262890683122, 1.000000000000000000, 0.9659258262890683122, 1.000000000000000000, 0.9659258262890683122, 1.000000000000000000, 0.9659258262890683122, 1.000000000000000000, 0.9659258262890683122, 1.000000000000000000, 0.9659258262890683122, 1.000000000000000000, 0.9659258262890683122, 1.000000000000000000, 0.9659258262890683122, 1.000000000000000000, 0.9659258262890683122, 1.000000000000000000, 0.9659258262890683122, 1.000000000000000000, 0.9659258262890683122, 1.000000000000000000, 0.9659258262890683122, 1.000000000000000000, 0.9659258262890683122, 1.000000000000000000, 0.9659258262890683122, 1.000000000000000000, 0.9659258262890683122, 1.000000000000000000, 0.9659258262890683122, 1.000000000000000000, 0.9659258262890683122, 1.000000000000000000, 0.9659258262890683122, 1.000000000000000000, 0.9659258262890683122, 1.000000000000000000, 0.9659258262890683122, 1.000000000000000000, 0.9659258262890683122, 1.000000000000000000, 0.9659258262890683122, 1.000000000000000000, 0.9659258262890683122, 1.000000000000000000, 0.9659258262890683122, 1.000000000000000000, 0.9659258262890683122, 1.000000000000000000, 0.9659258262890683122, 1.000000000000000000, 0.9659258262890683122, 1.000000000000000000) ) ) 
 REPRESENTATION_ITEM ( '' )  SURFACE ( )  );
#62124 = CARTESIAN_POINT ( 'NONE',  ( 1.614173228346456712, 0.000000000000000000, 0.5309055118110233007 ) ) ;
#62125 = CARTESIAN_POINT ( 'NONE',  ( -0.8333333333333323711, 0.2952755905511811885, 0.1292274648535926551 ) ) ;
#62126 = CARTESIAN_POINT ( 'NONE',  ( 1.358267716535433323, 0.1660481256975885056, 0.3530559997133364547 ) ) ;
#62128 = CARTESIAN_POINT ( 'NONE',  ( -1.011202504342156416, -2.294479370626195693E-15, 0.3464511005275217603 ) ) ;
#62127 = DIRECTION ( 'NONE',  ( 1.000000000000000000, 0.000000000000000000, 0.000000000000000000 ) ) ;
#62129 = CARTESIAN_POINT ( 'NONE',  ( 1.450131233595801428, -0.6692913385826773087, -0.1292274648535924053 ) ) ;
#62130 = CARTESIAN_POINT ( 'NONE',  ( -0.8727034120734901146, -0.05778040916215560624, -0.4822834645669293319 ) ) ;
#62131 = CARTESIAN_POINT ( 'NONE',  ( 0.2867679344610365999, -0.2867679344610365999, -0.3359386894675047142 ) ) ;
#62132 = CARTESIAN_POINT ( 'NONE',  ( 0.07217847769028949700, -0.08942795157528024563, -0.3641732283464568787 ) ) ;
#62133 = CARTESIAN_POINT ( 'NONE',  ( 0.3917322834645670104, -0.1049643490035303273, -0.3536745406824148286 ) ) ;
#62134 = CARTESIAN_POINT ( 'NONE',  ( -0.1640419947506553400, -0.08942795157528024563, -0.3641732283464568787 ) ) ;
#62135 = CARTESIAN_POINT ( 'NONE',  ( 0.5249343832021003964, 0.1283753931104746893, -0.1820866141732285504 ) ) ;
#62136 = CARTESIAN_POINT ( 'NONE',  ( 0.6102362204724416372, -0.5400638737290844871, 0.3530559997133364547 ) ) ;
#62137 = VECTOR ( 'NONE', #15710, 39.37007874015748143 ) ;
#62138 = CARTESIAN_POINT ( 'NONE',  ( -0.8792650918635160906, -0.3690944881889763329, 0.3153832671262228327 ) ) ;
#62139 = CARTESIAN_POINT ( 'NONE',  ( 0.2867679344610365999, -0.2867679344610365444, -2.452755905511811108 ) ) ;
#62140 = CARTESIAN_POINT ( 'NONE',  ( 1.430446194225722500, 0.05413385826771666132, 0.4176697321401328100 ) ) ;
#62141 = CARTESIAN_POINT ( 'NONE',  ( -0.8727034120734901146, -0.3162353388693405765, 0.4822834645669290543 ) ) ;
#62142 = CARTESIAN_POINT ( 'NONE',  ( -0.1265901696524993347, 0.4724409448818895907, -0.7132545931758530466 ) ) ;
#62143 = CARTESIAN_POINT ( 'NONE',  ( -0.1181102362204717315, 0.2952755905511811885, 0.000000000000000000 ) ) ;
#62144 = CARTESIAN_POINT ( 'NONE',  ( -0.6758530183727028406, 0.2952755905511811885, 0.1292274648535926551 ) ) ;
#62145 = CARTESIAN_POINT ( 'NONE',  ( 1.305774278215223960, -0.5511811023622046335, 0.09757992244046803654 ) ) ;
#62146 = CARTESIAN_POINT ( 'NONE',  ( 0.1968503937007881344, 0.1771653543307087630, 0.000000000000000000 ) ) ;
#62147 = CARTESIAN_POINT ( 'NONE',  ( -0.3608923884514428360, -0.6692913385826773087, -0.1292274648535924053 ) ) ;
#62148 = CARTESIAN_POINT ( 'NONE',  ( -0.6627296587926501115, 0.2952755905511810774, -0.1292274648535930714 ) ) ;
#62149 = CARTESIAN_POINT ( 'NONE',  ( -3.842312626974349943, 2.753838553078471918, 0.5314960629921259283 ) ) ;
#62150 = CARTESIAN_POINT ( 'NONE',  ( 1.548556430446194954, 0.1283753931104746893, -0.1820866141732285504 ) ) ;
#62151 = CARTESIAN_POINT ( 'NONE',  ( 0.1443569553805781891, 0.05413385826771626580, -0.4176697321401330321 ) ) ;
#62152 = ORIENTED_EDGE ( 'NONE', *, *, #48287, .F. ) ;
#62153 = B_SPLINE_CURVE_WITH_KNOTS ( 'NONE', 3,
 ( #41814, #35096, #67097, #74241, #73829, #47711, #54863, #29196 ),
 .UNSPECIFIED., .F., .F.,
 ( 4, 2, 2, 4 ),
 ( 0.03770802486988160396, 0.04014025118898163075, 0.04135636434853164067, 0.04257247750808165060 ),
 .UNSPECIFIED. ) ;
#62154 = CARTESIAN_POINT ( 'NONE',  ( -0.1998031496062994405, 0.3460692066303957537, -1.979658792650918597 ) ) ;
#62155 = CARTESIAN_POINT ( 'NONE',  ( 1.089238845144357537, -0.4281496062992124485, 0.4176697321401328655 ) ) ;
#62156 = CARTESIAN_POINT ( 'NONE',  ( -0.5511811023622041894, -0.1870078740157480601, -0.3641732283464567677 ) ) ;
#62157 = CARTESIAN_POINT ( 'NONE',  ( -0.6824146981627291497, -0.6046776061558809534, -0.2411417322834644161 ) ) ;
#62158 = CARTESIAN_POINT ( 'NONE',  ( 1.364829396325460076, 0.2306618581243848609, 0.2411417322834645549 ) ) ;
#62159 = CARTESIAN_POINT ( 'NONE',  ( 0.7939632545931766261, -0.3162353388693409650, -0.4822834645669289433 ) ) ;
#62160 = CARTESIAN_POINT ( 'NONE',  ( 1.220472440944879056, 0.8346805926620878280, 0.5309055118110235227 ) ) ;
#62161 = CARTESIAN_POINT ( 'NONE',  ( -1.135170603674539924, -0.5511811023622046335, 0.09757992244046803654 ) ) ;
#62163 = EDGE_CURVE ( 'NONE', #49328, #47474, #36607, .T. ) ;
#62162 = CARTESIAN_POINT ( 'NONE',  ( 0.1998031496062994128, -0.3460692066303957537, -0.1686351706036745557 ) ) ;
#62164 = CARTESIAN_POINT ( 'NONE',  ( 0.1998031496062992740, 0.3460692066303959757, -0.6167979002624671692 ) ) ;
#62165 = CARTESIAN_POINT ( 'NONE',  ( 0.3949938075777411073, -0.1058382717557499464, 0.04593175853018367782 ) ) ;
#62166 = CARTESIAN_POINT ( 'NONE',  ( 1.450131233595801428, -0.5511811023622048555, -0.09757992244046775898 ) ) ;
#62167 = CARTESIAN_POINT ( 'NONE',  ( 0.5643044619422579178, -0.3690944881889765550, -0.3153832671262227771 ) ) ;
#62168 = CARTESIAN_POINT ( 'NONE',  ( 0.5577427821522314977, -0.3162353388693409650, -0.4822834645669289433 ) ) ;
#62169 = LINE ( 'NONE', #31829, #25111 ) ;
#62170 = CARTESIAN_POINT ( 'NONE',  ( 0.2891555358219910499, 0.2891555358219910499, -0.8444881889763782290 ) ) ;
#62171 = CARTESIAN_POINT ( 'NONE',  ( 0.8923884514435703741, 0.1283753931104748280, 0.1820866141732283561 ) ) ;
#62172 = CARTESIAN_POINT ( 'NONE',  ( -0.1902887139107604098, 0.2952755905511810774, -0.1292274648535930714 ) ) ;
#62173 = CARTESIAN_POINT ( 'NONE',  ( -0.8858267716535425107, -0.5400638737290844871, 0.3530559997133364547 ) ) ;
#62174 = CARTESIAN_POINT ( 'NONE',  ( 1.141732283464567788, -0.6692913385826771977, 8.415575281601705876E-17 ) ) ;
#62175 = B_SPLINE_CURVE_WITH_KNOTS ( 'NONE', 3,
 ( #46256, #19762, #77008, #58044 ),
 .UNSPECIFIED., .F., .F.,
 ( 4, 4 ),
 ( 3.210432057752138185E-07, 0.001287787053612062362 ),
 .UNSPECIFIED. ) ;
#62176 = CARTESIAN_POINT ( 'NONE',  ( 0.4091458600556404646, -0.2362204724409448231, -1.207349081364829324 ) ) ;
#62177 = CARTESIAN_POINT ( 'NONE',  ( 0.3460692066303959757, -0.1998031496062991907, -2.309711286089239035 ) ) ;
#62178 = CARTESIAN_POINT ( 'NONE',  ( 0.05249343832021075018, 0.1283753931104746893, -0.1820866141732285504 ) ) ;
#62179 = ORIENTED_EDGE ( 'NONE', *, *, #63459, .T. ) ;
#62180 = CARTESIAN_POINT ( 'NONE',  ( -0.3917322834645670659, -7.196005306013484475E-17, -0.9809904443907629945 ) ) ;
#62181 = VERTEX_POINT ( 'NONE', #68610 ) ;
#62182 = AXIS2_PLACEMENT_3D ( 'NONE', #72581, #633, #13680 ) ;
#62183 = CARTESIAN_POINT ( 'NONE',  ( -0.7349081364829390672, 0.2306618581243847221, -0.2411417322834647770 ) ) ;
#62184 = CARTESIAN_POINT ( 'NONE',  ( -0.1443569553805765515, -0.4281496062992127816, -0.4176697321401328100 ) ) ;
#62185 = CARTESIAN_POINT ( 'NONE',  ( -0.4461942257217840213, -0.6046776061558809534, -0.2411417322834644161 ) ) ;
#62186 = CARTESIAN_POINT ( 'NONE',  ( 0.3937007874015754361, -0.1870078740157479769, 0.4822834645669291653 ) ) ;
#62187 = CARTESIAN_POINT ( 'NONE',  ( -0.2821522309711278487, -0.6692913385826773087, -0.1292274648535924053 ) ) ;
#62188 = CARTESIAN_POINT ( 'NONE',  ( -1.423884514435694859, -0.05778040916215560624, -0.4822834645669293319 ) ) ;
#62189 = CARTESIAN_POINT ( 'NONE',  ( -0.9580052493438311334, -0.4281496062992124485, 0.4176697321401328655 ) ) ;
#62190 = CARTESIAN_POINT ( 'NONE',  ( 0.8530183727034126306, 0.05413385826771626580, -0.4176697321401330321 ) ) ;
#62191 = CARTESIAN_POINT ( 'NONE',  ( 0.6167979002624678353, -0.4281496062992124485, 0.4176697321401328655 ) ) ;
#62192 = CARTESIAN_POINT ( 'NONE',  ( 0.2867679344610365999, 0.2867679344610365999, -1.074803149606299080 ) ) ;
#62193 = CARTESIAN_POINT ( 'NONE',  ( -0.2690288713910754526, -0.5511811023622046335, 0.09757992244046803654 ) ) ;
#62194 = EDGE_LOOP ( 'NONE', ( #2799, #69330, #20922, #27802 ) ) ;
#62195 = CARTESIAN_POINT ( 'NONE',  ( -0.3949938075777409963, -7.255918531996591613E-17, -1.456692913385826627 ) ) ;
#62196 = VERTEX_POINT ( 'NONE', #31115 ) ;
#62197 = CARTESIAN_POINT ( 'NONE',  ( -1.292650918635170010, -0.5511811023622046335, 0.09757992244046803654 ) ) ;
#62198 = CARTESIAN_POINT ( 'NONE',  ( -0.3805774278215216522, 0.05413385826771666132, 0.4176697321401328100 ) ) ;
#62199 = CARTESIAN_POINT ( 'NONE',  ( 0.7763038905084337360, 2.575861430505332611E-15, -0.3954974714151464621 ) ) ;
#62200 = CARTESIAN_POINT ( 'NONE',  ( -0.7677165354330699465, 0.1660481256975885056, 0.3530559997133364547 ) ) ;
#62201 = CARTESIAN_POINT ( 'NONE',  ( -0.7874015748031489847, -0.1870078740157479769, 0.4822834645669291653 ) ) ;
#62202 = CARTESIAN_POINT ( 'NONE',  ( -1.502624671916009680, -0.3162353388693405765, 0.4822834645669290543 ) ) ;
#62203 = DIRECTION ( 'NONE',  ( 0.000000000000000000, 0.000000000000000000, 1.000000000000000000 ) ) ;
#62204 = CARTESIAN_POINT ( 'NONE',  ( 1.122047244094488860, -0.4536011799217368745, -0.2665933059059886201 ) ) ;
#62205 = CARTESIAN_POINT ( 'NONE',  ( -0.2362204724409447953, -0.4091458600556404646, -1.010498687664042050 ) ) ;
#62206 = CARTESIAN_POINT ( 'NONE',  ( -0.1049643490035307020, 0.3917322834645669549, 0.06627296587926499727 ) ) ;
#62207 = CARTESIAN_POINT ( 'NONE',  ( -0.07217847769028813698, -0.2845877964562161244, -0.3641732283464567121 ) ) ;
#62208 = CARTESIAN_POINT ( 'NONE',  ( -0.5183727034120726440, 0.2952755905511811885, 0.1292274648535926551 ) ) ;
#62209 = CARTESIAN_POINT ( 'NONE',  ( 3.923644508792730523, 1.190792352294606449, 0.3242919053828030584 ) ) ;
#62210 = CARTESIAN_POINT ( 'NONE',  ( -0.1115485564304453947, -0.6692913385826771977, 0.1292274648535927661 ) ) ;
#62211 = ORIENTED_EDGE ( 'NONE', *, *, #53641, .T. ) ;
#62212 = CARTESIAN_POINT ( 'NONE',  ( 0.1998031496062992740, 0.3460692066303959757, -2.034120734908136718 ) ) ;
#62213 = CARTESIAN_POINT ( 'NONE',  ( 0.2473181295769235899, 2.056812631849083806E-16, 0.3954985857520053605 ) ) ;
#62214 = ORIENTED_EDGE ( 'NONE', *, *, #52674, .T. ) ;
#62215 = CARTESIAN_POINT ( 'NONE',  ( 0.2925321140481932369, -0.2925321140481931814, -1.435039370078740051 ) ) ;
#62216 = CARTESIAN_POINT ( 'NONE',  ( -0.03087045868620141853, 0.3974833285012848716, -2.755905511811078679 ) ) ;
#62217 = CARTESIAN_POINT ( 'NONE',  ( -0.7349081364829390672, 0.1283753931104746893, -0.1820866141732285504 ) ) ;
#62218 = CARTESIAN_POINT ( 'NONE',  ( -1.174540682414697335, -0.3162353388693409650, -0.4822834645669289433 ) ) ;
#62219 = CARTESIAN_POINT ( 'NONE',  ( -0.3458507752293909498, 0.3458507752293907833, -0.3346456692913385988 ) ) ;
#62220 = CARTESIAN_POINT ( 'NONE',  ( -0.7233831536535466622, 2.176714048050540473, 0.5048085489443566720 ) ) ;
#62221 = CARTESIAN_POINT ( 'NONE',  ( 4.797336870675656522E-17, -0.3917322834645670104, -2.840551181102362044 ) ) ;
#62222 = CARTESIAN_POINT ( 'NONE',  ( 1.279527559055118724, -0.5400638737290845981, -0.3530559997133363437 ) ) ;
#62223 = CARTESIAN_POINT ( 'NONE',  ( 0.4068241469816279987, -0.4281496062992127816, -0.4176697321401328100 ) ) ;
#62224 = CARTESIAN_POINT ( 'NONE',  ( 0.5708661417322842269, 0.1660481256975885056, 0.3530559997133364547 ) ) ;
#62225 = CARTESIAN_POINT ( 'NONE',  ( -0.5511811023622038563, -0.1870078740157479769, 0.3641732283464567677 ) ) ;
#62226 = CARTESIAN_POINT ( 'NONE',  ( -0.4396325459317579898, 0.2952755905511811885, 0.1292274648535926551 ) ) ;
#62227 = CARTESIAN_POINT ( 'NONE',  ( -0.4724409448818895907, -0.1265901696524993070, -2.484908136482939955 ) ) ;
#62228 = CARTESIAN_POINT ( 'NONE',  ( -1.010498687664041384, -0.4281496062992127816, -0.4176697321401328100 ) ) ;
#62229 = CARTESIAN_POINT ( 'NONE',  ( -9.674558042662122972E-17, 0.3949938075777409963, -2.438976377952756014 ) ) ;
#62230 = CARTESIAN_POINT ( 'NONE',  ( 1.437007874015748810, 0.07958543189024085140, 0.2665933059059887866 ) ) ;
#62231 = CARTESIAN_POINT ( 'NONE',  ( -0.3937007874015740483, -0.1870078740157480601, -0.3641732283464567677 ) ) ;
#62232 = CONICAL_SURFACE ( 'NONE', #55488, 1.244489337948955221, 0.7853981633974452814 ) ;
#62233 = CARTESIAN_POINT ( 'NONE',  ( 1.286089238845145033, -0.5023911411419708095, -0.1820866141732282451 ) ) ;
#62234 = CARTESIAN_POINT ( 'NONE',  ( 1.607611548556431069, 0.1771653543307087630, 0.09757992244046791164 ) ) ;
#62235 = CARTESIAN_POINT ( 'NONE',  ( -1.122047244094487306, 0.07958543189024071263, -0.2665933059059888421 ) ) ;
#62236 = CARTESIAN_POINT ( 'NONE',  ( 1.594488188976378673, 0.1660481256975885056, 0.3530559997133364547 ) ) ;
#62237 = CARTESIAN_POINT ( 'NONE',  ( -1.332020997375327642, -0.3162353388693409650, -0.4822834645669289433 ) ) ;
#62238 = CARTESIAN_POINT ( 'NONE',  ( -0.2427821522309703550, -0.3162353388693405765, 0.4822834645669290543 ) ) ;
#62239 = CARTESIAN_POINT ( 'NONE',  ( 2.094141031014959520, 1.724409448818898127, 0.4359958488159723644 ) ) ;
#62240 = CARTESIAN_POINT ( 'NONE',  ( -0.2493438320209966919, -0.3690944881889763329, 0.3153832671262228327 ) ) ;
#62241 = CARTESIAN_POINT ( 'NONE',  ( -1.509186351706035767, -0.004921259842519870586, -0.3153832671262229437 ) ) ;
#62242 = CARTESIAN_POINT ( 'NONE',  ( 0.8858267716535438430, 0.1660481256975885056, 0.3530559997133364547 ) ) ;
#62243 = CARTESIAN_POINT ( 'NONE',  ( -1.476377952755905110, -0.4536011799217368745, -0.2665933059059886201 ) ) ;
#62244 = CONICAL_SURFACE ( 'NONE', #19208, 1.181102362204724310, 0.7853981633974621568 ) ;
#62245 = CARTESIAN_POINT ( 'NONE',  ( 1.220472440944882386, -0.5511811023622047445, 6.969142054262312111E-17 ) ) ;
#62246 = CARTESIAN_POINT ( 'NONE',  ( -0.9120734908136475250, 0.2952755905511811885, 0.1292274648535926551 ) ) ;
#62247 = CARTESIAN_POINT ( 'NONE',  ( -0.3674540682414689785, 0.1283753931104748280, 0.1820866141732283561 ) ) ;
#62248 = CARTESIAN_POINT ( 'NONE',  ( 0.3372635250547070807, 0.3676148930005934123, -0.006554863637384360751 ) ) ;
#62249 = CARTESIAN_POINT ( 'NONE',  ( 0.09842519685039434474, -0.4536011799217368745, -0.2665933059059886201 ) ) ;
#62250 = CARTESIAN_POINT ( 'NONE',  ( -0.2821522309711278487, -0.6692913385826773087, -0.1292274648535924053 ) ) ;
#62251 = CARTESIAN_POINT ( 'NONE',  ( -0.1998031496062994405, 0.3460692066303957537, -0.8772965879265091083 ) ) ;
#62252 = EDGE_CURVE ( 'NONE', #38980, #55534, #12805, .T. ) ;
#62253 = CARTESIAN_POINT ( 'NONE',  ( 0.3917322834645669549, 0.1049643490035304660, -2.099081364829396446 ) ) ;
#62254 = CARTESIAN_POINT ( 'NONE',  ( 0.4921259842519691285, 0.07958543189024085140, 0.2665933059059887866 ) ) ;
#62255 = CARTESIAN_POINT ( 'NONE',  ( -0.2230971128608915943, 0.05413385826771666132, 0.4176697321401328100 ) ) ;
#62256 = CARTESIAN_POINT ( 'NONE',  ( -0.5905511811023613777, -0.6692913385826771977, 8.415575281601705876E-17 ) ) ;
#62257 = CARTESIAN_POINT ( 'NONE',  ( -0.8530183727034112984, -0.004921259842519576551, 0.3153832671262227771 ) ) ;
#62258 = CARTESIAN_POINT ( 'NONE',  ( 4.893765752498283924E-17, -0.3996062992125986035, -2.755905511811023612 ) ) ;
#62259 = CARTESIAN_POINT ( 'NONE',  ( -0.5971128608923877978, -0.5511811023622048555, -0.09757992244046775898 ) ) ;
#62260 = CARTESIAN_POINT ( 'NONE',  ( -0.1377952755905504645, -0.5400638737290845981, -0.3530559997133363437 ) ) ;
#62261 = CARTESIAN_POINT ( 'NONE',  ( -1.089238845144356427, -0.004921259842519576551, 0.3153832671262227771 ) ) ;
#62262 = CARTESIAN_POINT ( 'NONE',  ( -1.482939632545930975, 0.05413385826771666132, 0.4176697321401328100 ) ) ;
#62263 = CARTESIAN_POINT ( 'NONE',  ( 0.4613432605871740089, 1.990046790791744833E-15, -0.3954974714151458515 ) ) ;
#62264 = ORIENTED_EDGE ( 'NONE', *, *, #47242, .T. ) ;
#62265 = CARTESIAN_POINT ( 'NONE',  ( -1.522309711286088607, 0.1283753931104746893, -0.1820866141732285504 ) ) ;
#62266 = CARTESIAN_POINT ( 'NONE',  ( -0.4133858267716528645, 0.1660481256975883668, -0.3530559997133364547 ) ) ;
#62267 = CARTESIAN_POINT ( 'NONE',  ( -1.010498687664041384, 0.05413385826771666132, 0.4176697321401328100 ) ) ;
#62268 = CARTESIAN_POINT ( 'NONE',  ( 0.3917322834645669549, 0.1049643490035304660, -1.469160104986876769 ) ) ;
#62269 = CARTESIAN_POINT ( 'NONE',  ( -0.2798680777847367684, 0.2749078412854674691, -1.220472440944882164 ) ) ;
#62270 = CARTESIAN_POINT ( 'NONE',  ( 0.9580052493438327987, -0.4281496062992127816, -0.4176697321401328100 ) ) ;
#62271 = CARTESIAN_POINT ( 'NONE',  ( 0.5183727034120741983, -0.6692913385826771977, 0.1292274648535927661 ) ) ;
#62272 = CARTESIAN_POINT ( 'NONE',  ( 0.1265901696524989184, 0.4724409448818898127, -0.4658792650918635037 ) ) ;
#62273 = CARTESIAN_POINT ( 'NONE',  ( -0.2925321140481930149, -0.2925321140481933480, -2.498031496062992574 ) ) ;
#62274 = CARTESIAN_POINT ( 'NONE',  ( 0.9842519685039375910, 0.1771653543307087630, 0.000000000000000000 ) ) ;
#62275 = CARTESIAN_POINT ( 'NONE',  ( 0.1998031496062994405, -0.3460692066303958092, -0.7217847769028871152 ) ) ;
#62276 = EDGE_LOOP ( 'NONE', ( #78479, #1041, #1228, #11798 ) ) ;
#62277 = CARTESIAN_POINT ( 'NONE',  ( -0.8136482939632537770, 0.1283753931104746893, -0.1820866141732285504 ) ) ;
#62278 = CARTESIAN_POINT ( 'NONE',  ( 0.2867679344610365999, -0.2867679344610365444, -2.610236220472441193 ) ) ;
#62279 = ORIENTED_EDGE ( 'NONE', *, *, #12089, .F. ) ;
#62280 = CARTESIAN_POINT ( 'NONE',  ( 0.4002624671916016896, -0.3162353388693409650, -0.4822834645669289433 ) ) ;
#62281 = CARTESIAN_POINT ( 'NONE',  ( -0.3149606299212590610, -0.1870078740157479769, 0.4822834645669291653 ) ) ;
#62282 = CARTESIAN_POINT ( 'NONE',  ( -1.259842519685038686, -0.1870078740157480879, -0.4822834645669291653 ) ) ;
#62283 = CARTESIAN_POINT ( 'NONE',  ( 0.9251968503937015864, 0.1660481256975883668, -0.3530559997133364547 ) ) ;
#62284 = VECTOR ( 'NONE', #47030, 39.37007874015748143 ) ;
#62285 = CARTESIAN_POINT ( 'NONE',  ( -1.456692913385826182, 0.1771653543307087630, 0.000000000000000000 ) ) ;
#62286 = DIRECTION ( 'NONE',  ( 0.000000000000000000, 0.000000000000000000, -1.000000000000000000 ) ) ;
#62287 = CARTESIAN_POINT ( 'NONE',  ( -0.09842519685039295696, -0.5400638737290844871, 0.3530559997133364547 ) ) ;
#62288 = CARTESIAN_POINT ( 'NONE',  ( -1.305774278215222184, 0.2952755905511811885, 0.1292274648535926551 ) ) ;
#62289 = CARTESIAN_POINT ( 'NONE',  ( 0.3392501089628018329, -0.1958661417322834497, -1.917303518863830103 ) ) ;
#62290 = DIRECTION ( 'NONE',  ( -0.8660254037844432595, 0.000000000000000000, 0.4999999999999918954 ) ) ;
#62291 = CARTESIAN_POINT ( 'NONE',  ( 1.572991167713778227, 1.535433070866141447, -0.1227090857360983167 ) ) ;
#62292 = CARTESIAN_POINT ( 'NONE',  ( 0.3917322834645669549, 0.1049643490035304660, 0.04068241469816277767 ) ) ;
#62293 = CARTESIAN_POINT ( 'NONE',  ( 0.7874015748031503170, -0.1870078740157480601, -0.3641732283464567677 ) ) ;
#62294 = ORIENTED_EDGE ( 'NONE', *, *, #33188, .T. ) ;
#62295 = CARTESIAN_POINT ( 'NONE',  ( 0.1974969037888704704, 0.3420746716998660508, -0.3018372703412073865 ) ) ;
#62296 = CARTESIAN_POINT ( 'NONE',  ( -1.017060367454067249, -0.05778040916215522460, 0.4822834645669289988 ) ) ;
#62297 = ORIENTED_EDGE ( 'NONE', *, *, #80383, .T. ) ;
#62298 = CARTESIAN_POINT ( 'NONE',  ( -0.006561679790025524116, -0.2845877964562159024, 0.3641732283464567677 ) ) ;
#62299 = CARTESIAN_POINT ( 'NONE',  ( -1.463254593175852492, -0.6692913385826773087, -0.1292274648535924053 ) ) ;
#62300 = CARTESIAN_POINT ( 'NONE',  ( 0.3937007874015754361, -0.1870078740157480879, -0.4822834645669291653 ) ) ;
#62301 = CARTESIAN_POINT ( 'NONE',  ( 0.6233595800524939223, -0.3162353388693405765, 0.4822834645669290543 ) ) ;
#62302 = CARTESIAN_POINT ( 'NONE',  ( -0.6036745406824141069, 0.2306618581243848609, 0.2411417322834645549 ) ) ;
#62303 = CARTESIAN_POINT ( 'NONE',  ( -0.1958661417322833942, -0.3392501089628018884, -1.164717478511497983 ) ) ;
#62304 = CARTESIAN_POINT ( 'NONE',  ( -0.6496062992125976043, 0.1660481256975883668, -0.3530559997133364547 ) ) ;
#62305 = CARTESIAN_POINT ( 'NONE',  ( 0.3917322834645670104, 2.398668435337828261E-17, -2.564960629921259727 ) ) ;
#62306 = CARTESIAN_POINT ( 'NONE',  ( 1.305774278215223960, 0.1771653543307087075, -0.09757992244046823083 ) ) ;
#62307 = CARTESIAN_POINT ( 'NONE',  ( -0.8530183727034112984, 0.05413385826771666132, 0.4176697321401328100 ) ) ;
#62308 = CARTESIAN_POINT ( 'NONE',  ( 0.9317585301837276734, 0.05413385826771626580, -0.4176697321401330321 ) ) ;
#62309 = CARTESIAN_POINT ( 'NONE',  ( 1.227034120734908917, 0.2952755905511810774, -0.1292274648535930714 ) ) ;
#62310 = CARTESIAN_POINT ( 'NONE',  ( -0.2925321140481932924, 0.2925321140481931814, -0.9645669291338579976 ) ) ;
#62311 = CARTESIAN_POINT ( 'NONE',  ( -1.417322834645668772, -0.1870078740157479769, 0.4822834645669291653 ) ) ;
#62312 = CARTESIAN_POINT ( 'NONE',  ( 0.3996062992125984925, 0.1070741851644054637, -0.3589238845144357426 ) ) ;
#62313 = CARTESIAN_POINT ( 'NONE',  ( 0.3215223097112867578, -0.05778040916215522460, 0.4822834645669289988 ) ) ;
#62314 = CARTESIAN_POINT ( 'NONE',  ( -0.2925321140481930704, -0.2925321140481933480, -2.421259842519684735 ) ) ;
#62315 = CARTESIAN_POINT ( 'NONE',  ( -1.574803149606298192, -0.1870078740157480601, -0.3641732283464567677 ) ) ;
#62316 = CARTESIAN_POINT ( 'NONE',  ( 0.6627296587926517768, -0.5511811023622048555, -0.09757992244046775898 ) ) ;
#62317 = CARTESIAN_POINT ( 'NONE',  ( 0.7874015748031503170, -0.1870078740157479769, 0.4822834645669291653 ) ) ;
#62318 = CARTESIAN_POINT ( 'NONE',  ( 0.3458507752293908943, -0.3458507752293908943, -1.277559055118109965 ) ) ;
#62319 = CARTESIAN_POINT ( 'NONE',  ( 0.7545931758530189937, 0.1771653543307087075, -0.09757992244046823083 ) ) ;
#62320 = CARTESIAN_POINT ( 'NONE',  ( 0.8989501312335963501, -0.6692913385826773087, -0.1292274648535924053 ) ) ;
#62321 = CARTESIAN_POINT ( 'NONE',  ( -0.1058382717557497660, -0.3949938075777411073, -0.9363517060367456679 ) ) ;
#62322 = CARTESIAN_POINT ( 'NONE',  ( -0.8595800524934373854, -0.3162353388693409650, -0.4822834645669289433 ) ) ;
#62323 = CARTESIAN_POINT ( 'NONE',  ( 0.4744094488189113945, 1.537401574803149984, -3.937007874015760578 ) ) ;
#62324 = CARTESIAN_POINT ( 'NONE',  ( 1.043307086614173818, -0.4536011799217368745, -0.2665933059059886201 ) ) ;
#62325 = CARTESIAN_POINT ( 'NONE',  ( -0.4724409448818890911, -0.1870078740157479769, 0.4822834645669291653 ) ) ;
#62326 = CARTESIAN_POINT ( 'NONE',  ( -0.05249343832020938322, -0.6046776061558809534, -0.2411417322834644161 ) ) ;
#62327 = DIRECTION ( 'NONE',  ( -0.000000000000000000, -1.000000000000000000, -0.000000000000000000 ) ) ;
#62328 = CARTESIAN_POINT ( 'NONE',  ( -0.4855643044619415427, -0.4281496062992124485, 0.4176697321401328655 ) ) ;
#62329 = CARTESIAN_POINT ( 'NONE',  ( 0.2755905511811031494, 0.1771653543307087630, 0.000000000000000000 ) ) ;
#62330 = CARTESIAN_POINT ( 'NONE',  ( -2.777177547361640908, 1.169463170161808785, -0.3010181502270431464 ) ) ;
#62331 = CARTESIAN_POINT ( 'NONE',  ( 0.1837270341207357105, -0.5023911411419708095, -0.1820866141732282451 ) ) ;
#62332 = CARTESIAN_POINT ( 'NONE',  ( 0.9186351706036751663, -0.5023911411419708095, 0.1820866141732285504 ) ) ;
#62333 = CARTESIAN_POINT ( 'NONE',  ( -0.04537753515110386909, 1.065137975676527349, -1.631395471344458503 ) ) ;
#62334 = CARTESIAN_POINT ( 'NONE',  ( 0.2925321140481932369, -0.2925321140481931814, -1.750000000000000222 ) ) ;
#62335 = CARTESIAN_POINT ( 'NONE',  ( 0.3543307086614181922, -0.6692913385826771977, 8.415575281601705876E-17 ) ) ;
#62336 = CARTESIAN_POINT ( 'NONE',  ( 0.3917322834645670104, 2.398668435337828261E-17, -1.370078740157480324 ) ) ;
#62337 = CARTESIAN_POINT ( 'NONE',  ( 0.2238009295390077091, 2.409604939980833412E-17, -0.3464511005275205946 ) ) ;
#62338 = CARTESIAN_POINT ( 'NONE',  ( 0.2230971128608929543, 0.05413385826771626580, -0.4176697321401330321 ) ) ;
#62339 = CARTESIAN_POINT ( 'NONE',  ( -0.2296587926509179312, -0.2845877964562161244, -0.3641732283464567121 ) ) ;
#62340 = CARTESIAN_POINT ( 'NONE',  ( -0.1443569553805768291, -0.004921259842519576551, 0.3153832671262227771 ) ) ;
#62341 = CARTESIAN_POINT ( 'NONE',  ( -0.3346456692913377662, 0.1660481256975883668, -0.3530559997133364547 ) ) ;
#62342 = CARTESIAN_POINT ( 'NONE',  ( 0.8989501312335964611, 0.1771653543307087630, 0.09757992244046791164 ) ) ;
#62343 = CARTESIAN_POINT ( 'NONE',  ( -1.660104986876639543, -0.08942795157528024563, -0.3641732283464568787 ) ) ;
#62344 = CARTESIAN_POINT ( 'NONE',  ( 1.305774278215223960, 0.1771653543307087075, -0.09757992244046823083 ) ) ;
#62345 = CIRCLE ( 'NONE', #74504, 2.598425196850393970 ) ;
#62346 = CARTESIAN_POINT ( 'NONE',  ( 0.2099737532808405305, -0.6046776061558807314, 0.2411417322834647770 ) ) ;
#62347 = CARTESIAN_POINT ( 'NONE',  ( 1.154855643044620184, -0.6046776061558807314, 0.2411417322834647770 ) ) ;
#62348 = FACE_OUTER_BOUND ( 'NONE', #19012, .T. ) ;
#62349 = CARTESIAN_POINT ( 'NONE',  ( 0.02624671916010564918, 0.2306618581243848609, 0.2411417322834645549 ) ) ;
#62350 = CARTESIAN_POINT ( 'NONE',  ( 1.286089238845145033, -0.6046776061558809534, -0.2411417322834644161 ) ) ;
#62351 = CARTESIAN_POINT ( 'NONE',  ( 0.5971128608923891301, 0.2952755905511810774, -0.1292274648535930714 ) ) ;
#62352 = CARTESIAN_POINT ( 'NONE',  ( 0.3983403474834781299, 0.03178304480585100733, -1.929133858267716661 ) ) ;
#62353 = CARTESIAN_POINT ( 'NONE',  ( 0.7808398950131241190, -0.08942795157528024563, -0.3641732283464568787 ) ) ;
#62354 = CARTESIAN_POINT ( 'NONE',  ( 1.122047244094488860, -0.5400638737290845981, -0.3530559997133363437 ) ) ;
#62355 = CARTESIAN_POINT ( 'NONE',  ( 5.463695987328526437E-16, -0.1870078740157479769, 0.3641732283464567677 ) ) ;
#62356 = AXIS2_PLACEMENT_3D ( 'NONE', #3481, #16121, #28735 ) ;
#62357 = CARTESIAN_POINT ( 'NONE',  ( -0.1837270341207340729, 0.2306618581243847221, -0.2411417322834647770 ) ) ;
#62358 = CARTESIAN_POINT ( 'NONE',  ( 0.3608923884514443348, 0.2952755905511810774, -0.1292274648535930714 ) ) ;
#62359 = CARTESIAN_POINT ( 'NONE',  ( -0.7020997375328074108, -0.05778040916215522460, 0.4822834645669289988 ) ) ;
#62360 = CARTESIAN_POINT ( 'NONE',  ( -0.3805774278215216522, -0.3690944881889765550, -0.3153832671262227771 ) ) ;
#62361 = CARTESIAN_POINT ( 'NONE',  ( 0.7152230971128614723, -0.3162353388693409650, -0.4822834645669289433 ) ) ;
#62362 = CARTESIAN_POINT ( 'NONE',  ( 0.9776902887139113929, -0.5511811023622048555, -0.09757992244046775898 ) ) ;
#62363 = CARTESIAN_POINT ( 'NONE',  ( 0.2624671916010504757, 0.2306618581243848609, 0.2411417322834645549 ) ) ;
#62364 = LINE ( 'NONE', #23238, #24515 ) ;
#62366 = CARTESIAN_POINT ( 'NONE',  ( 4.893765752498283924E-17, -0.3996062992125986035, -1.181102362204724310 ) ) ;
#62365 = CARTESIAN_POINT ( 'NONE',  ( -1.033630966599879297, -2.567464376874931580E-15, -0.4445507791589072832 ) ) ;
#62367 = CARTESIAN_POINT ( 'NONE',  ( 1.528871391076116026, 0.2952755905511811885, 0.1292274648535926551 ) ) ;
#62368 = CARTESIAN_POINT ( 'NONE',  ( 0.1049643490035303689, 0.3917322834645670104, -2.032808398950130879 ) ) ;
#62369 = CARTESIAN_POINT ( 'NONE',  ( -1.200787401574802349, -0.5400638737290844871, 0.3530559997133364547 ) ) ;
#62370 = CARTESIAN_POINT ( 'NONE',  ( -0.4986876640419942164, -0.6046776061558807314, 0.2411417322834647770 ) ) ;
#62371 = CARTESIAN_POINT ( 'NONE',  ( -0.3458507752293906723, -0.3458507752293910609, -0.5314960629921260393 ) ) ;
#62372 = CARTESIAN_POINT ( 'NONE',  ( -0.3949938075777409408, -0.1058382717557502933, -2.880577427821522374 ) ) ;
#62373 = EDGE_LOOP ( 'NONE', ( #27548, #24229, #2697, #23339 ) ) ;
#62374 = CARTESIAN_POINT ( 'NONE',  ( 0.1902887139107617975, -0.5511811023622048555, -0.09757992244046775898 ) ) ;
#62375 = CARTESIAN_POINT ( 'NONE',  ( 0.1958661417322836440, -0.3392501089628017219, -1.343832020997375531 ) ) ;
#62376 = CARTESIAN_POINT ( 'NONE',  ( 0.7939632545931766261, -0.05778040916215522460, 0.4822834645669289988 ) ) ;
#62377 = CARTESIAN_POINT ( 'NONE',  ( 0.4724409448818896462, 0.1265901696524990294, -2.644356955380577912 ) ) ;
#62378 = CARTESIAN_POINT ( 'NONE',  ( -0.3129921259842521897, 1.496062992125984259, 0.000000000000000000 ) ) ;
#62379 = FACE_OUTER_BOUND ( 'NONE', #22873, .T. ) ;
#62380 = CARTESIAN_POINT ( 'NONE',  ( 1.049868766404200349, 0.2306618581243848609, 0.2411417322834645549 ) ) ;
#62381 = ADVANCED_FACE ( 'NONE', ( #24391 ), #56130, .F. ) ;
#62382 = CARTESIAN_POINT ( 'NONE',  ( 1.240157480314961314, -0.4536011799217367080, 0.2665933059059888421 ) ) ;
#62383 = CARTESIAN_POINT ( 'NONE',  ( -0.01312335958005186876, 0.05413385826771626580, -0.4176697321401330321 ) ) ;
#62384 = CARTESIAN_POINT ( 'NONE',  ( 0.1049643490035303689, 0.3917322834645668994, -0.7033927577089746919 ) ) ;
#62385 = CARTESIAN_POINT ( 'NONE',  ( -0.2821522309711278487, -0.6692913385826773087, -0.1292274648535924053 ) ) ;
#62386 = CARTESIAN_POINT ( 'NONE',  ( -1.108923884514435132, -0.2845877964562159024, 0.3641732283464567677 ) ) ;
#62387 = CARTESIAN_POINT ( 'NONE',  ( 0.5577427821522314977, -0.3162353388693409650, -0.4822834645669289433 ) ) ;
#62389 = ADVANCED_FACE ( 'NONE', ( #56783 ), #75343, .T. ) ;
#62388 = CARTESIAN_POINT ( 'NONE',  ( -0.6627296587926503335, -0.6692913385826771977, 0.1292274648535927661 ) ) ;
#62390 = CARTESIAN_POINT ( 'NONE',  ( 0.000000000000000000, 0.000000000000000000, -2.755905511811024056 ) ) ;
#62391 = DIRECTION ( 'NONE',  ( -0.000000000000000000, -1.000000000000000000, -0.000000000000000000 ) ) ;
#62392 = ORIENTED_EDGE ( 'NONE', *, *, #66038, .F. ) ;
#62393 = CARTESIAN_POINT ( 'NONE',  ( 0.1049643490035303967, 0.3917322834645670659, -2.037420890584989319 ) ) ;
#62394 = CARTESIAN_POINT ( 'NONE',  ( 0.3871391076115493490, -0.3162353388693405765, 0.4822834645669290543 ) ) ;
#62395 = CARTESIAN_POINT ( 'NONE',  ( -0.3149606299212590610, -0.1870078740157479769, 0.4822834645669291653 ) ) ;
#62396 = CARTESIAN_POINT ( 'NONE',  ( -1.450131233595799651, 0.2952755905511810774, -0.1292274648535930714 ) ) ;
#62397 = CARTESIAN_POINT ( 'NONE',  ( 0.9251968503937015864, -0.5400638737290844871, 0.3530559997133364547 ) ) ;
#62398 = CARTESIAN_POINT ( 'NONE',  ( 0.6233595800524942554, -0.05778040916215560624, -0.4822834645669293319 ) ) ;
#62399 = CARTESIAN_POINT ( 'NONE',  ( 0.1049643490035304938, -0.3917322834645669549, -1.272309711286089273 ) ) ;
#62400 = CARTESIAN_POINT ( 'NONE',  ( -0.9580052493438311334, -0.4281496062992124485, 0.4176697321401328655 ) ) ;
#62401 = CARTESIAN_POINT ( 'NONE',  ( 0.2952755905511819101, 0.1660481256975883668, -0.3530559997133364547 ) ) ;
#62402 = CARTESIAN_POINT ( 'NONE',  ( -0.3280839895013117347, 0.05413385826771626580, -0.4176697321401330321 ) ) ;
#62403 = CARTESIAN_POINT ( 'NONE',  ( 0.2230971128608932319, -0.3690944881889763329, 0.3153832671262228327 ) ) ;
#62404 = CARTESIAN_POINT ( 'NONE',  ( 1.692913385826772421, 0.1771653543307087630, 0.000000000000000000 ) ) ;
#62405 = CARTESIAN_POINT ( 'NONE',  ( -0.2362186021731760566, -0.1771678480211530127, 5.713829339669470819 ) ) ;
#62406 = CARTESIAN_POINT ( 'NONE',  ( 0.4396325459317590445, -0.6692913385826771977, 0.1292274648535927661 ) ) ;
#62407 = DIRECTION ( 'NONE',  ( -0.000000000000000000, 1.000000000000000000, -0.000000000000000000 ) ) ;
#62408 = CARTESIAN_POINT ( 'NONE',  ( 1.410761154855643795, -0.3162353388693405765, 0.4822834645669290543 ) ) ;
#62409 = CARTESIAN_POINT ( 'NONE',  ( 0.3392501089628018329, 0.1958661417322835607, -2.800524934383201714 ) ) ;
#62410 = ORIENTED_EDGE ( 'NONE', *, *, #43225, .T. ) ;
#62411 = ADVANCED_FACE ( 'NONE', ( #43732 ), #42510, .F. ) ;
#62412 = VERTEX_POINT ( 'NONE', #48826 ) ;
#62413 = CARTESIAN_POINT ( 'NONE',  ( 0.6102362204724416372, 0.1660481256975883668, -0.3530559997133364547 ) ) ;
#62414 = CARTESIAN_POINT ( 'NONE',  ( 0.2559055118110243332, -0.4536011799217368745, -0.2665933059059886201 ) ) ;
#62416 = FACE_OUTER_BOUND ( 'NONE', #43626, .T. ) ;
#62415 = DIRECTION ( 'NONE',  ( -1.000000000000000000, 0.000000000000000000, -0.000000000000000000 ) ) ;
#62417 = CARTESIAN_POINT ( 'NONE',  ( -0.2867679344610364334, -0.2867679344610367109, -0.7736220472440945573 ) ) ;
#62418 = CARTESIAN_POINT ( 'NONE',  ( 3.886287458032462006, 2.165354330708662012, 0.6299212598425202314 ) ) ;
#62419 =( LENGTH_UNIT ( ) NAMED_UNIT ( * ) SI_UNIT ( $, .METRE. ) );
#62420 = CIRCLE ( 'NONE', #73191, 0.1181102362204724116 ) ;
#62421 = CARTESIAN_POINT ( 'NONE',  ( -0.1998031496062994405, 0.3460692066303957537, -2.294619422572178102 ) ) ;
#62422 = CARTESIAN_POINT ( 'NONE',  ( 0.4855643044619428750, 0.05413385826771666132, 0.4176697321401328100 ) ) ;
#62423 = CARTESIAN_POINT ( 'NONE',  ( -1.253280839895012377, -0.3162353388693409650, -0.4822834645669289433 ) ) ;
#62424 = CARTESIAN_POINT ( 'NONE',  ( -1.049868766404198794, 0.2306618581243847221, -0.2411417322834647770 ) ) ;
#62425 = CARTESIAN_POINT ( 'NONE',  ( 0.5577427821522314977, -0.3162353388693409650, -0.4822834645669289433 ) ) ;
#62426 = CARTESIAN_POINT ( 'NONE',  ( 1.325459317585302665, 0.05413385826771626580, -0.4176697321401330321 ) ) ;
#62427 = CARTESIAN_POINT ( 'NONE',  ( 1.410761154855643795, -0.08942795157528024563, -0.3641732283464568787 ) ) ;
#62428 = CARTESIAN_POINT ( 'NONE',  ( 1.082677165354331228, 0.07958543189024071263, -0.2665933059059888421 ) ) ;
#62429 = CARTESIAN_POINT ( 'NONE',  ( -0.6627296587926501115, 0.2952755905511810774, -0.1292274648535930714 ) ) ;
#62430 = CARTESIAN_POINT ( 'NONE',  ( 0.3460692066303959202, -0.1998031496062991630, -0.3392388451443569819 ) ) ;
#62431 = CARTESIAN_POINT ( 'NONE',  ( 1.410761154855643795, -0.05778040916215560624, -0.4822834645669293319 ) ) ;
#62432 =( BOUNDED_CURVE ( )  B_SPLINE_CURVE ( 2, ( #5645, #82270, #24588, #51069, #70443, #12801, #168, #69631, #68805, #75953, #37226, #38042, #11976 ),
 .UNSPECIFIED., .F., .F. ) 
 B_SPLINE_CURVE_WITH_KNOTS ( ( 3, 2, 2, 2, 2, 2, 3 ),
 ( 0.8375000000000000222, 0.8416666666666666741, 0.8458333333333333259, 0.8499999999999999778, 0.8541666666666666297, 0.8583333333333332815, 0.8625000000000000444 ),
 .UNSPECIFIED. ) 
 CURVE ( )  GEOMETRIC_REPRESENTATION_ITEM ( )  RATIONAL_B_SPLINE_CURVE ( ( 1.000000000000000000, 0.9659258262890683122, 1.000000000000000000, 0.9659258262890683122, 1.000000000000000000, 0.9659258262890683122, 1.000000000000000000, 0.9659258262890683122, 1.000000000000000000, 0.9659258262890683122, 1.000000000000000000, 0.9659258262890683122, 1.000000000000000000 ) ) 
 REPRESENTATION_ITEM ( '' )  );
#62433 = CARTESIAN_POINT ( 'NONE',  ( -0.1049643490035307020, 0.3917322834645669549, -0.3136482939632545541 ) ) ;
#62434 = CARTESIAN_POINT ( 'NONE',  ( -0.4199475065616791736, -0.6046776061558807314, 0.2411417322834647770 ) ) ;
#62436 = CARTESIAN_POINT ( 'NONE',  ( -0.7137454485294953965, 2.793565526369265584, 0.4917280318828574082 ) ) ;
#62435 = CARTESIAN_POINT ( 'NONE',  ( 0.9711286089238851948, -0.6046776061558809534, -0.2411417322834644161 ) ) ;
#62437 = CARTESIAN_POINT ( 'NONE',  ( -1.010498687664041384, -0.3690944881889765550, -0.3153832671262227771 ) ) ;
#62438 = CARTESIAN_POINT ( 'NONE',  ( 0.4002624671916016896, -0.05778040916215522460, 0.4822834645669289988 ) ) ;
#62439 = CARTESIAN_POINT ( 'NONE',  ( 0.9055118110236227702, -0.5511811023622047445, 6.969142054262312111E-17 ) ) ;
#62440 = CARTESIAN_POINT ( 'NONE',  ( -0.2867679344610366554, 0.2867679344610365444, -1.517041051672229024 ) ) ;
#62441 = B_SPLINE_CURVE_WITH_KNOTS ( 'NONE', 3,
 ( #32522, #57767, #6852, #19907, #27463, #53121, #72505, #45134, #71253, #7275, #39679, #7706 ),
 .UNSPECIFIED., .F., .F.,
 ( 4, 2, 2, 2, 2, 4 ),
 ( 0.007992874908875454570, 0.009303755029337567456, 0.01061463514979968034, 0.01192551527026179323, 0.01258095533049286008, 0.01323639539072392693 ),
 .UNSPECIFIED. ) ;
#62442 = CARTESIAN_POINT ( 'NONE',  ( -1.410761154855642463, -0.08942795157527998196, 0.3641732283464567121 ) ) ;
#62443 = CARTESIAN_POINT ( 'NONE',  ( 0.8398950131233602345, -0.6046776061558807314, 0.2411417322834647770 ) ) ;
#62444 = DIRECTION ( 'NONE',  ( 0.000000000000000000, 0.000000000000000000, -1.000000000000000000 ) ) ;
#62445 = CARTESIAN_POINT ( 'NONE',  ( -0.5052493438320203589, -0.5511811023622046335, 0.09757992244046803654 ) ) ;
#62446 = CARTESIAN_POINT ( 'NONE',  ( -0.2296587926509179312, -0.3162353388693409650, -0.4822834645669289433 ) ) ;
#62447 = CARTESIAN_POINT ( 'NONE',  ( -1.181102362204723644, -0.1870078740157479769, 0.3641732283464567677 ) ) ;
#62448 = CARTESIAN_POINT ( 'NONE',  ( -0.5708661417322828946, 0.1660481256975883668, -0.3530559997133364547 ) ) ;
#62449 = CARTESIAN_POINT ( 'NONE',  ( 1.213910761154856299, 0.2952755905511811885, 0.1292274648535926551 ) ) ;
#62450 = CARTESIAN_POINT ( 'NONE',  ( -0.3392501089628017219, -0.1958661417322836995, -0.8366334890101857491 ) ) ;
#62451 = CARTESIAN_POINT ( 'NONE',  ( -0.8595800524934373854, -0.08942795157527998196, 0.3641732283464567121 ) ) ;
#62452 = CARTESIAN_POINT ( 'NONE',  ( 2.571961977011526290, 1.622068519643039330, 0.4668652553835664909 ) ) ;
#62453 = CARTESIAN_POINT ( 'NONE',  ( 1.358267716535433323, -0.5400638737290845981, -0.3530559997133363437 ) ) ;
#62454 = CARTESIAN_POINT ( 'NONE',  ( 0.4724409448818898682, 2.892866454678787531E-17, -2.242125984251968518 ) ) ;
#62455 = CARTESIAN_POINT ( 'NONE',  ( -1.371391076115484831, 0.2952755905511810774, -0.1292274648535930714 ) ) ;
#62457 = ADVANCED_FACE ( 'NONE', ( #55544 ), #11789, .T. ) ;
#62456 = CARTESIAN_POINT ( 'NONE',  ( -1.482939632545930975, -0.004921259842519576551, 0.3153832671262227771 ) ) ;
#62458 = CARTESIAN_POINT ( 'NONE',  ( -0.5708661417322828946, 0.07958543189024071263, -0.2665933059059888421 ) ) ;
#62459 = CARTESIAN_POINT ( 'NONE',  ( 0.7993346172249373716, 1.763362281772084768E-16, 0.3627985898453514602 ) ) ;
#62460 = CARTESIAN_POINT ( 'NONE',  ( -0.3805774278215216522, 0.05413385826771666132, 0.4176697321401328100 ) ) ;
#62461 = CARTESIAN_POINT ( 'NONE',  ( 0.03280839895013198948, -0.5511811023622048555, -0.09757992244046775898 ) ) ;
#62462 = CARTESIAN_POINT ( 'NONE',  ( -1.003937007874015297, -0.4536011799217368745, -0.2665933059059886201 ) ) ;
#62463 = CARTESIAN_POINT ( 'NONE',  ( -1.509186351706035767, 0.05413385826771626580, -0.4176697321401330321 ) ) ;
#62464 = CARTESIAN_POINT ( 'NONE',  ( 1.423884514435696191, -0.08942795157527998196, 0.3641732283464567121 ) ) ;
#62465 = CARTESIAN_POINT ( 'NONE',  ( 1.023622047244095334, -0.1870078740157479769, 0.4822834645669291653 ) ) ;
#62466 = FACE_OUTER_BOUND ( 'NONE', #83137, .T. ) ;
#62467 = CARTESIAN_POINT ( 'NONE',  ( 0.3543307086614181922, -0.5511811023622047445, 6.969142054262312111E-17 ) ) ;
#62468 = CARTESIAN_POINT ( 'NONE',  ( 0.1968503937007881344, 0.2952755905511811885, 0.000000000000000000 ) ) ;
#62469 = CARTESIAN_POINT ( 'NONE',  ( 1.003937007874016407, -0.5400638737290844871, 0.3530559997133364547 ) ) ;
#62470 = CARTESIAN_POINT ( 'NONE',  ( 0.8595800524934390507, -0.08942795157528024563, -0.3641732283464568787 ) ) ;
#62471 = VERTEX_POINT ( 'NONE', #3814 ) ;
#62472 = CARTESIAN_POINT ( 'NONE',  ( -1.194225721784776262, -0.4281496062992124485, 0.4176697321401328655 ) ) ;
#62473 = ADVANCED_FACE ( 'NONE', ( #4217 ), #73588, .T. ) ;
#62474 = CARTESIAN_POINT ( 'NONE',  ( -0.7677165354330699465, -0.5400638737290845981, -0.3530559997133363437 ) ) ;
#62475 = CARTESIAN_POINT ( 'NONE',  ( -0.1312335958005241554, 0.2306618581243848609, 0.2411417322834645549 ) ) ;
#62476 = CARTESIAN_POINT ( 'NONE',  ( -0.3460692066303958092, -0.1998031496062994683, -0.05249343832020999384 ) ) ;
#62477 = CARTESIAN_POINT ( 'NONE',  ( -0.3996062992125986590, 0.1070741851644051723, -2.629265091863517423 ) ) ;
#62478 = CARTESIAN_POINT ( 'NONE',  ( 0.2493438320209980519, -0.4281496062992127816, -0.4176697321401328100 ) ) ;
#62479 = CARTESIAN_POINT ( 'NONE',  ( 1.561679790026247350, -0.3690944881889763329, 0.3153832671262228327 ) ) ;
#62480 = CARTESIAN_POINT ( 'NONE',  ( -0.08530183727034056085, -0.3162353388693405765, 0.4822834645669290543 ) ) ;
#62481 = CARTESIAN_POINT ( 'NONE',  ( 0.8727034120734912248, -0.3162353388693409650, -0.4822834645669289433 ) ) ;
#62482 = CARTESIAN_POINT ( 'NONE',  ( 0.3460692066303959757, -0.1998031496062991907, -2.152230971128608950 ) ) ;
#62483 = CIRCLE ( 'NONE', #39657, 0.5120078740157480990 ) ;
#62484 = CARTESIAN_POINT ( 'NONE',  ( -0.3949938075777409408, -0.1058382717557502933, -1.305774278215223072 ) ) ;
#62485 = CARTESIAN_POINT ( 'NONE',  ( -9.787531504996567848E-17, 0.3996062992125986035, -2.834645669291338432 ) ) ;
#62486 = CARTESIAN_POINT ( 'NONE',  ( -0.5314960629921194890, 2.716535433070866645, -1.854472803289054283 ) ) ;
#62487 = CARTESIAN_POINT ( 'NONE',  ( -0.2867679344610366554, 0.2867679344610365444, -0.6417322834645668994 ) ) ;
#62488 = CARTESIAN_POINT ( 'NONE',  ( -0.6561679790026240244, -0.5023911411419708095, 0.1820866141732285504 ) ) ;
#62489 = CARTESIAN_POINT ( 'NONE',  ( -0.8070866141732276899, -0.5400638737290844871, 0.3530559997133364547 ) ) ;
#62490 = CARTESIAN_POINT ( 'NONE',  ( 0.3674540682414705883, 0.2306618581243847221, -0.2411417322834647770 ) ) ;
#62491 = CARTESIAN_POINT ( 'NONE',  ( -9.674558042662122972E-17, 0.3949938075777409963, -2.596456692913385655 ) ) ;
#62492 = CARTESIAN_POINT ( 'NONE',  ( 0.9055118110236227702, 0.2952755905511811885, 0.000000000000000000 ) ) ;
#62493 = CARTESIAN_POINT ( 'NONE',  ( -1.627296587926508442, 0.2306618581243848609, 0.2411417322834645549 ) ) ;
#62494 = CARTESIAN_POINT ( 'NONE',  ( 1.286089238845145033, 0.2306618581243848609, 0.2411417322834645549 ) ) ;
#62495 = CARTESIAN_POINT ( 'NONE',  ( -0.4091458600556402980, -0.2362204724409451284, -2.414698162729658648 ) ) ;
#62496 = CARTESIAN_POINT ( 'NONE',  ( 0.3996062992125986035, 2.446882876249141962E-17, -2.165354330708661568 ) ) ;
#62497 = CARTESIAN_POINT ( 'NONE',  ( -1.646051170424378096, -0.1870078740157480046, 1.254653134982923898E-17 ) ) ;
#62498 = CARTESIAN_POINT ( 'NONE',  ( 0.8989501312335963501, -0.6692913385826773087, -0.1292274648535924053 ) ) ;
#62499 = CARTESIAN_POINT ( 'NONE',  ( 0.4724409448818904789, -0.1870078740157479769, 0.4822834645669291653 ) ) ;
#62500 = CARTESIAN_POINT ( 'NONE',  ( 1.345144356955381593, -0.2845877964562161244, -0.3641732283464567121 ) ) ;
#62502 = CARTESIAN_POINT ( 'NONE',  ( -1.437007874015747477, 0.1660481256975883668, -0.3530559997133364547 ) ) ;
#62501 = CARTESIAN_POINT ( 'NONE',  ( -1.601049868766403650, 0.1283753931104746893, -0.1820866141732285504 ) ) ;
#62503 = CARTESIAN_POINT ( 'NONE',  ( 0.3392501089628018329, -0.1958661417322834497, -2.704705093666980087 ) ) ;
#62504 = CARTESIAN_POINT ( 'NONE',  ( -1.586052503253847501, 1.299212598425198095, 0.1653254495020568260 ) ) ;
#62505 = CARTESIAN_POINT ( 'NONE',  ( 0.6889763779527566800, -0.5400638737290844871, 0.3530559997133364547 ) ) ;
#62506 = CARTESIAN_POINT ( 'NONE',  ( 1.555118110236221041, 0.07958543189024071263, -0.2665933059059888421 ) ) ;
#62507 = CARTESIAN_POINT ( 'NONE',  ( -0.3871391076115479057, -0.3162353388693409650, -0.4822834645669289433 ) ) ;
#62508 = CARTESIAN_POINT ( 'NONE',  ( -0.5643044619422565855, 0.05413385826771626580, -0.4176697321401330321 ) ) ;
#62509 = CARTESIAN_POINT ( 'NONE',  ( 1.391076115485564868, -0.6046776061558807314, 0.2411417322834647770 ) ) ;
#62510 = CARTESIAN_POINT ( 'NONE',  ( -0.1049643490035302024, -0.3917322834645671215, -0.3143044619422573072 ) ) ;
#62511 = CARTESIAN_POINT ( 'NONE',  ( -0.3392501089628017219, -0.1958661417322836718, -1.461942257217847763 ) ) ;
#62512 = CARTESIAN_POINT ( 'NONE',  ( -0.1049643490035302024, -0.3917322834645671215, -2.269028871391075786 ) ) ;
#62513 = CARTESIAN_POINT ( 'NONE',  ( 1.601049868766404982, -0.6046776061558809534, -0.2411417322834644161 ) ) ;
#62514 = ORIENTED_EDGE ( 'NONE', *, *, #44940, .T. ) ;
#62515 = CARTESIAN_POINT ( 'NONE',  ( -0.1058382717557497937, -0.3949938075777411628, -2.749343832020997969 ) ) ;
#62516 = VERTEX_POINT ( 'NONE', #69436 ) ;
#62517 = LINE ( 'NONE', #16682, #26043 ) ;
#62518 = CARTESIAN_POINT ( 'NONE',  ( 1.581364829396326277, -0.08942795157527998196, 0.3641732283464567121 ) ) ;
#62519 = CARTESIAN_POINT ( 'NONE',  ( -0.2925321140481932924, 0.2925321140481931814, -0.9645669291338579976 ) ) ;
#62520 = CARTESIAN_POINT ( 'NONE',  ( 0.5618802787717186442, 7.570362723507360306E-16, 0.4118484887281971263 ) ) ;
#62521 = CARTESIAN_POINT ( 'NONE',  ( -0.09186351706036689768, 0.009842519685039144428, -0.3409548833797004797 ) ) ;
#62522 = B_SPLINE_CURVE_WITH_KNOTS ( 'NONE', 3,
 ( #69074, #57240, #57662, #18957, #12244, #18556, #56017 ),
 .UNSPECIFIED., .F., .F.,
 ( 4, 3, 4 ),
 ( 1.910166083080835130E-17, 0.001246230184515546152, 0.002492489877932653301 ),
 .UNSPECIFIED. ) ;
#62523 = CARTESIAN_POINT ( 'NONE',  ( -1.220472440944878834, 2.401574803149606474, -0.5309055118110234117 ) ) ;
#62524 = CARTESIAN_POINT ( 'NONE',  ( -0.5314960629921148261, 2.729659931386287042, -3.210901110887978582 ) ) ;
#62525 = CARTESIAN_POINT ( 'NONE',  ( -0.3917322834645669549, -0.1049643490035306603, -0.6030183727034120755 ) ) ;
#62526 = CARTESIAN_POINT ( 'NONE',  ( -0.8661417322834640276, -0.1870078740157479769, 0.3641732283464567677 ) ) ;
#62527 = CARTESIAN_POINT ( 'NONE',  ( -1.220472440944881054, 0.1771653543307087630, 0.000000000000000000 ) ) ;
#62528 = CARTESIAN_POINT ( 'NONE',  ( -0.06561679790026180015, -0.4281496062992127816, -0.4176697321401328100 ) ) ;
#62529 = CARTESIAN_POINT ( 'NONE',  ( 0.6364829396325465405, -0.05778040916215522460, 0.4822834645669289988 ) ) ;
#62530 = CARTESIAN_POINT ( 'NONE',  ( -1.213910761154854745, -0.6692913385826771977, 0.1292274648535927661 ) ) ;
#62531 = CARTESIAN_POINT ( 'NONE',  ( 0.3392501089628018329, 0.1958661417322835607, -0.2808398950131232863 ) ) ;
#62532 = ORIENTED_EDGE ( 'NONE', *, *, #81093, .F. ) ;
#62533 = CARTESIAN_POINT ( 'NONE',  ( 1.364829396325459854, -0.6046776061558809534, -0.2411417322834644161 ) ) ;
#62534 = DIRECTION ( 'NONE',  ( 1.000000000000000000, -0.000000000000000000, -0.000000000000000000 ) ) ;
#62535 = CARTESIAN_POINT ( 'NONE',  ( 7.456690011882655789, 3.916330350904249524, 5.973313079581529017 ) ) ;
#62536 = CARTESIAN_POINT ( 'NONE',  ( 0.3458507752293908943, -0.3458507752293908943, -1.830708661417322913 ) ) ;
#62537 = CARTESIAN_POINT ( 'NONE',  ( -0.01241954290193713825, 2.784432375088962958E-17, -0.3464511005275205946 ) ) ;
#62538 = CARTESIAN_POINT ( 'NONE',  ( -0.3412073490813641308, 0.1283753931104746893, -0.1820866141732285504 ) ) ;
#62539 = CARTESIAN_POINT ( 'NONE',  ( 0.4744094488189113945, 1.537401574803149984, -3.937007874015760578 ) ) ;
#62540 = CARTESIAN_POINT ( 'NONE',  ( -1.266404199475064773, -0.05778040916215560624, -0.4822834645669293319 ) ) ;
#62541 = CARTESIAN_POINT ( 'NONE',  ( 1.174540682414699111, -0.3162353388693405765, 0.4822834645669290543 ) ) ;
#62542 = VECTOR ( 'NONE', #64792, 39.37007874015748143 ) ;
#62544 = CARTESIAN_POINT ( 'NONE',  ( 0.6692913385826777528, 0.2066929133858268208, 0.000000000000000000 ) ) ;
#62543 = CARTESIAN_POINT ( 'NONE',  ( 3.937007874015748143, 1.537401574803149984, -0.4744094488188970171 ) ) ;
#62545 = EDGE_CURVE ( 'NONE', #74234, #1651, #37476, .T. ) ;
#62546 = CARTESIAN_POINT ( 'NONE',  ( 1.686351706036745890, 0.2952755905511811885, 0.1292274648535926551 ) ) ;
#62547 = CARTESIAN_POINT ( 'NONE',  ( -1.279527559055116948, -0.5400638737290844871, 0.3530559997133364547 ) ) ;
#62548 = CIRCLE ( 'NONE', #725, 0.1771653543307085410 ) ;
#62549 = CARTESIAN_POINT ( 'NONE',  ( 0.1049643490035303689, 0.3917322834645668994, -0.5459124427483446063 ) ) ;
#62550 = CARTESIAN_POINT ( 'NONE',  ( -0.07217847769028813698, -0.2845877964562161244, -0.3641732283464567121 ) ) ;
#62551 = CARTESIAN_POINT ( 'NONE',  ( -9.594673741351313045E-17, 0.3917322834645670104, -1.029527559055118280 ) ) ;
#62552 = EDGE_CURVE ( 'NONE', #17178, #36023, #33267, .T. ) ;
#62553 = CARTESIAN_POINT ( 'NONE',  ( -0.1574803149606292529, -0.1870078740157480601, -0.3641732283464567677 ) ) ;
#62554 = CARTESIAN_POINT ( 'NONE',  ( 0.6496062992125991586, 0.07958543189024085140, 0.2665933059059887866 ) ) ;
#62555 = CARTESIAN_POINT ( 'NONE',  ( 0.6036745406824153282, -0.6046776061558807314, 0.2411417322834647770 ) ) ;
#62556 = CARTESIAN_POINT ( 'NONE',  ( -0.9055118110236215490, -0.5511811023622047445, 6.969142054262312111E-17 ) ) ;
#62557 = CARTESIAN_POINT ( 'NONE',  ( -0.2867679344610364334, -0.2867679344610367109, -2.255905511811023612 ) ) ;
#62558 = CARTESIAN_POINT ( 'NONE',  ( 1.417322834645670104, -0.1870078740157479769, 0.4822834645669291653 ) ) ;
#62559 = CARTESIAN_POINT ( 'NONE',  ( -1.082677165354329896, -0.5400638737290845981, -0.3530559997133363437 ) ) ;
#62560 = CARTESIAN_POINT ( 'NONE',  ( 0.2362204724409451007, -0.4091458600556402980, -0.9560367454068241511 ) ) ;
#62561 = CARTESIAN_POINT ( 'NONE',  ( 0.1837270341207354329, 0.2306618581243848609, 0.2411417322834645549 ) ) ;
#62562 = CARTESIAN_POINT ( 'NONE',  ( -0.6692913385826764205, 0.2952755905511811885, 0.000000000000000000 ) ) ;
#62563 = CARTESIAN_POINT ( 'NONE',  ( 1.286089238845145033, -0.5023911411419708095, -0.1820866141732282451 ) ) ;
#62564 = CARTESIAN_POINT ( 'NONE',  ( 0.05249343832021075018, 0.1283753931104746893, -0.1820866141732285504 ) ) ;
#62565 = CARTESIAN_POINT ( 'NONE',  ( -0.1312335958005241554, 0.2306618581243848609, 0.2411417322834645549 ) ) ;
#62566 = CARTESIAN_POINT ( 'NONE',  ( -1.043307086614172041, -0.5400638737290844871, 0.3530559997133364547 ) ) ;
#62567 = DIRECTION ( 'NONE',  ( 0.000000000000000000, -1.000000000000000000, 0.000000000000000000 ) ) ;
#62568 = CARTESIAN_POINT ( 'NONE',  ( 1.594488188976378673, -0.4536011799217368745, -0.2665933059059886201 ) ) ;
#62569 = CARTESIAN_POINT ( 'NONE',  ( -0.1115485564304453947, -0.6692913385826771977, 0.1292274648535927661 ) ) ;
#62570 = VERTEX_POINT ( 'NONE', #5047 ) ;
#62571 = CARTESIAN_POINT ( 'NONE',  ( 0.3460692066303958092, 0.1998031496062993018, -1.940288713910761187 ) ) ;
#62572 = CARTESIAN_POINT ( 'NONE',  ( 1.017060367454068581, -0.05778040916215560624, -0.4822834645669293319 ) ) ;
#62573 = CARTESIAN_POINT ( 'NONE',  ( -0.8070866141732276899, -0.4536011799217367080, 0.2665933059059888421 ) ) ;
#62574 = CARTESIAN_POINT ( 'NONE',  ( -0.6758530183727028406, -0.6692913385826773087, -0.1292274648535924053 ) ) ;
#62575 = CARTESIAN_POINT ( 'NONE',  ( 1.266404199475066328, -0.3162353388693409650, -0.4822834645669289433 ) ) ;
#62576 = CARTESIAN_POINT ( 'NONE',  ( 0.7086614173228353852, -0.1870078740157479769, 0.4822834645669291653 ) ) ;
#62577 = CARTESIAN_POINT ( 'NONE',  ( 3.937007874015748143, 2.165354330708661568, 0.3149606299212600047 ) ) ;
#62578 = CARTESIAN_POINT ( 'NONE',  ( -1.187664041994750175, -0.08942795157528024563, -0.3641732283464568787 ) ) ;
#62579 = CARTESIAN_POINT ( 'NONE',  ( -0.1998031496062994405, 0.3460692066303957537, -0.08989501312335959615 ) ) ;
#62580 = CARTESIAN_POINT ( 'NONE',  ( -0.1998031496062991907, -0.3460692066303959757, -0.6955380577427822120 ) ) ;
#62581 = CARTESIAN_POINT ( 'NONE',  ( -0.3420746716998661618, 0.1974969037888702206, -0.1837270341207349611 ) ) ;
#62582 = CARTESIAN_POINT ( 'NONE',  ( 0.4671901501889602626, 1.453473631083803674, 2.571356120034363091 ) ) ;
#62583 = CARTESIAN_POINT ( 'NONE',  ( 1.561679790026247350, -0.004921259842519870586, -0.3153832671262229437 ) ) ;
#62584 = CARTESIAN_POINT ( 'NONE',  ( 0.6561679790026253567, 0.1283753931104748280, 0.1820866141732283561 ) ) ;
#62585 = CARTESIAN_POINT ( 'NONE',  ( 0.4199475065616803948, -0.6046776061558809534, -0.2411417322834644161 ) ) ;
#62586 = CARTESIAN_POINT ( 'NONE',  ( 0.2318981092368783414, -0.1830245018656607436, 0.1465342031617538066 ) ) ;
#62587 = CARTESIAN_POINT ( 'NONE',  ( -0.1974969037888704149, -0.3420746716998661063, -0.7723097112860893843 ) ) ;
#62588 = CARTESIAN_POINT ( 'NONE',  ( 0.8595800524934390507, -0.2845877964562159024, 0.3641732283464567677 ) ) ;
#62589 = CARTESIAN_POINT ( 'NONE',  ( -0.4002624671916004129, -0.3162353388693405765, 0.4822834645669290543 ) ) ;
#62590 = CARTESIAN_POINT ( 'NONE',  ( -0.7414698162729651543, -0.6692913385826771977, 0.1292274648535927661 ) ) ;
#62591 = CARTESIAN_POINT ( 'NONE',  ( 1.102362204724410155, -0.1870078740157480879, -0.4822834645669291653 ) ) ;
#62592 = CARTESIAN_POINT ( 'NONE',  ( 5.785732909357575061E-17, -0.4724409448818898682, -1.023622047244094446 ) ) ;
#62593 = CARTESIAN_POINT ( 'NONE',  ( -0.3996062992125985480, -0.1070741851644057135, -2.408136482939632561 ) ) ;
#62594 = VECTOR ( 'NONE', #48130, 39.37007874015748143 ) ;
#62595 = CARTESIAN_POINT ( 'NONE',  ( -0.2362204724409442680, -0.1870078740157480601, -0.3641732283464567677 ) ) ;
#62596 = ORIENTED_EDGE ( 'NONE', *, *, #42203, .T. ) ;
#62597 = CARTESIAN_POINT ( 'NONE',  ( -0.1958661417322833942, -0.3392501089628018884, -0.8497568485902381452 ) ) ;
#62598 = VERTEX_POINT ( 'NONE', #50062 ) ;
#62599 = CARTESIAN_POINT ( 'NONE',  ( -0.9317585301837263412, 0.05413385826771666132, 0.4176697321401328100 ) ) ;
#62600 = CARTESIAN_POINT ( 'NONE',  ( -0.2690288713910754526, -0.6692913385826771977, 0.1292274648535927661 ) ) ;
#62601 = CARTESIAN_POINT ( 'NONE',  ( -0.4986876640419939388, 0.2306618581243847221, -0.2411417322834647770 ) ) ;
#62602 = DIMENSIONAL_EXPONENTS ( 1.000000000000000000, 0.000000000000000000, 0.000000000000000000, 0.000000000000000000, 0.000000000000000000, 0.000000000000000000, 0.000000000000000000 ) ;
#62603 = CARTESIAN_POINT ( 'NONE',  ( 0.4921259842519691285, -0.5400638737290845981, -0.3530559997133363437 ) ) ;
#62604 = CARTESIAN_POINT ( 'NONE',  ( -0.4527559055118102749, -0.5400638737290845981, -0.3530559997133363437 ) ) ;
#62605 = CARTESIAN_POINT ( 'NONE',  ( -1.364829396325458521, -0.6046776061558807314, 0.2411417322834647770 ) ) ;
#62606 = CARTESIAN_POINT ( 'NONE',  ( -0.6299212598425188991, -0.1870078740157479769, 0.4822834645669291653 ) ) ;
#62607 = CARTESIAN_POINT ( 'NONE',  ( 0.9580052493438326877, 0.05413385826771666132, 0.4176697321401328100 ) ) ;
#62608 =( BOUNDED_SURFACE ( )  B_SPLINE_SURFACE ( 1, 2, ( 
 ( #69300, #24252, #10815, #11231, #50333, #55410, #4491, #12053, #81116, #36892, #37710, #42370, #16729, #37307, #17961, #62568, #75623, #63383, #68069, #43598, #62981, #36475, #62150, #5320, #29339, #56645, #23433, #49098, #74802, #30159, #26323, #44413, #77264, #38949, #19593, #39369, #57055, #6968, #45670, #39792, #58730, #26744, #46093, #82747, #51148, #76441, #45255, #33060, #71366, #51984, #12459, #52399, #32639, #38120, #31808, #19176, #1093, #44824, #7392, #668, #57468, #58302, #77689, #70107, #12878, #76842, #70522, #65054, #70952, #78108, #13297, #83162, #57881, #32223, #20439, #13715, #20019, #64218, #25900, #63795, #64632, #71785, #5719, #50743, #25069, #18770, #25481, #38537, #14140, #31389, #6552, #6133, #248, #51560, #46508, #47758, #72208, #67141, #28824, #14561, #41043, #7819, #40213, #53236, #53653, #79361, #27993, #21680, #16214, #47341, #33895, #73031, #22517, #33486, #48178, #80199, #59561, #15381, #73874, #65487, #72618, #1505, #1916, #34317, #54488, #59148, #22097, #35144, #66728, #9065, #28408, #2337, #27157, #34737, #60397, #52821, #60806, #14966, #78531, #2748, #20856, #65895, #8231, #27579, #78952, #40623, #8645, #54066, #79782, #41457, #21270, #46925, #66306, #59978, #73456, #15806, #9470, #3160, #49422, #37205, #10312, #35977, #81023, #43092, #50238, #23335, #74286, #67553, #42690, #75528, #75934, #49005, #56552, #43502, #68789, #62886, #36383, #41861, #24572, #75117, #80612, #17462, #74704, #5221, #29242, #69200, #11134, #9888, #35557, #61221, #30479, #24160, #81434, #3575, #36791, #49828, #17049, #11549, #54906, #4802, #62057, #56143, #22923, #17868, #62467, #29652, #48589, #30885, #16630, #42272, #23749, #68387, #67969, #4395, #82253, #61647, #3988, #81848, #10726, #55314, #30063, #55724, #69613, #37614, #6459, #70013, #27369, #33286, #64123, #83068, #56960, #53454, #1305, #12368, #63289, #40423, #25389, #33694, #44323, #58947, #63702, #38027, #18678, #40014, #82657, #18275, #65701, #43916, #27794, #5629, #66104, #26954, #11959, #52617, #21068, #31296, #72418, #78323, #53030, #76753, #46726, #24972, #8031, #12784, #59355, #50644, #1714, #20654, #6041, #76348, #78743, #31713, #57373, #46307, #51052, #19083, #72001, #14767, #44732, #70428, #14357, #38441, #8440, #34110, #59771, #2126, #15178, #67351, #47555, #3783, #9684, #41660, #60608, #34531, #29851, #61017, #73247, #40835, #16842, #2957, #10102, #21891, #35355, #41256, #15596, #79575, #16425, #60195, #79162, #42071, #21479, #4188, #66520, #42476, #3368, #47137, #29032, #80814, #8852, #48797, #80409, #67766, #16014, #72828, #22721, #54703, #36174, #74495, #28622, #2546, #48380, #61847, #28204, #53863, #66942, #9274, #54280, #22310, #74079, #35766, #55105, #34945, #79996, #10520, #47973, #73672, #61436, #29446, #23129, #68181, #50850, #23952, #49620, #11338, #56754, #63906, #36998, #4593, #81222, #56348, #5829, #6242, #62677, #70215, #57162, #82454, #76550, #50032, #55514, #38229, #63087, #10921, #31087, #5019, #18878, #42885, #82861, #24769, #23538, #49207, #74911, #44122, #37819, #11761, #17257, #31502, #68580, #36578, #62257, #30264, #75314, #81644, #25183, #44527, #17661, #50438, #82049, #76139, #55928, #63495, #43292, #12571, #68989, #30687, #18480, #24362, #75729, #18069, #43704, #69407, #37415, #5425, #69814, #12163, #359, #13829, #72322, #57580, #14668, #46626, #26016, #65175, #40326, #66004, #39062, #51257, #51674, #781, #78644, #31919, #71902, #1615, #45783, #1206, #13407, #26442, #52932, #6661, #7083, #20967, #12992, #77803, #27271, #44938, #25594, #14254, #20556, #20135, #7512, #83271, #76959, #52095, #71482, #71063, #64745, #39488, #19287, #33180, #58849, #70636, #38648, #26856, #52515, #64325, #78223, #46208, #39912, #65600, #32333, #7932, #33593, #57995, #77378, #19709, #45368, #32754, #58421, #59258, #22209, #35664, #48281, #54598, #15076, #29347, #9584, #40734, #34430, #21789, #61328, #47451, #9999, #3268, #60095, #35253, #28929, #47036, #15495, #79473, #73146, #41969, #47866, #3682, #22622, #2857, #27692, #59671, #60917, #34846, #41153, #23029, #2026 ),
 ( #66841, #67662, #73570, #9175, #53355, #55006, #80714, #60509, #48695, #16325, #80307, #28521, #54177, #72730, #15915, #74393, #42377, #79066, #21382, #66418, #28108, #2450, #16737, #8343, #53762, #73979, #79891, #34009, #8754, #41563, #67252, #69717, #31399, #74811, #43606, #10420, #17156, #55829, #56251, #81947, #30585, #24260, #18780, #49933, #36483, #75631, #25079, #36078, #50753, #82758, #62158, #17969, #76453, #68076, #75216, #4086, #4499, #36899, #57064, #61749, #24673, #37719, #69308, #37316, #49523, #62575, #5728, #42789, #43193, #29754, #49105, #11658, #63393, #81124, #55417, #50341, #56654, #62989, #5328, #23441, #68484, #4917, #30986, #23856, #17561, #82355, #10823, #76038, #18383, #30166, #81537, #44024, #12061, #68889, #11239, #77700, #58314, #78119, #12469, #45681, #1104, #78545, #14151, #65498, #1517, #38131, #6562, #31818, #679, #71798, #26755, #7404, #51158, #7830, #71377, #44423, #27171, #51995, #83172, #20030, #25911, #33497, #57478, #39807, #13727, #63805, #70118, #6144, #33075, #52410, #26334, #52833, #39381, #20452, #19604, #59159, #25492, #58742, #38959, #46105, #76853, #19186, #65066, #32234, #44835, #70533, #12889, #38548, #64228, #57892, #45266, #259, #64643, #51571, #77274, #70962, #13307, #6980, #32649, #14573, #72222, #40225, #9079, #72630, #28835, #34750, #66743, #2350, #59573, #54918, #2761, #14978, #65907, #41873, #28006, #35159, #46938, #60410, #66319, #40637, #21283, #41470, #1929, #20870, #67155, #46523, #29254, #8243, #67567, #28420, #33909, #54080, #22527, #27592, #73886, #22111, #9484, #41055, #53252, #47771, #79795, #61234, #16226, #53666, #78964, #73472, #3589, #8658, #34329, #59994, #79373, #21692, #47355, #15821, #60819, #80212, #73044, #15393, #35571, #3171, #54499, #48189, #9899, #37221, #4815, #75946, #49018, #74715, #36394, #81859, #5640, #62068, #29664, #22936, #81446, #30897, #31307, #4407, #11971, #82265, #24171, #18287, #75128, #30493, #68398, #80624, #5233, #48602, #55326, #36804, #10737, #23763, #11562, #17473, #16644, #74298, #49840, #49434, #30075, #37626, #42284, #67982, #10327, #68800, #17064, #56564, #11145, #43104, #55738, #35989, #61659, #62480, #42701, #4000, #43932, #56156, #62898, #23347, #75539, #17879, #43513, #81035, #69213, #24583, #50250, #69626, #63302, #65399, #76360, #78023, #45164, #7736, #38865, #58641, #18692, #26662, #58216, #19938, #77179, #56971, #582, #13219, #14053, #52316, #6469, #82669, #32553, #39707, #50660, #70026, #83079, #44335, #32139, #163, #6883, #77605, #32973, #38037, #38451, #71699, #12379, #24984, #64546, #26236, #13629, #51898, #20351, #25400, #51064, #12795, #45587, #63712, #64137, #6052, #31724, #57796, #7304, #57387, #25816, #76764, #1009, #71280, #46003, #51476, #19094, #44743, #39281, #70438, #64968, #19510, #70870, #20771, #60720, #60312, #1419, #33402, #27075, #22010, #15713, #72943, #41768, #40956, #41370, #8560, #3069, #67461, #79693, #27909, #47670, #52734, #67051, #59064, #40542, #78445, #27490, #2243, #80108, #46424, #73364, #28736, #47254, #2661, #14882, #53568, #54396, #8147, #34228, #22427, #14475, #79277, #48085, #72116, #40128, #9384, #35054, #21592, #8973, #73786, #65814, #15295, #66636, #72534, #66222, #34648, #33812, #28320, #53981, #16122, #59477, #1830, #53147, #78860, #21186, #46840, #59889, #43406, #61131, #11036, #49735, #43815, #62795, #30794, #50144, #3482, #55220, #80519, #23654, #37111, #75434, #56047, #16540, #56460, #36694, #42185, #35885, #23242, #5130, #48912, #11454, #4707, #61555, #62369, #30380, #48493, #16956, #80927, #74612, #69106, #49324, #42596, #29149, #82162, #24478, #36289, #75841, #17774, #81756, #68298, #29965, #74194, #75026, #18183, #9795, #54818, #22834, #67880, #29557, #3898, #35467, #10217, #10634, #24066, #61962, #4302, #55630, #81339, #17371, #43001, #68694, #76254, #45059, #11870, #18589, #57277, #57695, #57, #32036, #25711, #20251, #51371, #37933, #77074, #26563, #37522, #52217, #906, #63610, #19408, #77920, #76657, #477, #12275, #70761, #31616, #5947, #69921, #6777, #50550, #69520, #32449, #63196 ) ),
 .UNSPECIFIED., .F., .F., .F. ) 
 B_SPLINE_SURFACE_WITH_KNOTS ( ( 2, 2 ),
 ( 3, 2, 2, 2, 2, 2, 2, 2, 2, 2, 2, 2, 2, 2, 2, 2, 2, 2, 2, 2, 2, 2, 2, 2, 2, 2, 2, 2, 2, 2, 2, 2, 2, 2, 2, 2, 2, 2, 2, 2, 2, 2, 2, 2, 2, 2, 2, 2, 2, 2, 2, 2, 2, 2, 2, 2, 2, 2, 2, 2, 2, 2, 2, 2, 2, 2, 2, 2, 2, 2, 2, 2, 2, 2, 2, 2, 2, 2, 2, 2, 2, 2, 2, 2, 2, 2, 2, 2, 2, 2, 2, 2, 2, 2, 2, 2, 2, 2, 2, 2, 2, 2, 2, 2, 2, 2, 2, 2, 2, 2, 2, 2, 2, 2, 2, 2, 2, 2, 2, 2, 2, 2, 2, 2, 2, 2, 2, 2, 2, 2, 2, 2, 2, 2, 2, 2, 2, 2, 2, 2, 2, 2, 2, 2, 2, 2, 2, 2, 2, 2, 2, 2, 2, 2, 2, 2, 2, 2, 2, 2, 2, 2, 2, 2, 2, 2, 2, 2, 2, 2, 2, 2, 2, 2, 2, 2, 2, 2, 2, 2, 2, 2, 2, 2, 2, 2, 2, 2, 2, 2, 2, 2, 2, 2, 2, 2, 2, 2, 2, 2, 2, 2, 2, 2, 2, 2, 2, 2, 2, 2, 2, 2, 2, 2, 2, 2, 2, 2, 2, 2, 2, 2, 2, 2, 2, 2, 2, 2, 2, 2, 2, 2, 2, 2, 2, 2, 2, 2, 2, 2, 2, 2, 2, 2, 2, 2, 2, 2, 2, 2, 2, 2, 2, 2, 2, 3 ),
 ( 0.000000000000000000, 1.000000000000000000 ),
 ( 0.000000000000000000, 0.003787878787878787984, 0.007575757575757575968, 0.01136363636363636395, 0.01515151515151515194, 0.01893939393939393992, 0.02272727272727272790, 0.02651515151515151589, 0.03030303030303030387, 0.03409090909090908839, 0.03787878787878787984, 0.04166666666666666435, 0.04545454545454545581, 0.04924242424242424032, 0.05303030303030303177, 0.05681818181818181629, 0.06060606060606060774, 0.06439393939393939226, 0.06818181818181817677, 0.07196969696969697516, 0.07575757575757575968, 0.07954545454545454419, 0.08333333333333332871, 0.08712121212121212710, 0.09090909090909091161, 0.09469696969696969613, 0.09848484848484848064, 0.1022727272727272790, 0.1060606060606060635, 0.1098484848484848481, 0.1136363636363636326, 0.1174242424242424310, 0.1212121212121212155, 0.1250000000000000000, 0.1287878787878787845, 0.1325757575757575690, 0.1363636363636363535, 0.1401515151515151381, 0.1439393939393939503, 0.1477272727272727348, 0.1515151515151515194, 0.1553030303030303039, 0.1590909090909090884, 0.1628787878787878729, 0.1666666666666666574, 0.1704545454545454419, 0.1742424242424242542, 0.1780303030303030387, 0.1818181818181818232, 0.1856060606060606077, 0.1893939393939393923, 0.1931818181818181768, 0.1969696969696969613, 0.2007575757575757458, 0.2045454545454545581, 0.2083333333333333426, 0.2121212121212121271, 0.2159090909090909116, 0.2196969696969696961, 0.2234848484848484806, 0.2272727272727272652, 0.2310606060606060497, 0.2348484848484848619, 0.2386363636363636465, 0.2424242424242424310, 0.2462121212121212155, 0.2500000000000000000, 0.2537878787878787845, 0.2575757575757575690, 0.2613636363636363535, 0.2651515151515151381, 0.2689393939393939226, 0.2727272727272727071, 0.2765151515151514916, 0.2803030303030302761, 0.2840909090909091161, 0.2878787878787879007, 0.2916666666666666852, 0.2954545454545454697, 0.2992424242424242542, 0.3030303030303030387, 0.3068181818181818232, 0.3106060606060606077, 0.3143939393939393923, 0.3181818181818181768, 0.3219696969696969613, 0.3257575757575757458, 0.3295454545454545303, 0.3333333333333333148, 0.3371212121212120993, 0.3409090909090908839, 0.3446969696969697239, 0.3484848484848485084, 0.3522727272727272929, 0.3560606060606060774, 0.3598484848484848619, 0.3636363636363636465, 0.3674242424242424310, 0.3712121212121212155, 0.3750000000000000000, 0.3787878787878787845, 0.3825757575757575690, 0.3863636363636363535, 0.3901515151515151381, 0.3939393939393939226, 0.3977272727272727071, 0.4015151515151514916, 0.4053030303030302761, 0.4090909090909091161, 0.4128787878787879007, 0.4166666666666666852, 0.4204545454545454697, 0.4242424242424242542, 0.4280303030303030387, 0.4318181818181818232, 0.4356060606060606077, 0.4393939393939393923, 0.4431818181818181768, 0.4469696969696969613, 0.4507575757575757458, 0.4545454545454545303, 0.4583333333333333148, 0.4621212121212120993, 0.4659090909090908839, 0.4696969696969697239, 0.4734848484848485084, 0.4772727272727272929, 0.4810606060606060774, 0.4848484848484848619, 0.4886363636363636465, 0.4924242424242424310, 0.4962121212121212155, 0.5000000000000000000, 0.5037878787878787845, 0.5075757575757575690, 0.5113636363636363535, 0.5151515151515151381, 0.5189393939393939226, 0.5227272727272727071, 0.5265151515151514916, 0.5303030303030302761, 0.5340909090909090606, 0.5378787878787878451, 0.5416666666666666297, 0.5454545454545454142, 0.5492424242424241987, 0.5530303030303029832, 0.5568181818181817677, 0.5606060606060605522, 0.5643939393939394478, 0.5681818181818182323, 0.5719696969696970168, 0.5757575757575758013, 0.5795454545454545858, 0.5833333333333333703, 0.5871212121212121549, 0.5909090909090909394, 0.5946969696969697239, 0.5984848484848485084, 0.6022727272727272929, 0.6060606060606060774, 0.6098484848484848619, 0.6136363636363636465, 0.6174242424242424310, 0.6212121212121212155, 0.6250000000000000000, 0.6287878787878787845, 0.6325757575757575690, 0.6363636363636363535, 0.6401515151515151381, 0.6439393939393939226, 0.6477272727272727071, 0.6515151515151514916, 0.6553030303030302761, 0.6590909090909090606, 0.6628787878787878451, 0.6666666666666666297, 0.6704545454545454142, 0.6742424242424241987, 0.6780303030303029832, 0.6818181818181817677, 0.6856060606060605522, 0.6893939393939394478, 0.6931818181818182323, 0.6969696969696970168, 0.7007575757575758013, 0.7045454545454545858, 0.7083333333333333703, 0.7121212121212121549, 0.7159090909090909394, 0.7196969696969697239, 0.7234848484848485084, 0.7272727272727272929, 0.7310606060606060774, 0.7348484848484848619, 0.7386363636363636465, 0.7424242424242424310, 0.7462121212121212155, 0.7500000000000000000, 0.7537878787878787845, 0.7575757575757575690, 0.7613636363636363535, 0.7651515151515151381, 0.7689393939393939226, 0.7727272727272727071, 0.7765151515151514916, 0.7803030303030302761, 0.7840909090909090606, 0.7878787878787878451, 0.7916666666666666297, 0.7954545454545454142, 0.7992424242424241987, 0.8030303030303029832, 0.8068181818181817677, 0.8106060606060605522, 0.8143939393939394478, 0.8181818181818182323, 0.8219696969696970168, 0.8257575757575758013, 0.8295454545454545858, 0.8333333333333333703, 0.8371212121212121549, 0.8409090909090909394, 0.8446969696969697239, 0.8484848484848485084, 0.8522727272727272929, 0.8560606060606060774, 0.8598484848484848619, 0.8636363636363636465, 0.8674242424242424310, 0.8712121212121212155, 0.8750000000000000000, 0.8787878787878787845, 0.8825757575757575690, 0.8863636363636363535, 0.8901515151515151381, 0.8939393939393939226, 0.8977272727272727071, 0.9015151515151514916, 0.9053030303030302761, 0.9090909090909090606, 0.9128787878787878451, 0.9166666666666666297, 0.9204545454545454142, 0.9242424242424241987, 0.9280303030303029832, 0.9318181818181817677, 0.9356060606060605522, 0.9393939393939394478, 0.9431818181818182323, 0.9469696969696970168, 0.9507575757575758013, 0.9545454545454545858, 0.9583333333333333703, 0.9621212121212121549, 0.9659090909090909394 ),
 .UNSPECIFIED. ) 
 GEOMETRIC_REPRESENTATION_ITEM ( )  RATIONAL_B_SPLINE_SURFACE ( (
 ( 1.000000000000000000, 0.9659258262890683122, 1.000000000000000000, 0.9659258262890683122, 1.000000000000000000, 0.9659258262890683122, 1.000000000000000000, 0.9659258262890683122, 1.000000000000000000, 0.9659258262890683122, 1.000000000000000000, 0.9659258262890683122, 1.000000000000000000, 0.9659258262890683122, 1.000000000000000000, 0.9659258262890683122, 1.000000000000000000, 0.9659258262890683122, 1.000000000000000000, 0.9659258262890683122, 1.000000000000000000, 0.9659258262890683122, 1.000000000000000000, 0.9659258262890683122, 1.000000000000000000, 0.9659258262890683122, 1.000000000000000000, 0.9659258262890683122, 1.000000000000000000, 0.9659258262890683122, 1.000000000000000000, 0.9659258262890683122, 1.000000000000000000, 0.9659258262890683122, 1.000000000000000000, 0.9659258262890683122, 1.000000000000000000, 0.9659258262890683122, 1.000000000000000000, 0.9659258262890683122, 1.000000000000000000, 0.9659258262890683122, 1.000000000000000000, 0.9659258262890683122, 1.000000000000000000, 0.9659258262890683122, 1.000000000000000000, 0.9659258262890683122, 1.000000000000000000, 0.9659258262890683122, 1.000000000000000000, 0.9659258262890683122, 1.000000000000000000, 0.9659258262890683122, 1.000000000000000000, 0.9659258262890683122, 1.000000000000000000, 0.9659258262890683122, 1.000000000000000000, 0.9659258262890683122, 1.000000000000000000, 0.9659258262890683122, 1.000000000000000000, 0.9659258262890683122, 1.000000000000000000, 0.9659258262890683122, 1.000000000000000000, 0.9659258262890683122, 1.000000000000000000, 0.9659258262890683122, 1.000000000000000000, 0.9659258262890683122, 1.000000000000000000, 0.9659258262890683122, 1.000000000000000000, 0.9659258262890683122, 1.000000000000000000, 0.9659258262890683122, 1.000000000000000000, 0.9659258262890683122, 1.000000000000000000, 0.9659258262890683122, 1.000000000000000000, 0.9659258262890683122, 1.000000000000000000, 0.9659258262890683122, 1.000000000000000000, 0.9659258262890683122, 1.000000000000000000, 0.9659258262890683122, 1.000000000000000000, 0.9659258262890683122, 1.000000000000000000, 0.9659258262890683122, 1.000000000000000000, 0.9659258262890683122, 1.000000000000000000, 0.9659258262890683122, 1.000000000000000000, 0.9659258262890683122, 1.000000000000000000, 0.9659258262890683122, 1.000000000000000000, 0.9659258262890683122, 1.000000000000000000, 0.9659258262890683122, 1.000000000000000000, 0.9659258262890683122, 1.000000000000000000, 0.9659258262890683122, 1.000000000000000000, 0.9659258262890683122, 1.000000000000000000, 0.9659258262890683122, 1.000000000000000000, 0.9659258262890683122, 1.000000000000000000, 0.9659258262890683122, 1.000000000000000000, 0.9659258262890683122, 1.000000000000000000, 0.9659258262890683122, 1.000000000000000000, 0.9659258262890683122, 1.000000000000000000, 0.9659258262890683122, 1.000000000000000000, 0.9659258262890683122, 1.000000000000000000, 0.9659258262890683122, 1.000000000000000000, 0.9659258262890683122, 1.000000000000000000, 0.9659258262890683122, 1.000000000000000000, 0.9659258262890683122, 1.000000000000000000, 0.9659258262890683122, 1.000000000000000000, 0.9659258262890683122, 1.000000000000000000, 0.9659258262890683122, 1.000000000000000000, 0.9659258262890683122, 1.000000000000000000, 0.9659258262890683122, 1.000000000000000000, 0.9659258262890683122, 1.000000000000000000, 0.9659258262890683122, 1.000000000000000000, 0.9659258262890683122, 1.000000000000000000, 0.9659258262890683122, 1.000000000000000000, 0.9659258262890683122, 1.000000000000000000, 0.9659258262890683122, 1.000000000000000000, 0.9659258262890683122, 1.000000000000000000, 0.9659258262890683122, 1.000000000000000000, 0.9659258262890683122, 1.000000000000000000, 0.9659258262890683122, 1.000000000000000000, 0.9659258262890683122, 1.000000000000000000, 0.9659258262890683122, 1.000000000000000000, 0.9659258262890683122, 1.000000000000000000, 0.9659258262890683122, 1.000000000000000000, 0.9659258262890683122, 1.000000000000000000, 0.9659258262890683122, 1.000000000000000000, 0.9659258262890683122, 1.000000000000000000, 0.9659258262890683122, 1.000000000000000000, 0.9659258262890683122, 1.000000000000000000, 0.9659258262890683122, 1.000000000000000000, 0.9659258262890683122, 1.000000000000000000, 0.9659258262890683122, 1.000000000000000000, 0.9659258262890683122, 1.000000000000000000, 0.9659258262890683122, 1.000000000000000000, 0.9659258262890683122, 1.000000000000000000, 0.9659258262890683122, 1.000000000000000000, 0.9659258262890683122, 1.000000000000000000, 0.9659258262890683122, 1.000000000000000000, 0.9659258262890683122, 1.000000000000000000, 0.9659258262890683122, 1.000000000000000000, 0.9659258262890683122, 1.000000000000000000, 0.9659258262890683122, 1.000000000000000000, 0.9659258262890683122, 1.000000000000000000, 0.9659258262890683122, 1.000000000000000000, 0.9659258262890683122, 1.000000000000000000, 0.9659258262890683122, 1.000000000000000000, 0.9659258262890683122, 1.000000000000000000, 0.9659258262890683122, 1.000000000000000000, 0.9659258262890683122, 1.000000000000000000, 0.9659258262890683122, 1.000000000000000000, 0.9659258262890683122, 1.000000000000000000, 0.9659258262890683122, 1.000000000000000000, 0.9659258262890683122, 1.000000000000000000, 0.9659258262890683122, 1.000000000000000000, 0.9659258262890683122, 1.000000000000000000, 0.9659258262890683122, 1.000000000000000000, 0.9659258262890683122, 1.000000000000000000, 0.9659258262890683122, 1.000000000000000000, 0.9659258262890683122, 1.000000000000000000, 0.9659258262890683122, 1.000000000000000000, 0.9659258262890683122, 1.000000000000000000, 0.9659258262890683122, 1.000000000000000000, 0.9659258262890683122, 1.000000000000000000, 0.9659258262890683122, 1.000000000000000000, 0.9659258262890683122, 1.000000000000000000, 0.9659258262890683122, 1.000000000000000000, 0.9659258262890683122, 1.000000000000000000, 0.9659258262890683122, 1.000000000000000000, 0.9659258262890683122, 1.000000000000000000, 0.9659258262890683122, 1.000000000000000000, 0.9659258262890683122, 1.000000000000000000, 0.9659258262890683122, 1.000000000000000000, 0.9659258262890683122, 1.000000000000000000, 0.9659258262890683122, 1.000000000000000000, 0.9659258262890683122, 1.000000000000000000, 0.9659258262890683122, 1.000000000000000000, 0.9659258262890683122, 1.000000000000000000, 0.9659258262890683122, 1.000000000000000000, 0.9659258262890683122, 1.000000000000000000, 0.9659258262890683122, 1.000000000000000000, 0.9659258262890683122, 1.000000000000000000, 0.9659258262890683122, 1.000000000000000000, 0.9659258262890683122, 1.000000000000000000, 0.9659258262890683122, 1.000000000000000000, 0.9659258262890683122, 1.000000000000000000, 0.9659258262890683122, 1.000000000000000000, 0.9659258262890683122, 1.000000000000000000, 0.9659258262890683122, 1.000000000000000000, 0.9659258262890683122, 1.000000000000000000, 0.9659258262890683122, 1.000000000000000000, 0.9659258262890683122, 1.000000000000000000, 0.9659258262890683122, 1.000000000000000000, 0.9659258262890683122, 1.000000000000000000, 0.9659258262890683122, 1.000000000000000000, 0.9659258262890683122, 1.000000000000000000, 0.9659258262890683122, 1.000000000000000000, 0.9659258262890683122, 1.000000000000000000, 0.9659258262890683122, 1.000000000000000000, 0.9659258262890683122, 1.000000000000000000, 0.9659258262890683122, 1.000000000000000000, 0.9659258262890683122, 1.000000000000000000, 0.9659258262890683122, 1.000000000000000000, 0.9659258262890683122, 1.000000000000000000, 0.9659258262890683122, 1.000000000000000000, 0.9659258262890683122, 1.000000000000000000, 0.9659258262890683122, 1.000000000000000000, 0.9659258262890683122, 1.000000000000000000, 0.9659258262890683122, 1.000000000000000000, 0.9659258262890683122, 1.000000000000000000, 0.9659258262890683122, 1.000000000000000000, 0.9659258262890683122, 1.000000000000000000, 0.9659258262890683122, 1.000000000000000000, 0.9659258262890683122, 1.000000000000000000, 0.9659258262890683122, 1.000000000000000000, 0.9659258262890683122, 1.000000000000000000, 0.9659258262890683122, 1.000000000000000000, 0.9659258262890683122, 1.000000000000000000, 0.9659258262890683122, 1.000000000000000000, 0.9659258262890683122, 1.000000000000000000, 0.9659258262890683122, 1.000000000000000000, 0.9659258262890683122, 1.000000000000000000, 0.9659258262890683122, 1.000000000000000000, 0.9659258262890683122, 1.000000000000000000, 0.9659258262890683122, 1.000000000000000000, 0.9659258262890683122, 1.000000000000000000, 0.9659258262890683122, 1.000000000000000000, 0.9659258262890683122, 1.000000000000000000, 0.9659258262890683122, 1.000000000000000000, 0.9659258262890683122, 1.000000000000000000, 0.9659258262890683122, 1.000000000000000000, 0.9659258262890683122, 1.000000000000000000, 0.9659258262890683122, 1.000000000000000000, 0.9659258262890683122, 1.000000000000000000, 0.9659258262890683122, 1.000000000000000000, 0.9659258262890683122, 1.000000000000000000, 0.9659258262890683122, 1.000000000000000000, 0.9659258262890683122, 1.000000000000000000, 0.9659258262890683122, 1.000000000000000000, 0.9659258262890683122, 1.000000000000000000, 0.9659258262890683122, 1.000000000000000000, 0.9659258262890683122, 1.000000000000000000, 0.9659258262890683122, 1.000000000000000000, 0.9659258262890683122, 1.000000000000000000, 0.9659258262890683122, 1.000000000000000000, 0.9659258262890683122, 1.000000000000000000, 0.9659258262890683122, 1.000000000000000000, 0.9659258262890683122, 1.000000000000000000, 0.9659258262890683122, 1.000000000000000000, 0.9659258262890683122, 1.000000000000000000, 0.9659258262890683122, 1.000000000000000000, 0.9659258262890683122, 1.000000000000000000, 0.9659258262890683122, 1.000000000000000000, 0.9659258262890683122, 1.000000000000000000, 0.9659258262890683122, 1.000000000000000000, 0.9659258262890683122, 1.000000000000000000, 0.9659258262890683122, 1.000000000000000000, 0.9659258262890683122, 1.000000000000000000, 0.9659258262890683122, 1.000000000000000000, 0.9659258262890683122, 1.000000000000000000, 0.9659258262890683122, 1.000000000000000000, 0.9659258262890683122, 1.000000000000000000, 0.9659258262890683122, 1.000000000000000000, 0.9659258262890683122, 1.000000000000000000, 0.9659258262890683122, 1.000000000000000000, 0.9659258262890683122, 1.000000000000000000, 0.9659258262890683122, 1.000000000000000000, 0.9659258262890683122, 1.000000000000000000, 0.9659258262890683122, 1.000000000000000000, 0.9659258262890683122, 1.000000000000000000, 0.9659258262890683122, 1.000000000000000000, 0.9659258262890683122, 1.000000000000000000, 0.9659258262890683122, 1.000000000000000000, 0.9659258262890683122, 1.000000000000000000, 0.9659258262890683122, 1.000000000000000000, 0.9659258262890683122, 1.000000000000000000, 0.9659258262890683122, 1.000000000000000000, 0.9659258262890683122, 1.000000000000000000, 0.9659258262890683122, 1.000000000000000000, 0.9659258262890683122, 1.000000000000000000, 0.9659258262890683122, 1.000000000000000000, 0.9659258262890683122, 1.000000000000000000, 0.9659258262890683122, 1.000000000000000000, 0.9659258262890683122, 1.000000000000000000, 0.9659258262890683122, 1.000000000000000000, 0.9659258262890683122, 1.000000000000000000, 0.9659258262890683122, 1.000000000000000000, 0.9659258262890683122, 1.000000000000000000, 0.9659258262890683122, 1.000000000000000000, 0.9659258262890683122, 1.000000000000000000, 0.9659258262890683122, 1.000000000000000000, 0.9659258262890683122, 1.000000000000000000, 0.9659258262890683122, 1.000000000000000000),
 ( 1.000000000000000000, 0.9659258262890683122, 1.000000000000000000, 0.9659258262890683122, 1.000000000000000000, 0.9659258262890683122, 1.000000000000000000, 0.9659258262890683122, 1.000000000000000000, 0.9659258262890683122, 1.000000000000000000, 0.9659258262890683122, 1.000000000000000000, 0.9659258262890683122, 1.000000000000000000, 0.9659258262890683122, 1.000000000000000000, 0.9659258262890683122, 1.000000000000000000, 0.9659258262890683122, 1.000000000000000000, 0.9659258262890683122, 1.000000000000000000, 0.9659258262890683122, 1.000000000000000000, 0.9659258262890683122, 1.000000000000000000, 0.9659258262890683122, 1.000000000000000000, 0.9659258262890683122, 1.000000000000000000, 0.9659258262890683122, 1.000000000000000000, 0.9659258262890683122, 1.000000000000000000, 0.9659258262890683122, 1.000000000000000000, 0.9659258262890683122, 1.000000000000000000, 0.9659258262890683122, 1.000000000000000000, 0.9659258262890683122, 1.000000000000000000, 0.9659258262890683122, 1.000000000000000000, 0.9659258262890683122, 1.000000000000000000, 0.9659258262890683122, 1.000000000000000000, 0.9659258262890683122, 1.000000000000000000, 0.9659258262890683122, 1.000000000000000000, 0.9659258262890683122, 1.000000000000000000, 0.9659258262890683122, 1.000000000000000000, 0.9659258262890683122, 1.000000000000000000, 0.9659258262890683122, 1.000000000000000000, 0.9659258262890683122, 1.000000000000000000, 0.9659258262890683122, 1.000000000000000000, 0.9659258262890683122, 1.000000000000000000, 0.9659258262890683122, 1.000000000000000000, 0.9659258262890683122, 1.000000000000000000, 0.9659258262890683122, 1.000000000000000000, 0.9659258262890683122, 1.000000000000000000, 0.9659258262890683122, 1.000000000000000000, 0.9659258262890683122, 1.000000000000000000, 0.9659258262890683122, 1.000000000000000000, 0.9659258262890683122, 1.000000000000000000, 0.9659258262890683122, 1.000000000000000000, 0.9659258262890683122, 1.000000000000000000, 0.9659258262890683122, 1.000000000000000000, 0.9659258262890683122, 1.000000000000000000, 0.9659258262890683122, 1.000000000000000000, 0.9659258262890683122, 1.000000000000000000, 0.9659258262890683122, 1.000000000000000000, 0.9659258262890683122, 1.000000000000000000, 0.9659258262890683122, 1.000000000000000000, 0.9659258262890683122, 1.000000000000000000, 0.9659258262890683122, 1.000000000000000000, 0.9659258262890683122, 1.000000000000000000, 0.9659258262890683122, 1.000000000000000000, 0.9659258262890683122, 1.000000000000000000, 0.9659258262890683122, 1.000000000000000000, 0.9659258262890683122, 1.000000000000000000, 0.9659258262890683122, 1.000000000000000000, 0.9659258262890683122, 1.000000000000000000, 0.9659258262890683122, 1.000000000000000000, 0.9659258262890683122, 1.000000000000000000, 0.9659258262890683122, 1.000000000000000000, 0.9659258262890683122, 1.000000000000000000, 0.9659258262890683122, 1.000000000000000000, 0.9659258262890683122, 1.000000000000000000, 0.9659258262890683122, 1.000000000000000000, 0.9659258262890683122, 1.000000000000000000, 0.9659258262890683122, 1.000000000000000000, 0.9659258262890683122, 1.000000000000000000, 0.9659258262890683122, 1.000000000000000000, 0.9659258262890683122, 1.000000000000000000, 0.9659258262890683122, 1.000000000000000000, 0.9659258262890683122, 1.000000000000000000, 0.9659258262890683122, 1.000000000000000000, 0.9659258262890683122, 1.000000000000000000, 0.9659258262890683122, 1.000000000000000000, 0.9659258262890683122, 1.000000000000000000, 0.9659258262890683122, 1.000000000000000000, 0.9659258262890683122, 1.000000000000000000, 0.9659258262890683122, 1.000000000000000000, 0.9659258262890683122, 1.000000000000000000, 0.9659258262890683122, 1.000000000000000000, 0.9659258262890683122, 1.000000000000000000, 0.9659258262890683122, 1.000000000000000000, 0.9659258262890683122, 1.000000000000000000, 0.9659258262890683122, 1.000000000000000000, 0.9659258262890683122, 1.000000000000000000, 0.9659258262890683122, 1.000000000000000000, 0.9659258262890683122, 1.000000000000000000, 0.9659258262890683122, 1.000000000000000000, 0.9659258262890683122, 1.000000000000000000, 0.9659258262890683122, 1.000000000000000000, 0.9659258262890683122, 1.000000000000000000, 0.9659258262890683122, 1.000000000000000000, 0.9659258262890683122, 1.000000000000000000, 0.9659258262890683122, 1.000000000000000000, 0.9659258262890683122, 1.000000000000000000, 0.9659258262890683122, 1.000000000000000000, 0.9659258262890683122, 1.000000000000000000, 0.9659258262890683122, 1.000000000000000000, 0.9659258262890683122, 1.000000000000000000, 0.9659258262890683122, 1.000000000000000000, 0.9659258262890683122, 1.000000000000000000, 0.9659258262890683122, 1.000000000000000000, 0.9659258262890683122, 1.000000000000000000, 0.9659258262890683122, 1.000000000000000000, 0.9659258262890683122, 1.000000000000000000, 0.9659258262890683122, 1.000000000000000000, 0.9659258262890683122, 1.000000000000000000, 0.9659258262890683122, 1.000000000000000000, 0.9659258262890683122, 1.000000000000000000, 0.9659258262890683122, 1.000000000000000000, 0.9659258262890683122, 1.000000000000000000, 0.9659258262890683122, 1.000000000000000000, 0.9659258262890683122, 1.000000000000000000, 0.9659258262890683122, 1.000000000000000000, 0.9659258262890683122, 1.000000000000000000, 0.9659258262890683122, 1.000000000000000000, 0.9659258262890683122, 1.000000000000000000, 0.9659258262890683122, 1.000000000000000000, 0.9659258262890683122, 1.000000000000000000, 0.9659258262890683122, 1.000000000000000000, 0.9659258262890683122, 1.000000000000000000, 0.9659258262890683122, 1.000000000000000000, 0.9659258262890683122, 1.000000000000000000, 0.9659258262890683122, 1.000000000000000000, 0.9659258262890683122, 1.000000000000000000, 0.9659258262890683122, 1.000000000000000000, 0.9659258262890683122, 1.000000000000000000, 0.9659258262890683122, 1.000000000000000000, 0.9659258262890683122, 1.000000000000000000, 0.9659258262890683122, 1.000000000000000000, 0.9659258262890683122, 1.000000000000000000, 0.9659258262890683122, 1.000000000000000000, 0.9659258262890683122, 1.000000000000000000, 0.9659258262890683122, 1.000000000000000000, 0.9659258262890683122, 1.000000000000000000, 0.9659258262890683122, 1.000000000000000000, 0.9659258262890683122, 1.000000000000000000, 0.9659258262890683122, 1.000000000000000000, 0.9659258262890683122, 1.000000000000000000, 0.9659258262890683122, 1.000000000000000000, 0.9659258262890683122, 1.000000000000000000, 0.9659258262890683122, 1.000000000000000000, 0.9659258262890683122, 1.000000000000000000, 0.9659258262890683122, 1.000000000000000000, 0.9659258262890683122, 1.000000000000000000, 0.9659258262890683122, 1.000000000000000000, 0.9659258262890683122, 1.000000000000000000, 0.9659258262890683122, 1.000000000000000000, 0.9659258262890683122, 1.000000000000000000, 0.9659258262890683122, 1.000000000000000000, 0.9659258262890683122, 1.000000000000000000, 0.9659258262890683122, 1.000000000000000000, 0.9659258262890683122, 1.000000000000000000, 0.9659258262890683122, 1.000000000000000000, 0.9659258262890683122, 1.000000000000000000, 0.9659258262890683122, 1.000000000000000000, 0.9659258262890683122, 1.000000000000000000, 0.9659258262890683122, 1.000000000000000000, 0.9659258262890683122, 1.000000000000000000, 0.9659258262890683122, 1.000000000000000000, 0.9659258262890683122, 1.000000000000000000, 0.9659258262890683122, 1.000000000000000000, 0.9659258262890683122, 1.000000000000000000, 0.9659258262890683122, 1.000000000000000000, 0.9659258262890683122, 1.000000000000000000, 0.9659258262890683122, 1.000000000000000000, 0.9659258262890683122, 1.000000000000000000, 0.9659258262890683122, 1.000000000000000000, 0.9659258262890683122, 1.000000000000000000, 0.9659258262890683122, 1.000000000000000000, 0.9659258262890683122, 1.000000000000000000, 0.9659258262890683122, 1.000000000000000000, 0.9659258262890683122, 1.000000000000000000, 0.9659258262890683122, 1.000000000000000000, 0.9659258262890683122, 1.000000000000000000, 0.9659258262890683122, 1.000000000000000000, 0.9659258262890683122, 1.000000000000000000, 0.9659258262890683122, 1.000000000000000000, 0.9659258262890683122, 1.000000000000000000, 0.9659258262890683122, 1.000000000000000000, 0.9659258262890683122, 1.000000000000000000, 0.9659258262890683122, 1.000000000000000000, 0.9659258262890683122, 1.000000000000000000, 0.9659258262890683122, 1.000000000000000000, 0.9659258262890683122, 1.000000000000000000, 0.9659258262890683122, 1.000000000000000000, 0.9659258262890683122, 1.000000000000000000, 0.9659258262890683122, 1.000000000000000000, 0.9659258262890683122, 1.000000000000000000, 0.9659258262890683122, 1.000000000000000000, 0.9659258262890683122, 1.000000000000000000, 0.9659258262890683122, 1.000000000000000000, 0.9659258262890683122, 1.000000000000000000, 0.9659258262890683122, 1.000000000000000000, 0.9659258262890683122, 1.000000000000000000, 0.9659258262890683122, 1.000000000000000000, 0.9659258262890683122, 1.000000000000000000, 0.9659258262890683122, 1.000000000000000000, 0.9659258262890683122, 1.000000000000000000, 0.9659258262890683122, 1.000000000000000000, 0.9659258262890683122, 1.000000000000000000, 0.9659258262890683122, 1.000000000000000000, 0.9659258262890683122, 1.000000000000000000, 0.9659258262890683122, 1.000000000000000000, 0.9659258262890683122, 1.000000000000000000, 0.9659258262890683122, 1.000000000000000000, 0.9659258262890683122, 1.000000000000000000, 0.9659258262890683122, 1.000000000000000000, 0.9659258262890683122, 1.000000000000000000, 0.9659258262890683122, 1.000000000000000000, 0.9659258262890683122, 1.000000000000000000, 0.9659258262890683122, 1.000000000000000000, 0.9659258262890683122, 1.000000000000000000, 0.9659258262890683122, 1.000000000000000000, 0.9659258262890683122, 1.000000000000000000, 0.9659258262890683122, 1.000000000000000000, 0.9659258262890683122, 1.000000000000000000, 0.9659258262890683122, 1.000000000000000000, 0.9659258262890683122, 1.000000000000000000, 0.9659258262890683122, 1.000000000000000000, 0.9659258262890683122, 1.000000000000000000, 0.9659258262890683122, 1.000000000000000000, 0.9659258262890683122, 1.000000000000000000, 0.9659258262890683122, 1.000000000000000000, 0.9659258262890683122, 1.000000000000000000, 0.9659258262890683122, 1.000000000000000000, 0.9659258262890683122, 1.000000000000000000, 0.9659258262890683122, 1.000000000000000000, 0.9659258262890683122, 1.000000000000000000, 0.9659258262890683122, 1.000000000000000000, 0.9659258262890683122, 1.000000000000000000, 0.9659258262890683122, 1.000000000000000000, 0.9659258262890683122, 1.000000000000000000, 0.9659258262890683122, 1.000000000000000000, 0.9659258262890683122, 1.000000000000000000, 0.9659258262890683122, 1.000000000000000000, 0.9659258262890683122, 1.000000000000000000, 0.9659258262890683122, 1.000000000000000000, 0.9659258262890683122, 1.000000000000000000, 0.9659258262890683122, 1.000000000000000000, 0.9659258262890683122, 1.000000000000000000, 0.9659258262890683122, 1.000000000000000000, 0.9659258262890683122, 1.000000000000000000, 0.9659258262890683122, 1.000000000000000000, 0.9659258262890683122, 1.000000000000000000, 0.9659258262890683122, 1.000000000000000000, 0.9659258262890683122, 1.000000000000000000, 0.9659258262890683122, 1.000000000000000000, 0.9659258262890683122, 1.000000000000000000, 0.9659258262890683122, 1.000000000000000000, 0.9659258262890683122, 1.000000000000000000, 0.9659258262890683122, 1.000000000000000000, 0.9659258262890683122, 1.000000000000000000) ) ) 
 REPRESENTATION_ITEM ( '' )  SURFACE ( )  );
#62609 = CARTESIAN_POINT ( 'NONE',  ( -0.2867679344610364334, -0.2867679344610367109, -1.153543307086613900 ) ) ;
#62610 = CARTESIAN_POINT ( 'NONE',  ( -0.5446194225721777693, -0.08942795157527998196, 0.3641732283464567121 ) ) ;
#62611 = ORIENTED_EDGE ( 'NONE', *, *, #16161, .F. ) ;
#62612 = CARTESIAN_POINT ( 'NONE',  ( 0.2891555358219910499, -0.2891555358219909944, -1.515748031496063186 ) ) ;
#62613 = ORIENTED_EDGE ( 'NONE', *, *, #53024, .F. ) ;
#62614 = CARTESIAN_POINT ( 'NONE',  ( -1.450131233595799651, -0.5511811023622046335, 0.09757992244046803654 ) ) ;
#62615 = CARTESIAN_POINT ( 'NONE',  ( -0.9645669291338575535, 0.1660481256975883668, -0.3530559997133364547 ) ) ;
#62616 = CARTESIAN_POINT ( 'NONE',  ( -0.9383202099737524282, -0.3162353388693409650, -0.4822834645669289433 ) ) ;
#62617 = DIRECTION ( 'NONE',  ( 0.000000000000000000, 1.000000000000000000, 0.000000000000000000 ) ) ;
#62618 = CARTESIAN_POINT ( 'NONE',  ( -0.8989501312335946848, 0.2952755905511810774, -0.1292274648535930714 ) ) ;
#62619 = CARTESIAN_POINT ( 'NONE',  ( -0.7480314960629914633, 0.2952755905511811885, 0.000000000000000000 ) ) ;
#62620 = CARTESIAN_POINT ( 'NONE',  ( 0.4724409448818898682, 2.892866454678787531E-17, -1.220472440944881942 ) ) ;
#62621 = CARTESIAN_POINT ( 'NONE',  ( -1.712598425196849572, 0.1660481256975885056, 0.3530559997133364547 ) ) ;
#62622 = CARTESIAN_POINT ( 'NONE',  ( 0.6364829396325465405, -0.2845877964562161244, -0.3641732283464567121 ) ) ;
#62623 = DIRECTION ( 'NONE',  ( 0.000000000000000000, 0.000000000000000000, 1.000000000000000000 ) ) ;
#62624 = CARTESIAN_POINT ( 'NONE',  ( -0.1958661417322836718, 0.3392501089628017219, 0.05971128608923875758 ) ) ;
#62625 = CARTESIAN_POINT ( 'NONE',  ( 0.1902887139107617975, 0.1771653543307087630, 0.09757992244046791164 ) ) ;
#62626 = CARTESIAN_POINT ( 'NONE',  ( -0.4921259842519677963, 0.1660481256975883668, -0.3530559997133364547 ) ) ;
#62627 = CARTESIAN_POINT ( 'NONE',  ( 3.908697805448793972, 1.475019653495670546, 0.4713285578992283953 ) ) ;
#62628 = CARTESIAN_POINT ( 'NONE',  ( -0.07217847769028787330, -0.05778040916215522460, 0.4822834645669289988 ) ) ;
#62629 = ORIENTED_EDGE ( 'NONE', *, *, #733, .F. ) ;
#62630 = CARTESIAN_POINT ( 'NONE',  ( 0.2925321140481932369, 0.2925321140481932369, -2.185039370078739829 ) ) ;
#62631 = CARTESIAN_POINT ( 'NONE',  ( -0.8464566929133849893, 0.1012011053420777407, 0.2882089793578256898 ) ) ;
#62632 = ORIENTED_EDGE ( 'NONE', *, *, #39907, .F. ) ;
#62633 = CARTESIAN_POINT ( 'NONE',  ( 0.1070741851644054776, -0.3996062992125984925, -1.736876640419947604 ) ) ;
#62634 = CARTESIAN_POINT ( 'NONE',  ( -0.2032823926810630732, 0.2142011206082509445, 0.1316721176867485799 ) ) ;
#62635 = CARTESIAN_POINT ( 'NONE',  ( -1.332020997375327642, -0.2845877964562161244, -0.3641732283464567121 ) ) ;
#62636 = CARTESIAN_POINT ( 'NONE',  ( -0.7611548556430438595, 0.2306618581243848609, 0.2411417322834645549 ) ) ;
#62637 = CARTESIAN_POINT ( 'NONE',  ( -0.4091458600556402980, -0.2362204724409451284, -0.3674540682414698112 ) ) ;
#62638 = CARTESIAN_POINT ( 'NONE',  ( -0.4109299095364690735, 1.299823618673216830, 3.915510462780284140 ) ) ;
#62639 = CARTESIAN_POINT ( 'NONE',  ( 0.2867679344610365999, -0.2867679344610365444, 0.06692913385826775030 ) ) ;
#62640 = CARTESIAN_POINT ( 'NONE',  ( 1.463254593175853824, -0.6692913385826771977, 0.1292274648535927661 ) ) ;
#62641 = CARTESIAN_POINT ( 'NONE',  ( 0.6496062992125991586, 0.1660481256975885056, 0.3530559997133364547 ) ) ;
#62642 = CARTESIAN_POINT ( 'NONE',  ( 0.3805774278215230400, -0.4281496062992124485, 0.4176697321401328655 ) ) ;
#62643 = CARTESIAN_POINT ( 'NONE',  ( -1.233595800524933894, -0.5023911411419708095, -0.1820866141732282451 ) ) ;
#62644 = AXIS2_PLACEMENT_3D ( 'NONE', #50837, #5004, #57148 ) ;
#62645 = VECTOR ( 'NONE', #24439, 39.37007874015748143 ) ;
#62646 = CARTESIAN_POINT ( 'NONE',  ( -0.4068241469816267775, 0.05413385826771626580, -0.4176697321401330321 ) ) ;
#62647 = CARTESIAN_POINT ( 'NONE',  ( 0.3458507752293908943, 0.3458507752293908943, -2.261811023622047223 ) ) ;
#62648 = CARTESIAN_POINT ( 'NONE',  ( -0.7152230971128602510, -0.05778040916215560624, -0.4822834645669293319 ) ) ;
#62649 = EDGE_CURVE ( 'NONE', #55865, #49969, #63116, .T. ) ;
#62650 = CARTESIAN_POINT ( 'NONE',  ( 0.1058382717557499880, 0.3949938075777409408, -2.432414698162729927 ) ) ;
#62651 = CARTESIAN_POINT ( 'NONE',  ( 1.423884514435696191, -0.08942795157527998196, 0.3641732283464567121 ) ) ;
#62652 = CARTESIAN_POINT ( 'NONE',  ( -0.5052493438320203589, -0.5511811023622046335, 0.09757992244046803654 ) ) ;
#62653 = CARTESIAN_POINT ( 'NONE',  ( 1.128608923884515169, -0.5023911411419708095, -0.1820866141732282451 ) ) ;
#62654 = CARTESIAN_POINT ( 'NONE',  ( -1.627296587926508442, -0.6046776061558809534, -0.2411417322834644161 ) ) ;
#62655 = CARTESIAN_POINT ( 'NONE',  ( -1.161417322834644716, 0.07958543189024085140, 0.2665933059059887866 ) ) ;
#62656 = CARTESIAN_POINT ( 'NONE',  ( -3.224202737261815166, 2.716535433070866645, -0.5314960629921260393 ) ) ;
#62657 = CARTESIAN_POINT ( 'NONE',  ( 0.4396325459317593221, 0.1771653543307087075, -0.09757992244046823083 ) ) ;
#62658 = CARTESIAN_POINT ( 'NONE',  ( -0.2296587926509179312, -0.05778040916215522460, 0.4822834645669289988 ) ) ;
#62659 = CIRCLE ( 'NONE', #60011, 0.1937007874015748143 ) ;
#62660 = CARTESIAN_POINT ( 'NONE',  ( -1.901586028222560953, 1.118719813955022069, 0.2236424093447385852 ) ) ;
#62661 = CARTESIAN_POINT ( 'NONE',  ( 0.07874015748031558404, -0.1870078740157479769, 0.3641732283464567677 ) ) ;
#62662 = CARTESIAN_POINT ( 'NONE',  ( -1.646981627296586703, -0.2845877964562161244, -0.3641732283464567121 ) ) ;
#62663 = CARTESIAN_POINT ( 'NONE',  ( 0.7020997375328090762, -0.3162353388693405765, 0.4822834645669290543 ) ) ;
#62664 = DIRECTION ( 'NONE',  ( 0.000000000000000000, 0.000000000000000000, -1.000000000000000000 ) ) ;
#62665 = CARTESIAN_POINT ( 'NONE',  ( 1.568241469816273437, -0.2845877964562159024, 0.3641732283464567677 ) ) ;
#62666 = CARTESIAN_POINT ( 'NONE',  ( -1.108923884514435132, -0.3162353388693405765, 0.4822834645669290543 ) ) ;
#62667 = CARTESIAN_POINT ( 'NONE',  ( -0.3805774278215216522, -0.004921259842519576551, 0.3153832671262227771 ) ) ;
#62668 = CARTESIAN_POINT ( 'NONE',  ( 1.436417322834645516, 0.4405861044731112508, -0.3149606299212598381 ) ) ;
#62669 = CARTESIAN_POINT ( 'NONE',  ( 0.3477690288713918276, 0.1771653543307087630, 0.09757992244046791164 ) ) ;
#62670 = CARTESIAN_POINT ( 'NONE',  ( -1.240157480314959759, 0.1660481256975885056, 0.3530559997133364547 ) ) ;
#62671 = CARTESIAN_POINT ( 'NONE',  ( -0.3346456692913377662, 0.1660481256975883668, -0.3530559997133364547 ) ) ;
#62672 = CARTESIAN_POINT ( 'NONE',  ( -0.3996062992125985480, -7.340648628747423112E-17, -0.5885826771653542844 ) ) ;
#62673 = CARTESIAN_POINT ( 'NONE',  ( 0.1958661417322836440, -0.3392501089628017219, -2.381233595800524849 ) ) ;
#62674 = CARTESIAN_POINT ( 'NONE',  ( 0.4658792650918640033, -0.2845877964562159024, 0.3641732283464567677 ) ) ;
#62675 = CARTESIAN_POINT ( 'NONE',  ( -0.4199475065616791736, -0.6046776061558807314, 0.2411417322834647770 ) ) ;
#62676 = CARTESIAN_POINT ( 'NONE',  ( -0.6955380577427815458, 0.05413385826771666132, 0.4176697321401328100 ) ) ;
#62677 = CARTESIAN_POINT ( 'NONE',  ( -0.6824146981627288167, 0.1283753931104748280, 0.1820866141732283561 ) ) ;
#62678 = CARTESIAN_POINT ( 'NONE',  ( -3.929911103084700486, 1.125660643012857731, 0.2377022791102254007 ) ) ;
#62679 = CARTESIAN_POINT ( 'NONE',  ( -0.02624671916010428221, 0.2306618581243847221, -0.2411417322834647770 ) ) ;
#62680 = CARTESIAN_POINT ( 'NONE',  ( -1.049868766404198794, 0.1283753931104746893, -0.1820866141732285504 ) ) ;
#62681 = CARTESIAN_POINT ( 'NONE',  ( -1.535433070866141225, -0.6692913385826771977, 8.415575281601705876E-17 ) ) ;
#62682 = CARTESIAN_POINT ( 'NONE',  ( 0.2230971128608929543, 0.009842519685039144428, -0.3409548833797004797 ) ) ;
#62683 = ORIENTED_EDGE ( 'NONE', *, *, #21285, .T. ) ;
#62684 = CARTESIAN_POINT ( 'NONE',  ( -1.384514435695537005, 0.1771653543307087630, 0.09757992244046791164 ) ) ;
#62685 = CARTESIAN_POINT ( 'NONE',  ( -1.410761154855642463, -0.05778040916215522460, 0.4822834645669289988 ) ) ;
#62686 = CARTESIAN_POINT ( 'NONE',  ( -1.043307086614172707, 0.1660481256975883668, -0.3530559997133364547 ) ) ;
#62687 = CARTESIAN_POINT ( 'NONE',  ( 1.561679790026247350, -0.4281496062992124485, 0.4176697321401328655 ) ) ;
#62688 = CARTESIAN_POINT ( 'NONE',  ( -0.3917322834645669549, -0.1049643490035306603, -1.390419947506561504 ) ) ;
#62689 = DIRECTION ( 'NONE',  ( -0.000000000000000000, 0.000000000000000000, -1.000000000000000000 ) ) ;
#62690 = CARTESIAN_POINT ( 'NONE',  ( 1.095800524934383846, -0.05778040916215560624, -0.4822834645669293319 ) ) ;
#62691 = CARTESIAN_POINT ( 'NONE',  ( 0.6364829396325465405, -0.3162353388693409650, -0.4822834645669289433 ) ) ;
#62692 = DIRECTION ( 'NONE',  ( 0.000000000000000000, 1.000000000000000000, 0.000000000000000000 ) ) ;
#62693 = AXIS2_PLACEMENT_3D ( 'NONE', #27132, #58701, #47313 ) ;
#62694 = AXIS2_PLACEMENT_3D ( 'NONE', #37319, #62991, #22624 ) ;
#62696 = AXIS2_PLACEMENT_3D ( 'NONE', #636, #72584, #14932 ) ;
#62695 = CARTESIAN_POINT ( 'NONE',  ( -0.2925321140481930149, -0.2925321140481933480, -2.340551181102362488 ) ) ;
#62697 = CARTESIAN_POINT ( 'NONE',  ( 1.377952755905512472, -0.5511811023622047445, 6.969142054262312111E-17 ) ) ;
#62698 = CARTESIAN_POINT ( 'NONE',  ( 0.3460692066303959757, -0.1998031496062991907, -1.049868766404199460 ) ) ;
#62699 = ORIENTED_EDGE ( 'NONE', *, *, #25507, .F. ) ;
#62700 = CARTESIAN_POINT ( 'NONE',  ( -0.8595800524934373854, -0.08942795157527998196, 0.3641732283464567121 ) ) ;
#62701 = CARTESIAN_POINT ( 'NONE',  ( 0.1049643490035303689, 0.3917322834645670104, -2.820209973753280419 ) ) ;
#62702 = ORIENTED_EDGE ( 'NONE', *, *, #12540, .T. ) ;
#62703 = CARTESIAN_POINT ( 'NONE',  ( 0.5708661417322841158, -0.5400638737290845981, -0.3530559997133363437 ) ) ;
#62704 = CARTESIAN_POINT ( 'NONE',  ( -0.5971128608923877978, 0.2952755905511811885, 0.1292274648535926551 ) ) ;
#62705 =( REPRESENTATION_RELATIONSHIP ('NONE','NONE', #79348, #33107 ) REPRESENTATION_RELATIONSHIP_WITH_TRANSFORMATION ( #4765 )SHAPE_REPRESENTATION_RELATIONSHIP( ) );
#62706 = CARTESIAN_POINT ( 'NONE',  ( -1.299212598425196097, 0.2952755905511811885, 0.000000000000000000 ) ) ;
#62707 = CARTESIAN_POINT ( 'NONE',  ( 1.036745406824147731, 0.05413385826771666132, 0.4176697321401328100 ) ) ;
#62708 = CARTESIAN_POINT ( 'NONE',  ( -1.620734908136482577, 0.1771653543307087630, 0.09757992244046791164 ) ) ;
#62709 = CARTESIAN_POINT ( 'NONE',  ( -1.559171609364246924, 0.3937007874015747699, 0.4177787735906735578 ) ) ;
#62710 = CARTESIAN_POINT ( 'NONE',  ( -0.09186351706036663400, -0.4281496062992124485, 0.4176697321401328655 ) ) ;
#62711 = CARTESIAN_POINT ( 'NONE',  ( -1.364829396325458521, -0.6046776061558807314, 0.2411417322834647770 ) ) ;
#62712 = CARTESIAN_POINT ( 'NONE',  ( -1.607611548556429737, 0.2952755905511810774, -0.1292274648535930714 ) ) ;
#62713 = CARTESIAN_POINT ( 'NONE',  ( 0.4744094488189065095, 1.537401574803149984, -2.554262525012259477 ) ) ;
#62714 = CARTESIAN_POINT ( 'NONE',  ( -0.3392501089628019995, 0.1958661417322832277, -2.788057742782152459 ) ) ;
#62715 = CARTESIAN_POINT ( 'NONE',  ( 0.6627296587926517768, -0.5511811023622048555, -0.09757992244046775898 ) ) ;
#62716 = VERTEX_POINT ( 'NONE', #70246 ) ;
#62717 = CARTESIAN_POINT ( 'NONE',  ( -0.3420746716998661618, 0.1974969037888702206, -0.02624671916010504202 ) ) ;
#62718 = ORIENTED_EDGE ( 'NONE', *, *, #78043, .T. ) ;
#62720 = CIRCLE ( 'NONE', #6225, 1.198416298106748767 ) ;
#62719 = CARTESIAN_POINT ( 'NONE',  ( 0.1771653543307093182, 0.07958543189024085140, 0.2665933059059887866 ) ) ;
#62721 = CARTESIAN_POINT ( 'NONE',  ( -1.646981627296586703, -0.3162353388693409650, -0.4822834645669289433 ) ) ;
#62722 = CARTESIAN_POINT ( 'NONE',  ( 0.6824146981627303710, 0.2306618581243847221, -0.2411417322834647770 ) ) ;
#62723 = CARTESIAN_POINT ( 'NONE',  ( 0.4593175853018379162, -0.4281496062992124485, 0.4176697321401328655 ) ) ;
#62724 = CARTESIAN_POINT ( 'NONE',  ( -0.4855643044619415427, -0.4281496062992124485, 0.4176697321401328655 ) ) ;
#62725 = CARTESIAN_POINT ( 'NONE',  ( -0.1049643490035302301, -0.3917322834645671770, -1.328759473262154378 ) ) ;
#62726 = CARTESIAN_POINT ( 'NONE',  ( -1.404199475065615932, -0.4281496062992127816, -0.4176697321401328100 ) ) ;
#62727 = CARTESIAN_POINT ( 'NONE',  ( 0.3917322834645670104, 2.398668435337828261E-17, -2.722440944881889369 ) ) ;
#62728 = CARTESIAN_POINT ( 'NONE',  ( 1.417322834645670104, -0.1870078740157479769, 0.3641732283464567677 ) ) ;
#62729 = CARTESIAN_POINT ( 'NONE',  ( -1.227034120734907141, -0.6692913385826773087, -0.1292274648535924053 ) ) ;
#62730 = CARTESIAN_POINT ( 'NONE',  ( 0.6824146981627303710, -0.6046776061558807314, 0.2411417322834647770 ) ) ;
#62731 = CARTESIAN_POINT ( 'NONE',  ( 1.056430446194226658, 0.2952755905511811885, 0.1292274648535926551 ) ) ;
#62732 = CARTESIAN_POINT ( 'NONE',  ( -0.1998031496062994683, 0.3460692066303958092, -0.9580052493438320216 ) ) ;
#62733 = CARTESIAN_POINT ( 'NONE',  ( -1.227034120734907585, 0.2952755905511811885, 0.1292274648535926551 ) ) ;
#62734 = CARTESIAN_POINT ( 'NONE',  ( -0.2925321140481930149, -0.2925321140481933480, -0.4507874015748031815 ) ) ;
#62735 = B_SPLINE_CURVE_WITH_KNOTS ( 'NONE', 3,
 ( #82171, #24487, #37531, #63207, #31211, #56879, #82572 ),
 .UNSPECIFIED., .F., .F.,
 ( 4, 3, 4 ),
 ( 6.162975822039154730E-33, 0.001246232571205221906, 0.002492492258783241162 ),
 .UNSPECIFIED. ) ;
#62736 = CARTESIAN_POINT ( 'NONE',  ( 0.09186351706036799403, -0.4281496062992127816, -0.4176697321401328100 ) ) ;
#62737 = CARTESIAN_POINT ( 'NONE',  ( 0.1998031496062994405, -0.3460692066303958092, -2.454068241469816058 ) ) ;
#62738 = ADVANCED_FACE ( 'NONE', ( #45395 ), #361, .F. ) ;
#62739 = CARTESIAN_POINT ( 'NONE',  ( 4.797336870675656522E-17, -0.3917322834645670104, -1.738188976377952777 ) ) ;
#62740 = CARTESIAN_POINT ( 'NONE',  ( -1.561679790026246017, -0.3690944881889765550, -0.3153832671262227771 ) ) ;
#62741 = CARTESIAN_POINT ( 'NONE',  ( 0.4265091863517067594, 0.1771653543307087630, 0.09757992244046791164 ) ) ;
#62742 = CARTESIAN_POINT ( 'NONE',  ( 0.8530183727034126306, 0.05413385826771626580, -0.4176697321401330321 ) ) ;
#62743 = CARTESIAN_POINT ( 'NONE',  ( -1.157146581871515012E-16, 0.4724409448818898682, -1.021653543307086576 ) ) ;
#62744 = CARTESIAN_POINT ( 'NONE',  ( 0.7742782152230979209, -0.004921259842519870586, -0.3153832671262229437 ) ) ;
#62745 = CARTESIAN_POINT ( 'NONE',  ( 0.5511811023622054106, -0.1870078740157480879, -0.4822834645669291653 ) ) ;
#62746 = EDGE_CURVE ( 'NONE', #55552, #20068, #65537, .T. ) ;
#62747 = CARTESIAN_POINT ( 'NONE',  ( 0.3420746716998660508, 0.1974969037888705814, -0.8379265091863515869 ) ) ;
#62748 = CARTESIAN_POINT ( 'NONE',  ( -0.6561679790026240244, -0.6046776061558807314, 0.2411417322834647770 ) ) ;
#62749 = CARTESIAN_POINT ( 'NONE',  ( 0.2362204724409451007, -0.4091458600556402980, -1.113517060367454015 ) ) ;
#62750 = CARTESIAN_POINT ( 'NONE',  ( 0.9317585301837276734, -0.3690944881889763329, 0.3153832671262228327 ) ) ;
#62751 = CARTESIAN_POINT ( 'NONE',  ( 0.05249343832021075018, 0.2306618581243847221, -0.2411417322834647770 ) ) ;
#62752 = CARTESIAN_POINT ( 'NONE',  ( 0.000000000000000000, 0.000000000000000000, -2.755905511811024056 ) ) ;
#62753 = CARTESIAN_POINT ( 'NONE',  ( -0.1181102362204717315, 0.2952755905511811885, 0.000000000000000000 ) ) ;
#62754 = CARTESIAN_POINT ( 'NONE',  ( 0.2034120734908144990, -0.5511811023622046335, 0.09757992244046803654 ) ) ;
#62755 = CARTESIAN_POINT ( 'NONE',  ( -2.571257611060566717, 1.453715418023197703, -0.4672341690643354584 ) ) ;
#62756 = CARTESIAN_POINT ( 'NONE',  ( -0.3871391076115479057, -0.3162353388693409650, -0.4822834645669289433 ) ) ;
#62757 = CARTESIAN_POINT ( 'NONE',  ( 0.5774278215223103139, -0.5023911411419708095, -0.1820866141732282451 ) ) ;
#62758 = AXIS2_PLACEMENT_3D ( 'NONE', #1207, #39489, #52096 ) ;
#62759 = CARTESIAN_POINT ( 'NONE',  ( -0.04553727834043951039, 1.065153152349019416, -1.442679039838661303 ) ) ;
#62760 = CARTESIAN_POINT ( 'NONE',  ( -0.3460692066303960313, 0.1998031496062989965, -1.835301837270341352 ) ) ;
#62761 = CARTESIAN_POINT ( 'NONE',  ( 0.3412073490813655186, -0.6046776061558809534, -0.2411417322834644161 ) ) ;
#62762 = VECTOR ( 'NONE', #3040, 39.37007874015748143 ) ;
#62763 = VECTOR ( 'NONE', #16158, 39.37007874015748143 ) ;
#62764 = AXIS2_PLACEMENT_3D ( 'NONE', #31312, #50255, #49845 ) ;
#62765 = CARTESIAN_POINT ( 'NONE',  ( 1.194225721784777594, -0.004921259842519576551, 0.3153832671262227771 ) ) ;
#62766 = CARTESIAN_POINT ( 'NONE',  ( -0.4790026246719154557, -0.2845877964562159024, 0.3641732283464567677 ) ) ;
#62767 = CARTESIAN_POINT ( 'NONE',  ( -0.9317585301837263412, -0.004921259842519576551, 0.3153832671262227771 ) ) ;
#62768 = CARTESIAN_POINT ( 'NONE',  ( -0.1377952755905504645, -0.5400638737290845981, -0.3530559997133363437 ) ) ;
#62769 = CARTESIAN_POINT ( 'NONE',  ( 0.2821522309711292364, -0.6692913385826771977, 0.1292274648535927661 ) ) ;
#62770 = CARTESIAN_POINT ( 'NONE',  ( 0.9776902887139113929, -0.5511811023622048555, -0.09757992244046775898 ) ) ;
#62771 = CARTESIAN_POINT ( 'NONE',  ( -1.574803149606298636, -0.1870078740157479769, 0.3641732283464567677 ) ) ;
#62772 = CARTESIAN_POINT ( 'NONE',  ( 1.601049868766404982, 0.1283753931104748280, 0.1820866141732283561 ) ) ;
#62773 = CARTESIAN_POINT ( 'NONE',  ( 0.5839895013123367340, 0.2952755905511811885, 0.1292274648535926551 ) ) ;
#62774 = CARTESIAN_POINT ( 'NONE',  ( 2.362204724409448620, 1.929133858267716661, 0.5118110236220555498 ) ) ;
#62775 = CARTESIAN_POINT ( 'NONE',  ( 0.1837270341207354329, 0.2306618581243848609, 0.2411417322834645549 ) ) ;
#62776 = CARTESIAN_POINT ( 'NONE',  ( 0.1049643490035303689, 0.3917322834645670104, -0.8654855643044619962 ) ) ;
#62777 = CARTESIAN_POINT ( 'NONE',  ( 0.9776902887139113929, -0.6692913385826773087, -0.1292274648535924053 ) ) ;
#62778 = CARTESIAN_POINT ( 'NONE',  ( 0.4658792650918641698, -0.05778040916215560624, -0.4822834645669293319 ) ) ;
#62779 = CARTESIAN_POINT ( 'NONE',  ( -1.033875059083676717, 1.724409448818897905, -0.4359958488159722534 ) ) ;
#62780 = CARTESIAN_POINT ( 'NONE',  ( 0.2755905511811031494, 0.1771653543307087630, 0.000000000000000000 ) ) ;
#62781 = CARTESIAN_POINT ( 'NONE',  ( 1.056430446194226658, 0.2952755905511811885, 0.1292274648535926551 ) ) ;
#62782 = CARTESIAN_POINT ( 'NONE',  ( 0.01312335958005323398, -0.004921259842519576551, 0.3153832671262227771 ) ) ;
#62783 = CARTESIAN_POINT ( 'NONE',  ( -0.4002624671916004129, -0.3162353388693405765, 0.4822834645669290543 ) ) ;
#62784 = CARTESIAN_POINT ( 'NONE',  ( 0.2493438320209980519, -0.4281496062992127816, -0.4176697321401328100 ) ) ;
#62785 = CARTESIAN_POINT ( 'NONE',  ( -0.8202099737532799750, 0.2952755905511810774, -0.1292274648535930714 ) ) ;
#62786 = CARTESIAN_POINT ( 'NONE',  ( -0.3543307086614165824, -0.5511811023622047445, 6.969142054262312111E-17 ) ) ;
#62787 = CARTESIAN_POINT ( 'NONE',  ( 0.4986876640419954376, 0.2306618581243848609, 0.2411417322834645549 ) ) ;
#62788 = CARTESIAN_POINT ( 'NONE',  ( 0.9448818897637802916, -0.1870078740157480601, -0.3641732283464567677 ) ) ;
#62789 = CARTESIAN_POINT ( 'NONE',  ( -0.3805774278215216522, 0.05413385826771666132, 0.4176697321401328100 ) ) ;
#62790 = CARTESIAN_POINT ( 'NONE',  ( 1.168329637866469151, 0.004960608223778500969, -0.3437734562760191848 ) ) ;
#62792 = CARTESIAN_POINT ( 'NONE',  ( 0.2925321140481932369, 0.2925321140481932369, -1.082677165354330562 ) ) ;
#62791 = CARTESIAN_POINT ( 'NONE',  ( -0.6365311798329505999, 1.942272084518551489, 0.5177672855601881396 ) ) ;
#62793 = CARTESIAN_POINT ( 'NONE',  ( 1.640419947506562393, -0.4281496062992124485, 0.4176697321401328655 ) ) ;
#62794 = CARTESIAN_POINT ( 'NONE',  ( -0.1049643490035301885, -0.3917322834645671215, -1.954068241469816281 ) ) ;
#62795 = CARTESIAN_POINT ( 'NONE',  ( -1.062992125984250968, -0.6692913385826771977, 8.415575281601705876E-17 ) ) ;
#62796 = CARTESIAN_POINT ( 'NONE',  ( -0.8727034120734901146, -0.05778040916215560624, -0.4822834645669293319 ) ) ;
#62797 =( BOUNDED_CURVE ( )  B_SPLINE_CURVE ( 1, ( #29049, #47990 ),
 .UNSPECIFIED., .F., .F. ) 
 B_SPLINE_CURVE_WITH_KNOTS ( ( 2, 2 ),
 ( 3.469446951953614189E-18, 0.002000000000000001776 ),
 .UNSPECIFIED. ) 
 CURVE ( )  GEOMETRIC_REPRESENTATION_ITEM ( )  RATIONAL_B_SPLINE_CURVE ( ( 0.9875488213027527884, 0.9875488213027527884 ) ) 
 REPRESENTATION_ITEM ( '' )  );
#62798 = CARTESIAN_POINT ( 'NONE',  ( 0.4724409448818898682, 2.892866454678787531E-17, -0.4330708661417322913 ) ) ;
#62799 = CARTESIAN_POINT ( 'NONE',  ( 0.2891555358219910499, -0.2891555358219909944, -2.933070866141733291 ) ) ;
#62800 = ORIENTED_EDGE ( 'NONE', *, *, #35790, .F. ) ;
#62801 = CARTESIAN_POINT ( 'NONE',  ( 0.4133858267716541968, 0.07958543189024085140, 0.2665933059059887866 ) ) ;
#62802 = CARTESIAN_POINT ( 'NONE',  ( 0.1049643490035304938, -0.3917322834645669549, -1.494750656167978642 ) ) ;
#62803 = CARTESIAN_POINT ( 'NONE',  ( 0.8333333333333340365, 0.2952755905511810774, -0.1292274648535930714 ) ) ;
#62804 = CARTESIAN_POINT ( 'NONE',  ( -0.4091458600556402980, -0.2362204724409451284, -2.572178477690288734 ) ) ;
#62805 = FACE_OUTER_BOUND ( 'NONE', #7243, .T. ) ;
#62806 = CARTESIAN_POINT ( 'NONE',  ( -1.594488188976377563, -0.4536011799217367080, 0.2665933059059888421 ) ) ;
#62807 = CARTESIAN_POINT ( 'NONE',  ( 1.325459317585302665, -0.4281496062992124485, 0.4176697321401328655 ) ) ;
#62808 = CARTESIAN_POINT ( 'NONE',  ( 1.450131233595801428, 0.1771653543307087630, 0.09757992244046791164 ) ) ;
#62809 = CARTESIAN_POINT ( 'NONE',  ( -0.02624671916010428221, 0.2306618581243847221, -0.2411417322834647770 ) ) ;
#62810 = CARTESIAN_POINT ( 'NONE',  ( 0.3392501089628018329, -0.1958661417322834497, -0.8149413141394206139 ) ) ;
#62811 = CARTESIAN_POINT ( 'NONE',  ( -0.4855643044619415427, 0.05413385826771626580, -0.4176697321401330321 ) ) ;
#62812 = CARTESIAN_POINT ( 'NONE',  ( -1.187664041994750175, -0.08942795157528024563, -0.3641732283464568787 ) ) ;
#62813 = CARTESIAN_POINT ( 'NONE',  ( 0.4396325459317590445, -0.6692913385826771977, 0.1292274648535927661 ) ) ;
#62814 = CARTESIAN_POINT ( 'NONE',  ( -0.3280839895013117347, -0.4281496062992124485, 0.4176697321401328655 ) ) ;
#62815 = CARTESIAN_POINT ( 'NONE',  ( -1.220472440944878834, 2.401574803149606474, -0.5309055118110234117 ) ) ;
#62816 = VECTOR ( 'NONE', #20207, 39.37007874015748143 ) ;
#62817 = DIRECTION ( 'NONE',  ( 0.000000000000000000, 0.000000000000000000, -1.000000000000000000 ) ) ;
#62818 = ORIENTED_EDGE ( 'NONE', *, *, #9419, .F. ) ;
#62819 = CARTESIAN_POINT ( 'NONE',  ( 0.3917322834645670659, -0.1049643490035303273, -1.998050811844831243 ) ) ;
#62820 = CARTESIAN_POINT ( 'NONE',  ( 0.5052493438320218022, -0.6692913385826773087, -0.1292274648535924053 ) ) ;
#62821 = CARTESIAN_POINT ( 'NONE',  ( -0.3608923884514428360, -0.6692913385826773087, -0.1292274648535924053 ) ) ;
#62822 = CARTESIAN_POINT ( 'NONE',  ( -1.246719160104985846, -0.4281496062992127816, -0.4176697321401328100 ) ) ;
#62823 = CARTESIAN_POINT ( 'NONE',  ( 0.8005249343832027131, 0.05413385826771666132, 0.4176697321401328100 ) ) ;
#62824 = CARTESIAN_POINT ( 'NONE',  ( 0.6167979002624679463, 0.05413385826771626580, -0.4176697321401330321 ) ) ;
#62825 = CARTESIAN_POINT ( 'NONE',  ( -0.3392501089628019995, 0.1958661417322832277, -1.370734908136483021 ) ) ;
#62826 = CARTESIAN_POINT ( 'NONE',  ( -0.7414698162729651543, 0.2952755905511810774, -0.1292274648535930714 ) ) ;
#62827 = CARTESIAN_POINT ( 'NONE',  ( 0.05249343832021075018, -0.6046776061558807314, 0.2411417322834647770 ) ) ;
#62828 = CARTESIAN_POINT ( 'NONE',  ( -0.5839895013123351797, -0.6692913385826771977, 0.1292274648535927661 ) ) ;
#62829 = CARTESIAN_POINT ( 'NONE',  ( 0.2559055118110243332, 0.07958543189024085140, 0.2665933059059887866 ) ) ;
#62830 = CYLINDRICAL_SURFACE ( 'NONE', #35574, 1.181102362204724310 ) ;
#62831 = CARTESIAN_POINT ( 'NONE',  ( -0.2635424796782920853, -0.1334565945130699871, 5.584901928512098657 ) ) ;
#62832 = CARTESIAN_POINT ( 'NONE',  ( -0.1115485564304456306, 0.2952755905511810774, -0.1292274648535930714 ) ) ;
#62833 = DIRECTION ( 'NONE',  ( 0.000000000000000000, 0.000000000000000000, 1.000000000000000000 ) ) ;
#62834 = CARTESIAN_POINT ( 'NONE',  ( -1.607611548556429737, 0.2952755905511810774, -0.1292274648535930714 ) ) ;
#62835 = CARTESIAN_POINT ( 'NONE',  ( 0.3392501089628018884, -0.1958661417322834220, -2.931758530183726563 ) ) ;
#62836 = ORIENTED_EDGE ( 'NONE', *, *, #77984, .F. ) ;
#62837 = VERTEX_POINT ( 'NONE', #56031 ) ;
#62838 = CARTESIAN_POINT ( 'NONE',  ( 0.6364829396325465405, -0.3162353388693409650, -0.4822834645669289433 ) ) ;
#62839 = CARTESIAN_POINT ( 'NONE',  ( 0.02624671916010564918, 0.1283753931104748280, 0.1820866141732283561 ) ) ;
#62841 = FACE_OUTER_BOUND ( 'NONE', #33515, .T. ) ;
#62840 = DIRECTION ( 'NONE',  ( -0.000000000000000000, -1.000000000000000000, -0.000000000000000000 ) ) ;
#62842 = CARTESIAN_POINT ( 'NONE',  ( -0.1958661417322834220, -0.3392501089628018884, -1.252624671916010568 ) ) ;
#62843 = CARTESIAN_POINT ( 'NONE',  ( 0.2925321140481932369, -0.2925321140481931814, -2.852362204724409711 ) ) ;
#62844 = CARTESIAN_POINT ( 'NONE',  ( 0.2821522309711292364, -0.6692913385826771977, 0.1292274648535927661 ) ) ;
#62845 = CARTESIAN_POINT ( 'NONE',  ( -1.167979002624671470, 0.05413385826771666132, 0.4176697321401328100 ) ) ;
#62846 = CARTESIAN_POINT ( 'NONE',  ( -1.095800524934382292, -0.05778040916215522460, 0.4822834645669289988 ) ) ;
#62847 = CARTESIAN_POINT ( 'NONE',  ( 0.1640419947506569498, -0.05778040916215522460, 0.4822834645669289988 ) ) ;
#62848 = CARTESIAN_POINT ( 'NONE',  ( 1.043307086614173818, -0.5400638737290845981, -0.3530559997133363437 ) ) ;
#62849 = CARTESIAN_POINT ( 'NONE',  ( 1.469816272965879911, -0.5023911411419708095, 0.1820866141732285504 ) ) ;
#62850 = CARTESIAN_POINT ( 'NONE',  ( 1.299212598425197429, -0.5511811023622047445, 6.969142054262312111E-17 ) ) ;
#62851 = CARTESIAN_POINT ( 'NONE',  ( -1.036745406824146176, -0.4281496062992124485, 0.4176697321401328655 ) ) ;
#62852 = CARTESIAN_POINT ( 'NONE',  ( -0.3996062992125986590, 0.1070741851644051723, -0.5820209973753280863 ) ) ;
#62853 = CARTESIAN_POINT ( 'NONE',  ( 1.568241469816273659, -0.05778040916215560624, -0.4822834645669293319 ) ) ;
#62854 = CARTESIAN_POINT ( 'NONE',  ( -0.1049643490035302024, -0.3917322834645671215, -0.3792650918635169233 ) ) ;
#62855 = CARTESIAN_POINT ( 'NONE',  ( -0.1049868766404193215, -0.6046776061558807314, 0.2411417322834647770 ) ) ;
#62857 = DIRECTION ( 'NONE',  ( -1.000000000000000000, 0.000000000000000000, -0.000000000000000000 ) ) ;
#62856 = CARTESIAN_POINT ( 'NONE',  ( 1.043307086614173818, 0.1660481256975885056, 0.3530559997133364547 ) ) ;
#62858 = CARTESIAN_POINT ( 'NONE',  ( -1.384514435695537005, 0.1771653543307087630, 0.09757992244046791164 ) ) ;
#62859 = CARTESIAN_POINT ( 'NONE',  ( 0.2690288713910767848, 0.2952755905511811885, 0.1292274648535926551 ) ) ;
#62860 = CARTESIAN_POINT ( 'NONE',  ( 0.8333333333333340365, 0.1771653543307087075, -0.09757992244046823083 ) ) ;
#62861 = CARTESIAN_POINT ( 'NONE',  ( 0.5314960629920847390, 2.755905511811024056, 3.937007874015794773 ) ) ;
#62862 = CARTESIAN_POINT ( 'NONE',  ( 0.7939632545931766261, -0.3162353388693409650, -0.4822834645669289433 ) ) ;
#62863 = CARTESIAN_POINT ( 'NONE',  ( -0.4824498642376744417, -2.567464376874931580E-15, -0.4445507791589072832 ) ) ;
#62864 = CARTESIAN_POINT ( 'NONE',  ( -0.6430446194225716283, -0.3690944881889763329, 0.3153832671262228327 ) ) ;
#62865 = CARTESIAN_POINT ( 'NONE',  ( -0.4724409448818890911, -0.1870078740157479769, 0.4822834645669291653 ) ) ;
#62866 = CARTESIAN_POINT ( 'NONE',  ( 1.450131233595801428, -0.6692913385826773087, -0.1292274648535924053 ) ) ;
#62867 = EDGE_CURVE ( 'NONE', #22548, #34118, #81106, .T. ) ;
#62868 = CARTESIAN_POINT ( 'NONE',  ( -0.6955380577427815458, -0.4281496062992127816, -0.4176697321401328100 ) ) ;
#62869 = CARTESIAN_POINT ( 'NONE',  ( 1.364829396325460076, 0.2306618581243848609, 0.2411417322834645549 ) ) ;
#62870 = CARTESIAN_POINT ( 'NONE',  ( 0.1049643490035303967, 0.3917322834645670659, -0.9350586858605794971 ) ) ;
#62871 = CARTESIAN_POINT ( 'NONE',  ( -1.056430446194224881, -0.5511811023622046335, 0.09757992244046803654 ) ) ;
#62872 = CARTESIAN_POINT ( 'NONE',  ( -0.7137454485294953965, 2.244094488188976388, 0.4917280318828573527 ) ) ;
#62873 = CARTESIAN_POINT ( 'NONE',  ( 1.345144356955381593, -0.3162353388693409650, -0.4822834645669289433 ) ) ;
#62874 = CIRCLE ( 'NONE', #25242, 1.220472440944881942 ) ;
#62875 = CARTESIAN_POINT ( 'NONE',  ( -0.4724409448818898682, -8.678599364036362592E-17, -2.005905511811023612 ) ) ;
#62876 = CARTESIAN_POINT ( 'NONE',  ( -0.09115970038225217065, 2.409604939980833412E-17, -0.3464511005275205946 ) ) ;
#62877 = CARTESIAN_POINT ( 'NONE',  ( -1.469816272965878357, 0.1283753931104748280, 0.1820866141732283561 ) ) ;
#62878 = CARTESIAN_POINT ( 'NONE',  ( -0.9055118110236215490, 0.1771653543307087630, 0.000000000000000000 ) ) ;
#62879 = CARTESIAN_POINT ( 'NONE',  ( 0.7988977408164235072, -1.206088964116209378E-16, 0.3791475997938230647 ) ) ;
#62880 = CARTESIAN_POINT ( 'NONE',  ( -0.2165354330708654795, 0.1660481256975885056, 0.3530559997133364547 ) ) ;
#62881 = CARTESIAN_POINT ( 'NONE',  ( 0.01968503937007957949, -0.4536011799217368745, -0.2665933059059886201 ) ) ;
#62882 = CARTESIAN_POINT ( 'NONE',  ( -1.187664041994750175, -0.08942795157528024563, -0.3641732283464568787 ) ) ;
#62883 = CARTESIAN_POINT ( 'NONE',  ( 1.417322834645670104, -0.1870078740157479769, 0.3641732283464567677 ) ) ;
#62884 = CARTESIAN_POINT ( 'NONE',  ( 1.095800524934383846, -0.05778040916215560624, -0.4822834645669293319 ) ) ;
#62885 = CARTESIAN_POINT ( 'NONE',  ( 1.555118110236221041, -0.5400638737290844871, 0.3530559997133364547 ) ) ;
#62886 = CARTESIAN_POINT ( 'NONE',  ( 0.5446194225721792126, -0.2845877964562159024, 0.3641732283464567677 ) ) ;
#62887 = CARTESIAN_POINT ( 'NONE',  ( 0.4593175853018380828, 0.05413385826771626580, -0.4176697321401330321 ) ) ;
#62888 = CARTESIAN_POINT ( 'NONE',  ( 0.8792650918635177559, -0.3690944881889765550, -0.3153832671262227771 ) ) ;
#62889 = EDGE_LOOP ( 'NONE', ( #72008, #32686, #42113, #6614 ) ) ;
#62890 = CARTESIAN_POINT ( 'NONE',  ( -1.010498687664041384, 0.05413385826771666132, 0.4176697321401328100 ) ) ;
#62891 = EDGE_CURVE ( 'NONE', #58154, #9606, #80092, .T. ) ;
#62892 = CARTESIAN_POINT ( 'NONE',  ( -1.338582677165353729, -0.1870078740157479769, 0.4822834645669291653 ) ) ;
#62893 = CARTESIAN_POINT ( 'NONE',  ( -0.03280839895013062252, -0.6692913385826771977, 0.1292274648535927661 ) ) ;
#62894 = CARTESIAN_POINT ( 'NONE',  ( 0.3996062992125985480, 0.1070741851644054637, -0.1246719160104987068 ) ) ;
#62895 = CARTESIAN_POINT ( 'NONE',  ( -0.1070741851644056997, 0.3996062992125984925, -2.445538057742782101 ) ) ;
#62896 = CARTESIAN_POINT ( 'NONE',  ( 0.4921259842519691285, 0.1660481256975885056, 0.3530559997133364547 ) ) ;
#62897 = CARTESIAN_POINT ( 'NONE',  ( 1.555118110236221041, -0.4536011799217367080, 0.2665933059059888421 ) ) ;
#62898 = CARTESIAN_POINT ( 'NONE',  ( -0.1181102362204717315, -0.6692913385826771977, 8.415575281601705876E-17 ) ) ;
#62899 = CARTESIAN_POINT ( 'NONE',  ( 0.2887139107611556010, -0.6046776061558807314, 0.2411417322834647770 ) ) ;
#62900 = CARTESIAN_POINT ( 'NONE',  ( -0.1998031496062994683, 0.3460692066303958092, -2.217847769028871596 ) ) ;
#62901 = CARTESIAN_POINT ( 'NONE',  ( -0.1058382717557497937, -0.3949938075777411628, -1.646981627296588035 ) ) ;
#62902 = CARTESIAN_POINT ( 'NONE',  ( -0.1998031496062991907, -0.3460692066303959757, -2.900262467191600635 ) ) ;
#62903 = CARTESIAN_POINT ( 'NONE',  ( 3.937007874015748143, 1.724409448818897905, -0.4359958488159719758 ) ) ;
#62904 = CARTESIAN_POINT ( 'NONE',  ( 0.3917322834645670104, 2.398668435337828261E-17, -0.5826771653543306728 ) ) ;
#62905 = CARTESIAN_POINT ( 'NONE',  ( -0.4002624671916004129, -0.08942795157528024563, -0.3641732283464568787 ) ) ;
#62906 = CARTESIAN_POINT ( 'NONE',  ( -0.7545931758530177724, 0.2952755905511811885, 0.1292274648535926551 ) ) ;
#62907 = CARTESIAN_POINT ( 'NONE',  ( 0.2690288713910767848, -0.6692913385826773087, -0.1292274648535924053 ) ) ;
#62908 = EDGE_CURVE ( 'NONE', #48835, #59512, #19780, .T. ) ;
#62909 = CARTESIAN_POINT ( 'NONE',  ( -0.3420746716998662729, 0.1974969037888702206, -2.622703412073491336 ) ) ;
#62910 = CARTESIAN_POINT ( 'NONE',  ( 1.017060367454068803, -0.3162353388693405765, 0.4822834645669290543 ) ) ;
#62911 = B_SPLINE_CURVE_WITH_KNOTS ( 'NONE', 3,
 ( #12943, #73098, #28472, #34381, #54133, #15031, #80265, #8710, #8295, #47824, #15874, #40687, #60872, #35210, #72683, #79848 ),
 .UNSPECIFIED., .F., .F.,
 ( 4, 2, 2, 2, 2, 2, 2, 4 ),
 ( 0.000000000000000000, 0.0003923911760484576224, 0.0007847823520969152448, 0.001177173528145373030, 0.001569564704193830490, 0.001961955880242287949, 0.002354347056290746060, 0.003139129408387677025 ),
 .UNSPECIFIED. ) ;
#62912 = CARTESIAN_POINT ( 'NONE',  ( -1.509186351706035767, -0.4281496062992124485, 0.4176697321401328655 ) ) ;
#62913 = CARTESIAN_POINT ( 'NONE',  ( 0.8923884514435701520, -0.6046776061558809534, -0.2411417322834644161 ) ) ;
#62914 = CARTESIAN_POINT ( 'NONE',  ( 0.4091458600556404646, -0.2362204724409448231, -2.782152230971128848 ) ) ;
#62915 = CARTESIAN_POINT ( 'NONE',  ( -0.1070741851644051862, -0.3996062992125987146, -2.119422572178477626 ) ) ;
#62916 = CARTESIAN_POINT ( 'NONE',  ( 1.587926509186352586, -0.4281496062992127816, -0.4176697321401328100 ) ) ;
#62917 = CARTESIAN_POINT ( 'NONE',  ( 0.9120734908136489683, -0.6692913385826771977, 0.1292274648535927661 ) ) ;
#62918 = CARTESIAN_POINT ( 'NONE',  ( 0.6955380577427828781, 0.05413385826771626580, -0.4176697321401330321 ) ) ;
#62919 = CARTESIAN_POINT ( 'NONE',  ( 1.036745406824147508, -0.3690944881889765550, -0.3153832671262227771 ) ) ;
#62921 = CARTESIAN_POINT ( 'NONE',  ( -1.443569553805773564, 0.2306618581243847221, -0.2411417322834647770 ) ) ;
#62920 = CARTESIAN_POINT ( 'NONE',  ( -1.627296587926508442, 0.1283753931104748280, 0.1820866141732283561 ) ) ;
#62922 = CARTESIAN_POINT ( 'NONE',  ( -0.2867679344610365999, 0.2867679344610364889, -0.2618110236220473341 ) ) ;
#62923 = CARTESIAN_POINT ( 'NONE',  ( 0.6955380577427828781, -0.4281496062992124485, 0.4176697321401328655 ) ) ;
#62924 = CARTESIAN_POINT ( 'NONE',  ( 1.633858267716535639, -0.4536011799217367080, 0.2665933059059888421 ) ) ;
#62925 = CARTESIAN_POINT ( 'NONE',  ( -0.3083989501312330295, -0.05778040916215522460, 0.4822834645669289988 ) ) ;
#62926 = CARTESIAN_POINT ( 'NONE',  ( -1.017060367454067249, -0.3162353388693409650, -0.4822834645669289433 ) ) ;
#62927 = CARTESIAN_POINT ( 'NONE',  ( 1.017060367454068581, -0.05778040916215560624, -0.4822834645669293319 ) ) ;
#62928 = CARTESIAN_POINT ( 'NONE',  ( -0.2867679344610365999, 0.2867679344610364889, -0.5767716535433071723 ) ) ;
#62929 = CARTESIAN_POINT ( 'NONE',  ( 0.3917322834645670104, 2.398668435337828261E-17, -1.370078740157480324 ) ) ;
#62930 =( BOUNDED_CURVE ( )  B_SPLINE_CURVE ( 2, ( #17644, #3766, #43276, #68973, #11323, #82032, #75713, #18054, #43687, #80797, #23114, #32737, #20119 ),
 .UNSPECIFIED., .F., .F. ) 
 B_SPLINE_CURVE_WITH_KNOTS ( ( 3, 2, 2, 2, 2, 2, 3 ),
 ( 0.3875000000000000111, 0.3916666666666666630, 0.3958333333333333148, 0.4000000000000000222, 0.4041666666666667296, 0.4083333333333333814, 0.4125000000000000333 ),
 .UNSPECIFIED. ) 
 CURVE ( )  GEOMETRIC_REPRESENTATION_ITEM ( )  RATIONAL_B_SPLINE_CURVE ( ( 1.000000000000000000, 0.9659258262890683122, 1.000000000000000000, 0.9659258262890683122, 1.000000000000000000, 0.9659258262890683122, 1.000000000000000000, 0.9659258262890683122, 1.000000000000000000, 0.9659258262890683122, 1.000000000000000000, 0.9659258262890678681, 1.000000000000000444 ) ) 
 REPRESENTATION_ITEM ( '' )  );
#62931 = CARTESIAN_POINT ( 'NONE',  ( -0.3917322834645671215, 0.1049643490035301469, -2.702099737532808632 ) ) ;
#62932 = CARTESIAN_POINT ( 'NONE',  ( -1.476377952755905110, 0.07958543189024085140, 0.2665933059059887866 ) ) ;
#62933 = VERTEX_POINT ( 'NONE', #3468 ) ;
#62934 = CARTESIAN_POINT ( 'NONE',  ( 0.3949938075777409963, 2.418639510665530435E-17, -2.795275590551181022 ) ) ;
#62935 = ORIENTED_EDGE ( 'NONE', *, *, #8539, .F. ) ;
#62936 = DIRECTION ( 'NONE',  ( -0.000000000000000000, -1.000000000000000000, -0.000000000000000000 ) ) ;
#62937 = CARTESIAN_POINT ( 'NONE',  ( 1.338582677165355062, -0.1870078740157480601, -0.3641732283464567677 ) ) ;
#62938 = CARTESIAN_POINT ( 'NONE',  ( -0.1070741851644056997, 0.3996062992125986035, -1.266404199475065440 ) ) ;
#62939 = CARTESIAN_POINT ( 'NONE',  ( 1.371391076115485941, 0.1771653543307087630, 0.09757992244046791164 ) ) ;
#62940 = DIRECTION ( 'NONE',  ( -1.000000000000000000, -0.000000000000000000, -0.000000000000000000 ) ) ;
#62941 = DIRECTION ( 'NONE',  ( -1.000000000000000000, 0.000000000000000000, 0.000000000000000000 ) ) ;
#62942 = CARTESIAN_POINT ( 'NONE',  ( 0.000000000000000000, 0.07874015748031502893, -3.937007874015748143 ) ) ;
#62943 = CARTESIAN_POINT ( 'NONE',  ( -0.3392501089628019995, 0.1958661417322832277, -0.2683727034120735877 ) ) ;
#62944 = CARTESIAN_POINT ( 'NONE',  ( -0.8267716535433065062, 0.1771653543307087630, 0.000000000000000000 ) ) ;
#62945 = CARTESIAN_POINT ( 'NONE',  ( -1.207349081364828880, 0.1283753931104746893, -0.1820866141732285504 ) ) ;
#62946 = CARTESIAN_POINT ( 'NONE',  ( -1.410761154855641575, -0.3162353388693409650, -0.4822834645669289433 ) ) ;
#62947 = CARTESIAN_POINT ( 'NONE',  ( 0.1181102362204730916, -0.6692913385826771977, 8.415575281601705876E-17 ) ) ;
#62948 = CARTESIAN_POINT ( 'NONE',  ( -1.423884514435694859, -0.05778040916215560624, -0.4822834645669293319 ) ) ;
#62949 = ORIENTED_EDGE ( 'NONE', *, *, #25177, .F. ) ;
#62950 = CARTESIAN_POINT ( 'NONE',  ( 1.443569553805774897, 0.2306618581243848609, 0.2411417322834645549 ) ) ;
#62951 = CARTESIAN_POINT ( 'NONE',  ( 0.3503937007874015075, -0.3044824468161027586, -0.01968503937007903132 ) ) ;
#62952 = CARTESIAN_POINT ( 'NONE',  ( 3.489184436367526398, 2.418298854841256951, 4.436297187341772030 ) ) ;
#62953 = CARTESIAN_POINT ( 'NONE',  ( 0.4724409448818898682, 2.892866454678787531E-17, -2.007874015748031482 ) ) ;
#62954 = CARTESIAN_POINT ( 'NONE',  ( 2.152711368484104604, 1.622209144264168845, 0.4670403427556030218 ) ) ;
#62955 = CARTESIAN_POINT ( 'NONE',  ( -0.3740157480314953431, 0.07958543189024085140, 0.2665933059059887866 ) ) ;
#62956 = CARTESIAN_POINT ( 'NONE',  ( -1.200787401574802349, -0.5400638737290844871, 0.3530559997133364547 ) ) ;
#62957 = CARTESIAN_POINT ( 'NONE',  ( 0.8923884514435703741, 0.2306618581243848609, 0.2411417322834645549 ) ) ;
#62958 = ORIENTED_EDGE ( 'NONE', *, *, #67735, .T. ) ;
#62960 = CARTESIAN_POINT ( 'NONE',  ( -0.3503937007874015630, 0.000000000000000000, 0.000000000000000000 ) ) ;
#62959 = DIRECTION ( 'NONE',  ( 1.000000000000000000, 0.000000000000000000, 0.000000000000000000 ) ) ;
#62961 = CARTESIAN_POINT ( 'NONE',  ( -1.673228346456691717, 0.1660481256975883668, -0.3530559997133364547 ) ) ;
#62962 = CARTESIAN_POINT ( 'NONE',  ( -1.220472440944881054, 0.2952755905511811885, 0.000000000000000000 ) ) ;
#62963 = CARTESIAN_POINT ( 'NONE',  ( -0.3917322834645668994, -0.1049643490035306742, -0.4409255661079247157 ) ) ;
#62964 = CARTESIAN_POINT ( 'NONE',  ( 0.1771653543307093182, 0.07958543189024085140, 0.2665933059059887866 ) ) ;
#62965 = CARTESIAN_POINT ( 'NONE',  ( 0.1049643490035303689, 0.3917322834645670104, -0.7080052493438320216 ) ) ;
#62966 = CARTESIAN_POINT ( 'NONE',  ( -0.5708661417322825615, -0.4536011799217367080, 0.2665933059059888421 ) ) ;
#62967 = CARTESIAN_POINT ( 'NONE',  ( 0.6299212598425204535, -0.1870078740157479769, 0.3641732283464567677 ) ) ;
#62968 = CARTESIAN_POINT ( 'NONE',  ( 0.5052493438320215802, 0.2952755905511811885, 0.1292274648535926551 ) ) ;
#62969 = CARTESIAN_POINT ( 'NONE',  ( -0.5577427821522301654, -0.2845877964562159024, 0.3641732283464567677 ) ) ;
#62970 = CARTESIAN_POINT ( 'NONE',  ( 0.3392501089628018329, 0.1958661417322835607, -2.643044619422571628 ) ) ;
#62971 = CARTESIAN_POINT ( 'NONE',  ( 1.318897637795276356, 0.1660481256975883668, -0.3530559997133364547 ) ) ;
#62972 = CARTESIAN_POINT ( 'NONE',  ( -1.174540682414697335, -0.05778040916215522460, 0.4822834645669289988 ) ) ;
#62973 = CARTESIAN_POINT ( 'NONE',  ( 5.785732909357575061E-17, -0.4724409448818898682, -0.7854330708661416693 ) ) ;
#62974 = CARTESIAN_POINT ( 'NONE',  ( -0.01968503937007793844, -0.5400638737290844871, 0.3530559997133364547 ) ) ;
#62975 = CARTESIAN_POINT ( 'NONE',  ( -0.4133858267716528645, -0.5400638737290844871, 0.3530559997133364547 ) ) ;
#62976 = CARTESIAN_POINT ( 'NONE',  ( 1.233595800524935227, 0.1283753931104746893, -0.1820866141732285504 ) ) ;
#62977 = CARTESIAN_POINT ( 'NONE',  ( 0.2099737532808405305, 0.1283753931104746893, -0.1820866141732285504 ) ) ;
#62978 = CARTESIAN_POINT ( 'NONE',  ( -0.02624671916010428221, -0.6046776061558807314, 0.2411417322834647770 ) ) ;
#62979 = CARTESIAN_POINT ( 'NONE',  ( -1.154855643044618851, 0.2306618581243848609, 0.2411417322834645549 ) ) ;
#62980 = CARTESIAN_POINT ( 'NONE',  ( -0.2952755905511810774, 0.000000000000000000, 6.043307086614173151 ) ) ;
#62981 = CARTESIAN_POINT ( 'NONE',  ( 1.561679790026247350, -0.004921259842519870586, -0.3153832671262229437 ) ) ;
#62982 = CARTESIAN_POINT ( 'NONE',  ( -0.2165354330708654795, 0.1660481256975885056, 0.3530559997133364547 ) ) ;
#62983 = CARTESIAN_POINT ( 'NONE',  ( -1.246719160104986512, 0.05413385826771666132, 0.4176697321401328100 ) ) ;
#62984 = ORIENTED_EDGE ( 'NONE', *, *, #28526, .F. ) ;
#62985 = CARTESIAN_POINT ( 'NONE',  ( -0.1070741851644056997, 0.3996062992125984925, -2.130577427821522374 ) ) ;
#62986 = CARTESIAN_POINT ( 'NONE',  ( 1.082677165354331228, -0.5400638737290844871, 0.3530559997133364547 ) ) ;
#62987 = CARTESIAN_POINT ( 'NONE',  ( -0.6692913385826764205, -0.5511811023622047445, 6.969142054262312111E-17 ) ) ;
#62988 = CARTESIAN_POINT ( 'NONE',  ( -0.5708661417322828946, 0.1660481256975883668, -0.3530559997133364547 ) ) ;
#62989 = CARTESIAN_POINT ( 'NONE',  ( 1.187664041994751285, -0.05778040916215522460, 0.4822834645669289988 ) ) ;
#62990 = CARTESIAN_POINT ( 'NONE',  ( 1.102362204724410155, -0.1870078740157480879, -0.4822834645669291653 ) ) ;
#62991 = DIRECTION ( 'NONE',  ( 0.000000000000000000, -1.000000000000000000, 0.000000000000000000 ) ) ;
#62992 = CARTESIAN_POINT ( 'NONE',  ( -1.089238845144356427, -0.004921259842519576551, 0.3153832671262227771 ) ) ;
#62993 = CARTESIAN_POINT ( 'NONE',  ( 0.1998031496062994128, -0.3460692066303957537, -0.6410761154855643129 ) ) ;
#62994 = CARTESIAN_POINT ( 'NONE',  ( 4.893765752498283924E-17, -0.3996062992125986035, -0.8661417322834645827 ) ) ;
#62995 = CARTESIAN_POINT ( 'NONE',  ( -0.3420746716998659953, -0.1974969037888706647, -0.3674540682414698667 ) ) ;
#62996 = CARTESIAN_POINT ( 'NONE',  ( 0.2772244525506746826, 1.152387065982276360, -1.451133023321481419 ) ) ;
#62997 = CARTESIAN_POINT ( 'NONE',  ( 1.076115485564305141, 0.1283753931104746893, -0.1820866141732285504 ) ) ;
#62998 = CARTESIAN_POINT ( 'NONE',  ( 0.5708661417322841158, -0.4536011799217368745, -0.2665933059059886201 ) ) ;
#62999 = CARTESIAN_POINT ( 'NONE',  ( 0.4986876640419954376, 0.2306618581243848609, 0.2411417322834645549 ) ) ;
#63000 = LINE ( 'NONE', #57075, #3827 ) ;
#63001 = CARTESIAN_POINT ( 'NONE',  ( 0.3420746716998660508, -0.1974969037888704149, -1.126640419947506633 ) ) ;
#63002 = CARTESIAN_POINT ( 'NONE',  ( 0.6955380577427828781, -0.3690944881889763329, 0.3153832671262228327 ) ) ;
#63003 = CARTESIAN_POINT ( 'NONE',  ( -0.1837270341207340729, 0.2306618581243847221, -0.2411417322834647770 ) ) ;
#63004 = CARTESIAN_POINT ( 'NONE',  ( -1.049868766404198794, -0.6046776061558807314, 0.2411417322834647770 ) ) ;
#63005 = CARTESIAN_POINT ( 'NONE',  ( 1.115485564304462551, -0.4281496062992127816, -0.4176697321401328100 ) ) ;
#63006 = CARTESIAN_POINT ( 'NONE',  ( -0.4724409448818895907, -0.1265901696524993070, -1.778215223097112663 ) ) ;
#63007 = CARTESIAN_POINT ( 'NONE',  ( -0.2925321140481932369, 0.2925321140481931814, -2.696850393700787052 ) ) ;
#63008 = CARTESIAN_POINT ( 'NONE',  ( 0.1181102362204730916, -0.5511811023622047445, 6.969142054262312111E-17 ) ) ;
#63009 = EDGE_CURVE ( 'NONE', #2500, #58583, #48283, .T. ) ;
#63010 = VERTEX_POINT ( 'NONE', #16106 ) ;
#63011 = ORIENTED_EDGE ( 'NONE', *, *, #77836, .F. ) ;
#63012 = CARTESIAN_POINT ( 'NONE',  ( -0.7020997375328076329, -0.3162353388693409650, -0.4822834645669289433 ) ) ;
#63013 = CARTESIAN_POINT ( 'NONE',  ( -0.7283464566929126471, -0.5400638737290844871, 0.3530559997133364547 ) ) ;
#63014 = CARTESIAN_POINT ( 'NONE',  ( -0.1902887139107604098, 0.2952755905511810774, -0.1292274648535930714 ) ) ;
#63015 = CARTESIAN_POINT ( 'NONE',  ( 0.2624671916010504757, 0.2306618581243848609, 0.2411417322834645549 ) ) ;
#63016 = EDGE_CURVE ( 'NONE', #47922, #7036, #2447, .T. ) ;
#63017 = CARTESIAN_POINT ( 'NONE',  ( -0.5971128608923877978, -0.6692913385826773087, -0.1292274648535924053 ) ) ;
#63018 = CARTESIAN_POINT ( 'NONE',  ( -1.253280839895012377, -0.3162353388693409650, -0.4822834645669289433 ) ) ;
#63019 = CARTESIAN_POINT ( 'NONE',  ( -0.9842519685039365918, -0.6692913385826771977, 8.415575281601705876E-17 ) ) ;
#63020 = CARTESIAN_POINT ( 'NONE',  ( 0.9120734908136489683, -0.6692913385826771977, 0.1292274648535927661 ) ) ;
#63021 = CARTESIAN_POINT ( 'NONE',  ( -0.2867679344610365999, 0.2867679344610364889, -1.586614173228346747 ) ) ;
#63022 = CARTESIAN_POINT ( 'NONE',  ( -0.4461942257217840213, -0.5023911411419708095, -0.1820866141732282451 ) ) ;
#63023 = EDGE_LOOP ( 'NONE', ( #62596, #28212 ) ) ;
#63024 = CARTESIAN_POINT ( 'NONE',  ( -0.2891555358219908833, -0.2891555358219912164, -1.476377952755905332 ) ) ;
#63025 = ORIENTED_EDGE ( 'NONE', *, *, #31934, .F. ) ;
#63026 = CARTESIAN_POINT ( 'NONE',  ( -1.167979002624671470, -0.3690944881889765550, -0.3153832671262227771 ) ) ;
#63027 = CARTESIAN_POINT ( 'NONE',  ( -1.141732283464566011, 0.2952755905511811885, 0.000000000000000000 ) ) ;
#63028 = CARTESIAN_POINT ( 'NONE',  ( -0.9514435695538050464, -0.05778040916215560624, -0.4822834645669293319 ) ) ;
#63029 = CARTESIAN_POINT ( 'NONE',  ( 0.2925321140481932369, 0.2925321140481932369, 0.01968503937007873641 ) ) ;
#63030 = CARTESIAN_POINT ( 'NONE',  ( -0.8267716535433065062, -0.6692913385826771977, 8.415575281601705876E-17 ) ) ;
#63031 = CARTESIAN_POINT ( 'NONE',  ( -0.7939632545931754048, -0.3162353388693405765, 0.4822834645669290543 ) ) ;
#63032 = CARTESIAN_POINT ( 'NONE',  ( -1.594488188976377119, 0.1660481256975883668, -0.3530559997133364547 ) ) ;
#63033 = CARTESIAN_POINT ( 'NONE',  ( 0.000000000000000000, 0.000000000000000000, 0.000000000000000000 ) ) ;
#63034 = CARTESIAN_POINT ( 'NONE',  ( 0.5446194225721792126, -0.2845877964562159024, 0.3641732283464567677 ) ) ;
#63035 = DIRECTION ( 'NONE',  ( -0.000000000000000000, -1.000000000000000000, -0.000000000000000000 ) ) ;
#63036 = CARTESIAN_POINT ( 'NONE',  ( 0.3917322834645670104, 2.398668435337828261E-17, -0.04527559055118119541 ) ) ;
#63037 = CARTESIAN_POINT ( 'NONE',  ( 0.06561679790026316017, -0.004921259842519870586, -0.3153832671262229437 ) ) ;
#63038 = CARTESIAN_POINT ( 'NONE',  ( -0.4133858267716528645, -0.5400638737290844871, 0.3530559997133364547 ) ) ;
#63039 = CARTESIAN_POINT ( 'NONE',  ( 1.476377952755906220, 0.1660481256975883668, -0.3530559997133364547 ) ) ;
#63040 = CARTESIAN_POINT ( 'NONE',  ( -0.09186351706036663400, -0.4281496062992124485, 0.4176697321401328655 ) ) ;
#63041 = EDGE_LOOP ( 'NONE', ( #11597, #77215, #30482, #19544, #83191 ) ) ;
#63042 = CARTESIAN_POINT ( 'NONE',  ( 4.893765752498283924E-17, -0.3996062992125986035, -1.968503937007873850 ) ) ;
#63043 = ORIENTED_EDGE ( 'NONE', *, *, #44641, .T. ) ;
#63044 = CARTESIAN_POINT ( 'NONE',  ( -0.1070741851644051862, -0.3996062992125986590, -1.566272965879265344 ) ) ;
#63045 = CARTESIAN_POINT ( 'NONE',  ( 0.000000000000000000, 2.145669291338582418, 0.000000000000000000 ) ) ;
#63046 = CARTESIAN_POINT ( 'NONE',  ( -1.312335958005248715, -0.5023911411419708095, -0.1820866141732282451 ) ) ;
#63047 = CARTESIAN_POINT ( 'NONE',  ( -1.581364829396324945, -0.3162353388693405765, 0.4822834645669290543 ) ) ;
#63048 = CARTESIAN_POINT ( 'NONE',  ( 0.2362204724409451007, -0.4091458600556402980, -0.5643044619422572516 ) ) ;
#63049 = ADVANCED_FACE ( 'NONE', ( #48478 ), #41751, .T. ) ;
#63050 = CARTESIAN_POINT ( 'NONE',  ( 0.2017716535433070613, -0.2017716535433070890, -0.3937007874015748254 ) ) ;
#63051 = CARTESIAN_POINT ( 'NONE',  ( -0.3392501089628019995, 0.1958661417322832277, -2.788057742782152459 ) ) ;
#63052 = CARTESIAN_POINT ( 'NONE',  ( 1.233595800524935227, 0.2306618581243847221, -0.2411417322834647770 ) ) ;
#63053 = CARTESIAN_POINT ( 'NONE',  ( 0.6167979002624678353, -0.4281496062992124485, 0.4176697321401328655 ) ) ;
#63054 = CARTESIAN_POINT ( 'NONE',  ( 0.2887139107611556010, 0.2306618581243847221, -0.2411417322834647770 ) ) ;
#63055 = CARTESIAN_POINT ( 'NONE',  ( -1.240157480314959759, -0.4536011799217368745, -0.2665933059059886201 ) ) ;
#63056 = CARTESIAN_POINT ( 'NONE',  ( -0.4265091863517051496, 0.2952755905511810774, -0.1292274648535930714 ) ) ;
#63057 = CARTESIAN_POINT ( 'NONE',  ( 0.3458507752293908943, 0.3458507752293908943, -2.576771653543307394 ) ) ;
#63058 = CARTESIAN_POINT ( 'NONE',  ( -1.036745406824146176, 0.05413385826771626580, -0.4176697321401330321 ) ) ;
#63059 = EDGE_CURVE ( 'NONE', #44871, #33221, #35451, .T. ) ;
#63060 = CARTESIAN_POINT ( 'NONE',  ( 0.3949938075777409963, 2.418639510665530743E-17, -2.399606299212599048 ) ) ;
#63061 = CARTESIAN_POINT ( 'NONE',  ( 1.286089238845145033, 0.1283753931104748280, 0.1820866141732283561 ) ) ;
#63062 = CARTESIAN_POINT ( 'NONE',  ( -0.2690288713910754526, 0.1771653543307087075, -0.09757992244046823083 ) ) ;
#63063 = CARTESIAN_POINT ( 'NONE',  ( 1.089238845144357759, -0.004921259842519870586, -0.3153832671262229437 ) ) ;
#63064 = CARTESIAN_POINT ( 'NONE',  ( -1.397637795275589623, 0.1660481256975885056, 0.3530559997133364547 ) ) ;
#63065 = CARTESIAN_POINT ( 'NONE',  ( -1.233595800524933894, -0.5023911411419708095, -0.1820866141732282451 ) ) ;
#63066 = LINE ( 'NONE', #55492, #45303 ) ;
#63067 = CARTESIAN_POINT ( 'NONE',  ( 0.7217847769028878924, -0.004921259842519576551, 0.3153832671262227771 ) ) ;
#63068 = CARTESIAN_POINT ( 'NONE',  ( -1.036745406824146176, -0.4281496062992124485, 0.4176697321401328655 ) ) ;
#63069 = EDGE_CURVE ( 'NONE', #52953, #31040, #54801, .T. ) ;
#63070 = DIRECTION ( 'NONE',  ( 0.000000000000000000, 0.000000000000000000, 1.000000000000000000 ) ) ;
#63071 = CARTESIAN_POINT ( 'NONE',  ( -0.09186351706036663400, -0.3690944881889763329, 0.3153832671262228327 ) ) ;
#63072 = CARTESIAN_POINT ( 'NONE',  ( -1.548556430446193399, 0.1283753931104748280, 0.1820866141732283561 ) ) ;
#63073 = CARTESIAN_POINT ( 'NONE',  ( 0.7152230971128616943, -0.05778040916215522460, 0.4822834645669289988 ) ) ;
#63074 = CARTESIAN_POINT ( 'NONE',  ( 0.6970755509724333443, 0.02791078216816508459, -0.4328096321851889194 ) ) ;
#63075 = CARTESIAN_POINT ( 'NONE',  ( 1.194225721784777594, -0.3690944881889765550, -0.3153832671262227771 ) ) ;
#63076 = CARTESIAN_POINT ( 'NONE',  ( -0.9776902887139098386, -0.6692913385826771977, 0.1292274648535927661 ) ) ;
#63077 = CARTESIAN_POINT ( 'NONE',  ( -0.09842519685039295696, -0.4536011799217367080, 0.2665933059059888421 ) ) ;
#63078 = DIRECTION ( 'NONE',  ( 1.000000000000000000, -0.000000000000000000, -0.000000000000000000 ) ) ;
#63079 = CARTESIAN_POINT ( 'NONE',  ( 0.1246719160104994284, -0.5511811023622046335, 0.09757992244046803654 ) ) ;
#63080 = CARTESIAN_POINT ( 'NONE',  ( -0.9908136482939626788, -0.6692913385826773087, -0.1292274648535924053 ) ) ;
#63081 = CARTESIAN_POINT ( 'NONE',  ( -0.6102362204724400829, -0.5400638737290845981, -0.3530559997133363437 ) ) ;
#63082 = CARTESIAN_POINT ( 'NONE',  ( 0.1998031496062994128, -0.3460692066303957537, -0.7985564304461942875 ) ) ;
#63083 = CARTESIAN_POINT ( 'NONE',  ( 0.1049643490035304938, -0.3917322834645669549, -2.059711286089238591 ) ) ;
#63084 = CARTESIAN_POINT ( 'NONE',  ( 0.4790026246719167324, -0.08942795157527998196, 0.3641732283464567121 ) ) ;
#63085 = CARTESIAN_POINT ( 'NONE',  ( -0.2362204724409440182, -0.1870078740157479769, 0.4822834645669291653 ) ) ;
#63086 = CARTESIAN_POINT ( 'NONE',  ( -0.8005249343832011588, 0.05413385826771626580, -0.4176697321401330321 ) ) ;
#63087 = CARTESIAN_POINT ( 'NONE',  ( -0.7349081364829387342, -0.5023911411419708095, 0.1820866141732285504 ) ) ;
#63088 = CARTESIAN_POINT ( 'NONE',  ( -3.910221821200592363, 1.414556597369199586, 0.4584944303835873369 ) ) ;
#63089 = CARTESIAN_POINT ( 'NONE',  ( -0.2099737532808391705, 0.2306618581243848609, 0.2411417322834645549 ) ) ;
#63090 = AXIS2_PLACEMENT_3D ( 'NONE', #26605, #45525, #7673 ) ;
#63091 = CARTESIAN_POINT ( 'NONE',  ( -1.620734908136482577, -0.5511811023622048555, -0.09757992244046775898 ) ) ;
#63092 = CARTESIAN_POINT ( 'NONE',  ( 1.614173228346457378, 0.2952755905511811885, 0.000000000000000000 ) ) ;
#63093 = CYLINDRICAL_SURFACE ( 'NONE', #52854, 0.5118110236220471121 ) ;
#63094 = EDGE_LOOP ( 'NONE', ( #12317, #6164 ) ) ;
#63095 = FACE_OUTER_BOUND ( 'NONE', #14706, .T. ) ;
#63096 = CARTESIAN_POINT ( 'NONE',  ( -1.450131233595799651, -0.6692913385826771977, 0.1292274648535927661 ) ) ;
#63097 = CARTESIAN_POINT ( 'NONE',  ( -1.049868766404198794, 0.2306618581243847221, -0.2411417322834647770 ) ) ;
#63098 = CARTESIAN_POINT ( 'NONE',  ( 1.509186351706037543, -0.4281496062992127816, -0.4176697321401328100 ) ) ;
#63099 = CARTESIAN_POINT ( 'NONE',  ( 0.2867679344610365999, 0.2867679344610365999, -1.797244094488188892 ) ) ;
#63100 = CARTESIAN_POINT ( 'NONE',  ( 0.1450607720586929161, 2.784432375088962958E-17, -0.3464511005275205946 ) ) ;
#63101 = CARTESIAN_POINT ( 'NONE',  ( 0.8070866141732289112, -0.5400638737290845981, -0.3530559997133363437 ) ) ;
#63102 = CARTESIAN_POINT ( 'NONE',  ( 0.4068241469816281097, 0.05413385826771666132, 0.4176697321401328100 ) ) ;
#63103 = CARTESIAN_POINT ( 'NONE',  ( 0.000000000000000000, 2.755905511811024056, 0.000000000000000000 ) ) ;
#63104 = CARTESIAN_POINT ( 'NONE',  ( 0.3996062992125985480, 2.446882876249141654E-17, -2.714566929133858331 ) ) ;
#63105 = CARTESIAN_POINT ( 'NONE',  ( 1.082677165354331228, -0.4536011799217367080, 0.2665933059059888421 ) ) ;
#63106 = EDGE_CURVE ( 'NONE', #6972, #71206, #51835, .T. ) ;
#63107 = CARTESIAN_POINT ( 'NONE',  ( 4.893765752498283924E-17, -0.3996062992125986035, -0.8661417322834645827 ) ) ;
#63108 = ORIENTED_EDGE ( 'NONE', *, *, #58635, .T. ) ;
#63109 = CARTESIAN_POINT ( 'NONE',  ( 0.3392501089628018329, 0.1958661417322835607, -2.643044619422571628 ) ) ;
#63110 = ORIENTED_EDGE ( 'NONE', *, *, #34659, .T. ) ;
#63111 = CARTESIAN_POINT ( 'NONE',  ( 0.5839895013123367340, -0.6692913385826773087, -0.1292274648535924053 ) ) ;
#63112 = CARTESIAN_POINT ( 'NONE',  ( -0.8267716535433065062, -0.6692913385826771977, 8.415575281601705876E-17 ) ) ;
#63113 = CARTESIAN_POINT ( 'NONE',  ( 1.541994750656168645, -0.6692913385826771977, 0.1292274648535927661 ) ) ;
#63114 = CARTESIAN_POINT ( 'NONE',  ( 1.187664041994751285, -0.05778040916215522460, 0.4822834645669289988 ) ) ;
#63115 = CARTESIAN_POINT ( 'NONE',  ( 1.535433070866142558, 0.2952755905511811885, 0.000000000000000000 ) ) ;
#63116 = LINE ( 'NONE', #48410, #7735 ) ;
#63117 = CARTESIAN_POINT ( 'NONE',  ( -0.2427821522309703550, -0.3162353388693405765, 0.4822834645669290543 ) ) ;
#63118 = CARTESIAN_POINT ( 'NONE',  ( -1.292650918635170010, 0.2952755905511810774, -0.1292274648535930714 ) ) ;
#63119 = CARTESIAN_POINT ( 'NONE',  ( -1.601049868766403650, 0.2306618581243847221, -0.2411417322834647770 ) ) ;
#63120 = CARTESIAN_POINT ( 'NONE',  ( 0.3635064842674253227, 1.231191414405742535, -2.723505603036860734 ) ) ;
#63121 = CARTESIAN_POINT ( 'NONE',  ( -0.3917322834645669549, -0.1049643490035306603, -2.650262467191601079 ) ) ;
#63122 = CARTESIAN_POINT ( 'NONE',  ( 0.8595800524934390507, -0.2845877964562159024, 0.3641732283464567677 ) ) ;
#63123 = EDGE_LOOP ( 'NONE', ( #51936, #59109, #1509, #50397, #35309 ) ) ;
#63124 = CARTESIAN_POINT ( 'NONE',  ( -0.1974969037888703871, -0.3420746716998661063, -0.3805774278215224293 ) ) ;
#63125 = ORIENTED_EDGE ( 'NONE', *, *, #22, .F. ) ;
#63126 = CARTESIAN_POINT ( 'NONE',  ( -0.1377952755905504645, 0.07958543189024085140, 0.2665933059059887866 ) ) ;
#63127 = CARTESIAN_POINT ( 'NONE',  ( 2.829146054566470614, 1.111778211650228609, -0.2101609992702737073 ) ) ;
#63128 = CARTESIAN_POINT ( 'NONE',  ( 0.7086614173228352742, -0.1870078740157480879, -0.4822834645669291653 ) ) ;
#63129 = CARTESIAN_POINT ( 'NONE',  ( 0.2690288713910767848, -0.6692913385826773087, -0.1292274648535924053 ) ) ;
#63130 = CARTESIAN_POINT ( 'NONE',  ( -0.4133858267716528645, 0.1660481256975883668, -0.3530559997133364547 ) ) ;
#63131 = CARTESIAN_POINT ( 'NONE',  ( 0.1958661417322834775, 0.3392501089628018884, -1.715898580873702617 ) ) ;
#63132 = CARTESIAN_POINT ( 'NONE',  ( -1.213910761154854745, -0.6692913385826771977, 0.1292274648535927661 ) ) ;
#63133 = CARTESIAN_POINT ( 'NONE',  ( -0.3392501089628017219, -0.1958661417322836718, -2.814304461942257252 ) ) ;
#63134 = CARTESIAN_POINT ( 'NONE',  ( 1.200787401574803681, -0.4536011799217368745, -0.2665933059059886201 ) ) ;
#63135 = CARTESIAN_POINT ( 'NONE',  ( -1.561679790026246017, -0.4281496062992127816, -0.4176697321401328100 ) ) ;
#63136 = CARTESIAN_POINT ( 'NONE',  ( 1.003937007874016407, -0.5400638737290844871, 0.3530559997133364547 ) ) ;
#63137 = CARTESIAN_POINT ( 'NONE',  ( 0.9776902887139113929, -0.6692913385826773087, -0.1292274648535924053 ) ) ;
#63138 = CARTESIAN_POINT ( 'NONE',  ( 0.2925321140481932369, -0.2925321140481932369, -1.043307086614173151 ) ) ;
#63139 = CARTESIAN_POINT ( 'NONE',  ( -1.377952755905511140, 0.2952755905511811885, 0.000000000000000000 ) ) ;
#63140 = CARTESIAN_POINT ( 'NONE',  ( -0.1070741851644051862, -0.3996062992125986590, -0.3064304461942257141 ) ) ;
#63141 = CARTESIAN_POINT ( 'NONE',  ( -0.1574803149606292529, -0.1870078740157479769, 0.4822834645669291653 ) ) ;
#63142 = CARTESIAN_POINT ( 'NONE',  ( 0.3996062992125986590, -0.1070741851644053111, -2.316272965879265122 ) ) ;
#63143 = CARTESIAN_POINT ( 'NONE',  ( 0.2867679344610365999, 0.2867679344610365999, -1.639763779527558807 ) ) ;
#63144 = CARTESIAN_POINT ( 'NONE',  ( 1.351706036745407680, 0.05413385826771666132, 0.4176697321401328100 ) ) ;
#63145 = CARTESIAN_POINT ( 'NONE',  ( 0.09186351706036827158, -0.004921259842519576551, 0.3153832671262227771 ) ) ;
#63146 = CARTESIAN_POINT ( 'NONE',  ( 0.7611548556430451917, -0.6046776061558807314, 0.2411417322834647770 ) ) ;
#63147 = CARTESIAN_POINT ( 'NONE',  ( 0.1265901696524989462, 0.4724409448818897572, -1.015091863517060267 ) ) ;
#63148 = CARTESIAN_POINT ( 'NONE',  ( 0.7283464566929143125, 0.07958543189024085140, 0.2665933059059887866 ) ) ;
#63149 = CARTESIAN_POINT ( 'NONE',  ( 0.3215223097112867578, -0.05778040916215522460, 0.4822834645669289988 ) ) ;
#63150 = CARTESIAN_POINT ( 'NONE',  ( 0.1058382717557499880, 0.3949938075777409408, -1.172572178477690574 ) ) ;
#63151 = CARTESIAN_POINT ( 'NONE',  ( -0.7939632545931754048, -0.3162353388693405765, 0.4822834645669290543 ) ) ;
#63152 = CARTESIAN_POINT ( 'NONE',  ( -0.4724409448818898682, -8.678599364036362592E-17, -1.061023622047243986 ) ) ;
#63153 = DIMENSIONAL_EXPONENTS ( 1.000000000000000000, 0.000000000000000000, 0.000000000000000000, 0.000000000000000000, 0.000000000000000000, 0.000000000000000000, 0.000000000000000000 ) ;
#63154 = CARTESIAN_POINT ( 'NONE',  ( 1.141732283464567566, 0.1771653543307087630, 0.000000000000000000 ) ) ;
#63155 = CARTESIAN_POINT ( 'NONE',  ( -0.5314960629921396951, 2.559055118110236560, 3.900966923095587457 ) ) ;
#63156 = CARTESIAN_POINT ( 'NONE',  ( -0.4330708661417315697, 0.2952755905511811885, 0.000000000000000000 ) ) ;
#63157 = B_SPLINE_CURVE_WITH_KNOTS ( 'NONE', 3,
 ( #52914, #72714, #39895, #29638, #7916, #4380, #33577, #59240 ),
 .UNSPECIFIED., .F., .F.,
 ( 4, 2, 2, 4 ),
 ( 0.03812540793793221111, 0.03934516121038392211, 0.04056491448283564005, 0.04300442102773906206 ),
 .UNSPECIFIED. ) ;
#63158 = CARTESIAN_POINT ( 'NONE',  ( -0.08530183727034056085, -0.2845877964562159024, 0.3641732283464567677 ) ) ;
#63159 = CARTESIAN_POINT ( 'NONE',  ( -2.565164815102350282, 1.469861850861822195, -0.4698711669589719642 ) ) ;
#63160 = CARTESIAN_POINT ( 'NONE',  ( -0.5183727034120726440, -0.6692913385826773087, -0.1292274648535924053 ) ) ;
#63161 = CARTESIAN_POINT ( 'NONE',  ( 0.6824146981627303710, 0.1283753931104746893, -0.1820866141732285504 ) ) ;
#63162 = B_SPLINE_CURVE_WITH_KNOTS ( 'NONE', 3,
 ( #18470, #37406, #75306, #36989 ),
 .UNSPECIFIED., .F., .F.,
 ( 4, 4 ),
 ( 1.999999999897049408E-07, 0.006970199999999935128 ),
 .UNSPECIFIED. ) ;
#63163 = CARTESIAN_POINT ( 'NONE',  ( -0.2925321140481930149, -0.2925321140481933480, -1.868110236220472675 ) ) ;
#63164 = CARTESIAN_POINT ( 'NONE',  ( 0.3477690288713918276, -0.6692913385826773087, -0.1292274648535924053 ) ) ;
#63165 = CARTESIAN_POINT ( 'NONE',  ( 1.253280839895013710, -0.08942795157528024563, -0.3641732283464568787 ) ) ;
#63166 = FACE_OUTER_BOUND ( 'NONE', #12505, .T. ) ;
#63167 = CARTESIAN_POINT ( 'NONE',  ( -0.2624671916010490880, 0.1283753931104746893, -0.1820866141732285504 ) ) ;
#63168 = CARTESIAN_POINT ( 'NONE',  ( -0.5577427821522301654, -0.08942795157528024563, -0.3641732283464568787 ) ) ;
#63169 = CARTESIAN_POINT ( 'NONE',  ( -0.3018372703412066094, -0.4281496062992127816, -0.4176697321401328100 ) ) ;
#63170 = CARTESIAN_POINT ( 'NONE',  ( 0.1312335958005255154, -0.6046776061558807314, 0.2411417322834647770 ) ) ;
#63171 = CARTESIAN_POINT ( 'NONE',  ( 0.8530183727034128527, -0.3690944881889763329, 0.3153832671262228327 ) ) ;
#63172 = CARTESIAN_POINT ( 'NONE',  ( 0.3132322334736995506, 1.180770478131392354, -1.077509718351006063 ) ) ;
#63173 = CARTESIAN_POINT ( 'NONE',  ( 1.443569553805774897, 0.1283753931104748280, 0.1820866141732283561 ) ) ;
#63174 = CARTESIAN_POINT ( 'NONE',  ( 0.9448818897637802916, -0.1870078740157480879, -0.4822834645669291653 ) ) ;
#63175 = DIRECTION ( 'NONE',  ( -1.000000000000000000, -3.469446951953613696E-16, 0.000000000000000000 ) ) ;
#63176 = CARTESIAN_POINT ( 'NONE',  ( -0.4265091863517051496, 0.2952755905511810774, -0.1292274648535930714 ) ) ;
#63177 = CARTESIAN_POINT ( 'NONE',  ( 0.3917322834645670104, -0.1049643490035303411, -0.8261154855643043637 ) ) ;
#63178 = CARTESIAN_POINT ( 'NONE',  ( 0.8202099737532814183, -0.6692913385826773087, -0.1292274648535924053 ) ) ;
#63179 = CARTESIAN_POINT ( 'NONE',  ( 0.7020997375328090762, -0.3162353388693405765, 0.4822834645669290543 ) ) ;
#63180 = CARTESIAN_POINT ( 'NONE',  ( -0.06215494498385511213, 1.066821167736317966, -3.936548014160229148 ) ) ;
#63181 = CARTESIAN_POINT ( 'NONE',  ( 0.3477690288713918276, -0.5511811023622048555, -0.09757992244046775898 ) ) ;
#63182 = CARTESIAN_POINT ( 'NONE',  ( 1.286089238845145033, -0.6046776061558809534, -0.2411417322834644161 ) ) ;
#63183 = CARTESIAN_POINT ( 'NONE',  ( -0.02624671916010428221, -0.5023911411419708095, 0.1820866141732285504 ) ) ;
#63184 = CARTESIAN_POINT ( 'NONE',  ( -0.4921259842519677963, 0.1660481256975883668, -0.3530559997133364547 ) ) ;
#63185 = FACE_OUTER_BOUND ( 'NONE', #5041, .T. ) ;
#63186 = CARTESIAN_POINT ( 'NONE',  ( 0.3674540682414705883, 0.2306618581243847221, -0.2411417322834647770 ) ) ;
#63187 = CARTESIAN_POINT ( 'NONE',  ( -0.6167979002624665030, -0.4281496062992127816, -0.4176697321401328100 ) ) ;
#63188 = CARTESIAN_POINT ( 'NONE',  ( -0.2755905511811018171, 0.1771653543307087630, 0.000000000000000000 ) ) ;
#63189 = CARTESIAN_POINT ( 'NONE',  ( 0.3871391076115492380, -0.05778040916215560624, -0.4822834645669293319 ) ) ;
#63190 = CARTESIAN_POINT ( 'NONE',  ( 0.7874015748031503170, -0.1870078740157480601, -0.3641732283464567677 ) ) ;
#63191 = CARTESIAN_POINT ( 'NONE',  ( -0.4527559055118102749, -0.5400638737290845981, -0.3530559997133363437 ) ) ;
#63192 = CARTESIAN_POINT ( 'NONE',  ( 1.114781747626347963, 3.405574981839577511E-16, 0.3464511005275203726 ) ) ;
#63194 = CARTESIAN_POINT ( 'NONE',  ( 1.397637795275591177, -0.5400638737290844871, 0.3530559997133364547 ) ) ;
#63193 = CARTESIAN_POINT ( 'NONE',  ( -0.9324623468618411515, 0.000000000000000000, 0.3464511005275205946 ) ) ;
#63195 = FACE_OUTER_BOUND ( 'NONE', #44142, .T. ) ;
#63196 = CARTESIAN_POINT ( 'NONE',  ( -1.653543307086613234, -0.1870078740157479769, 0.4822834645669291653 ) ) ;
#63197 = CARTESIAN_POINT ( 'NONE',  ( -0.9842519685039365918, -0.6692913385826771977, 8.415575281601705876E-17 ) ) ;
#63198 = CARTESIAN_POINT ( 'NONE',  ( 0.4091458600556404646, -0.2362204724409448231, -0.2624671916010498651 ) ) ;
#63199 = EDGE_CURVE ( 'NONE', #4444, #8202, #46930, .T. ) ;
#63200 = CARTESIAN_POINT ( 'NONE',  ( -0.1974969037888703871, -0.3420746716998661063, -2.900262467191600635 ) ) ;
#63201 = VERTEX_POINT ( 'NONE', #42170 ) ;
#63202 = CARTESIAN_POINT ( 'NONE',  ( 0.2887139107611556010, 0.1283753931104746893, -0.1820866141732285504 ) ) ;
#63203 = CARTESIAN_POINT ( 'NONE',  ( -0.1049643490035302024, -0.3917322834645671215, -1.324146981627296826 ) ) ;
#63204 = VECTOR ( 'NONE', #59014, 39.37007874015748143 ) ;
#63205 = CARTESIAN_POINT ( 'NONE',  ( 0.6561679790026253567, 0.2306618581243848609, 0.2411417322834645549 ) ) ;
#63206 = CARTESIAN_POINT ( 'NONE',  ( -0.1265901696524993347, 0.4724409448818895907, -2.683727034120735322 ) ) ;
#63207 = CARTESIAN_POINT ( 'NONE',  ( -0.5622787594981818460, -5.582469467804009507E-15, -0.3954985857520081360 ) ) ;
#63208 = CARTESIAN_POINT ( 'NONE',  ( -0.4724409448818890911, -0.1870078740157480601, -0.3641732283464567677 ) ) ;
#63209 = DIRECTION ( 'NONE',  ( -0.000000000000000000, 1.000000000000000000, -0.000000000000000000 ) ) ;
#63210 = CARTESIAN_POINT ( 'NONE',  ( 1.299212598425197429, -0.6692913385826771977, 8.415575281601705876E-17 ) ) ;
#63211 = CARTESIAN_POINT ( 'NONE',  ( 0.9973753280839902091, 0.1283753931104746893, -0.1820866141732285504 ) ) ;
#63212 = CARTESIAN_POINT ( 'NONE',  ( -0.1706036745406816491, 0.05413385826771626580, -0.4176697321401330321 ) ) ;
#63213 = CARTESIAN_POINT ( 'NONE',  ( -0.3917322834645669549, -7.196005306013483243E-17, -0.7493245162391581893 ) ) ;
#63214 = CARTESIAN_POINT ( 'NONE',  ( -0.5971128608923877978, -0.6692913385826773087, -0.1292274648535924053 ) ) ;
#63215 = CARTESIAN_POINT ( 'NONE',  ( -1.345144356955379816, -0.08942795157528024563, -0.3641732283464568787 ) ) ;
#63216 = CARTESIAN_POINT ( 'NONE',  ( -0.3871391076115479057, -0.3162353388693409650, -0.4822834645669289433 ) ) ;
#63217 = CARTESIAN_POINT ( 'NONE',  ( -1.614173228346457378, 1.055049524192299693, 0.1372047244094476981 ) ) ;
#63218 = DIRECTION ( 'NONE',  ( -1.196716813021146393E-16, 0.7071067811865616726, -0.7071067811865334729 ) ) ;
#63219 = ORIENTED_EDGE ( 'NONE', *, *, #33733, .T. ) ;
#63220 = CARTESIAN_POINT ( 'NONE',  ( 0.2867679344610366554, 0.2867679344610366554, -1.866817216044307060 ) ) ;
#63221 = CARTESIAN_POINT ( 'NONE',  ( 0.6167979002624679463, 0.05413385826771626580, -0.4176697321401330321 ) ) ;
#63222 = ORIENTED_EDGE ( 'NONE', *, *, #70277, .T. ) ;
#63223 = CARTESIAN_POINT ( 'NONE',  ( -0.2624671916010490880, 0.2306618581243847221, -0.2411417322834647770 ) ) ;
#63224 = CARTESIAN_POINT ( 'NONE',  ( -1.404199475065615932, -0.4281496062992127816, -0.4176697321401328100 ) ) ;
#63225 = CARTESIAN_POINT ( 'NONE',  ( 0.5511811023622054106, -0.1870078740157480879, -0.4822834645669291653 ) ) ;
#63226 = CARTESIAN_POINT ( 'NONE',  ( -0.05905511811023545637, 0.1660481256975885056, 0.3530559997133364547 ) ) ;
#63227 = CARTESIAN_POINT ( 'NONE',  ( 0.2867679344610365999, 0.2867679344610365999, -1.482283464566929387 ) ) ;
#63228 = CARTESIAN_POINT ( 'NONE',  ( -0.9776902887139098386, -0.6692913385826771977, 0.1292274648535927661 ) ) ;
#63229 = CARTESIAN_POINT ( 'NONE',  ( 0.2493438320209980519, 0.05413385826771666132, 0.4176697321401328100 ) ) ;
#63230 = CARTESIAN_POINT ( 'NONE',  ( -0.2952755905511803003, -0.5400638737290845981, -0.3530559997133363437 ) ) ;
#63231 = CARTESIAN_POINT ( 'NONE',  ( 0.2952755905511819101, 0.07958543189024071263, -0.2665933059059888421 ) ) ;
#63232 = DIRECTION ( 'NONE',  ( -1.000000000000000000, -0.000000000000000000, -0.000000000000000000 ) ) ;
#63233 = CARTESIAN_POINT ( 'NONE',  ( -0.02624671916010428221, -0.6046776061558807314, 0.2411417322834647770 ) ) ;
#63234 = CARTESIAN_POINT ( 'NONE',  ( -2.787279214012418738, 0.000000000000000000, 0.000000000000000000 ) ) ;
#63235 = CARTESIAN_POINT ( 'NONE',  ( 1.581364829396326277, -0.05778040916215522460, 0.4822834645669289988 ) ) ;
#63236 = CARTESIAN_POINT ( 'NONE',  ( -0.2867679344610364334, -0.2867679344610367109, -2.570866141732283339 ) ) ;
#63237 = ORIENTED_EDGE ( 'NONE', *, *, #31645, .F. ) ;
#63238 = ORIENTED_EDGE ( 'NONE', *, *, #22805, .T. ) ;
#63239 = CARTESIAN_POINT ( 'NONE',  ( 0.4724409448818904789, -0.1870078740157480879, -0.4822834645669291653 ) ) ;
#63240 = CARTESIAN_POINT ( 'NONE',  ( 0.07217847769028949700, -0.08942795157528024563, -0.3641732283464568787 ) ) ;
#63242 = CARTESIAN_POINT ( 'NONE',  ( 0.5314960629921325896, 2.742776584231126247, -1.881758995267129642 ) ) ;
#63241 = CARTESIAN_POINT ( 'NONE',  ( 1.266404199475066328, -0.2845877964562161244, -0.3641732283464567121 ) ) ;
#63243 = CARTESIAN_POINT ( 'NONE',  ( -0.1049643490035307020, 0.3917322834645669549, -1.036089238845144589 ) ) ;
#63244 = CARTESIAN_POINT ( 'NONE',  ( -0.4091458600556405756, 0.2362204724409446288, 0.05446194225721784354 ) ) ;
#63245 =( NAMED_UNIT ( * ) SI_UNIT ( $, .STERADIAN. ) SOLID_ANGLE_UNIT ( ) );
#63246 = CARTESIAN_POINT ( 'NONE',  ( -0.1058382717557503072, 0.3949938075777408852, 0.07414698162729657649 ) ) ;
#63247 = CARTESIAN_POINT ( 'NONE',  ( 0.2690288713910767848, -0.6692913385826773087, -0.1292274648535924053 ) ) ;
#63248 = CARTESIAN_POINT ( 'NONE',  ( -1.161417322834644716, 0.1660481256975885056, 0.3530559997133364547 ) ) ;
#63249 = CARTESIAN_POINT ( 'NONE',  ( -1.345144356955379816, -0.05778040916215560624, -0.4822834645669293319 ) ) ;
#63250 = CARTESIAN_POINT ( 'NONE',  ( 0.1443569553805781891, -0.4281496062992124485, 0.4176697321401328655 ) ) ;
#63251 = CARTESIAN_POINT ( 'NONE',  ( 0.8989501312335963501, -0.6692913385826773087, -0.1292274648535924053 ) ) ;
#63252 = CARTESIAN_POINT ( 'NONE',  ( 1.476377952755906442, -0.4536011799217367080, 0.2665933059059888421 ) ) ;
#63253 = CARTESIAN_POINT ( 'NONE',  ( 0.7349081364829403995, 0.1283753931104748280, 0.1820866141732283561 ) ) ;
#63254 = CARTESIAN_POINT ( 'NONE',  ( -1.043307086614172041, -0.5400638737290844871, 0.3530559997133364547 ) ) ;
#63255 = CARTESIAN_POINT ( 'NONE',  ( -0.2925321140481930149, -0.2925321140481933480, -0.4507874015748031815 ) ) ;
#63256 = CARTESIAN_POINT ( 'NONE',  ( -1.568241469816272105, -0.2845877964562161244, -0.3641732283464567121 ) ) ;
#63257 = CARTESIAN_POINT ( 'NONE',  ( -0.3392501089628017219, -0.1958661417322836718, -0.2020997375328083545 ) ) ;
#63259 = CARTESIAN_POINT ( 'NONE',  ( 0.000000000000000000, 0.000000000000000000, -2.755905511811024056 ) ) ;
#63258 = CARTESIAN_POINT ( 'NONE',  ( 1.023622047244095334, -0.1870078740157479769, 0.4822834645669291653 ) ) ;
#63260 = CARTESIAN_POINT ( 'NONE',  ( -1.522309711286088607, 0.1283753931104746893, -0.1820866141732285504 ) ) ;
#63261 = CARTESIAN_POINT ( 'NONE',  ( 0.07874015748031558404, -0.1870078740157479769, 0.4822834645669291653 ) ) ;
#63262 = CARTESIAN_POINT ( 'NONE',  ( 0.8070866141732288002, 0.07958543189024085140, 0.2665933059059887866 ) ) ;
#63263 = CARTESIAN_POINT ( 'NONE',  ( -1.692913385826770645, 0.1771653543307087630, 0.000000000000000000 ) ) ;
#63264 = CARTESIAN_POINT ( 'NONE',  ( 1.023622047244095334, -0.1870078740157479769, 0.4822834645669291653 ) ) ;
#63265 = LINE ( 'NONE', #68767, #77420 ) ;
#63266 = CARTESIAN_POINT ( 'NONE',  ( -0.3674540682414692561, -0.5023911411419708095, -0.1820866141732282451 ) ) ;
#63267 = CARTESIAN_POINT ( 'NONE',  ( -0.5971128608923877978, 0.2952755905511811885, 0.1292274648535926551 ) ) ;
#63268 = CARTESIAN_POINT ( 'NONE',  ( 1.423884514435696413, -0.3162353388693409650, -0.4822834645669289433 ) ) ;
#63269 = CARTESIAN_POINT ( 'NONE',  ( -1.003937007874015297, -0.5400638737290845981, -0.3530559997133363437 ) ) ;
#63270 = AXIS2_PLACEMENT_3D ( 'NONE', #35509, #29602, #11082 ) ;
#63271 = CARTESIAN_POINT ( 'NONE',  ( 1.450131233595801428, -0.6692913385826773087, -0.1292274648535924053 ) ) ;
#63272 = CARTESIAN_POINT ( 'NONE',  ( 0.3917322834645670659, -0.1049643490035303273, -0.8956886071204221977 ) ) ;
#63273 = B_SPLINE_CURVE_WITH_KNOTS ( 'NONE', 3,
 ( #56702, #43240, #25540, #81995 ),
 .UNSPECIFIED., .F., .F.,
 ( 4, 4 ),
 ( 1.040834085586084411E-17, 0.001346657832031600320 ),
 .UNSPECIFIED. ) ;
#63274 = CARTESIAN_POINT ( 'NONE',  ( -1.194225721784776262, -0.3690944881889763329, 0.3153832671262228327 ) ) ;
#63275 = CARTESIAN_POINT ( 'NONE',  ( 1.074111983884923571, 1.191141316951608076, 0.3246562585368536480 ) ) ;
#63276 = CARTESIAN_POINT ( 'NONE',  ( 1.141732283464567566, 0.2952755905511811885, 0.000000000000000000 ) ) ;
#63277 = CARTESIAN_POINT ( 'NONE',  ( -0.4724409448818899238, 0.1265901696524986686, -2.471784776902887337 ) ) ;
#63278 = CARTESIAN_POINT ( 'NONE',  ( -1.515748031496062076, 0.1660481256975883668, -0.3530559997133364547 ) ) ;
#63279 = CARTESIAN_POINT ( 'NONE',  ( -1.633858267716534529, 0.07958543189024085140, 0.2665933059059887866 ) ) ;
#63280 = CARTESIAN_POINT ( 'NONE',  ( -1.181102362204723644, -0.1870078740157480601, -0.3641732283464567677 ) ) ;
#63282 = CARTESIAN_POINT ( 'NONE',  ( 1.541994750656168645, 0.1771653543307087075, -0.09757992244046823083 ) ) ;
#63281 =( BOUNDED_CURVE ( )  B_SPLINE_CURVE ( 2, ( #39760, #14108, #6939, #20410, #32611, #65456, #7788, #33455, #59117, #1474, #27128, #52792, #78502 ),
 .UNSPECIFIED., .F., .F. ) 
 B_SPLINE_CURVE_WITH_KNOTS ( ( 3, 2, 2, 2, 2, 2, 3 ),
 ( 0.2194878114796872115, 0.2196969696969696961, 0.2234848484848484806, 0.2272727272727272652, 0.2310606060606060497, 0.2348484848484848619, 0.2350576430657673466 ),
 .UNSPECIFIED. ) 
 CURVE ( )  GEOMETRIC_REPRESENTATION_ITEM ( )  RATIONAL_B_SPLINE_CURVE ( ( 0.9964447847208424136, 0.9981185001348094055, 1.000000000000000000, 0.9659258262890683122, 1.000000000000000000, 0.9659258262890683122, 1.000000000000000000, 0.9659258262890683122, 1.000000000000000000, 0.9659258262890683122, 1.000000000000000000, 0.9981185001348095165, 0.9964447847208426357 ) ) 
 REPRESENTATION_ITEM ( '' )  );
#63283 = CARTESIAN_POINT ( 'NONE',  ( -0.5118110236220466680, 0.2952755905511811885, 0.000000000000000000 ) ) ;
#63284 = CARTESIAN_POINT ( 'NONE',  ( 0.07217847769028949700, -0.2845877964562159024, 0.3641732283464567677 ) ) ;
#63285 = CARTESIAN_POINT ( 'NONE',  ( -1.450131233595799651, -0.5511811023622046335, 0.09757992244046803654 ) ) ;
#63286 = CARTESIAN_POINT ( 'NONE',  ( 1.259842519685040019, -0.1870078740157479769, 0.3641732283464567677 ) ) ;
#63287 = CARTESIAN_POINT ( 'NONE',  ( 0.9645669291338591078, -0.5400638737290845981, -0.3530559997133363437 ) ) ;
#63288 = CARTESIAN_POINT ( 'NONE',  ( 1.535433070866142335, -0.6692913385826771977, 8.415575281601705876E-17 ) ) ;
#63289 = CARTESIAN_POINT ( 'NONE',  ( 0.1574803149606306130, -0.1870078740157480601, -0.3641732283464567677 ) ) ;
#63290 = CARTESIAN_POINT ( 'NONE',  ( 0.5380577427821529035, -0.4281496062992124485, 0.4176697321401328655 ) ) ;
#63291 = VECTOR ( 'NONE', #26029, 39.37007874015748143 ) ;
#63292 = CARTESIAN_POINT ( 'NONE',  ( 1.187664041994751285, -0.2845877964562161244, -0.3641732283464567121 ) ) ;
#63293 = ORIENTED_EDGE ( 'NONE', *, *, #32000, .T. ) ;
#63294 = CARTESIAN_POINT ( 'NONE',  ( -1.489501312335957062, -0.05778040916215522460, 0.4822834645669289988 ) ) ;
#63295 = EDGE_CURVE ( 'NONE', #6920, #3121, #76020, .T. ) ;
#63296 = CARTESIAN_POINT ( 'NONE',  ( -1.423884514435694859, -0.05778040916215560624, -0.4822834645669293319 ) ) ;
#63297 = CARTESIAN_POINT ( 'NONE',  ( -0.2034120734908131112, -0.6692913385826773087, -0.1292274648535924053 ) ) ;
#63298 = CARTESIAN_POINT ( 'NONE',  ( -9.787531504996567848E-17, 0.3996062992125986035, -0.3149606299212598381 ) ) ;
#63299 = CARTESIAN_POINT ( 'NONE',  ( -9.787531504996566615E-17, 0.3996062992125985480, -2.753937007874015741 ) ) ;
#63300 = CARTESIAN_POINT ( 'NONE',  ( 0.3740157480314966754, 0.1660481256975883668, -0.3530559997133364547 ) ) ;
#63301 = CARTESIAN_POINT ( 'NONE',  ( 1.017060367454068581, -0.08942795157528024563, -0.3641732283464568787 ) ) ;
#63302 = CARTESIAN_POINT ( 'NONE',  ( -0.1837270341207340729, 0.2306618581243847221, -0.2411417322834647770 ) ) ;
#63303 = CARTESIAN_POINT ( 'NONE',  ( 0.4724409448818904789, -0.1870078740157479769, 0.4822834645669291653 ) ) ;
#63304 = CARTESIAN_POINT ( 'NONE',  ( 0.1998031496062992740, 0.3460692066303959757, -2.349081364829396446 ) ) ;
#63305 = CARTESIAN_POINT ( 'NONE',  ( -0.3949938075777409408, -0.1058382717557502933, -1.463254593175853158 ) ) ;
#63306 = CARTESIAN_POINT ( 'NONE',  ( -0.1070741851644056997, 0.3996062992125986035, -2.841207349081364963 ) ) ;
#63307 = CARTESIAN_POINT ( 'NONE',  ( -0.4824498642376744417, -2.567464376874931580E-15, -0.4445507791589072832 ) ) ;
#63308 = CARTESIAN_POINT ( 'NONE',  ( -0.2867679344610366554, 0.2867679344610365444, -0.4842519685039368693 ) ) ;
#63309 = CARTESIAN_POINT ( 'NONE',  ( -0.5446194225721777693, -0.2845877964562161244, -0.3641732283464567121 ) ) ;
#63310 = CARTESIAN_POINT ( 'NONE',  ( -0.5971128608923877978, 0.2952755905511811885, 0.1292274648535926551 ) ) ;
#63311 = CARTESIAN_POINT ( 'NONE',  ( -0.3949938075777408852, -0.1058382717557502933, -2.642388451443569597 ) ) ;
#63312 = B_SPLINE_CURVE_WITH_KNOTS ( 'NONE', 3,
 ( #12699, #25721, #38358, #32045 ),
 .UNSPECIFIED., .F., .F.,
 ( 4, 4 ),
 ( 3.593986969204291827E-07, 0.001287825409103274298 ),
 .UNSPECIFIED. ) ;
#63313 = CARTESIAN_POINT ( 'NONE',  ( 0.7808398950131241190, -0.05778040916215560624, -0.4822834645669293319 ) ) ;
#63314 = CARTESIAN_POINT ( 'NONE',  ( -1.404199475065615932, -0.4281496062992127816, -0.4176697321401328100 ) ) ;
#63315 = CARTESIAN_POINT ( 'NONE',  ( 0.9514435695538062676, -0.05778040916215522460, 0.4822834645669289988 ) ) ;
#63316 = CARTESIAN_POINT ( 'NONE',  ( -0.1265901696524993347, 0.4724409448818895907, -2.683727034120735322 ) ) ;
#63317 = CARTESIAN_POINT ( 'NONE',  ( 0.1998031496062994405, -0.3460692066303958092, -2.296587926509186417 ) ) ;
#63318 = CARTESIAN_POINT ( 'NONE',  ( 1.627296587926509996, -0.6046776061558807314, 0.2411417322834647770 ) ) ;
#63319 = CARTESIAN_POINT ( 'NONE',  ( 0.8267716535433077274, 0.2952755905511811885, 0.000000000000000000 ) ) ;
#63320 = CARTESIAN_POINT ( 'NONE',  ( 0.6758530183727039509, 0.2952755905511810774, -0.1292274648535930714 ) ) ;
#63321 = CARTESIAN_POINT ( 'NONE',  ( 0.9908136482939640111, 0.1771653543307087075, -0.09757992244046823083 ) ) ;
#63322 = CARTESIAN_POINT ( 'NONE',  ( 1.450131233595801428, -0.6692913385826773087, -0.1292274648535924053 ) ) ;
#63323 = CARTESIAN_POINT ( 'NONE',  ( 0.3392501089628018884, -0.1958661417322834220, -0.03215223097112869521 ) ) ;
#63324 = FACE_OUTER_BOUND ( 'NONE', #66310, .T. ) ;
#63325 = CARTESIAN_POINT ( 'NONE',  ( 0.8595800524934390507, -0.3162353388693405765, 0.4822834645669290543 ) ) ;
#63326 = CARTESIAN_POINT ( 'NONE',  ( 1.673228346456693494, 0.07958543189024085140, 0.2665933059059887866 ) ) ;
#63327 = CARTESIAN_POINT ( 'NONE',  ( -0.4068241469816267775, 0.05413385826771626580, -0.4176697321401330321 ) ) ;
#63328 = CARTESIAN_POINT ( 'NONE',  ( -1.161417322834644716, -0.5400638737290845981, -0.3530559997133363437 ) ) ;
#63329 = PRESENTATION_LAYER_ASSIGNMENT (  '', '', ( #52567 ) ) ;
#63330 = CARTESIAN_POINT ( 'NONE',  ( 1.010498687664042716, 0.05413385826771626580, -0.4176697321401330321 ) ) ;
#63331 = CARTESIAN_POINT ( 'NONE',  ( 0.2867679344610365999, 0.2867679344610365999, -0.5374015748031496509 ) ) ;
#63332 = CARTESIAN_POINT ( 'NONE',  ( 0.1049643490035304938, -0.3917322834645669549, -1.337270341207349000 ) ) ;
#63333 = CARTESIAN_POINT ( 'NONE',  ( -0.3392501089628019995, 0.1958661417322832277, -2.853018372703412187 ) ) ;
#63334 = CARTESIAN_POINT ( 'NONE',  ( 1.391076115485564868, 0.2306618581243847221, -0.2411417322834647770 ) ) ;
#63335 = ORIENTED_EDGE ( 'NONE', *, *, #10620, .T. ) ;
#63336 = CARTESIAN_POINT ( 'NONE',  ( -0.2925321140481930704, -0.2925321140481933480, -0.05905511811023622659 ) ) ;
#63337 = ORIENTED_EDGE ( 'NONE', *, *, #22330, .F. ) ;
#63338 = CARTESIAN_POINT ( 'NONE',  ( -1.604771003085130765, 0.4514378173630708146, 0.1466069496707738118 ) ) ;
#63339 = CARTESIAN_POINT ( 'NONE',  ( 1.515748031496063186, -0.4536011799217368745, -0.2665933059059886201 ) ) ;
#63340 = CARTESIAN_POINT ( 'NONE',  ( 0.1998031496062992740, 0.3460692066303959757, -1.246719160104986734 ) ) ;
#63341 = CARTESIAN_POINT ( 'NONE',  ( 1.377952755905512472, 0.1771653543307087630, 0.000000000000000000 ) ) ;
#63342 = CARTESIAN_POINT ( 'NONE',  ( 0.6192220670824153395, 2.084810923686589862E-15, -0.4118477457932985253 ) ) ;
#63343 = DIRECTION ( 'NONE',  ( 0.000000000000000000, 0.000000000000000000, -1.000000000000000000 ) ) ;
#63344 = CARTESIAN_POINT ( 'NONE',  ( 0.4330708661417329575, 1.726086921369708538, 0.000000000000000000 ) ) ;
#63345 = CARTESIAN_POINT ( 'NONE',  ( 0.2867679344610365999, -0.2867679344610365444, -0.3405511811023621549 ) ) ;
#63346 = CARTESIAN_POINT ( 'NONE',  ( -0.5314960629921250401, 0.07958543189024085140, 0.2665933059059887866 ) ) ;
#63347 = CARTESIAN_POINT ( 'NONE',  ( -1.587926509186350810, -0.3690944881889763329, 0.3153832671262228327 ) ) ;
#63348 = CARTESIAN_POINT ( 'NONE',  ( -1.174540682414697335, -0.05778040916215522460, 0.4822834645669289988 ) ) ;
#63349 = CARTESIAN_POINT ( 'NONE',  ( 0.04593175853018440641, 0.2952755905511810774, -0.1292274648535930714 ) ) ;
#63350 = CARTESIAN_POINT ( 'NONE',  ( 1.607611548556431069, 0.2952755905511811885, 0.1292274648535926551 ) ) ;
#63351 = VECTOR ( 'NONE', #69058, 39.37007874015748143 ) ;
#63352 = ORIENTED_EDGE ( 'NONE', *, *, #7798, .F. ) ;
#63353 = CARTESIAN_POINT ( 'NONE',  ( 1.601049868766404982, 0.2306618581243848609, 0.2411417322834645549 ) ) ;
#63354 = CARTESIAN_POINT ( 'NONE',  ( 4.871931309127654153, 2.418298854841256951, 6.711999692612117485 ) ) ;
#63355 = CARTESIAN_POINT ( 'NONE',  ( 0.3458507752293908943, 0.3458507752293908943, -2.027559055118109743 ) ) ;
#63356 = CARTESIAN_POINT ( 'NONE',  ( 1.586052503253845281, 1.023622047244095556, -0.1653254495020587966 ) ) ;
#63357 = CARTESIAN_POINT ( 'NONE',  ( -0.4002624671916004129, -0.2845877964562159024, 0.3641732283464567677 ) ) ;
#63358 = CARTESIAN_POINT ( 'NONE',  ( -1.246719160104985846, -0.4281496062992127816, -0.4176697321401328100 ) ) ;
#63359 = CARTESIAN_POINT ( 'NONE',  ( 0.8530183727034128527, -0.4281496062992124485, 0.4176697321401328655 ) ) ;
#63360 = ORIENTED_EDGE ( 'NONE', *, *, #78140, .T. ) ;
#63362 = CARTESIAN_POINT ( 'NONE',  ( 5.785732909357575061E-17, -0.4724409448818898682, -2.675196850393700920 ) ) ;
#63361 = CARTESIAN_POINT ( 'NONE',  ( 0.7283464566929142014, 0.1660481256975885056, 0.3530559997133364547 ) ) ;
#63363 = CARTESIAN_POINT ( 'NONE',  ( 1.102362204724410155, -0.1870078740157480879, -0.4822834645669291653 ) ) ;
#63364 = CARTESIAN_POINT ( 'NONE',  ( -1.023622047244094002, -0.1870078740157480879, -0.4822834645669291653 ) ) ;
#63365 = CARTESIAN_POINT ( 'NONE',  ( -0.1958661417322836440, 0.3392501089628016664, -0.4081171671577935034 ) ) ;
#63366 = CARTESIAN_POINT ( 'NONE',  ( -0.2230971128608915943, -0.3690944881889765550, -0.3153832671262227771 ) ) ;
#63367 = CARTESIAN_POINT ( 'NONE',  ( -0.1958661417322834220, -0.3392501089628018884, -0.7801837270341208663 ) ) ;
#63368 = CARTESIAN_POINT ( 'NONE',  ( -0.3477690288713902178, 0.1771653543307087075, -0.09757992244046823083 ) ) ;
#63369 = CARTESIAN_POINT ( 'NONE',  ( 0.5052493438320215802, 0.1771653543307087630, 0.09757992244046791164 ) ) ;
#63370 = CARTESIAN_POINT ( 'NONE',  ( 0.3280839895013130669, 0.05413385826771666132, 0.4176697321401328100 ) ) ;
#63371 = CARTESIAN_POINT ( 'NONE',  ( -0.5774278215223089816, -0.5023911411419708095, 0.1820866141732285504 ) ) ;
#63372 = CARTESIAN_POINT ( 'NONE',  ( 0.1958661417322836440, -0.3392501089628017219, -2.918635170603674389 ) ) ;
#63373 = CARTESIAN_POINT ( 'NONE',  ( 1.220472440944882386, -0.6692913385826771977, 8.415575281601705876E-17 ) ) ;
#63374 = CARTESIAN_POINT ( 'NONE',  ( -0.9055118110236215490, -0.6692913385826771977, 8.415575281601705876E-17 ) ) ;
#63375 = CARTESIAN_POINT ( 'NONE',  ( -0.2362204724409451284, 0.4091458600556402425, -1.034776902887139194 ) ) ;
#63376 = CARTESIAN_POINT ( 'NONE',  ( -0.3805774278215216522, -0.4281496062992127816, -0.4176697321401328100 ) ) ;
#63377 = CARTESIAN_POINT ( 'NONE',  ( -0.7545931758530176614, -0.6692913385826773087, -0.1292274648535924053 ) ) ;
#63378 = CARTESIAN_POINT ( 'NONE',  ( 1.377952755905512472, 0.1771653543307087630, 0.000000000000000000 ) ) ;
#63379 = CARTESIAN_POINT ( 'NONE',  ( 0.1181102362204730916, -0.5511811023622047445, 6.969142054262312111E-17 ) ) ;
#63380 = CARTESIAN_POINT ( 'NONE',  ( -0.4986876640419942164, -0.6046776061558807314, 0.2411417322834647770 ) ) ;
#63381 = CARTESIAN_POINT ( 'NONE',  ( -1.227034120734907141, -0.6692913385826773087, -0.1292274648535924053 ) ) ;
#63382 = CARTESIAN_POINT ( 'NONE',  ( -0.7270051398050848546, 2.375327444609086402, 0.4916655823645582069 ) ) ;
#63383 = CARTESIAN_POINT ( 'NONE',  ( 1.581364829396326277, -0.2845877964562161244, -0.3641732283464567121 ) ) ;
#63384 = CARTESIAN_POINT ( 'NONE',  ( -0.4199475065616791736, -0.6046776061558807314, 0.2411417322834647770 ) ) ;
#63385 = PRESENTATION_LAYER_ASSIGNMENT (  '', '', ( #5590 ) ) ;
#63386 = CARTESIAN_POINT ( 'NONE',  ( -1.135170603674539924, -0.6692913385826771977, 0.1292274648535927661 ) ) ;
#63387 = ORIENTED_EDGE ( 'NONE', *, *, #50646, .F. ) ;
#63388 = CARTESIAN_POINT ( 'NONE',  ( 0.3996062992125985480, 2.446882876249141654E-17, -2.084645669291338432 ) ) ;
#63389 = CARTESIAN_POINT ( 'NONE',  ( 1.272965879265092637, 0.05413385826771666132, 0.4176697321401328100 ) ) ;
#63390 = CARTESIAN_POINT ( 'NONE',  ( -0.7349081364829390672, 0.1283753931104746893, -0.1820866141732285504 ) ) ;
#63391 = CARTESIAN_POINT ( 'NONE',  ( -0.2925321140481932369, 0.2925321140481931259, -1.513779527559055094 ) ) ;
#63392 = CARTESIAN_POINT ( 'NONE',  ( -0.9055118110236215490, 0.2952755905511811885, 0.000000000000000000 ) ) ;
#63393 = CARTESIAN_POINT ( 'NONE',  ( 1.220472440944882608, 0.2952755905511811885, 0.000000000000000000 ) ) ;
#63394 = CARTESIAN_POINT ( 'NONE',  ( 0.8792650918635177559, 0.05413385826771666132, 0.4176697321401328100 ) ) ;
#63395 = CARTESIAN_POINT ( 'NONE',  ( -0.2017716535433071445, -0.2017716535433071445, -0.3937007874015748254 ) ) ;
#63396 = CARTESIAN_POINT ( 'NONE',  ( -1.272965879265091305, -0.3690944881889763329, 0.3153832671262228327 ) ) ;
#63397 = CARTESIAN_POINT ( 'NONE',  ( -0.3996062992125985480, -7.340648628747423112E-17, -0.5885826771653542844 ) ) ;
#63398 = CARTESIAN_POINT ( 'NONE',  ( 0.3996062992125986590, -0.1070741851644053111, -1.056430446194225992 ) ) ;
#63399 = CARTESIAN_POINT ( 'NONE',  ( 0.3949938075777411073, -0.1058382717557499464, -0.2690288713910761742 ) ) ;
#63400 = CARTESIAN_POINT ( 'NONE',  ( 0.3790285851608848899, 0.1011035889004421734, -1.220472440944882164 ) ) ;
#63401 = CARTESIAN_POINT ( 'NONE',  ( 1.266404199475066328, -0.2845877964562161244, -0.3641732283464567121 ) ) ;
#63402 = CARTESIAN_POINT ( 'NONE',  ( 0.9251968503937015864, -0.4536011799217367080, 0.2665933059059888421 ) ) ;
#63403 = CARTESIAN_POINT ( 'NONE',  ( 0.4658792650918640033, -0.3162353388693405765, 0.4822834645669290543 ) ) ;
#63404 = CARTESIAN_POINT ( 'NONE',  ( 0.4606732211678724598, 1.763126522798933227, -0.5309055118110237448 ) ) ;
#63405 = CARTESIAN_POINT ( 'NONE',  ( -9.674558042662122972E-17, 0.3949938075777409963, -1.494094488188976388 ) ) ;
#63406 = CARTESIAN_POINT ( 'NONE',  ( 0.9908136482939640111, -0.5511811023622046335, 0.09757992244046803654 ) ) ;
#63407 =( BOUNDED_SURFACE ( )  B_SPLINE_SURFACE ( 1, 2, ( 
 ( #31331, #11995, #10760, #63326, #57413, #44358, #17906, #43955, #43128, #62924, #23787, #56996, #17498, #17087, #56588, #75973, #49458, #69651, #37649, #81470, #5258, #62506, #82693, #49865, #11173, #30922, #36833, #4435, #24195, #38062, #25012, #81884, #43542, #36420, #42724, #69241, #50685, #4844, #30519, #18313, #70049, #76383, #82289, #12404, #68420, #63738, #75565, #56181, #31751, #23374, #49042, #74739, #77632, #25425, #78473, #38479, #51090, #64997, #38894, #20797, #76787, #6910, #26266, #46453, #19119, #32582, #14082, #51927, #65839, #1445, #189, #77206, #72146, #14502, #58245, #6496, #8172, #64163, #13656, #40155, #39734, #44768, #33837, #70895, #33429, #32166, #7332, #33000, #59090, #70465, #83106, #19535, #12822, #78051, #65430, #13245, #57822, #25842, #51502, #45192, #64573, #610, #19964, #46032, #45615, #71309, #39309, #27102, #58670, #1035, #20380, #26689, #52344, #71727, #7763, #52764, #21622, #60750, #14907, #47282, #67082, #72560, #10249, #74227, #3102, #54429, #80139, #2690, #2274, #42218, #72972, #53175, #67913, #47700, #28767, #80554, #73396, #40989, #48119, #15746, #59504, #16572, #40567, #41801, #22040, #22461, #73817, #66248, #27937, #15324, #16154, #53595, #67492, #9414, #41400, #59919, #35084, #1857, #66668, #35499, #79304, #27519, #22866, #21211, #9828, #3514, #8587, #61163, #29183, #54851, #48527, #78890, #46866, #34258, #9007, #34679, #60342, #28350, #54011, #79723, #30828, #69555, #61996, #82599, #24916, #76291, #49359, #23275, #43441, #16988, #18217, #50584, #5571, #69956, #29999, #43033, #36727, #68729, #4333, #55663, #5164, #69139, #75468, #36322, #17808, #35920, #75056, #11903, #81372, #18622, #56903, #80960, #11490, #63231, #68328, #75875, #37144, #37557, #44265, #62829, #56493, #82195, #24512, #23685, #62403, #31236, #49768, #50180, #43852, #61586, #17403, #3932, #29590, #55253, #11069, #48945, #74646, #42631, #10666, #4742, #30415, #56083, #81788, #24099, #13150, #19443, #38382, #6398, #33340, #27009, #45093, #19025, #78377, #76691, #26169, #52670, #52251, #63643, #59002, #92, #45934, #44673, #19870, #45520, #71633, #83008, #7669, #32068, #37967, #7236, #26599, #25745, #25329, #12723, #70368, #20708, #64059, #1357, #31653, #58576, #46361, #50993, #70797, #13985, #77110, #51408, #32910, #12310, #71215, #64476, #57729, #38800, #6813, #13558, #32484, #58147, #39214, #516, #5982, #57310, #64899, #941, #77957, #51830, #77535, #20285, #39641, #65332, #48025, #15232, #2599, #28676, #40892, #34164, #47608, #66573, #16064, #80047, #59410, #41307, #72883, #21949, #28257, #27423, #46781, #40480, #73303, #53918, #79631, #66993, #72472, #54337, #22366, #73725, #8498, #33748, #34583, #1766, #9325, #72054, #3009, #14411, #66158, #53508, #21532, #27847, #14821, #59826, #40065, #65752, #47191, #2180, #8085, #79216, #15651, #53085, #78797, #8907, #21121, #60251, #34995, #60660, #71484, #13831, #14256, #51260, #59260, #57998, #6245, #58851, #78225, #77380, #76962, #64328, #12995, #20969, #38651, #52934, #83274, #26858, #1617, #19291, #71065, #65603, #45370, #19711, #1208, #14671, #39490, #32756, #44942, #6664, #26018, #65177, #70639, #51677, #7514, #32336, #63909, #78647, #33183, #52517, #20558, #7085, #362, #46628, #13409, #57583, #72324, #52097, #46210, #27273, #77806, #39064, #71905, #20137, #31922, #25597, #64747, #39914, #26444, #7934, #33595, #58423, #784, #45785, #52302, #13613, #33387, #78008, #7719, #78845, #59050, #20758, #1404, #64530, #34213, #77589, #6867, #46408, #20336, #59876, #32536, #45988, #65384, #2230, #58200, #71684, #53134, #27060, #21578, #40529, #39267, #53555, #27895, #78430, #72102, #1814, #14460, #64949, #39693, #8547, #52719, #65799, #33798, #72519, #7289, #79263, #47240, #72930, #14036, #26221, #40112, #19923, #21172, #38850, #568, #51884, #32959, #8133, #59463, #27476, #58626, #993, #45573, #71266, #46827, #26648, #14867, #66208, #29136, #29950, #55206, #66621, #36276, #3055, #48897, #21995, #22822, #48480, #74599, #2647, #10619, #9370, #40942, #10204, #29544, #28721, #28304, #15700, #47656 ),
 ( #67448, #79678, #41357, #60706, #16528, #53966, #54384, #74181, #73352, #49309, #55614, #42172, #35873, #61539, #41753, #67038, #81325, #80094, #8959, #23639, #3470, #67867, #61948, #54803, #22414, #3884, #80507, #15281, #34633, #35041, #80914, #61118, #23227, #16942, #48071, #73773, #16109, #42583, #9782, #68284, #4288, #60297, #35453, #56850, #75010, #30782, #50946, #75417, #32020, #12673, #36678, #50535, #18974, #24050, #31601, #82548, #76643, #70318, #38332, #5115, #11440, #37507, #63182, #68680, #57680, #82960, #64008, #17761, #50127, #12260, #25278, #5520, #44216, #69906, #44623, #69092, #6349, #11022, #63594, #5929, #81741, #31186, #18573, #30366, #42, #57261, #25695, #62354, #17357, #42985, #4692, #69505, #37917, #37096, #24867, #43392, #56033, #62781, #49721, #76239, #56443, #82146, #24461, #75827, #18168, #43801, #11854, #8034, #77904, #45467, #58950, #58096, #6761, #52200, #66107, #53033, #26547, #71581, #64427, #45044, #13932, #33698, #71165, #461, #46310, #46729, #59358, #1308, #33289, #64846, #26117, #45883, #7184, #20235, #1717, #39589, #26957, #65278, #77059, #72421, #32433, #19392, #52620, #32855, #14770, #70745, #58524, #7617, #40426, #13097, #889, #65704, #78326, #34113, #78746, #51778, #8443, #77483, #59774, #13505, #20657, #19818, #39161, #27372, #21071, #2129, #38750, #72004, #14360, #40017, #51356, #48383, #34533, #41259, #79578, #74498, #10523, #66523, #68184, #15599, #47140, #35769, #66945, #16845, #61020, #8855, #42479, #10105, #16428, #15181, #67769, #61850, #23132, #22313, #74082, #47557, #67354, #28207, #61439, #21894, #21482, #3371, #29035, #53866, #42074, #3786, #2549, #41663, #9277, #29449, #54283, #73250, #35358, #60198, #34948, #28625, #36177, #55108, #2960, #47976, #40838, #72831, #73675, #80817, #60611, #79999, #22724, #48800, #27797, #54706, #9687, #16017, #80412, #53457, #79165, #56350, #44124, #24364, #69409, #82051, #29854, #82863, #42888, #55517, #11763, #43294, #25185, #81225, #11340, #30689, #50852, #23541, #37000, #18482, #50034, #70217, #5831, #4596, #18880, #30267, #76552, #23954, #62679, #10924, #49622, #69816, #12165, #44529, #49210, #75316, #5021, #68583, #37821, #24771, #36581, #17663, #55931, #12574, #38231, #62260, #4191, #68991, #74914, #63497, #75731, #17260, #37417, #81646, #18071, #43706, #63089, #5427, #31089, #56756, #82456, #31504, #50440, #76141, #57164, #2345, #15388, #78959, #34324, #59986, #66735, #57997, #9074, #57582, #53661, #79368, #70638, #21278, #8653, #28001, #19289, #54075, #47350, #21687, #51259, #73039, #15816, #60405, #59568, #41050, #1512, #46933, #64327, #34745, #27166, #83273, #14973, #66314, #6663, #2756, #28415, #38650, #72625, #20865, #79790, #8238, #52828, #40632, #12994, #44941, #65902, #22106, #47766, #40220, #1924, #76961, #25596, #27587, #73464, #78540, #32335, #63908, #6244, #31921, #46515, #72217, #14568, #33904, #53244, #54912, #10318, #81440, #61653, #23341, #35983, #67150, #36798, #80205, #9479, #49012, #80618, #62474, #35154, #48596, #67976, #4809, #60814, #74292, #55732, #3994, #24165, #43098, #41868, #56150, #67562, #30485, #61228, #16638, #48184, #3581, #23754, #49428, #81854, #3166, #29248, #42278, #22522, #75122, #62062, #73881, #22930, #9894, #49834, #75533, #16221, #41465, #29658, #28830, #17467, #55320, #54494, #74709, #35565, #81029, #17055, #42695, #68392, #10731, #36388, #4401, #68794, #30069, #11139, #76354, #38445, #51470, #31718, #70432, #12789, #19504, #11965, #45158, #11556, #6463, #32133, #24577, #57378, #83073, #31301, #75940, #12373, #56965, #70020, #57790, #38031, #25394, #63706, #43507, #13213, #56558, #69207, #51058, #82663, #38859, #37213, #24978, #44329, #64540, #62892, #50651, #157, #6046, #577, #70862, #18281, #32547, #43923, #6877, #37620, #18686, #50244, #63296, #25810, #77173, #58211, #5227, #5634, #76758, #82259, #26231, #64128, #69620, #19088, #44737, #51894, #17873, #30891, #34642, #65394, #13624, #2239, #33397, #40951, #27485, #72939, #15291, #7729, #14048, #40122, #65809, #71275, #60307, #27904, #66631, #20346, #52729, #14878 ) ),
 .UNSPECIFIED., .F., .F., .F. ) 
 B_SPLINE_SURFACE_WITH_KNOTS ( ( 2, 2 ),
 ( 3, 2, 2, 2, 2, 2, 2, 2, 2, 2, 2, 2, 2, 2, 2, 2, 2, 2, 2, 2, 2, 2, 2, 2, 2, 2, 2, 2, 2, 2, 2, 2, 2, 2, 2, 2, 2, 2, 2, 2, 2, 2, 2, 2, 2, 2, 2, 2, 2, 2, 2, 2, 2, 2, 2, 2, 2, 2, 2, 2, 2, 2, 2, 2, 2, 2, 2, 2, 2, 2, 2, 2, 2, 2, 2, 2, 2, 2, 2, 2, 2, 2, 2, 2, 2, 2, 2, 2, 2, 2, 2, 2, 2, 2, 2, 2, 2, 2, 2, 2, 2, 2, 2, 2, 2, 2, 2, 2, 2, 2, 2, 2, 2, 2, 2, 2, 2, 2, 2, 2, 2, 2, 2, 2, 2, 2, 2, 2, 2, 2, 2, 2, 2, 2, 2, 2, 2, 2, 2, 2, 2, 2, 2, 2, 2, 2, 2, 2, 2, 2, 2, 2, 2, 2, 2, 2, 2, 2, 2, 2, 2, 2, 2, 2, 2, 2, 2, 2, 2, 2, 2, 2, 2, 2, 2, 2, 2, 2, 2, 2, 2, 2, 2, 2, 2, 2, 2, 2, 2, 2, 2, 2, 2, 2, 2, 2, 2, 2, 2, 2, 2, 2, 2, 2, 2, 2, 2, 2, 2, 2, 2, 2, 2, 2, 2, 2, 2, 2, 2, 2, 2, 2, 2, 2, 2, 2, 2, 2, 2, 2, 2, 2, 2, 2, 2, 2, 2, 2, 2, 2, 2, 2, 2, 2, 2, 2, 2, 2, 2, 2, 2, 2, 2, 2, 2, 3 ),
 ( 0.000000000000000000, 1.000000000000000000 ),
 ( 0.000000000000000000, 0.003787878787878787984, 0.007575757575757575968, 0.01136363636363636395, 0.01515151515151515194, 0.01893939393939393992, 0.02272727272727272790, 0.02651515151515151589, 0.03030303030303030387, 0.03409090909090908839, 0.03787878787878787984, 0.04166666666666666435, 0.04545454545454545581, 0.04924242424242424032, 0.05303030303030303177, 0.05681818181818181629, 0.06060606060606060774, 0.06439393939393939226, 0.06818181818181817677, 0.07196969696969697516, 0.07575757575757575968, 0.07954545454545454419, 0.08333333333333332871, 0.08712121212121212710, 0.09090909090909091161, 0.09469696969696969613, 0.09848484848484848064, 0.1022727272727272790, 0.1060606060606060635, 0.1098484848484848481, 0.1136363636363636326, 0.1174242424242424310, 0.1212121212121212155, 0.1250000000000000000, 0.1287878787878787845, 0.1325757575757575690, 0.1363636363636363535, 0.1401515151515151381, 0.1439393939393939503, 0.1477272727272727348, 0.1515151515151515194, 0.1553030303030303039, 0.1590909090909090884, 0.1628787878787878729, 0.1666666666666666574, 0.1704545454545454419, 0.1742424242424242542, 0.1780303030303030387, 0.1818181818181818232, 0.1856060606060606077, 0.1893939393939393923, 0.1931818181818181768, 0.1969696969696969613, 0.2007575757575757458, 0.2045454545454545581, 0.2083333333333333426, 0.2121212121212121271, 0.2159090909090909116, 0.2196969696969696961, 0.2234848484848484806, 0.2272727272727272652, 0.2310606060606060497, 0.2348484848484848619, 0.2386363636363636465, 0.2424242424242424310, 0.2462121212121212155, 0.2500000000000000000, 0.2537878787878787845, 0.2575757575757575690, 0.2613636363636363535, 0.2651515151515151381, 0.2689393939393939226, 0.2727272727272727071, 0.2765151515151514916, 0.2803030303030302761, 0.2840909090909091161, 0.2878787878787879007, 0.2916666666666666852, 0.2954545454545454697, 0.2992424242424242542, 0.3030303030303030387, 0.3068181818181818232, 0.3106060606060606077, 0.3143939393939393923, 0.3181818181818181768, 0.3219696969696969613, 0.3257575757575757458, 0.3295454545454545303, 0.3333333333333333148, 0.3371212121212120993, 0.3409090909090908839, 0.3446969696969697239, 0.3484848484848485084, 0.3522727272727272929, 0.3560606060606060774, 0.3598484848484848619, 0.3636363636363636465, 0.3674242424242424310, 0.3712121212121212155, 0.3750000000000000000, 0.3787878787878787845, 0.3825757575757575690, 0.3863636363636363535, 0.3901515151515151381, 0.3939393939393939226, 0.3977272727272727071, 0.4015151515151514916, 0.4053030303030302761, 0.4090909090909091161, 0.4128787878787879007, 0.4166666666666666852, 0.4204545454545454697, 0.4242424242424242542, 0.4280303030303030387, 0.4318181818181818232, 0.4356060606060606077, 0.4393939393939393923, 0.4431818181818181768, 0.4469696969696969613, 0.4507575757575757458, 0.4545454545454545303, 0.4583333333333333148, 0.4621212121212120993, 0.4659090909090908839, 0.4696969696969697239, 0.4734848484848485084, 0.4772727272727272929, 0.4810606060606060774, 0.4848484848484848619, 0.4886363636363636465, 0.4924242424242424310, 0.4962121212121212155, 0.5000000000000000000, 0.5037878787878787845, 0.5075757575757575690, 0.5113636363636363535, 0.5151515151515151381, 0.5189393939393939226, 0.5227272727272727071, 0.5265151515151514916, 0.5303030303030302761, 0.5340909090909090606, 0.5378787878787878451, 0.5416666666666666297, 0.5454545454545454142, 0.5492424242424241987, 0.5530303030303029832, 0.5568181818181817677, 0.5606060606060605522, 0.5643939393939394478, 0.5681818181818182323, 0.5719696969696970168, 0.5757575757575758013, 0.5795454545454545858, 0.5833333333333333703, 0.5871212121212121549, 0.5909090909090909394, 0.5946969696969697239, 0.5984848484848485084, 0.6022727272727272929, 0.6060606060606060774, 0.6098484848484848619, 0.6136363636363636465, 0.6174242424242424310, 0.6212121212121212155, 0.6250000000000000000, 0.6287878787878787845, 0.6325757575757575690, 0.6363636363636363535, 0.6401515151515151381, 0.6439393939393939226, 0.6477272727272727071, 0.6515151515151514916, 0.6553030303030302761, 0.6590909090909090606, 0.6628787878787878451, 0.6666666666666666297, 0.6704545454545454142, 0.6742424242424241987, 0.6780303030303029832, 0.6818181818181817677, 0.6856060606060605522, 0.6893939393939394478, 0.6931818181818182323, 0.6969696969696970168, 0.7007575757575758013, 0.7045454545454545858, 0.7083333333333333703, 0.7121212121212121549, 0.7159090909090909394, 0.7196969696969697239, 0.7234848484848485084, 0.7272727272727272929, 0.7310606060606060774, 0.7348484848484848619, 0.7386363636363636465, 0.7424242424242424310, 0.7462121212121212155, 0.7500000000000000000, 0.7537878787878787845, 0.7575757575757575690, 0.7613636363636363535, 0.7651515151515151381, 0.7689393939393939226, 0.7727272727272727071, 0.7765151515151514916, 0.7803030303030302761, 0.7840909090909090606, 0.7878787878787878451, 0.7916666666666666297, 0.7954545454545454142, 0.7992424242424241987, 0.8030303030303029832, 0.8068181818181817677, 0.8106060606060605522, 0.8143939393939394478, 0.8181818181818182323, 0.8219696969696970168, 0.8257575757575758013, 0.8295454545454545858, 0.8333333333333333703, 0.8371212121212121549, 0.8409090909090909394, 0.8446969696969697239, 0.8484848484848485084, 0.8522727272727272929, 0.8560606060606060774, 0.8598484848484848619, 0.8636363636363636465, 0.8674242424242424310, 0.8712121212121212155, 0.8750000000000000000, 0.8787878787878787845, 0.8825757575757575690, 0.8863636363636363535, 0.8901515151515151381, 0.8939393939393939226, 0.8977272727272727071, 0.9015151515151514916, 0.9053030303030302761, 0.9090909090909090606, 0.9128787878787878451, 0.9166666666666666297, 0.9204545454545454142, 0.9242424242424241987, 0.9280303030303029832, 0.9318181818181817677, 0.9356060606060605522, 0.9393939393939394478, 0.9431818181818182323, 0.9469696969696970168, 0.9507575757575758013, 0.9545454545454545858, 0.9583333333333333703, 0.9621212121212121549, 0.9659090909090909394 ),
 .UNSPECIFIED. ) 
 GEOMETRIC_REPRESENTATION_ITEM ( )  RATIONAL_B_SPLINE_SURFACE ( (
 ( 1.000000000000000000, 0.9659258262890683122, 1.000000000000000000, 0.9659258262890683122, 1.000000000000000000, 0.9659258262890683122, 1.000000000000000000, 0.9659258262890683122, 1.000000000000000000, 0.9659258262890683122, 1.000000000000000000, 0.9659258262890683122, 1.000000000000000000, 0.9659258262890683122, 1.000000000000000000, 0.9659258262890683122, 1.000000000000000000, 0.9659258262890683122, 1.000000000000000000, 0.9659258262890683122, 1.000000000000000000, 0.9659258262890683122, 1.000000000000000000, 0.9659258262890683122, 1.000000000000000000, 0.9659258262890683122, 1.000000000000000000, 0.9659258262890683122, 1.000000000000000000, 0.9659258262890683122, 1.000000000000000000, 0.9659258262890683122, 1.000000000000000000, 0.9659258262890683122, 1.000000000000000000, 0.9659258262890683122, 1.000000000000000000, 0.9659258262890683122, 1.000000000000000000, 0.9659258262890683122, 1.000000000000000000, 0.9659258262890683122, 1.000000000000000000, 0.9659258262890683122, 1.000000000000000000, 0.9659258262890683122, 1.000000000000000000, 0.9659258262890683122, 1.000000000000000000, 0.9659258262890683122, 1.000000000000000000, 0.9659258262890683122, 1.000000000000000000, 0.9659258262890683122, 1.000000000000000000, 0.9659258262890683122, 1.000000000000000000, 0.9659258262890683122, 1.000000000000000000, 0.9659258262890683122, 1.000000000000000000, 0.9659258262890683122, 1.000000000000000000, 0.9659258262890683122, 1.000000000000000000, 0.9659258262890683122, 1.000000000000000000, 0.9659258262890683122, 1.000000000000000000, 0.9659258262890683122, 1.000000000000000000, 0.9659258262890683122, 1.000000000000000000, 0.9659258262890683122, 1.000000000000000000, 0.9659258262890683122, 1.000000000000000000, 0.9659258262890683122, 1.000000000000000000, 0.9659258262890683122, 1.000000000000000000, 0.9659258262890683122, 1.000000000000000000, 0.9659258262890683122, 1.000000000000000000, 0.9659258262890683122, 1.000000000000000000, 0.9659258262890683122, 1.000000000000000000, 0.9659258262890683122, 1.000000000000000000, 0.9659258262890683122, 1.000000000000000000, 0.9659258262890683122, 1.000000000000000000, 0.9659258262890683122, 1.000000000000000000, 0.9659258262890683122, 1.000000000000000000, 0.9659258262890683122, 1.000000000000000000, 0.9659258262890683122, 1.000000000000000000, 0.9659258262890683122, 1.000000000000000000, 0.9659258262890683122, 1.000000000000000000, 0.9659258262890683122, 1.000000000000000000, 0.9659258262890683122, 1.000000000000000000, 0.9659258262890683122, 1.000000000000000000, 0.9659258262890683122, 1.000000000000000000, 0.9659258262890683122, 1.000000000000000000, 0.9659258262890683122, 1.000000000000000000, 0.9659258262890683122, 1.000000000000000000, 0.9659258262890683122, 1.000000000000000000, 0.9659258262890683122, 1.000000000000000000, 0.9659258262890683122, 1.000000000000000000, 0.9659258262890683122, 1.000000000000000000, 0.9659258262890683122, 1.000000000000000000, 0.9659258262890683122, 1.000000000000000000, 0.9659258262890683122, 1.000000000000000000, 0.9659258262890683122, 1.000000000000000000, 0.9659258262890683122, 1.000000000000000000, 0.9659258262890683122, 1.000000000000000000, 0.9659258262890683122, 1.000000000000000000, 0.9659258262890683122, 1.000000000000000000, 0.9659258262890683122, 1.000000000000000000, 0.9659258262890683122, 1.000000000000000000, 0.9659258262890683122, 1.000000000000000000, 0.9659258262890683122, 1.000000000000000000, 0.9659258262890683122, 1.000000000000000000, 0.9659258262890683122, 1.000000000000000000, 0.9659258262890683122, 1.000000000000000000, 0.9659258262890683122, 1.000000000000000000, 0.9659258262890683122, 1.000000000000000000, 0.9659258262890683122, 1.000000000000000000, 0.9659258262890683122, 1.000000000000000000, 0.9659258262890683122, 1.000000000000000000, 0.9659258262890683122, 1.000000000000000000, 0.9659258262890683122, 1.000000000000000000, 0.9659258262890683122, 1.000000000000000000, 0.9659258262890683122, 1.000000000000000000, 0.9659258262890683122, 1.000000000000000000, 0.9659258262890683122, 1.000000000000000000, 0.9659258262890683122, 1.000000000000000000, 0.9659258262890683122, 1.000000000000000000, 0.9659258262890683122, 1.000000000000000000, 0.9659258262890683122, 1.000000000000000000, 0.9659258262890683122, 1.000000000000000000, 0.9659258262890683122, 1.000000000000000000, 0.9659258262890683122, 1.000000000000000000, 0.9659258262890683122, 1.000000000000000000, 0.9659258262890683122, 1.000000000000000000, 0.9659258262890683122, 1.000000000000000000, 0.9659258262890683122, 1.000000000000000000, 0.9659258262890683122, 1.000000000000000000, 0.9659258262890683122, 1.000000000000000000, 0.9659258262890683122, 1.000000000000000000, 0.9659258262890683122, 1.000000000000000000, 0.9659258262890683122, 1.000000000000000000, 0.9659258262890683122, 1.000000000000000000, 0.9659258262890683122, 1.000000000000000000, 0.9659258262890683122, 1.000000000000000000, 0.9659258262890683122, 1.000000000000000000, 0.9659258262890683122, 1.000000000000000000, 0.9659258262890683122, 1.000000000000000000, 0.9659258262890683122, 1.000000000000000000, 0.9659258262890683122, 1.000000000000000000, 0.9659258262890683122, 1.000000000000000000, 0.9659258262890683122, 1.000000000000000000, 0.9659258262890683122, 1.000000000000000000, 0.9659258262890683122, 1.000000000000000000, 0.9659258262890683122, 1.000000000000000000, 0.9659258262890683122, 1.000000000000000000, 0.9659258262890683122, 1.000000000000000000, 0.9659258262890683122, 1.000000000000000000, 0.9659258262890683122, 1.000000000000000000, 0.9659258262890683122, 1.000000000000000000, 0.9659258262890683122, 1.000000000000000000, 0.9659258262890683122, 1.000000000000000000, 0.9659258262890683122, 1.000000000000000000, 0.9659258262890683122, 1.000000000000000000, 0.9659258262890683122, 1.000000000000000000, 0.9659258262890683122, 1.000000000000000000, 0.9659258262890683122, 1.000000000000000000, 0.9659258262890683122, 1.000000000000000000, 0.9659258262890683122, 1.000000000000000000, 0.9659258262890683122, 1.000000000000000000, 0.9659258262890683122, 1.000000000000000000, 0.9659258262890683122, 1.000000000000000000, 0.9659258262890683122, 1.000000000000000000, 0.9659258262890683122, 1.000000000000000000, 0.9659258262890683122, 1.000000000000000000, 0.9659258262890683122, 1.000000000000000000, 0.9659258262890683122, 1.000000000000000000, 0.9659258262890683122, 1.000000000000000000, 0.9659258262890683122, 1.000000000000000000, 0.9659258262890683122, 1.000000000000000000, 0.9659258262890683122, 1.000000000000000000, 0.9659258262890683122, 1.000000000000000000, 0.9659258262890683122, 1.000000000000000000, 0.9659258262890683122, 1.000000000000000000, 0.9659258262890683122, 1.000000000000000000, 0.9659258262890683122, 1.000000000000000000, 0.9659258262890683122, 1.000000000000000000, 0.9659258262890683122, 1.000000000000000000, 0.9659258262890683122, 1.000000000000000000, 0.9659258262890683122, 1.000000000000000000, 0.9659258262890683122, 1.000000000000000000, 0.9659258262890683122, 1.000000000000000000, 0.9659258262890683122, 1.000000000000000000, 0.9659258262890683122, 1.000000000000000000, 0.9659258262890683122, 1.000000000000000000, 0.9659258262890683122, 1.000000000000000000, 0.9659258262890683122, 1.000000000000000000, 0.9659258262890683122, 1.000000000000000000, 0.9659258262890683122, 1.000000000000000000, 0.9659258262890683122, 1.000000000000000000, 0.9659258262890683122, 1.000000000000000000, 0.9659258262890683122, 1.000000000000000000, 0.9659258262890683122, 1.000000000000000000, 0.9659258262890683122, 1.000000000000000000, 0.9659258262890683122, 1.000000000000000000, 0.9659258262890683122, 1.000000000000000000, 0.9659258262890683122, 1.000000000000000000, 0.9659258262890683122, 1.000000000000000000, 0.9659258262890683122, 1.000000000000000000, 0.9659258262890683122, 1.000000000000000000, 0.9659258262890683122, 1.000000000000000000, 0.9659258262890683122, 1.000000000000000000, 0.9659258262890683122, 1.000000000000000000, 0.9659258262890683122, 1.000000000000000000, 0.9659258262890683122, 1.000000000000000000, 0.9659258262890683122, 1.000000000000000000, 0.9659258262890683122, 1.000000000000000000, 0.9659258262890683122, 1.000000000000000000, 0.9659258262890683122, 1.000000000000000000, 0.9659258262890683122, 1.000000000000000000, 0.9659258262890683122, 1.000000000000000000, 0.9659258262890683122, 1.000000000000000000, 0.9659258262890683122, 1.000000000000000000, 0.9659258262890683122, 1.000000000000000000, 0.9659258262890683122, 1.000000000000000000, 0.9659258262890683122, 1.000000000000000000, 0.9659258262890683122, 1.000000000000000000, 0.9659258262890683122, 1.000000000000000000, 0.9659258262890683122, 1.000000000000000000, 0.9659258262890683122, 1.000000000000000000, 0.9659258262890683122, 1.000000000000000000, 0.9659258262890683122, 1.000000000000000000, 0.9659258262890683122, 1.000000000000000000, 0.9659258262890683122, 1.000000000000000000, 0.9659258262890683122, 1.000000000000000000, 0.9659258262890683122, 1.000000000000000000, 0.9659258262890683122, 1.000000000000000000, 0.9659258262890683122, 1.000000000000000000, 0.9659258262890683122, 1.000000000000000000, 0.9659258262890683122, 1.000000000000000000, 0.9659258262890683122, 1.000000000000000000, 0.9659258262890683122, 1.000000000000000000, 0.9659258262890683122, 1.000000000000000000, 0.9659258262890683122, 1.000000000000000000, 0.9659258262890683122, 1.000000000000000000, 0.9659258262890683122, 1.000000000000000000, 0.9659258262890683122, 1.000000000000000000, 0.9659258262890683122, 1.000000000000000000, 0.9659258262890683122, 1.000000000000000000, 0.9659258262890683122, 1.000000000000000000, 0.9659258262890683122, 1.000000000000000000, 0.9659258262890683122, 1.000000000000000000, 0.9659258262890683122, 1.000000000000000000, 0.9659258262890683122, 1.000000000000000000, 0.9659258262890683122, 1.000000000000000000, 0.9659258262890683122, 1.000000000000000000, 0.9659258262890683122, 1.000000000000000000, 0.9659258262890683122, 1.000000000000000000, 0.9659258262890683122, 1.000000000000000000, 0.9659258262890683122, 1.000000000000000000, 0.9659258262890683122, 1.000000000000000000, 0.9659258262890683122, 1.000000000000000000, 0.9659258262890683122, 1.000000000000000000, 0.9659258262890683122, 1.000000000000000000, 0.9659258262890683122, 1.000000000000000000, 0.9659258262890683122, 1.000000000000000000, 0.9659258262890683122, 1.000000000000000000, 0.9659258262890683122, 1.000000000000000000, 0.9659258262890683122, 1.000000000000000000, 0.9659258262890683122, 1.000000000000000000, 0.9659258262890683122, 1.000000000000000000, 0.9659258262890683122, 1.000000000000000000, 0.9659258262890683122, 1.000000000000000000, 0.9659258262890683122, 1.000000000000000000, 0.9659258262890683122, 1.000000000000000000, 0.9659258262890683122, 1.000000000000000000, 0.9659258262890683122, 1.000000000000000000, 0.9659258262890683122, 1.000000000000000000, 0.9659258262890683122, 1.000000000000000000, 0.9659258262890683122, 1.000000000000000000, 0.9659258262890683122, 1.000000000000000000, 0.9659258262890683122, 1.000000000000000000, 0.9659258262890683122, 1.000000000000000000, 0.9659258262890683122, 1.000000000000000000, 0.9659258262890683122, 1.000000000000000000, 0.9659258262890683122, 1.000000000000000000, 0.9659258262890683122, 1.000000000000000000, 0.9659258262890683122, 1.000000000000000000, 0.9659258262890683122, 1.000000000000000000, 0.9659258262890683122, 1.000000000000000000, 0.9659258262890683122, 1.000000000000000000),
 ( 1.000000000000000000, 0.9659258262890683122, 1.000000000000000000, 0.9659258262890683122, 1.000000000000000000, 0.9659258262890683122, 1.000000000000000000, 0.9659258262890683122, 1.000000000000000000, 0.9659258262890683122, 1.000000000000000000, 0.9659258262890683122, 1.000000000000000000, 0.9659258262890683122, 1.000000000000000000, 0.9659258262890683122, 1.000000000000000000, 0.9659258262890683122, 1.000000000000000000, 0.9659258262890683122, 1.000000000000000000, 0.9659258262890683122, 1.000000000000000000, 0.9659258262890683122, 1.000000000000000000, 0.9659258262890683122, 1.000000000000000000, 0.9659258262890683122, 1.000000000000000000, 0.9659258262890683122, 1.000000000000000000, 0.9659258262890683122, 1.000000000000000000, 0.9659258262890683122, 1.000000000000000000, 0.9659258262890683122, 1.000000000000000000, 0.9659258262890683122, 1.000000000000000000, 0.9659258262890683122, 1.000000000000000000, 0.9659258262890683122, 1.000000000000000000, 0.9659258262890683122, 1.000000000000000000, 0.9659258262890683122, 1.000000000000000000, 0.9659258262890683122, 1.000000000000000000, 0.9659258262890683122, 1.000000000000000000, 0.9659258262890683122, 1.000000000000000000, 0.9659258262890683122, 1.000000000000000000, 0.9659258262890683122, 1.000000000000000000, 0.9659258262890683122, 1.000000000000000000, 0.9659258262890683122, 1.000000000000000000, 0.9659258262890683122, 1.000000000000000000, 0.9659258262890683122, 1.000000000000000000, 0.9659258262890683122, 1.000000000000000000, 0.9659258262890683122, 1.000000000000000000, 0.9659258262890683122, 1.000000000000000000, 0.9659258262890683122, 1.000000000000000000, 0.9659258262890683122, 1.000000000000000000, 0.9659258262890683122, 1.000000000000000000, 0.9659258262890683122, 1.000000000000000000, 0.9659258262890683122, 1.000000000000000000, 0.9659258262890683122, 1.000000000000000000, 0.9659258262890683122, 1.000000000000000000, 0.9659258262890683122, 1.000000000000000000, 0.9659258262890683122, 1.000000000000000000, 0.9659258262890683122, 1.000000000000000000, 0.9659258262890683122, 1.000000000000000000, 0.9659258262890683122, 1.000000000000000000, 0.9659258262890683122, 1.000000000000000000, 0.9659258262890683122, 1.000000000000000000, 0.9659258262890683122, 1.000000000000000000, 0.9659258262890683122, 1.000000000000000000, 0.9659258262890683122, 1.000000000000000000, 0.9659258262890683122, 1.000000000000000000, 0.9659258262890683122, 1.000000000000000000, 0.9659258262890683122, 1.000000000000000000, 0.9659258262890683122, 1.000000000000000000, 0.9659258262890683122, 1.000000000000000000, 0.9659258262890683122, 1.000000000000000000, 0.9659258262890683122, 1.000000000000000000, 0.9659258262890683122, 1.000000000000000000, 0.9659258262890683122, 1.000000000000000000, 0.9659258262890683122, 1.000000000000000000, 0.9659258262890683122, 1.000000000000000000, 0.9659258262890683122, 1.000000000000000000, 0.9659258262890683122, 1.000000000000000000, 0.9659258262890683122, 1.000000000000000000, 0.9659258262890683122, 1.000000000000000000, 0.9659258262890683122, 1.000000000000000000, 0.9659258262890683122, 1.000000000000000000, 0.9659258262890683122, 1.000000000000000000, 0.9659258262890683122, 1.000000000000000000, 0.9659258262890683122, 1.000000000000000000, 0.9659258262890683122, 1.000000000000000000, 0.9659258262890683122, 1.000000000000000000, 0.9659258262890683122, 1.000000000000000000, 0.9659258262890683122, 1.000000000000000000, 0.9659258262890683122, 1.000000000000000000, 0.9659258262890683122, 1.000000000000000000, 0.9659258262890683122, 1.000000000000000000, 0.9659258262890683122, 1.000000000000000000, 0.9659258262890683122, 1.000000000000000000, 0.9659258262890683122, 1.000000000000000000, 0.9659258262890683122, 1.000000000000000000, 0.9659258262890683122, 1.000000000000000000, 0.9659258262890683122, 1.000000000000000000, 0.9659258262890683122, 1.000000000000000000, 0.9659258262890683122, 1.000000000000000000, 0.9659258262890683122, 1.000000000000000000, 0.9659258262890683122, 1.000000000000000000, 0.9659258262890683122, 1.000000000000000000, 0.9659258262890683122, 1.000000000000000000, 0.9659258262890683122, 1.000000000000000000, 0.9659258262890683122, 1.000000000000000000, 0.9659258262890683122, 1.000000000000000000, 0.9659258262890683122, 1.000000000000000000, 0.9659258262890683122, 1.000000000000000000, 0.9659258262890683122, 1.000000000000000000, 0.9659258262890683122, 1.000000000000000000, 0.9659258262890683122, 1.000000000000000000, 0.9659258262890683122, 1.000000000000000000, 0.9659258262890683122, 1.000000000000000000, 0.9659258262890683122, 1.000000000000000000, 0.9659258262890683122, 1.000000000000000000, 0.9659258262890683122, 1.000000000000000000, 0.9659258262890683122, 1.000000000000000000, 0.9659258262890683122, 1.000000000000000000, 0.9659258262890683122, 1.000000000000000000, 0.9659258262890683122, 1.000000000000000000, 0.9659258262890683122, 1.000000000000000000, 0.9659258262890683122, 1.000000000000000000, 0.9659258262890683122, 1.000000000000000000, 0.9659258262890683122, 1.000000000000000000, 0.9659258262890683122, 1.000000000000000000, 0.9659258262890683122, 1.000000000000000000, 0.9659258262890683122, 1.000000000000000000, 0.9659258262890683122, 1.000000000000000000, 0.9659258262890683122, 1.000000000000000000, 0.9659258262890683122, 1.000000000000000000, 0.9659258262890683122, 1.000000000000000000, 0.9659258262890683122, 1.000000000000000000, 0.9659258262890683122, 1.000000000000000000, 0.9659258262890683122, 1.000000000000000000, 0.9659258262890683122, 1.000000000000000000, 0.9659258262890683122, 1.000000000000000000, 0.9659258262890683122, 1.000000000000000000, 0.9659258262890683122, 1.000000000000000000, 0.9659258262890683122, 1.000000000000000000, 0.9659258262890683122, 1.000000000000000000, 0.9659258262890683122, 1.000000000000000000, 0.9659258262890683122, 1.000000000000000000, 0.9659258262890683122, 1.000000000000000000, 0.9659258262890683122, 1.000000000000000000, 0.9659258262890683122, 1.000000000000000000, 0.9659258262890683122, 1.000000000000000000, 0.9659258262890683122, 1.000000000000000000, 0.9659258262890683122, 1.000000000000000000, 0.9659258262890683122, 1.000000000000000000, 0.9659258262890683122, 1.000000000000000000, 0.9659258262890683122, 1.000000000000000000, 0.9659258262890683122, 1.000000000000000000, 0.9659258262890683122, 1.000000000000000000, 0.9659258262890683122, 1.000000000000000000, 0.9659258262890683122, 1.000000000000000000, 0.9659258262890683122, 1.000000000000000000, 0.9659258262890683122, 1.000000000000000000, 0.9659258262890683122, 1.000000000000000000, 0.9659258262890683122, 1.000000000000000000, 0.9659258262890683122, 1.000000000000000000, 0.9659258262890683122, 1.000000000000000000, 0.9659258262890683122, 1.000000000000000000, 0.9659258262890683122, 1.000000000000000000, 0.9659258262890683122, 1.000000000000000000, 0.9659258262890683122, 1.000000000000000000, 0.9659258262890683122, 1.000000000000000000, 0.9659258262890683122, 1.000000000000000000, 0.9659258262890683122, 1.000000000000000000, 0.9659258262890683122, 1.000000000000000000, 0.9659258262890683122, 1.000000000000000000, 0.9659258262890683122, 1.000000000000000000, 0.9659258262890683122, 1.000000000000000000, 0.9659258262890683122, 1.000000000000000000, 0.9659258262890683122, 1.000000000000000000, 0.9659258262890683122, 1.000000000000000000, 0.9659258262890683122, 1.000000000000000000, 0.9659258262890683122, 1.000000000000000000, 0.9659258262890683122, 1.000000000000000000, 0.9659258262890683122, 1.000000000000000000, 0.9659258262890683122, 1.000000000000000000, 0.9659258262890683122, 1.000000000000000000, 0.9659258262890683122, 1.000000000000000000, 0.9659258262890683122, 1.000000000000000000, 0.9659258262890683122, 1.000000000000000000, 0.9659258262890683122, 1.000000000000000000, 0.9659258262890683122, 1.000000000000000000, 0.9659258262890683122, 1.000000000000000000, 0.9659258262890683122, 1.000000000000000000, 0.9659258262890683122, 1.000000000000000000, 0.9659258262890683122, 1.000000000000000000, 0.9659258262890683122, 1.000000000000000000, 0.9659258262890683122, 1.000000000000000000, 0.9659258262890683122, 1.000000000000000000, 0.9659258262890683122, 1.000000000000000000, 0.9659258262890683122, 1.000000000000000000, 0.9659258262890683122, 1.000000000000000000, 0.9659258262890683122, 1.000000000000000000, 0.9659258262890683122, 1.000000000000000000, 0.9659258262890683122, 1.000000000000000000, 0.9659258262890683122, 1.000000000000000000, 0.9659258262890683122, 1.000000000000000000, 0.9659258262890683122, 1.000000000000000000, 0.9659258262890683122, 1.000000000000000000, 0.9659258262890683122, 1.000000000000000000, 0.9659258262890683122, 1.000000000000000000, 0.9659258262890683122, 1.000000000000000000, 0.9659258262890683122, 1.000000000000000000, 0.9659258262890683122, 1.000000000000000000, 0.9659258262890683122, 1.000000000000000000, 0.9659258262890683122, 1.000000000000000000, 0.9659258262890683122, 1.000000000000000000, 0.9659258262890683122, 1.000000000000000000, 0.9659258262890683122, 1.000000000000000000, 0.9659258262890683122, 1.000000000000000000, 0.9659258262890683122, 1.000000000000000000, 0.9659258262890683122, 1.000000000000000000, 0.9659258262890683122, 1.000000000000000000, 0.9659258262890683122, 1.000000000000000000, 0.9659258262890683122, 1.000000000000000000, 0.9659258262890683122, 1.000000000000000000, 0.9659258262890683122, 1.000000000000000000, 0.9659258262890683122, 1.000000000000000000, 0.9659258262890683122, 1.000000000000000000, 0.9659258262890683122, 1.000000000000000000, 0.9659258262890683122, 1.000000000000000000, 0.9659258262890683122, 1.000000000000000000, 0.9659258262890683122, 1.000000000000000000, 0.9659258262890683122, 1.000000000000000000, 0.9659258262890683122, 1.000000000000000000, 0.9659258262890683122, 1.000000000000000000, 0.9659258262890683122, 1.000000000000000000, 0.9659258262890683122, 1.000000000000000000, 0.9659258262890683122, 1.000000000000000000, 0.9659258262890683122, 1.000000000000000000, 0.9659258262890683122, 1.000000000000000000, 0.9659258262890683122, 1.000000000000000000, 0.9659258262890683122, 1.000000000000000000, 0.9659258262890683122, 1.000000000000000000, 0.9659258262890683122, 1.000000000000000000, 0.9659258262890683122, 1.000000000000000000, 0.9659258262890683122, 1.000000000000000000, 0.9659258262890683122, 1.000000000000000000, 0.9659258262890683122, 1.000000000000000000, 0.9659258262890683122, 1.000000000000000000, 0.9659258262890683122, 1.000000000000000000, 0.9659258262890683122, 1.000000000000000000, 0.9659258262890683122, 1.000000000000000000, 0.9659258262890683122, 1.000000000000000000, 0.9659258262890683122, 1.000000000000000000, 0.9659258262890683122, 1.000000000000000000, 0.9659258262890683122, 1.000000000000000000, 0.9659258262890683122, 1.000000000000000000, 0.9659258262890683122, 1.000000000000000000, 0.9659258262890683122, 1.000000000000000000, 0.9659258262890683122, 1.000000000000000000, 0.9659258262890683122, 1.000000000000000000, 0.9659258262890683122, 1.000000000000000000, 0.9659258262890683122, 1.000000000000000000, 0.9659258262890683122, 1.000000000000000000, 0.9659258262890683122, 1.000000000000000000, 0.9659258262890683122, 1.000000000000000000, 0.9659258262890683122, 1.000000000000000000, 0.9659258262890683122, 1.000000000000000000, 0.9659258262890683122, 1.000000000000000000, 0.9659258262890683122, 1.000000000000000000, 0.9659258262890683122, 1.000000000000000000, 0.9659258262890683122, 1.000000000000000000) ) ) 
 REPRESENTATION_ITEM ( '' )  SURFACE ( )  );
#63408 = CARTESIAN_POINT ( 'NONE',  ( -0.2887139107611542133, -0.6046776061558809534, -0.2411417322834644161 ) ) ;
#63409 = CARTESIAN_POINT ( 'NONE',  ( -1.338582677165353729, -0.1870078740157479769, 0.4822834645669291653 ) ) ;
#63410 = CARTESIAN_POINT ( 'NONE',  ( 1.364829396325460076, 0.2306618581243848609, 0.2411417322834645549 ) ) ;
#63411 = CARTESIAN_POINT ( 'NONE',  ( 0.3458507752293908943, -0.3458507752293908943, -1.515748031496062742 ) ) ;
#63412 = CARTESIAN_POINT ( 'NONE',  ( -0.3460692066303958092, -0.1998031496062994683, -2.572178477690288734 ) ) ;
#63413 = CARTESIAN_POINT ( 'NONE',  ( -0.2034120734908131112, -0.5511811023622048555, -0.09757992244046775898 ) ) ;
#63414 = VERTEX_POINT ( 'NONE', #49719 ) ;
#63415 = VERTEX_POINT ( 'NONE', #62779 ) ;
#63416 = CARTESIAN_POINT ( 'NONE',  ( -0.8005249343832013809, -0.4281496062992124485, 0.4176697321401328655 ) ) ;
#63417 = CARTESIAN_POINT ( 'NONE',  ( -0.5971128608923877978, -0.6692913385826773087, -0.1292274648535924053 ) ) ;
#63419 = CARTESIAN_POINT ( 'NONE',  ( -0.5905511811023613777, -0.6692913385826771977, 8.415575281601705876E-17 ) ) ;
#63418 = CARTESIAN_POINT ( 'NONE',  ( -0.8464566929133852113, 0.07958543189024085140, 0.2665933059059887866 ) ) ;
#63420 = CARTESIAN_POINT ( 'NONE',  ( 0.3149606299212606708, -0.1870078740157480879, -0.4822834645669291653 ) ) ;
#63421 = CARTESIAN_POINT ( 'NONE',  ( -0.2887139107611542133, -0.6046776061558809534, -0.2411417322834644161 ) ) ;
#63422 = CARTESIAN_POINT ( 'NONE',  ( -1.410761154855641575, -0.3162353388693409650, -0.4822834645669289433 ) ) ;
#63423 = CARTESIAN_POINT ( 'NONE',  ( -0.8005249343832013809, -0.4281496062992124485, 0.4176697321401328655 ) ) ;
#63424 = CARTESIAN_POINT ( 'NONE',  ( 0.6496062992125991586, 0.1660481256975885056, 0.3530559997133364547 ) ) ;
#63425 = ADVANCED_FACE ( 'NONE', ( #31184 ), #26590, .T. ) ;
#63426 = EDGE_CURVE ( 'NONE', #33327, #55113, #5518, .T. ) ;
#63427 = CARTESIAN_POINT ( 'NONE',  ( -0.1958661417322836718, 0.3392501089628017219, -1.422572178477690574 ) ) ;
#63428 = CARTESIAN_POINT ( 'NONE',  ( -0.3346456692913377662, 0.07958543189024071263, -0.2665933059059888421 ) ) ;
#63429 = EDGE_LOOP ( 'NONE', ( #71318, #28855, #67176, #58690 ) ) ;
#63430 = CARTESIAN_POINT ( 'NONE',  ( -0.1058382717557503211, 0.3949938075777409408, -1.581364829396325389 ) ) ;
#63431 = ORIENTED_EDGE ( 'NONE', *, *, #34823, .T. ) ;
#63432 = CARTESIAN_POINT ( 'NONE',  ( -1.325459317585300889, -0.3690944881889765550, -0.3153832671262227771 ) ) ;
#63433 = CARTESIAN_POINT ( 'NONE',  ( -1.246719160104985846, -0.4281496062992127816, -0.4176697321401328100 ) ) ;
#63434 = CARTESIAN_POINT ( 'NONE',  ( -0.7677165354330699465, -0.5400638737290845981, -0.3530559997133363437 ) ) ;
#63435 = CARTESIAN_POINT ( 'NONE',  ( 0.3996062992125986035, 0.1070741851644054776, -0.2821522309711286258 ) ) ;
#63436 = CARTESIAN_POINT ( 'NONE',  ( -1.325459317585300889, -0.4281496062992127816, -0.4176697321401328100 ) ) ;
#63437 = CARTESIAN_POINT ( 'NONE',  ( -1.003937007874015297, -0.5400638737290845981, -0.3530559997133363437 ) ) ;
#63438 = CARTESIAN_POINT ( 'NONE',  ( -1.581364829396324945, -0.05778040916215560624, -0.4822834645669293319 ) ) ;
#63439 = CARTESIAN_POINT ( 'NONE',  ( -1.719160104986876103, 0.05413385826771666132, 0.4176697321401328100 ) ) ;
#63440 = CARTESIAN_POINT ( 'NONE',  ( 0.3674540682414705883, -0.5023911411419708095, 0.1820866141732285504 ) ) ;
#63441 = CARTESIAN_POINT ( 'NONE',  ( 1.392101432702376629, 0.000000000000000000, 0.9507481457704560768 ) ) ;
#63442 = CARTESIAN_POINT ( 'NONE',  ( 0.2952755905511810774, 3.179810529374183920E-17, 5.879133660591329580 ) ) ;
#63443 = CARTESIAN_POINT ( 'NONE',  ( 0.08530183727034192087, -0.2845877964562161244, -0.3641732283464567121 ) ) ;
#63444 = CARTESIAN_POINT ( 'NONE',  ( -0.4855643044619415427, 0.05413385826771626580, -0.4176697321401330321 ) ) ;
#63445 = CARTESIAN_POINT ( 'NONE',  ( 1.456692913385827515, 0.2952755905511811885, 0.000000000000000000 ) ) ;
#63446 = CARTESIAN_POINT ( 'NONE',  ( -0.3412073490813641308, 0.2306618581243847221, -0.2411417322834647770 ) ) ;
#63447 = ORIENTED_EDGE ( 'NONE', *, *, #70567, .T. ) ;
#63448 = CARTESIAN_POINT ( 'NONE',  ( 4.893765752498283924E-17, -0.3996062992125986035, -2.125984251968504157 ) ) ;
#63449 = CARTESIAN_POINT ( 'NONE',  ( -0.5314960629921171575, 2.716535433070866645, -2.543486866223390930 ) ) ;
#63450 = ORIENTED_EDGE ( 'NONE', *, *, #62163, .F. ) ;
#63451 = CARTESIAN_POINT ( 'NONE',  ( 0.1998031496062992463, 0.3460692066303959202, -1.638451443569553634 ) ) ;
#63453 = CIRCLE ( 'NONE', #67496, 3.937007874015748143 ) ;
#63452 = CARTESIAN_POINT ( 'NONE',  ( -0.7152230971128602510, -0.3162353388693405765, 0.4822834645669290543 ) ) ;
#63454 = CARTESIAN_POINT ( 'NONE',  ( 1.351706036745407458, -0.4281496062992127816, -0.4176697321401328100 ) ) ;
#63455 = CARTESIAN_POINT ( 'NONE',  ( -0.9580052493438311334, -0.3690944881889763329, 0.3153832671262228327 ) ) ;
#63456 = CARTESIAN_POINT ( 'NONE',  ( -1.377952755905511140, 0.2952755905511811885, 0.000000000000000000 ) ) ;
#63457 = CARTESIAN_POINT ( 'NONE',  ( -0.4724409448818895907, -0.1265901696524993070, -0.6758530183727035068 ) ) ;
#63458 = CARTESIAN_POINT ( 'NONE',  ( 4.821444091131311894E-16, 0.07874015748031502893, 3.937007874015748143 ) ) ;
#63459 = EDGE_CURVE ( 'NONE', #7122, #23435, #29786, .T. ) ;
#63460 = CARTESIAN_POINT ( 'NONE',  ( 4.797336870675656522E-17, -0.3917322834645670104, -0.07086614173228342195 ) ) ;
#63461 = CARTESIAN_POINT ( 'NONE',  ( 1.128608923884515169, -0.6046776061558809534, -0.2411417322834644161 ) ) ;
#63462 = CARTESIAN_POINT ( 'NONE',  ( -0.3917322834645671215, 0.1049643490035301469, -2.007217847769029007 ) ) ;
#63463 = CARTESIAN_POINT ( 'NONE',  ( 0.05905511811023709395, -0.5400638737290844871, 0.3530559997133364547 ) ) ;
#63464 = CARTESIAN_POINT ( 'NONE',  ( -1.194225721784776262, -0.3690944881889763329, 0.3153832671262228327 ) ) ;
#63465 = CARTESIAN_POINT ( 'NONE',  ( -0.2034120734908131112, -0.6692913385826773087, -0.1292274648535924053 ) ) ;
#63466 = CARTESIAN_POINT ( 'NONE',  ( -0.4724409448818899238, 0.1265901696524986686, -2.629265091863517423 ) ) ;
#63467 = ADVANCED_FACE ( 'NONE', ( #13095 ), #33331, .F. ) ;
#63468 = CARTESIAN_POINT ( 'NONE',  ( -0.7480314960629914633, 0.2952755905511811885, 0.000000000000000000 ) ) ;
#63469 = CARTESIAN_POINT ( 'NONE',  ( 0.3949938075777409963, 2.418639510665530743E-17, -2.242125984251968518 ) ) ;
#63470 = CARTESIAN_POINT ( 'NONE',  ( 0.6889763779527563470, 0.07958543189024071263, -0.2665933059059888421 ) ) ;
#63471 = CARTESIAN_POINT ( 'NONE',  ( -0.2165354330708654795, -0.4536011799217368745, -0.2665933059059886201 ) ) ;
#63472 = CARTESIAN_POINT ( 'NONE',  ( 0.8070866141732289112, -0.4536011799217368745, -0.2665933059059886201 ) ) ;
#63473 = CARTESIAN_POINT ( 'NONE',  ( -1.607611548556429737, -0.6692913385826771977, 0.1292274648535927661 ) ) ;
#63474 = CARTESIAN_POINT ( 'NONE',  ( 1.371391076115485719, -0.6692913385826773087, -0.1292274648535924053 ) ) ;
#63475 = CARTESIAN_POINT ( 'NONE',  ( 0.4921259842519691285, -0.4536011799217368745, -0.2665933059059886201 ) ) ;
#63476 = CARTESIAN_POINT ( 'NONE',  ( -0.9973753280839886548, 0.2306618581243848609, 0.2411417322834645549 ) ) ;
#63477 = CARTESIAN_POINT ( 'NONE',  ( 1.266404199475066328, -0.05778040916215522460, 0.4822834645669289988 ) ) ;
#63478 = B_SPLINE_CURVE_WITH_KNOTS ( 'NONE', 3,
 ( #39764, #33458, #59120, #1477 ),
 .UNSPECIFIED., .F., .F.,
 ( 4, 4 ),
 ( 0.1211256351025462169, 0.1225682571257921682 ),
 .UNSPECIFIED. ) ;
#63479 = CARTESIAN_POINT ( 'NONE',  ( -3.924389226575468737, 2.559055118110236560, -0.3149606299212599492 ) ) ;
#63480 = CARTESIAN_POINT ( 'NONE',  ( -0.1049868766404193215, -0.5023911411419708095, 0.1820866141732285504 ) ) ;
#63481 = CARTESIAN_POINT ( 'NONE',  ( 0.1674892343164159914, -2.191421614605370878E-15, 0.4445507791589071167 ) ) ;
#63482 = CARTESIAN_POINT ( 'NONE',  ( 0.3280839895013130669, -0.4281496062992127816, -0.4176697321401328100 ) ) ;
#63483 = FACE_OUTER_BOUND ( 'NONE', #54743, .T. ) ;
#63484 = CARTESIAN_POINT ( 'NONE',  ( 1.482939632545932307, -0.004921259842519870586, -0.3153832671262229437 ) ) ;
#63485 = CARTESIAN_POINT ( 'NONE',  ( -1.463254593175852492, -0.6692913385826773087, -0.1292274648535924053 ) ) ;
#63486 = CARTESIAN_POINT ( 'NONE',  ( -0.4461942257217840213, -0.5023911411419708095, -0.1820866141732282451 ) ) ;
#63487 = DIRECTION ( 'NONE',  ( 0.000000000000000000, 0.000000000000000000, -1.000000000000000000 ) ) ;
#63488 = CARTESIAN_POINT ( 'NONE',  ( -1.003937007874015297, -0.5400638737290845981, -0.3530559997133363437 ) ) ;
#63489 = CARTESIAN_POINT ( 'NONE',  ( -0.7152230971128602510, -0.3162353388693405765, 0.4822834645669290543 ) ) ;
#63490 = CARTESIAN_POINT ( 'NONE',  ( 0.3460692066303959202, -0.1998031496062991630, -0.6541994750656167090 ) ) ;
#63491 = CARTESIAN_POINT ( 'NONE',  ( 0.3392501089628018329, 0.1958661417322835607, -2.263123359580052618 ) ) ;
#63492 = CARTESIAN_POINT ( 'NONE',  ( 0.5314960629921264834, 0.07958543189024071263, -0.2665933059059888421 ) ) ;
#63493 = CARTESIAN_POINT ( 'NONE',  ( -0.5183727034120726440, 0.2952755905511811885, 0.1292274648535926551 ) ) ;
#63494 = CARTESIAN_POINT ( 'NONE',  ( -0.6364829396325453192, -0.05778040916215560624, -0.4822834645669293319 ) ) ;
#63495 = CARTESIAN_POINT ( 'NONE',  ( -0.9251968503937002541, -0.4536011799217368745, -0.2665933059059886201 ) ) ;
#63496 = CARTESIAN_POINT ( 'NONE',  ( 0.6199123404867349363, 8.471767977567108961E-16, -0.4445507791589058955 ) ) ;
#63497 = CARTESIAN_POINT ( 'NONE',  ( -0.1640419947506553400, -0.05778040916215560624, -0.4822834645669293319 ) ) ;
#63498 = B_SPLINE_CURVE_WITH_KNOTS ( 'NONE', 3,
 ( #9816, #54417, #41389, #16977, #54838, #80128, #74216 ),
 .UNSPECIFIED., .F., .F.,
 ( 4, 3, 4 ),
 ( 1.735570302229820823E-18, 0.001246230184515536828, 0.002492489877932635954 ),
 .UNSPECIFIED. ) ;
#63499 = PLANE ( 'NONE',  #65666 ) ;
#63500 = CARTESIAN_POINT ( 'NONE',  ( 1.089238845144357537, -0.4281496062992124485, 0.4176697321401328655 ) ) ;
#63501 = CARTESIAN_POINT ( 'NONE',  ( 0.4724409448818898682, 2.892866454678787531E-17, -1.062992125984252079 ) ) ;
#63502 = CIRCLE ( 'NONE', #35343, 3.937007874015748143 ) ;
#63503 = CARTESIAN_POINT ( 'NONE',  ( -0.1958661417322833942, -0.3392501089628018884, -1.952119053314647523 ) ) ;
#63504 = EDGE_LOOP ( 'NONE', ( #64467, #20387 ) ) ;
#63505 = CARTESIAN_POINT ( 'NONE',  ( -3.886287458032462006, 2.755905511811024056, 0.6299212598425196763 ) ) ;
#63506 = CARTESIAN_POINT ( 'NONE',  ( -1.358267716535432434, 0.1660481256975883668, -0.3530559997133364547 ) ) ;
#63507 = VECTOR ( 'NONE', #35186, 39.37007874015748143 ) ;
#63508 = CARTESIAN_POINT ( 'NONE',  ( -0.6889763779527552368, -0.5400638737290845981, -0.3530559997133363437 ) ) ;
#63509 = EDGE_CURVE ( 'NONE', #5361, #50786, #32018, .T. ) ;
#63510 = CARTESIAN_POINT ( 'NONE',  ( 1.469816272965879911, 0.2306618581243847221, -0.2411417322834647770 ) ) ;
#63511 = CARTESIAN_POINT ( 'NONE',  ( -0.1049643490035302024, -0.3917322834645671215, -2.046587926509185973 ) ) ;
#63512 = CARTESIAN_POINT ( 'NONE',  ( -0.05722014593895823065, 0.3876764156950353035, -1.220472440944881720 ) ) ;
#63513 = CARTESIAN_POINT ( 'NONE',  ( 1.017060367454068803, -0.3162353388693405765, 0.4822834645669290543 ) ) ;
#63514 = CARTESIAN_POINT ( 'NONE',  ( 0.08530183727034192087, -0.05778040916215522460, 0.4822834645669289988 ) ) ;
#63515 = CARTESIAN_POINT ( 'NONE',  ( 0.4744094488189113945, 1.537401574803149984, -3.937007874015760578 ) ) ;
#63516 = CARTESIAN_POINT ( 'NONE',  ( -9.787531504996566615E-17, 0.3996062992125985480, -2.753937007874015741 ) ) ;
#63517 = CARTESIAN_POINT ( 'NONE',  ( 1.305774278215223960, 0.1771653543307087075, -0.09757992244046823083 ) ) ;
#63518 = CARTESIAN_POINT ( 'NONE',  ( -0.3996062992125987146, 0.1070741851644051862, -0.8202099737532806412 ) ) ;
#63519 = EDGE_LOOP ( 'NONE', ( #31941, #62005, #49757, #68445, #68110 ) ) ;
#63520 = CARTESIAN_POINT ( 'NONE',  ( -0.3917322834645670104, -7.196005306013484475E-17, -2.551181102362204633 ) ) ;
#63521 = ORIENTED_EDGE ( 'NONE', *, *, #25905, .T. ) ;
#63522 = CARTESIAN_POINT ( 'NONE',  ( 0.5971128608923890191, -0.6692913385826771977, 0.1292274648535927661 ) ) ;
#63523 = CARTESIAN_POINT ( 'NONE',  ( -0.7349081364829390672, 0.2306618581243847221, -0.2411417322834647770 ) ) ;
#63524 = CARTESIAN_POINT ( 'NONE',  ( 1.568241469816273437, -0.3162353388693405765, 0.4822834645669290543 ) ) ;
#63525 = CARTESIAN_POINT ( 'NONE',  ( 0.7545931758530189937, 0.2952755905511810774, -0.1292274648535930714 ) ) ;
#63526 = CARTESIAN_POINT ( 'NONE',  ( -1.509186351706035767, -0.3690944881889763329, 0.3153832671262228327 ) ) ;
#63527 = CARTESIAN_POINT ( 'NONE',  ( 1.614173228346457378, 0.2952755905511811885, 0.000000000000000000 ) ) ;
#63528 = CARTESIAN_POINT ( 'NONE',  ( -0.1968503937007867743, 0.2952755905511811885, 0.000000000000000000 ) ) ;
#63529 = CARTESIAN_POINT ( 'NONE',  ( -1.463254593175852492, 0.2952755905511811885, 0.1292274648535926551 ) ) ;
#63530 = CARTESIAN_POINT ( 'NONE',  ( 1.587926509186352142, 0.05413385826771666132, 0.4176697321401328100 ) ) ;
#63531 = CARTESIAN_POINT ( 'NONE',  ( 0.4044922606986875446, 1.289103360985770941, -2.676033440910250860 ) ) ;
#63532 = CARTESIAN_POINT ( 'NONE',  ( -0.3917322834645671215, 0.1049643490035301469, -0.1824146981627296216 ) ) ;
#63533 = CARTESIAN_POINT ( 'NONE',  ( 0.7677165354330716118, 0.07958543189024071263, -0.2665933059059888421 ) ) ;
#63534 = ORIENTED_EDGE ( 'NONE', *, *, #46886, .T. ) ;
#63535 = CARTESIAN_POINT ( 'NONE',  ( -0.3949938075777409963, -7.255918531996591613E-17, -0.3543307086614174151 ) ) ;
#63536 = ORIENTED_EDGE ( 'NONE', *, *, #24986, .T. ) ;
#63537 = CARTESIAN_POINT ( 'NONE',  ( -0.2230971128608915943, -0.3690944881889765550, -0.3153832671262227771 ) ) ;
#63538 = CARTESIAN_POINT ( 'NONE',  ( 2.565212732165838450, 1.469708627452554595, -0.4698506773045480478 ) ) ;
#63539 = CARTESIAN_POINT ( 'NONE',  ( 0.3412073490813655186, 0.2306618581243848609, 0.2411417322834645549 ) ) ;
#63540 = CARTESIAN_POINT ( 'NONE',  ( 0.4199475065616803948, -0.6046776061558809534, -0.2411417322834644161 ) ) ;
#63541 = CARTESIAN_POINT ( 'NONE',  ( -0.6364829396325453192, -0.3162353388693405765, 0.4822834645669290543 ) ) ;
#63542 = CARTESIAN_POINT ( 'NONE',  ( 0.1049643490035304799, -0.3917322834645670104, -1.499363147802836860 ) ) ;
#63543 = CARTESIAN_POINT ( 'NONE',  ( -1.049868766404198794, -0.6046776061558807314, 0.2411417322834647770 ) ) ;
#63544 = CARTESIAN_POINT ( 'NONE',  ( -0.2867679344610365999, 0.2867679344610364889, -2.781496062992125040 ) ) ;
#63545 = CARTESIAN_POINT ( 'NONE',  ( 1.515748031496063186, -0.4536011799217368745, -0.2665933059059886201 ) ) ;
#63546 = CARTESIAN_POINT ( 'NONE',  ( 0.7152230971128616943, -0.05778040916215522460, 0.4822834645669289988 ) ) ;
#63547 = CARTESIAN_POINT ( 'NONE',  ( 1.161417322834646493, -0.5400638737290844871, 0.3530559997133364547 ) ) ;
#63548 = CARTESIAN_POINT ( 'NONE',  ( 0.2925321140481932369, -0.2925321140481932369, -0.7283464566929134243 ) ) ;
#63549 = CARTESIAN_POINT ( 'NONE',  ( -1.312335958005248715, -0.6046776061558809534, -0.2411417322834644161 ) ) ;
#63550 = CARTESIAN_POINT ( 'NONE',  ( 0.3460692066303959202, -0.1998031496062991630, -0.4967191601049869010 ) ) ;
#63551 = CARTESIAN_POINT ( 'NONE',  ( -0.1070741851644051862, -0.3996062992125986590, 0.008530183727034094596 ) ) ;
#63552 = CARTESIAN_POINT ( 'NONE',  ( -0.3018372703412066094, 0.05413385826771666132, 0.4176697321401328100 ) ) ;
#63553 = CARTESIAN_POINT ( 'NONE',  ( -0.2925321140481930704, -0.2925321140481933480, -2.893700787401574992 ) ) ;
#63554 = EDGE_CURVE ( 'NONE', #21629, #9606, #68297, .T. ) ;
#63555 = CARTESIAN_POINT ( 'NONE',  ( -0.3392501089628017219, -0.1958661417322836718, -1.711942257217847763 ) ) ;
#63556 = CARTESIAN_POINT ( 'NONE',  ( 1.095800524934383846, -0.3162353388693405765, 0.4822834645669290543 ) ) ;
#63557 = CARTESIAN_POINT ( 'NONE',  ( 1.259842519685040019, -0.1870078740157480879, -0.4822834645669291653 ) ) ;
#63558 = CARTESIAN_POINT ( 'NONE',  ( 0.07217847769028949700, -0.2845877964562159024, 0.3641732283464567677 ) ) ;
#63559 = CARTESIAN_POINT ( 'NONE',  ( 0.7152230971128614723, -0.3162353388693409650, -0.4822834645669289433 ) ) ;
#63560 = CARTESIAN_POINT ( 'NONE',  ( -0.3458507752293906723, -0.3458507752293910609, -1.710629921259842812 ) ) ;
#63561 = CARTESIAN_POINT ( 'NONE',  ( 0.3346456692913393205, -0.4536011799217368745, -0.2665933059059886201 ) ) ;
#63562 = CARTESIAN_POINT ( 'NONE',  ( 0.2624671916010504757, -0.6046776061558809534, -0.2411417322834644161 ) ) ;
#63563 = CONICAL_SURFACE ( 'NONE', #60923, 1.181102362204724310, 0.7853981633974621568 ) ;
#63564 = CARTESIAN_POINT ( 'NONE',  ( 0.2891555358219910499, 0.2891555358219910499, -0.8444881889763782290 ) ) ;
#63565 = CARTESIAN_POINT ( 'NONE',  ( -0.8858267716535425107, 0.1660481256975883668, -0.3530559997133364547 ) ) ;
#63566 = CARTESIAN_POINT ( 'NONE',  ( 1.036745406824147508, -0.3690944881889765550, -0.3153832671262227771 ) ) ;
#63567 = DIRECTION ( 'NONE',  ( 1.000000000000000000, 0.000000000000000000, 0.000000000000000000 ) ) ;
#63568 = CARTESIAN_POINT ( 'NONE',  ( -0.4265091863517051496, 0.2952755905511810774, -0.1292274648535930714 ) ) ;
#63569 = CARTESIAN_POINT ( 'NONE',  ( 0.1049868766404206816, 0.1283753931104748280, 0.1820866141732283561 ) ) ;
#63570 = CARTESIAN_POINT ( 'NONE',  ( -2.558801921130022805, 1.494646310179101656, -0.4725519687354814979 ) ) ;
#63571 = CARTESIAN_POINT ( 'NONE',  ( -0.3083989501312330295, -0.05778040916215522460, 0.4822834645669289988 ) ) ;
#63572 = CARTESIAN_POINT ( 'NONE',  ( 0.2624671916010504757, -0.5023911411419708095, -0.1820866141732282451 ) ) ;
#63573 = CARTESIAN_POINT ( 'NONE',  ( 0.3460692066303959202, -0.1998031496062991630, -1.914041994750656395 ) ) ;
#63574 = CARTESIAN_POINT ( 'NONE',  ( 0.2296587926509192634, -0.3162353388693405765, 0.4822834645669290543 ) ) ;
#63575 = CARTESIAN_POINT ( 'NONE',  ( 1.115485564304462551, -0.3690944881889765550, -0.3153832671262227771 ) ) ;
#63576 = CARTESIAN_POINT ( 'NONE',  ( 0.3817677560323445296, -4.069555009745408348E-17, -0.3627989612356148363 ) ) ;
#63577 = CARTESIAN_POINT ( 'NONE',  ( -0.3083989501312330295, -0.08942795157527998196, 0.3641732283464567121 ) ) ;
#63578 = ADVANCED_FACE ( 'NONE', ( #50533, #76237 ), #19390, .T. ) ;
#63579 = CARTESIAN_POINT ( 'NONE',  ( -0.8595800524934373854, -0.2845877964562161244, -0.3641732283464567121 ) ) ;
#63580 = CARTESIAN_POINT ( 'NONE',  ( -0.1312335958005241554, -0.6046776061558809534, -0.2411417322834644161 ) ) ;
#63581 = CARTESIAN_POINT ( 'NONE',  ( -0.1049868766404193215, 0.2306618581243847221, -0.2411417322834647770 ) ) ;
#63582 = CARTESIAN_POINT ( 'NONE',  ( 1.023622047244095334, -0.1870078740157479769, 0.3641732283464567677 ) ) ;
#63583 = CARTESIAN_POINT ( 'NONE',  ( 0.4712520375767828007, 1.474486464701640021, -1.018310922256620676 ) ) ;
#63584 = CARTESIAN_POINT ( 'NONE',  ( 1.515748031496063186, -0.4536011799217368745, -0.2665933059059886201 ) ) ;
#63585 = EDGE_CURVE ( 'NONE', #29291, #74748, #15813, .T. ) ;
#63586 = CARTESIAN_POINT ( 'NONE',  ( 0.9580052493438327987, -0.4281496062992127816, -0.4176697321401328100 ) ) ;
#63587 = DIRECTION ( 'NONE',  ( -3.491481338843133355E-15, -0.000000000000000000, 1.000000000000000000 ) ) ;
#63588 = CARTESIAN_POINT ( 'NONE',  ( -0.3280839895013117347, -0.4281496062992124485, 0.4176697321401328655 ) ) ;
#63589 = CARTESIAN_POINT ( 'NONE',  ( -0.1049643490035302024, -0.3917322834645671215, -0.7867454068241470644 ) ) ;
#63590 = CARTESIAN_POINT ( 'NONE',  ( 0.8727034120734913358, -0.05778040916215522460, 0.4822834645669289988 ) ) ;
#63591 = CARTESIAN_POINT ( 'NONE',  ( 0.5380577427821529035, -0.4281496062992124485, 0.4176697321401328655 ) ) ;
#63592 = CARTESIAN_POINT ( 'NONE',  ( 2.795275590551181466, 1.299212598425198095, -1.617488608965169241E-16 ) ) ;
#63593 = CARTESIAN_POINT ( 'NONE',  ( 0.2230971128608932319, -0.3690944881889763329, 0.3153832671262228327 ) ) ;
#63594 = CARTESIAN_POINT ( 'NONE',  ( 1.181102362204725198, -0.1870078740157479769, 0.4822834645669291653 ) ) ;
#63595 = CARTESIAN_POINT ( 'NONE',  ( -0.1902887139107604098, -0.5511811023622046335, 0.09757992244046803654 ) ) ;
#63596 = CARTESIAN_POINT ( 'NONE',  ( -0.2362204724409440182, -0.1870078740157479769, 0.4822834645669291653 ) ) ;
#63597 = DIRECTION ( 'NONE',  ( -0.000000000000000000, -1.000000000000000000, -0.000000000000000000 ) ) ;
#63598 = CARTESIAN_POINT ( 'NONE',  ( 0.3477690288713918276, 0.2952755905511811885, 0.1292274648535926551 ) ) ;
#63599 = CARTESIAN_POINT ( 'NONE',  ( -0.9317585301837263412, -0.4281496062992127816, -0.4176697321401328100 ) ) ;
#63600 = VECTOR ( 'NONE', #77048, 39.37007874015748143 ) ;
#63601 = CARTESIAN_POINT ( 'NONE',  ( -0.7020997375328076329, -0.2845877964562161244, -0.3641732283464567121 ) ) ;
#63602 = CARTESIAN_POINT ( 'NONE',  ( 0.5839895013123367340, -0.6692913385826773087, -0.1292274648535924053 ) ) ;
#63603 = CARTESIAN_POINT ( 'NONE',  ( -1.187664041994750175, -0.05778040916215560624, -0.4822834645669293319 ) ) ;
#63604 = CARTESIAN_POINT ( 'NONE',  ( -0.5446194225721777693, -0.05778040916215522460, 0.4822834645669289988 ) ) ;
#63605 = DIRECTION ( 'NONE',  ( -0.8660254037844433705, 0.000000000000000000, 0.4999999999999920064 ) ) ;
#63607 = CARTESIAN_POINT ( 'NONE',  ( 1.377952755905512472, -0.6692913385826771977, 8.415575281601705876E-17 ) ) ;
#63606 = CARTESIAN_POINT ( 'NONE',  ( -0.6575345472713096662, 1.929133858267489954, 0.5309055118110236338 ) ) ;
#63608 = CARTESIAN_POINT ( 'NONE',  ( 1.423884514435696413, -0.3162353388693409650, -0.4822834645669289433 ) ) ;
#63609 = CARTESIAN_POINT ( 'NONE',  ( -0.1049643490035307020, 0.3917322834645669549, -2.045931758530183497 ) ) ;
#63610 = CARTESIAN_POINT ( 'NONE',  ( -1.561679790026246017, -0.4281496062992127816, -0.4176697321401328100 ) ) ;
#63611 = CARTESIAN_POINT ( 'NONE',  ( -0.8398950131233589023, -0.6046776061558809534, -0.2411417322834644161 ) ) ;
#63612 = CARTESIAN_POINT ( 'NONE',  ( 0.2362204724409451007, -0.4091458600556402980, -0.2493438320209973857 ) ) ;
#63613 = CARTESIAN_POINT ( 'NONE',  ( 0.2891555358219910499, -0.2891555358219909944, -2.775590551181102317 ) ) ;
#63614 = EDGE_LOOP ( 'NONE', ( #197, #78245, #37544, #8860, #35090, #42824, #74122 ) ) ;
#63615 = CARTESIAN_POINT ( 'NONE',  ( -0.1771653543307080136, 0.07958543189024071263, -0.2665933059059888421 ) ) ;
#63616 = CARTESIAN_POINT ( 'NONE',  ( 0.1958661417322834775, 0.3392501089628018884, -1.553805774278215202 ) ) ;
#63617 = CARTESIAN_POINT ( 'NONE',  ( 0.7611548556430451917, -0.6046776061558807314, 0.2411417322834647770 ) ) ;
#63618 = CARTESIAN_POINT ( 'NONE',  ( -0.4724409448818898682, -8.678599364036362592E-17, -2.874015748031495843 ) ) ;
#63619 = CARTESIAN_POINT ( 'NONE',  ( -1.559171609364246924, 1.128537896298103416, 0.2406134192599649890 ) ) ;
#63620 = CARTESIAN_POINT ( 'NONE',  ( -0.6496062992125976043, 0.07958543189024071263, -0.2665933059059888421 ) ) ;
#63621 = CARTESIAN_POINT ( 'NONE',  ( -0.2549859370038549677, -0.1502491711592393864, 0.1564451348283543985 ) ) ;
#63622 = CARTESIAN_POINT ( 'NONE',  ( 1.384514435695538559, 0.2952755905511810774, -0.1292274648535930714 ) ) ;
#63623 = CARTESIAN_POINT ( 'NONE',  ( 1.010498687664042716, -0.004921259842519870586, -0.3153832671262229437 ) ) ;
#63624 = CARTESIAN_POINT ( 'NONE',  ( 0.1246719160104994284, 0.2952755905511810774, -0.1292274648535930714 ) ) ;
#63625 = CARTESIAN_POINT ( 'NONE',  ( -0.2867679344610364334, -0.2867679344610368219, -0.9264898705698668691 ) ) ;
#63626 = CARTESIAN_POINT ( 'NONE',  ( -0.2493438320209966919, -0.4281496062992124485, 0.4176697321401328655 ) ) ;
#63627 = CARTESIAN_POINT ( 'NONE',  ( -1.141732283464566011, -0.5511811023622047445, 6.969142054262312111E-17 ) ) ;
#63628 = CARTESIAN_POINT ( 'NONE',  ( -0.4002624671916004129, -0.05778040916215560624, -0.4822834645669293319 ) ) ;
#63629 = CARTESIAN_POINT ( 'NONE',  ( 1.587926509186352586, -0.4281496062992127816, -0.4176697321401328100 ) ) ;
#63630 = CYLINDRICAL_SURFACE ( 'NONE', #12675, 0.2165354330708660624 ) ;
#63631 = ORIENTED_EDGE ( 'NONE', *, *, #62070, .T. ) ;
#63632 = CARTESIAN_POINT ( 'NONE',  ( -9.594673741351313045E-17, 0.3917322834645670659, -2.043982570375014962 ) ) ;
#63633 = CARTESIAN_POINT ( 'NONE',  ( 0.2755905511811031494, 0.2952755905511811885, 0.000000000000000000 ) ) ;
#63634 = ORIENTED_EDGE ( 'NONE', *, *, #18368, .T. ) ;
#63635 = CARTESIAN_POINT ( 'NONE',  ( -0.9776902887139098386, -0.6692913385826771977, 0.1292274648535927661 ) ) ;
#63636 = CARTESIAN_POINT ( 'NONE',  ( -1.338582677165353729, -0.1870078740157479769, 0.4822834645669291653 ) ) ;
#63637 = CARTESIAN_POINT ( 'NONE',  ( 0.8464566929133865436, 0.1660481256975883668, -0.3530559997133364547 ) ) ;
#63638 = CARTESIAN_POINT ( 'NONE',  ( -0.05249343832020911260, 0.2306618581243848609, 0.2411417322834645549 ) ) ;
#63639 = CARTESIAN_POINT ( 'NONE',  ( 0.1958661417322836440, -0.3392501089628017219, -1.278871391076115582 ) ) ;
#63640 = CARTESIAN_POINT ( 'NONE',  ( -0.7808398950131225646, -0.05778040916215522460, 0.4822834645669289988 ) ) ;
#63641 = CARTESIAN_POINT ( 'NONE',  ( -0.3083989501312330295, -0.3162353388693409650, -0.4822834645669289433 ) ) ;
#63642 = CARTESIAN_POINT ( 'NONE',  ( -0.9120734908136475250, -0.6692913385826773087, -0.1292274648535924053 ) ) ;
#63643 = CARTESIAN_POINT ( 'NONE',  ( 0.006561679790026889343, -0.2845877964562161244, -0.3641732283464567121 ) ) ;
#63644 = CARTESIAN_POINT ( 'NONE',  ( -0.002049465651541999486, 0.3981765293560903807, -3.148631409696656626E-18 ) ) ;
#63645 = CARTESIAN_POINT ( 'NONE',  ( -0.08530183727034056085, -0.05778040916215560624, -0.4822834645669293319 ) ) ;
#63646 = CARTESIAN_POINT ( 'NONE',  ( 0.3307086614173228023, -0.3647102339900947787, 0.000000000000000000 ) ) ;
#63647 = CARTESIAN_POINT ( 'NONE',  ( 1.338582677165355062, -0.1870078740157480879, -0.4822834645669291653 ) ) ;
#63648 = CARTESIAN_POINT ( 'NONE',  ( 0.3917322834645670104, 2.398668435337828261E-17, -2.787401574803149096 ) ) ;
#63649 = ORIENTED_EDGE ( 'NONE', *, *, #63898, .T. ) ;
#63650 = EDGE_LOOP ( 'NONE', ( #37310, #62279, #46557, #61270 ) ) ;
#63651 = CARTESIAN_POINT ( 'NONE',  ( 0.1706036745406830368, -0.4281496062992127816, -0.4176697321401328100 ) ) ;
#63652 = CARTESIAN_POINT ( 'NONE',  ( 0.07874015748031558404, -0.1870078740157480601, -0.3641732283464567677 ) ) ;
#63654 = CARTESIAN_POINT ( 'NONE',  ( 1.603475055217291612, 0.5037964761735346242, -0.04573490813648244807 ) ) ;
#63653 = CARTESIAN_POINT ( 'NONE',  ( 1.489501312335958172, -0.2845877964562159024, 0.3641732283464567677 ) ) ;
#63655 = CARTESIAN_POINT ( 'NONE',  ( -0.3392501089628017219, -0.1958661417322836718, -1.239501312335958172 ) ) ;
#63656 = CARTESIAN_POINT ( 'NONE',  ( 0.4724409448818897572, -0.1265901696524988906, -0.1883202099737532054 ) ) ;
#63657 = CARTESIAN_POINT ( 'NONE',  ( 1.640419947506562393, -0.3690944881889763329, 0.3153832671262228327 ) ) ;
#63658 = CARTESIAN_POINT ( 'NONE',  ( -1.614173228346455824, 0.2952755905511811885, 0.000000000000000000 ) ) ;
#63659 = CARTESIAN_POINT ( 'NONE',  ( -0.3949938075777411073, 0.1058382717557497660, 0.2053805774278214813 ) ) ;
#63660 = CARTESIAN_POINT ( 'NONE',  ( 0.6364829396325465405, -0.05778040916215522460, 0.4822834645669289988 ) ) ;
#63661 = CARTESIAN_POINT ( 'NONE',  ( -1.207349081364828436, -0.6046776061558807314, 0.2411417322834647770 ) ) ;
#63662 = CIRCLE ( 'NONE', #59644, 2.165354330708661568 ) ;
#63663 = CARTESIAN_POINT ( 'NONE',  ( -1.253280839895012377, -0.05778040916215522460, 0.4822834645669289988 ) ) ;
#63664 = CARTESIAN_POINT ( 'NONE',  ( 0.3215223097112867578, -0.05778040916215522460, 0.4822834645669289988 ) ) ;
#63665 = CARTESIAN_POINT ( 'NONE',  ( 1.141732283464567566, 0.2952755905511811885, 0.000000000000000000 ) ) ;
#63666 = CARTESIAN_POINT ( 'NONE',  ( 1.515748031496063408, 0.07958543189024085140, 0.2665933059059887866 ) ) ;
#63667 = CARTESIAN_POINT ( 'NONE',  ( 0.9645669291338591078, -0.4536011799217368745, -0.2665933059059886201 ) ) ;
#63668 = CARTESIAN_POINT ( 'NONE',  ( -0.7349081364829387342, -0.6046776061558807314, 0.2411417322834647770 ) ) ;
#63669 = CARTESIAN_POINT ( 'NONE',  ( -0.3460692066303957537, -0.1998031496062994405, -0.4442257217847768724 ) ) ;
#63670 = CARTESIAN_POINT ( 'NONE',  ( 1.692913385826772421, 0.2952755905511811885, 0.000000000000000000 ) ) ;
#63671 = CARTESIAN_POINT ( 'NONE',  ( 0.3392501089628018329, 0.1958661417322835607, -0.4383202099737532609 ) ) ;
#63673 = CARTESIAN_POINT ( 'NONE',  ( 0.000000000000000000, 1.724409448818897461, 0.000000000000000000 ) ) ;
#63672 = CARTESIAN_POINT ( 'NONE',  ( 0.8923884514435703741, 0.2306618581243848609, 0.2411417322834645549 ) ) ;
#63674 = CARTESIAN_POINT ( 'NONE',  ( -1.443569553805773564, -0.5023911411419708095, 0.1820866141732285504 ) ) ;
#63675 = CARTESIAN_POINT ( 'NONE',  ( 0.04593175853018440641, -0.6692913385826771977, 0.1292274648535927661 ) ) ;
#63676 = CARTESIAN_POINT ( 'NONE',  ( 0.9645669291338588858, 0.07958543189024085140, 0.2665933059059887866 ) ) ;
#63677 = EDGE_CURVE ( 'NONE', #4124, #9295, #54817, .T. ) ;
#63678 = CIRCLE ( 'NONE', #81195, 3.228346456692913424 ) ;
#63679 = LINE ( 'NONE', #62861, #78550 ) ;
#63680 = CARTESIAN_POINT ( 'NONE',  ( 1.010498687664042716, -0.4281496062992124485, 0.4176697321401328655 ) ) ;
#63681 = CARTESIAN_POINT ( 'NONE',  ( -0.4840268112322907434, 0.02791078216816347476, -0.4328096321851898631 ) ) ;
#63682 = CARTESIAN_POINT ( 'NONE',  ( -0.3280839895013117347, -0.3690944881889763329, 0.3153832671262228327 ) ) ;
#63683 = CARTESIAN_POINT ( 'NONE',  ( -0.5643044619422565855, 0.05413385826771626580, -0.4176697321401330321 ) ) ;
#63684 = CARTESIAN_POINT ( 'NONE',  ( 1.535433070866142558, 0.2952755905511811885, 0.000000000000000000 ) ) ;
#63685 = CARTESIAN_POINT ( 'NONE',  ( -1.049868766404198794, 0.2306618581243847221, -0.2411417322834647770 ) ) ;
#63686 = CARTESIAN_POINT ( 'NONE',  ( 1.443569553805774897, -0.6046776061558809534, -0.2411417322834644161 ) ) ;
#63687 = CARTESIAN_POINT ( 'NONE',  ( -0.2867679344610365444, -0.2867679344610367664, -1.000675483760841811 ) ) ;
#63688 = CARTESIAN_POINT ( 'NONE',  ( -1.187664041994749731, -0.2845877964562159024, 0.3641732283464567677 ) ) ;
#63689 = CARTESIAN_POINT ( 'NONE',  ( -0.7233831536535030304, 2.232734770847148997, 0.5048085489442963869 ) ) ;
#63690 = CARTESIAN_POINT ( 'NONE',  ( 1.174540682414699111, -0.05778040916215560624, -0.4822834645669293319 ) ) ;
#63691 = CARTESIAN_POINT ( 'NONE',  ( -0.4091458600556405756, 0.2362204724409446288, -2.307742782152230721 ) ) ;
#63692 = CARTESIAN_POINT ( 'NONE',  ( -1.725721784776902190, -0.05778040916215522460, 0.4822834645669289988 ) ) ;
#63693 = CARTESIAN_POINT ( 'NONE',  ( 1.673228346456693494, 0.1660481256975885056, 0.3530559997133364547 ) ) ;
#63694 = CARTESIAN_POINT ( 'NONE',  ( -1.194225721784776262, -0.004921259842519870586, -0.3153832671262229437 ) ) ;
#63695 = CARTESIAN_POINT ( 'NONE',  ( 1.170763242744970123, 4.257495641787552160E-16, -0.4281993546915526805 ) ) ;
#63696 = CARTESIAN_POINT ( 'NONE',  ( -0.5905511811023613777, -0.6692913385826771977, 8.415575281601705876E-17 ) ) ;
#63697 = CARTESIAN_POINT ( 'NONE',  ( 0.07874015748031558404, -0.1870078740157479769, 0.3641732283464567677 ) ) ;
#63698 = CARTESIAN_POINT ( 'NONE',  ( -1.574803149606298636, -0.1870078740157479769, 0.3641732283464567677 ) ) ;
#63699 = CARTESIAN_POINT ( 'NONE',  ( 0.8661417322834652488, -0.1870078740157480601, -0.3641732283464567677 ) ) ;
#63700 = CARTESIAN_POINT ( 'NONE',  ( 0.8792650918635177559, 0.05413385826771666132, 0.4176697321401328100 ) ) ;
#63701 = CARTESIAN_POINT ( 'NONE',  ( 1.502624671916010790, -0.3162353388693409650, -0.4822834645669289433 ) ) ;
#63702 = CARTESIAN_POINT ( 'NONE',  ( 0.1181102362204730916, 0.1771653543307087630, 0.000000000000000000 ) ) ;
#63703 = CARTESIAN_POINT ( 'NONE',  ( 0.5643044619422579178, 0.05413385826771666132, 0.4176697321401328100 ) ) ;
#63704 = CARTESIAN_POINT ( 'NONE',  ( 0.6692913385826777528, 0.1771653543307087630, 0.000000000000000000 ) ) ;
#63705 = CARTESIAN_POINT ( 'NONE',  ( -1.653543307086613234, -0.1870078740157479769, 0.4822834645669291653 ) ) ;
#63706 = CARTESIAN_POINT ( 'NONE',  ( -1.259842519685038686, -0.1870078740157480879, -0.4822834645669291653 ) ) ;
#63707 = CARTESIAN_POINT ( 'NONE',  ( -0.3412073490813641308, -0.6046776061558807314, 0.2411417322834647770 ) ) ;
#63708 = CARTESIAN_POINT ( 'NONE',  ( 0.1070741851644054915, -0.3996062992125985480, -0.2427821522309711599 ) ) ;
#63709 = CARTESIAN_POINT ( 'NONE',  ( -0.2925321140481930149, -0.2925321140481933480, -2.655511811023622215 ) ) ;
#63710 = CARTESIAN_POINT ( 'NONE',  ( 0.5314960629921264834, 0.1660481256975883668, -0.3530559997133364547 ) ) ;
#63711 = CARTESIAN_POINT ( 'NONE',  ( 1.154855643044620184, 0.1283753931104746893, -0.1820866141732285504 ) ) ;
#63712 = CARTESIAN_POINT ( 'NONE',  ( -0.4790026246719152336, -0.05778040916215560624, -0.4822834645669293319 ) ) ;
#63713 = CARTESIAN_POINT ( 'NONE',  ( 0.3871391076115492380, -0.05778040916215560624, -0.4822834645669293319 ) ) ;
#63714 = CARTESIAN_POINT ( 'NONE',  ( 0.1070741851644054915, -0.3996062992125986035, -2.132545931758530244 ) ) ;
#63715 = CARTESIAN_POINT ( 'NONE',  ( 4.837279021331060870E-17, -0.3949938075777409963, -1.338582677165354173 ) ) ;
#63716 = CARTESIAN_POINT ( 'NONE',  ( 0.3996062992125986035, 0.1070741851644054776, -2.801837270341207553 ) ) ;
#63717 = CARTESIAN_POINT ( 'NONE',  ( 2.795275590551181910, 1.805669738366189048, 0.000000000000000000 ) ) ;
#63718 = VECTOR ( 'NONE', #46974, 39.37007874015748143 ) ;
#63719 = CARTESIAN_POINT ( 'NONE',  ( 0.3917322834645670104, 2.398668435337828261E-17, -0.7401574803149605364 ) ) ;
#63720 = CARTESIAN_POINT ( 'NONE',  ( -0.3608923884514428360, -0.5511811023622048555, -0.09757992244046775898 ) ) ;
#63721 = CARTESIAN_POINT ( 'NONE',  ( -1.095800524934382292, -0.05778040916215522460, 0.4822834645669289988 ) ) ;
#63722 = CARTESIAN_POINT ( 'NONE',  ( -0.1058382717557503072, 0.3949938075777408852, -2.760498687664042716 ) ) ;
#63723 = CARTESIAN_POINT ( 'NONE',  ( 0.6496062992125991586, -0.5400638737290845981, -0.3530559997133363437 ) ) ;
#63724 = CARTESIAN_POINT ( 'NONE',  ( 1.417322834645670104, -0.1870078740157479769, 0.4822834645669291653 ) ) ;
#63725 = CARTESIAN_POINT ( 'NONE',  ( 0.7349081364829402885, -0.6046776061558809534, -0.2411417322834644161 ) ) ;
#63726 = CARTESIAN_POINT ( 'NONE',  ( -0.3458507752293909498, 0.3458507752293907833, -2.696850393700787052 ) ) ;
#63727 = CARTESIAN_POINT ( 'NONE',  ( -0.1070741851644056997, 0.3996062992125986035, -2.368766404199475151 ) ) ;
#63728 = CARTESIAN_POINT ( 'NONE',  ( 1.673228346456693494, 0.1660481256975885056, 0.3530559997133364547 ) ) ;
#63729 = CARTESIAN_POINT ( 'NONE',  ( 0.4855643044619428750, 0.05413385826771666132, 0.4176697321401328100 ) ) ;
#63730 = CARTESIAN_POINT ( 'NONE',  ( 0.7414698162729663755, -0.6692913385826773087, -0.1292274648535924053 ) ) ;
#63731 = CIRCLE ( 'NONE', #27461, 0.3149606299212598381 ) ;
#63732 = CARTESIAN_POINT ( 'NONE',  ( 0.7414698162729663755, -0.5511811023622048555, -0.09757992244046775898 ) ) ;
#63733 = CARTESIAN_POINT ( 'NONE',  ( 1.108923884514436686, -0.3162353388693409650, -0.4822834645669289433 ) ) ;
#63734 = CARTESIAN_POINT ( 'NONE',  ( -0.3392501089628017219, -0.1958661417322836718, 0.02034120734908127781 ) ) ;
#63735 = CARTESIAN_POINT ( 'NONE',  ( 0.3608923884514443348, 0.2952755905511810774, -0.1292274648535930714 ) ) ;
#63736 = CARTESIAN_POINT ( 'NONE',  ( 0.9908136482939640111, -0.6692913385826771977, 0.1292274648535927661 ) ) ;
#63737 = CARTESIAN_POINT ( 'NONE',  ( 0.2559055118110243332, 0.1660481256975885056, 0.3530559997133364547 ) ) ;
#63738 = CARTESIAN_POINT ( 'NONE',  ( 1.397637795275591177, 0.07958543189024071263, -0.2665933059059888421 ) ) ;
#63739 = CARTESIAN_POINT ( 'NONE',  ( -0.8661417322834640276, -0.1870078740157480879, -0.4822834645669291653 ) ) ;
#63740 = CARTESIAN_POINT ( 'NONE',  ( -0.8267716535433065062, -0.6692913385826771977, 8.415575281601705876E-17 ) ) ;
#63741 = CARTESIAN_POINT ( 'NONE',  ( 1.351706036745407458, -0.4281496062992127816, -0.4176697321401328100 ) ) ;
#63742 = CARTESIAN_POINT ( 'NONE',  ( 0.3917322834645670104, 2.398668435337828261E-17, -0.5177165354330709457 ) ) ;
#63743 = CARTESIAN_POINT ( 'NONE',  ( 0.1958661417322836440, -0.3392501089628017219, -1.343832020997375531 ) ) ;
#63744 = CARTESIAN_POINT ( 'NONE',  ( -9.594673741351313045E-17, 0.3917322834645670104, -2.826771653543306506 ) ) ;
#63745 = EDGE_LOOP ( 'NONE', ( #20155, #42523, #5379, #80931, #58676, #28023, #16348, #2341, #63025, #506, #46895, #13119, #76390, #54631, #69617, #26392, #19126, #33846, #75862, #43574, #53907 ) ) ;
#63746 = CARTESIAN_POINT ( 'NONE',  ( -0.1998031496062994683, 0.3460692066303958092, -0.1706036745406824540 ) ) ;
#63747 = ORIENTED_EDGE ( 'NONE', *, *, #5614, .F. ) ;
#63748 = FACE_OUTER_BOUND ( 'NONE', #65105, .T. ) ;
#63749 = CARTESIAN_POINT ( 'NONE',  ( 1.437007874015748810, 0.07958543189024085140, 0.2665933059059887866 ) ) ;
#63750 = CARTESIAN_POINT ( 'NONE',  ( -0.3460692066303960868, 0.1998031496062990242, -1.601049868766404094 ) ) ;
#63751 = CARTESIAN_POINT ( 'NONE',  ( 1.227034120734908917, 0.1771653543307087075, -0.09757992244046823083 ) ) ;
#63752 = FACE_OUTER_BOUND ( 'NONE', #80434, .T. ) ;
#63753 = CARTESIAN_POINT ( 'NONE',  ( -0.2707102524865197535, 1.857296401297248600, 0.1576108120785336686 ) ) ;
#63754 = CARTESIAN_POINT ( 'NONE',  ( 0.2867679344610365999, -0.2867679344610365444, -0.8129921259842518566 ) ) ;
#63755 = CARTESIAN_POINT ( 'NONE',  ( -0.5511811023622038563, -0.1870078740157479769, 0.3641732283464567677 ) ) ;
#63756 = CARTESIAN_POINT ( 'NONE',  ( -1.568241469816272105, -0.08942795157527998196, 0.3641732283464567121 ) ) ;
#63757 = CARTESIAN_POINT ( 'NONE',  ( -1.404199475065615932, -0.4281496062992127816, -0.4176697321401328100 ) ) ;
#63758 = CARTESIAN_POINT ( 'NONE',  ( 0.2952755905511816326, -0.5400638737290844871, 0.3530559997133364547 ) ) ;
#63759 = CARTESIAN_POINT ( 'NONE',  ( 1.594488188976378673, 0.1660481256975885056, 0.3530559997133364547 ) ) ;
#63760 = ORIENTED_EDGE ( 'NONE', *, *, #22925, .T. ) ;
#63761 = CARTESIAN_POINT ( 'NONE',  ( 0.000000000000000000, 1.724409448818897905, 2.362204724409448620 ) ) ;
#63762 = CARTESIAN_POINT ( 'NONE',  ( 0.000000000000000000, 0.000000000000000000, 0.000000000000000000 ) ) ;
#63763 = CARTESIAN_POINT ( 'NONE',  ( 0.4091458600556404646, -0.2362204724409448231, -2.152230971128608950 ) ) ;
#63764 = PLANE ( 'NONE',  #53270 ) ;
#63765 = CARTESIAN_POINT ( 'NONE',  ( -0.6167979002624665030, -0.3690944881889765550, -0.3153832671262227771 ) ) ;
#63766 = EDGE_CURVE ( 'NONE', #58800, #80266, #56870, .T. ) ;
#63767 = CARTESIAN_POINT ( 'NONE',  ( -1.148293963254592542, 0.2952755905511811885, 0.1292274648535926551 ) ) ;
#63768 = CARTESIAN_POINT ( 'NONE',  ( 1.049868766404200349, 0.2306618581243848609, 0.2411417322834645549 ) ) ;
#63769 = ORIENTED_EDGE ( 'NONE', *, *, #72539, .F. ) ;
#63771 = CARTESIAN_POINT ( 'NONE',  ( -1.595398199321657051, 0.7585570207896576989, 0.1559797534342473035 ) ) ;
#63770 = CARTESIAN_POINT ( 'NONE',  ( 0.7217847769028878924, 0.05413385826771666132, 0.4176697321401328100 ) ) ;
#63772 = CARTESIAN_POINT ( 'NONE',  ( 1.082677165354331228, 0.1660481256975883668, -0.3530559997133364547 ) ) ;
#63773 = CARTESIAN_POINT ( 'NONE',  ( -1.345144356955379816, -0.05778040916215560624, -0.4822834645669293319 ) ) ;
#63774 = CARTESIAN_POINT ( 'NONE',  ( 0.2867679344610365999, 0.2867679344610365999, -1.005230028050182245 ) ) ;
#63775 = EDGE_CURVE ( 'NONE', #29190, #69836, #48781, .T. ) ;
#63776 = CARTESIAN_POINT ( 'NONE',  ( -0.4986876640419942164, -0.5023911411419708095, 0.1820866141732285504 ) ) ;
#63777 = CARTESIAN_POINT ( 'NONE',  ( 0.1049643490035304799, -0.3917322834645669549, -0.6423884514435697080 ) ) ;
#63778 = CONICAL_SURFACE ( 'NONE', #7310, 0.09842519685039351207, 1.029744258676652091 ) ;
#63779 = CARTESIAN_POINT ( 'NONE',  ( -0.6955380577427815458, -0.004921259842519576551, 0.3153832671262227771 ) ) ;
#63780 = CARTESIAN_POINT ( 'NONE',  ( 0.2230971128608929543, -0.004921259842519870586, -0.3153832671262229437 ) ) ;
#63781 = CARTESIAN_POINT ( 'NONE',  ( 0.01312335958005323398, 0.05413385826771666132, 0.4176697321401328100 ) ) ;
#63782 = CARTESIAN_POINT ( 'NONE',  ( -0.7939632545931750718, -0.08942795157528024563, -0.3641732283464568787 ) ) ;
#63783 = CARTESIAN_POINT ( 'NONE',  ( -0.1958661417322836995, 0.3392501089628017219, 0.1476184794937513700 ) ) ;
#63784 = CARTESIAN_POINT ( 'NONE',  ( 1.286089238845145033, 0.2306618581243848609, 0.2411417322834645549 ) ) ;
#63785 = CARTESIAN_POINT ( 'NONE',  ( -1.272965879265091305, 0.05413385826771626580, -0.4176697321401330321 ) ) ;
#63786 = CARTESIAN_POINT ( 'NONE',  ( 0.3458507752293908943, 0.3458507752293908943, -1.001968503937007871 ) ) ;
#63787 = CARTESIAN_POINT ( 'NONE',  ( -0.1640419947506555343, -0.3162353388693405765, 0.4822834645669290543 ) ) ;
#63788 = CARTESIAN_POINT ( 'NONE',  ( -0.9776902887139098386, 0.2952755905511810774, -0.1292274648535930714 ) ) ;
#63789 = CARTESIAN_POINT ( 'NONE',  ( 1.207349081364829990, 0.1283753931104748280, 0.1820866141732283561 ) ) ;
#63790 = AXIS2_PLACEMENT_3D ( 'NONE', #63103, #62692, #5034 ) ;
#63791 = CARTESIAN_POINT ( 'NONE',  ( -0.1902887139107604098, -0.5511811023622046335, 0.09757992244046803654 ) ) ;
#63792 = CARTESIAN_POINT ( 'NONE',  ( -0.4527559055118102749, 0.1660481256975885056, 0.3530559997133364547 ) ) ;
#63793 = CARTESIAN_POINT ( 'NONE',  ( -1.259842519685038686, -0.1870078740157480879, -0.4822834645669291653 ) ) ;
#63794 = DIRECTION ( 'NONE',  ( 0.000000000000000000, 0.000000000000000000, 1.000000000000000000 ) ) ;
#63795 = CARTESIAN_POINT ( 'NONE',  ( 1.174540682414699111, -0.2845877964562159024, 0.3641732283464567677 ) ) ;
#63796 = CARTESIAN_POINT ( 'NONE',  ( -0.3937007874015740483, -0.1870078740157479769, 0.4822834645669291653 ) ) ;
#63797 = CARTESIAN_POINT ( 'NONE',  ( -1.699475065616797398, 0.2952755905511811885, 0.1292274648535926551 ) ) ;
#63798 = ORIENTED_EDGE ( 'NONE', *, *, #30238, .T. ) ;
#63799 = CARTESIAN_POINT ( 'NONE',  ( 0.3996062992125984925, 0.1070741851644054637, -2.406167979002624246 ) ) ;
#63800 = CARTESIAN_POINT ( 'NONE',  ( -0.9448818897637790704, -0.1870078740157480601, -0.3641732283464567677 ) ) ;
#63801 = CARTESIAN_POINT ( 'NONE',  ( 1.187664041994751285, -0.3162353388693409650, -0.4822834645669289433 ) ) ;
#63802 = CARTESIAN_POINT ( 'NONE',  ( -1.049868766404198794, 0.1283753931104746893, -0.1820866141732285504 ) ) ;
#63803 = CARTESIAN_POINT ( 'NONE',  ( -0.1998031496062991630, -0.3460692066303959202, -1.244750656167979086 ) ) ;
#63804 = CARTESIAN_POINT ( 'NONE',  ( -1.115485564304461219, -0.4281496062992124485, 0.4176697321401328655 ) ) ;
#63805 = CARTESIAN_POINT ( 'NONE',  ( 0.8727034120734913358, -0.05778040916215522460, 0.4822834645669289988 ) ) ;
#63806 = CARTESIAN_POINT ( 'NONE',  ( 0.9645669291338591078, -0.5400638737290845981, -0.3530559997133363437 ) ) ;
#63807 = CARTESIAN_POINT ( 'NONE',  ( 1.482939632545932307, 0.05413385826771626580, -0.4176697321401330321 ) ) ;
#63808 = CARTESIAN_POINT ( 'NONE',  ( -1.601049868766403650, -0.5023911411419708095, 0.1820866141732285504 ) ) ;
#63809 = CARTESIAN_POINT ( 'NONE',  ( -0.1070741851644051862, -0.3996062992125986035, -0.4639107611548556331 ) ) ;
#63810 = CARTESIAN_POINT ( 'NONE',  ( -0.3996062992125986035, -7.340648628747425578E-17, -0.8267716535433070613 ) ) ;
#63811 = CARTESIAN_POINT ( 'NONE',  ( 0.3420746716998660508, -0.1974969037888703871, -0.1049868766404199877 ) ) ;
#63812 = DIRECTION ( 'NONE',  ( 0.000000000000000000, -1.000000000000000000, 0.000000000000000000 ) ) ;
#63813 = CARTESIAN_POINT ( 'NONE',  ( 1.305774278215223960, -0.5511811023622046335, 0.09757992244046803654 ) ) ;
#63814 = CARTESIAN_POINT ( 'NONE',  ( 0.7086614173228352742, -0.1870078740157480601, -0.3641732283464567677 ) ) ;
#63815 = CARTESIAN_POINT ( 'NONE',  ( 0.1312335958005255154, -0.6046776061558807314, 0.2411417322834647770 ) ) ;
#63816 = CARTESIAN_POINT ( 'NONE',  ( 1.581364829396326277, -0.05778040916215522460, 0.4822834645669289988 ) ) ;
#63817 = CARTESIAN_POINT ( 'NONE',  ( 0.1058382717557500852, -0.3949938075777408852, -1.264435695538058013 ) ) ;
#63818 = CARTESIAN_POINT ( 'NONE',  ( 0.8464566929133866546, -0.4536011799217367080, 0.2665933059059888421 ) ) ;
#63819 = CARTESIAN_POINT ( 'NONE',  ( -0.4855643044619415427, 0.05413385826771626580, -0.4176697321401330321 ) ) ;
#63820 = CARTESIAN_POINT ( 'NONE',  ( -1.377952755905511140, -0.6692913385826771977, 8.415575281601705876E-17 ) ) ;
#63821 = CARTESIAN_POINT ( 'NONE',  ( 1.049868766404200349, 0.2306618581243848609, 0.2411417322834645549 ) ) ;
#63822 = CARTESIAN_POINT ( 'NONE',  ( -0.4724409448818898682, -8.678599364036362592E-17, -1.614173228346456712 ) ) ;
#63823 = CARTESIAN_POINT ( 'NONE',  ( -0.7773926554473638006, -2.191421614605370878E-15, 0.4445507791589071167 ) ) ;
#63824 = ORIENTED_EDGE ( 'NONE', *, *, #41919, .F. ) ;
#63825 = ORIENTED_EDGE ( 'NONE', *, *, #30136, .F. ) ;
#63826 = CARTESIAN_POINT ( 'NONE',  ( -1.299212598425196097, -0.6692913385826771977, 8.415575281601705876E-17 ) ) ;
#63827 = EDGE_CURVE ( 'NONE', #11296, #29599, #52093, .T. ) ;
#63828 = CARTESIAN_POINT ( 'NONE',  ( -0.7086614173228339419, -0.1870078740157479769, 0.4822834645669291653 ) ) ;
#63830 = CARTESIAN_POINT ( 'NONE',  ( -0.9186351706036736120, -0.6046776061558809534, -0.2411417322834644161 ) ) ;
#63829 = CARTESIAN_POINT ( 'NONE',  ( -0.7086614173228339419, -0.1870078740157479769, 0.3641732283464567677 ) ) ;
#63831 = CARTESIAN_POINT ( 'NONE',  ( 0.2867679344610365999, 0.2867679344610365999, -2.107592232774591068 ) ) ;
#63832 = AXIS2_PLACEMENT_3D ( 'NONE', #78912, #77655, #58693 ) ;
#63833 = CARTESIAN_POINT ( 'NONE',  ( -0.2559055118110227234, -0.5400638737290844871, 0.3530559997133364547 ) ) ;
#63834 = CARTESIAN_POINT ( 'NONE',  ( 1.614173228346457378, 0.2952755905511811885, 0.000000000000000000 ) ) ;
#63835 = CARTESIAN_POINT ( 'NONE',  ( -0.9514435695538050464, -0.3162353388693405765, 0.4822834645669290543 ) ) ;
#63836 = CARTESIAN_POINT ( 'NONE',  ( 0.3937007874015754361, -0.1870078740157480879, -0.4822834645669291653 ) ) ;
#63837 = CARTESIAN_POINT ( 'NONE',  ( -0.8727034120734901146, -0.3162353388693405765, 0.4822834645669290543 ) ) ;
#63838 = CARTESIAN_POINT ( 'NONE',  ( 0.1049643490035304938, -0.3917322834645669549, -1.494750656167978642 ) ) ;
#63839 = CARTESIAN_POINT ( 'NONE',  ( -0.8202099737532799750, 0.1771653543307087075, -0.09757992244046823083 ) ) ;
#63840 = ORIENTED_EDGE ( 'NONE', *, *, #33956, .F. ) ;
#63841 = CARTESIAN_POINT ( 'NONE',  ( 0.1974969037888706369, -0.3420746716998659953, -1.666666666666666741 ) ) ;
#63842 = EDGE_LOOP ( 'NONE', ( #43430, #16579, #59690, #19239 ) ) ;
#63843 = CARTESIAN_POINT ( 'NONE',  ( -1.607611548556429737, -0.5511811023622046335, 0.09757992244046803654 ) ) ;
#63844 = CARTESIAN_POINT ( 'NONE',  ( -1.174540682414697335, -0.05778040916215522460, 0.4822834645669289988 ) ) ;
#63845 = CARTESIAN_POINT ( 'NONE',  ( -0.8792650918635160906, -0.4281496062992124485, 0.4176697321401328655 ) ) ;
#63846 = CARTESIAN_POINT ( 'NONE',  ( -0.1998031496062994683, 0.3460692066303958092, -0.1706036745406823985 ) ) ;
#63847 = CARTESIAN_POINT ( 'NONE',  ( -1.181102362204723644, -0.1870078740157480879, -0.4822834645669291653 ) ) ;
#63848 = CARTESIAN_POINT ( 'NONE',  ( -1.391076115485563758, 0.2306618581243848609, 0.2411417322834645549 ) ) ;
#63849 = CARTESIAN_POINT ( 'NONE',  ( 2.795275590551181466, 1.968503937007874960, 0.000000000000000000 ) ) ;
#63850 = FACE_OUTER_BOUND ( 'NONE', #10147, .T. ) ;
#63851 = VECTOR ( 'NONE', #66789, 39.37007874015748854 ) ;
#63852 = CARTESIAN_POINT ( 'NONE',  ( 0.5511811023622055217, -0.1870078740157479769, 0.3641732283464567677 ) ) ;
#63853 = CARTESIAN_POINT ( 'NONE',  ( 3.264097702071373064, 2.755905511811024056, 0.5314960629921260393 ) ) ;
#63854 = CARTESIAN_POINT ( 'NONE',  ( -0.2867679344610365999, 0.2867679344610364889, -0.5767716535433071723 ) ) ;
#63855 = CARTESIAN_POINT ( 'NONE',  ( -0.5708661417322828946, 0.07958543189024071263, -0.2665933059059888421 ) ) ;
#63856 = CARTESIAN_POINT ( 'NONE',  ( -0.9580052493438311334, 0.05413385826771626580, -0.4176697321401330321 ) ) ;
#63857 = CARTESIAN_POINT ( 'NONE',  ( 1.489501312335958172, -0.05778040916215560624, -0.4822834645669293319 ) ) ;
#63858 = CARTESIAN_POINT ( 'NONE',  ( -0.3149606299212590610, -0.1870078740157480879, -0.4822834645669291653 ) ) ;
#63859 = CARTESIAN_POINT ( 'NONE',  ( 0.4177787735907000366, 0.000000000000000000, -1.559171609364239375 ) ) ;
#63860 = ORIENTED_EDGE ( 'NONE', *, *, #41759, .T. ) ;
#63861 = CARTESIAN_POINT ( 'NONE',  ( -0.1998031496062994405, 0.3460692066303957537, -2.137139107611548905 ) ) ;
#63862 = CARTESIAN_POINT ( 'NONE',  ( -0.5774278215223089816, -0.6046776061558807314, 0.2411417322834647770 ) ) ;
#63863 = CARTESIAN_POINT ( 'NONE',  ( 1.377952755905512472, -0.6692913385826771977, 8.415575281601705876E-17 ) ) ;
#63864 = CARTESIAN_POINT ( 'NONE',  ( -1.259842519685038686, -0.1870078740157479769, 0.3641732283464567677 ) ) ;
#63865 = CARTESIAN_POINT ( 'NONE',  ( -1.253280839895012377, -0.05778040916215522460, 0.4822834645669289988 ) ) ;
#63866 = CARTESIAN_POINT ( 'NONE',  ( -0.3458507752293909498, 0.3458507752293907833, -0.6496062992125984925 ) ) ;
#63867 = CARTESIAN_POINT ( 'NONE',  ( -0.4736532623569962297, 1.506389555808205660, 3.908412207303153973 ) ) ;
#63868 = CARTESIAN_POINT ( 'NONE',  ( 0.3917322834645670104, -0.1049643490035303411, -0.1036745406824146343 ) ) ;
#63869 = CARTESIAN_POINT ( 'NONE',  ( -0.3917322834645669549, -0.1049643490035306603, -2.177821522309711266 ) ) ;
#63870 = CARTESIAN_POINT ( 'NONE',  ( 0.1181102362204730916, 0.2952755905511811885, 0.000000000000000000 ) ) ;
#63871 = CARTESIAN_POINT ( 'NONE',  ( -1.036745406824146176, -0.3690944881889763329, 0.3153832671262228327 ) ) ;
#63872 = CARTESIAN_POINT ( 'NONE',  ( -0.1968503937007867743, -0.6692913385826771977, 8.415575281601705876E-17 ) ) ;
#63873 = CARTESIAN_POINT ( 'NONE',  ( -0.4724409448818895907, -0.1265901696524993070, -2.799868766404198794 ) ) ;
#63874 = CARTESIAN_POINT ( 'NONE',  ( -0.7611548556430438595, 0.2306618581243848609, 0.2411417322834645549 ) ) ;
#63875 = CARTESIAN_POINT ( 'NONE',  ( -0.9842519685039365918, -0.6692913385826771977, 8.415575281601705876E-17 ) ) ;
#63876 = CARTESIAN_POINT ( 'NONE',  ( 0.3949938075777409963, 2.418639510665530743E-17, -2.084645669291338876 ) ) ;
#63877 = CARTESIAN_POINT ( 'NONE',  ( 0.9580052493438326877, -0.004921259842519576551, 0.3153832671262227771 ) ) ;
#63878 = CARTESIAN_POINT ( 'NONE',  ( -0.9448818897637790704, -0.1870078740157479769, 0.3641732283464567677 ) ) ;
#63879 = CARTESIAN_POINT ( 'NONE',  ( 0.8333333333333340365, -0.5511811023622046335, 0.09757992244046803654 ) ) ;
#63880 = CARTESIAN_POINT ( 'NONE',  ( -1.686351706036744558, 0.2952755905511810774, -0.1292274648535930714 ) ) ;
#63881 = CARTESIAN_POINT ( 'NONE',  ( 1.515748031496063186, -0.5400638737290845981, -0.3530559997133363437 ) ) ;
#63882 = PRODUCT_DEFINITION_CONTEXT ( 'detailed design', #75624, 'design' ) ;
#63883 = CARTESIAN_POINT ( 'NONE',  ( 0.5774278215223104249, 0.1283753931104748280, 0.1820866141732283561 ) ) ;
#63884 = CARTESIAN_POINT ( 'NONE',  ( 0.3392501089628018329, 0.1958661417322835607, -1.540682414698162805 ) ) ;
#63885 = CARTESIAN_POINT ( 'NONE',  ( -0.8530183727034112984, 0.05413385826771666132, 0.4176697321401328100 ) ) ;
#63886 = CARTESIAN_POINT ( 'NONE',  ( 1.305774278215223960, 0.2952755905511810774, -0.1292274648535930714 ) ) ;
#63887 = CARTESIAN_POINT ( 'NONE',  ( -0.2362204724409451284, 0.4091458600556402425, 0.06758530183727033680 ) ) ;
#63888 = CARTESIAN_POINT ( 'NONE',  ( -0.2427821522309703550, -0.2845877964562159024, 0.3641732283464567677 ) ) ;
#63889 = CARTESIAN_POINT ( 'NONE',  ( -3.937007874015748143, 1.724409448818897905, -0.4359958488159722534 ) ) ;
#63890 = CARTESIAN_POINT ( 'NONE',  ( 0.3805774278215230400, -0.4281496062992124485, 0.4176697321401328655 ) ) ;
#63891 = CARTESIAN_POINT ( 'NONE',  ( 0.2549859370038549122, 0.1502491711592394974, 0.1564451348283543708 ) ) ;
#63892 = CARTESIAN_POINT ( 'NONE',  ( 1.017060367454068581, -0.08942795157528024563, -0.3641732283464568787 ) ) ;
#63893 = CARTESIAN_POINT ( 'NONE',  ( 0.1640419947506569498, -0.08942795157527998196, 0.3641732283464567121 ) ) ;
#63894 = CARTESIAN_POINT ( 'NONE',  ( 0.2427821522309719648, -0.05778040916215522460, 0.4822834645669289988 ) ) ;
#63895 = CARTESIAN_POINT ( 'NONE',  ( -1.358267716535432434, 0.1660481256975883668, -0.3530559997133364547 ) ) ;
#63896 = CARTESIAN_POINT ( 'NONE',  ( -0.8333333333333323711, 0.1771653543307087630, 0.09757992244046791164 ) ) ;
#63897 = DIRECTION ( 'NONE',  ( 1.000000000000000000, 0.000000000000000000, -0.000000000000000000 ) ) ;
#63898 = EDGE_CURVE ( 'NONE', #895, #78156, #56194, .T. ) ;
#63899 = CARTESIAN_POINT ( 'NONE',  ( -0.3543307086614165824, 0.2952755905511811885, 0.000000000000000000 ) ) ;
#63900 = CARTESIAN_POINT ( 'NONE',  ( 0.3460692066303959202, -0.1998031496062991630, -1.284120734908136496 ) ) ;
#63901 =( BOUNDED_CURVE ( )  B_SPLINE_CURVE ( 2, ( #78401, #71658, #20311, #77563, #38824, #58600, #19897, #14010, #45962, #52277, #542, #13586, #25772 ),
 .UNSPECIFIED., .F., .F. ) 
 B_SPLINE_CURVE_WITH_KNOTS ( ( 3, 2, 2, 2, 2, 2, 3 ),
 ( 0.4915129128166190742, 0.4924242424242424310, 0.4962121212121212155, 0.5000000000000000000, 0.5037878787878787845, 0.5075757575757575690, 0.5084870871833810924 ),
 .UNSPECIFIED. ) 
 CURVE ( )  GEOMETRIC_REPRESENTATION_ITEM ( )  RATIONAL_B_SPLINE_CURVE ( ( 0.9875488213027530104, 0.9918020599134685922, 1.000000000000000000, 0.9659258262890683122, 1.000000000000000000, 0.9659258262890683122, 1.000000000000000000, 0.9659258262890683122, 1.000000000000000000, 0.9659258262890683122, 1.000000000000000000, 0.9918020599134671489, 0.9875488213027514561 ) ) 
 REPRESENTATION_ITEM ( '' )  );
#63902 = CARTESIAN_POINT ( 'NONE',  ( 0.3917322834645670104, 2.398668435337828261E-17, -2.407480314960630086 ) ) ;
#63903 = CARTESIAN_POINT ( 'NONE',  ( 0.3871391076115492380, -0.08942795157528024563, -0.3641732283464568787 ) ) ;
#63904 = CARTESIAN_POINT ( 'NONE',  ( -0.4658792650918627265, -0.3162353388693409650, -0.4822834645669289433 ) ) ;
#63905 = CARTESIAN_POINT ( 'NONE',  ( -1.174540682414697335, -0.05778040916215522460, 0.4822834645669289988 ) ) ;
#63906 = CARTESIAN_POINT ( 'NONE',  ( -0.6364829396325453192, -0.08942795157528024563, -0.3641732283464568787 ) ) ;
#63907 = CARTESIAN_POINT ( 'NONE',  ( -3.937006426163500716, 1.063004141356476140, 0.03136679951920979398 ) ) ;
#63908 = CARTESIAN_POINT ( 'NONE',  ( -0.6364829396325453192, -0.05778040916215560624, -0.4822834645669293319 ) ) ;
#63909 = CARTESIAN_POINT ( 'NONE',  ( -0.9186351706036736120, -0.5023911411419708095, -0.1820866141732282451 ) ) ;
#63910 = CARTESIAN_POINT ( 'NONE',  ( -1.423884514435694859, -0.2845877964562159024, 0.3641732283464567677 ) ) ;
#63911 = CARTESIAN_POINT ( 'NONE',  ( 1.187664041994751285, -0.3162353388693409650, -0.4822834645669289433 ) ) ;
#63912 = CARTESIAN_POINT ( 'NONE',  ( -0.4702989522381291199, 1.601790779910749807, 1.018730689361767583 ) ) ;
#63913 = CARTESIAN_POINT ( 'NONE',  ( 0.3392501089628018884, -0.1958661417322833942, -2.306449761976065105 ) ) ;
#63914 = VERTEX_POINT ( 'NONE', #459 ) ;
#63915 = CARTESIAN_POINT ( 'NONE',  ( 0.4177787735906991484, 1.312623414240987163, -1.404325600637324367 ) ) ;
#63916 = CARTESIAN_POINT ( 'NONE',  ( -1.345144356955379816, -0.05778040916215560624, -0.4822834645669293319 ) ) ;
#63917 = CARTESIAN_POINT ( 'NONE',  ( -1.017060367454067249, -0.3162353388693409650, -0.4822834645669289433 ) ) ;
#63918 = EDGE_CURVE ( 'NONE', #66254, #10557, #64978, .T. ) ;
#63919 = CARTESIAN_POINT ( 'NONE',  ( -1.568241469816272105, -0.3162353388693409650, -0.4822834645669289433 ) ) ;
#63920 = CARTESIAN_POINT ( 'NONE',  ( 0.1958661417322834775, 0.3392501089628018884, -2.118766404199475151 ) ) ;
#63921 = CARTESIAN_POINT ( 'NONE',  ( -0.3758920641862481538, 0.1123167701215816577, -1.220472440944881942 ) ) ;
#63922 = EDGE_CURVE ( 'NONE', #45375, #3191, #66922, .T. ) ;
#63923 = CARTESIAN_POINT ( 'NONE',  ( 0.9186351706036752773, 0.2306618581243847221, -0.2411417322834647770 ) ) ;
#63924 = CARTESIAN_POINT ( 'NONE',  ( -0.01968503937007793844, 0.1660481256975883668, -0.3530559997133364547 ) ) ;
#63925 = CARTESIAN_POINT ( 'NONE',  ( -0.6986524979670485358, -2.191421614605370878E-15, 0.4445507791589071167 ) ) ;
#63926 = CARTESIAN_POINT ( 'NONE',  ( 0.1070741851644053527, 0.3996062992125985480, -2.747375328083989210 ) ) ;
#63927 = CARTESIAN_POINT ( 'NONE',  ( 1.161417322834646271, 0.07958543189024071263, -0.2665933059059888421 ) ) ;
#63928 = CARTESIAN_POINT ( 'NONE',  ( 0.3460692066303959757, -0.1998031496062991907, -1.207349081364829324 ) ) ;
#63929 = ORIENTED_EDGE ( 'NONE', *, *, #28395, .T. ) ;
#63930 = CARTESIAN_POINT ( 'NONE',  ( 0.3917322834645670104, 2.398668435337828261E-17, -2.944881889763779181 ) ) ;
#63931 = VERTEX_POINT ( 'NONE', #33695 ) ;
#63932 = CARTESIAN_POINT ( 'NONE',  ( 0.04593175853018440641, 0.2952755905511810774, -0.1292274648535930714 ) ) ;
#63933 = CARTESIAN_POINT ( 'NONE',  ( -0.9055118110236215490, 0.2952755905511811885, 0.000000000000000000 ) ) ;
#63934 = CARTESIAN_POINT ( 'NONE',  ( -1.535433070866141225, -0.6692913385826771977, 8.415575281601705876E-17 ) ) ;
#63935 = CARTESIAN_POINT ( 'NONE',  ( 0.5905511811023629321, 0.2952755905511811885, 0.000000000000000000 ) ) ;
#63936 = CARTESIAN_POINT ( 'NONE',  ( -1.627296587926508442, 0.1283753931104748280, 0.1820866141732283561 ) ) ;
#63937 = CARTESIAN_POINT ( 'NONE',  ( 1.358267716535433323, -0.5400638737290845981, -0.3530559997133363437 ) ) ;
#63938 = CARTESIAN_POINT ( 'NONE',  ( -0.6561679790026240244, 0.2306618581243847221, -0.2411417322834647770 ) ) ;
#63939 = CARTESIAN_POINT ( 'NONE',  ( -1.161417322834644716, 0.1660481256975885056, 0.3530559997133364547 ) ) ;
#63940 = CARTESIAN_POINT ( 'NONE',  ( 1.410761154855643795, -0.3162353388693405765, 0.4822834645669290543 ) ) ;
#63941 = CARTESIAN_POINT ( 'NONE',  ( 1.666666666666667185, 0.05413385826771666132, 0.4176697321401328100 ) ) ;
#63942 = CARTESIAN_POINT ( 'NONE',  ( -0.1049868766404193215, 0.2306618581243847221, -0.2411417322834647770 ) ) ;
#63943 = CARTESIAN_POINT ( 'NONE',  ( 0.1049643490035304938, -0.3917322834645669549, -0.2349081364829396223 ) ) ;
#63944 = CARTESIAN_POINT ( 'NONE',  ( 0.5183727034120741983, -0.5511811023622046335, 0.09757992244046803654 ) ) ;
#63945 = ORIENTED_EDGE ( 'NONE', *, *, #75955, .F. ) ;
#63946 = CARTESIAN_POINT ( 'NONE',  ( 4.837279021331060870E-17, -0.3949938075777409963, -0.7086614173228346081 ) ) ;
#63947 = ORIENTED_EDGE ( 'NONE', *, *, #50925, .F. ) ;
#63948 = CARTESIAN_POINT ( 'NONE',  ( -0.08530183727034056085, -0.08942795157528024563, -0.3641732283464568787 ) ) ;
#63949 = AXIS2_PLACEMENT_3D ( 'NONE', #66709, #9042, #6437 ) ;
#63950 = CARTESIAN_POINT ( 'NONE',  ( 2.647193076292333025, 1.325969025732682605, -0.4256800600601902684 ) ) ;
#63951 = CARTESIAN_POINT ( 'NONE',  ( 0.07874015748031558404, -0.1870078740157480879, -0.4822834645669291653 ) ) ;
#63952 = CARTESIAN_POINT ( 'NONE',  ( -0.09186351706036689768, 0.05413385826771626580, -0.4176697321401330321 ) ) ;
#63953 = CARTESIAN_POINT ( 'NONE',  ( -0.7742782152230965886, 0.05413385826771666132, 0.4176697321401328100 ) ) ;
#63954 = CARTESIAN_POINT ( 'NONE',  ( -0.1049643490035302301, -0.3917322834645671770, -1.643720103183414105 ) ) ;
#63955 = CARTESIAN_POINT ( 'NONE',  ( -1.207349081364828436, -0.6046776061558807314, 0.2411417322834647770 ) ) ;
#63956 = CARTESIAN_POINT ( 'NONE',  ( -0.1958661417322834220, -0.3392501089628018884, -2.827427821522309426 ) ) ;
#63957 = CARTESIAN_POINT ( 'NONE',  ( 0.7217847769028878924, -0.3690944881889765550, -0.3153832671262227771 ) ) ;
#63958 = CARTESIAN_POINT ( 'NONE',  ( 1.089238845144357759, 0.05413385826771626580, -0.4176697321401330321 ) ) ;
#63959 = CARTESIAN_POINT ( 'NONE',  ( 0.9711286089238851948, -0.6046776061558809534, -0.2411417322834644161 ) ) ;
#63960 = CARTESIAN_POINT ( 'NONE',  ( -0.1070741851644051862, -0.3996062992125987146, -1.017060367454067915 ) ) ;
#63961 = CARTESIAN_POINT ( 'NONE',  ( -1.325459317585300889, -0.4281496062992127816, -0.4176697321401328100 ) ) ;
#63962 = CARTESIAN_POINT ( 'NONE',  ( -0.1070741851644051862, -0.3996062992125986590, -0.1489501312335958227 ) ) ;
#63963 = CARTESIAN_POINT ( 'NONE',  ( 0.3460692066303959202, -0.1998031496062991630, -0.02427821522309713681 ) ) ;
#63964 = CARTESIAN_POINT ( 'NONE',  ( 0.05905511811023681640, 0.1660481256975883668, -0.3530559997133364547 ) ) ;
#63965 = CARTESIAN_POINT ( 'NONE',  ( 0.3460692066303959202, 0.1998031496062993295, -2.808398950131233640 ) ) ;
#63966 = CARTESIAN_POINT ( 'NONE',  ( -0.1958661417322834220, -0.3392501089628018884, -1.882545931758530244 ) ) ;
#63967 = CARTESIAN_POINT ( 'NONE',  ( 1.233595800524935227, -0.6046776061558807314, 0.2411417322834647770 ) ) ;
#63968 = CIRCLE ( 'NONE', #68021, 0.1771653543307086798 ) ;
#63969 = CARTESIAN_POINT ( 'NONE',  ( 1.246719160104987623, 0.05413385826771626580, -0.4176697321401330321 ) ) ;
#63970 = CARTESIAN_POINT ( 'NONE',  ( 0.2034120734908144990, -0.5511811023622046335, 0.09757992244046803654 ) ) ;
#63971 = CARTESIAN_POINT ( 'NONE',  ( 0.9055118110236227702, -0.6692913385826771977, 8.415575281601705876E-17 ) ) ;
#63972 = CARTESIAN_POINT ( 'NONE',  ( -0.4091458600556402980, -0.2362204724409451284, -1.546587926509186639 ) ) ;
#63973 = CARTESIAN_POINT ( 'NONE',  ( 0.1509186351706045259, -0.08942795157528024563, -0.3641732283464568787 ) ) ;
#63974 = CARTESIAN_POINT ( 'NONE',  ( 0.1771653543307093182, 0.1660481256975885056, 0.3530559997133364547 ) ) ;
#63975 = CARTESIAN_POINT ( 'NONE',  ( -0.3420746716998662729, 0.1974969037888702206, -1.047900262467191590 ) ) ;
#63976 = CARTESIAN_POINT ( 'NONE',  ( -1.246719160104986512, 0.05413385826771666132, 0.4176697321401328100 ) ) ;
#63977 = CARTESIAN_POINT ( 'NONE',  ( 0.9973753280839902091, 0.1283753931104746893, -0.1820866141732285504 ) ) ;
#63978 = CARTESIAN_POINT ( 'NONE',  ( -2.362204724409448620, 1.929133858267716661, 0.5118110236220224651 ) ) ;
#63979 = CARTESIAN_POINT ( 'NONE',  ( -0.4527559055118102749, 0.1660481256975885056, 0.3530559997133364547 ) ) ;
#63980 = CARTESIAN_POINT ( 'NONE',  ( -0.3149606299212590610, -0.1870078740157480601, -0.3641732283464567677 ) ) ;
#63981 = DIRECTION ( 'NONE',  ( 0.000000000000000000, 1.000000000000000000, 0.000000000000000000 ) ) ;
#63982 = CARTESIAN_POINT ( 'NONE',  ( -0.4199475065616791736, 0.2306618581243847221, -0.2411417322834647770 ) ) ;
#63983 = CARTESIAN_POINT ( 'NONE',  ( 0.4199475065616803948, -0.5023911411419708095, -0.1820866141732282451 ) ) ;
#63984 = EDGE_CURVE ( 'NONE', #32456, #32791, #15179, .T. ) ;
#63985 = CARTESIAN_POINT ( 'NONE',  ( -0.2925321140481932369, 0.2925321140481931259, -2.143700787401574548 ) ) ;
#63986 = CARTESIAN_POINT ( 'NONE',  ( -0.01312335958005186876, 0.05413385826771626580, -0.4176697321401330321 ) ) ;
#63987 = CARTESIAN_POINT ( 'NONE',  ( 0.3917322834645669549, 2.398668435337827645E-17, -1.772946563483252858 ) ) ;
#63988 = CARTESIAN_POINT ( 'NONE',  ( 1.213910761154856299, 0.1771653543307087630, 0.09757992244046791164 ) ) ;
#63989 = DIRECTION ( 'NONE',  ( -0.000000000000000000, -0.000000000000000000, -1.000000000000000000 ) ) ;
#63990 = CARTESIAN_POINT ( 'NONE',  ( -0.8202099737532801971, -0.5511811023622046335, 0.09757992244046803654 ) ) ;
#63991 = CARTESIAN_POINT ( 'NONE',  ( -0.8136482939632537770, -0.5023911411419708095, 0.1820866141732285504 ) ) ;
#63992 = CARTESIAN_POINT ( 'NONE',  ( -0.2821522309711278487, -0.6692913385826773087, -0.1292274648535924053 ) ) ;
#63993 = CARTESIAN_POINT ( 'NONE',  ( -0.03937007874015669567, -0.6692913385826771977, 8.415575281601705876E-17 ) ) ;
#63994 = CARTESIAN_POINT ( 'NONE',  ( 0.4855643044619430415, -0.3690944881889765550, -0.3153832671262227771 ) ) ;
#63995 = CARTESIAN_POINT ( 'NONE',  ( -0.2524772379609336315, 0.1532855601034649740, 5.612412912560979628 ) ) ;
#63996 = CARTESIAN_POINT ( 'NONE',  ( 1.391076115485564868, -0.5023911411419708095, 0.1820866141732285504 ) ) ;
#63997 = CARTESIAN_POINT ( 'NONE',  ( 0.7742782152230979209, 0.05413385826771626580, -0.4176697321401330321 ) ) ;
#63998 = CARTESIAN_POINT ( 'NONE',  ( 0.4426497960380878505, 1.366130357955170016, -2.105050863655339111 ) ) ;
#63999 = CARTESIAN_POINT ( 'NONE',  ( -0.2427821522309703550, -0.05778040916215560624, -0.4822834645669293319 ) ) ;
#64000 = CARTESIAN_POINT ( 'NONE',  ( 0.3392501089628018884, -0.1958661417322834220, -0.9770341207349081403 ) ) ;
#64001 = CARTESIAN_POINT ( 'NONE',  ( -1.476377952755905110, -0.5400638737290845981, -0.3530559997133363437 ) ) ;
#64003 = CARTESIAN_POINT ( 'NONE',  ( 0.8858267716535438430, 0.1660481256975885056, 0.3530559997133364547 ) ) ;
#64002 = VECTOR ( 'NONE', #41551, 39.37007874015748143 ) ;
#64004 = CIRCLE ( 'NONE', #43865, 0.07874015748031502893 ) ;
#64005 = CARTESIAN_POINT ( 'NONE',  ( 0.4002624671916016896, -0.05778040916215522460, 0.4822834645669289988 ) ) ;
#64006 = CARTESIAN_POINT ( 'NONE',  ( -0.4501861592487448327, 1.384549727180958811, -3.911202737410993890 ) ) ;
#64007 = CARTESIAN_POINT ( 'NONE',  ( 0.2034120734908144990, -0.5511811023622046335, 0.09757992244046803654 ) ) ;
#64008 = CARTESIAN_POINT ( 'NONE',  ( 1.259842519685040019, -0.1870078740157480879, -0.4822834645669291653 ) ) ;
#64009 = CARTESIAN_POINT ( 'NONE',  ( -0.2887139107611542133, 0.1283753931104748280, 0.1820866141732283561 ) ) ;
#64010 = CARTESIAN_POINT ( 'NONE',  ( -0.6036745406824141069, -0.6046776061558809534, -0.2411417322834644161 ) ) ;
#64011 = CARTESIAN_POINT ( 'NONE',  ( 0.8530183727034126306, 0.05413385826771626580, -0.4176697321401330321 ) ) ;
#64012 = CARTESIAN_POINT ( 'NONE',  ( 0.2821522309711292364, -0.6692913385826771977, 0.1292274648535927661 ) ) ;
#64013 = CARTESIAN_POINT ( 'NONE',  ( -0.9842519685039360366, 0.2952755905511811885, 0.000000000000000000 ) ) ;
#64014 = CARTESIAN_POINT ( 'NONE',  ( -0.6299212598425188991, -0.1870078740157479769, 0.3641732283464567677 ) ) ;
#64015 = CARTESIAN_POINT ( 'NONE',  ( 0.1968503937007881344, 0.2952755905511811885, 0.000000000000000000 ) ) ;
#64016 = CARTESIAN_POINT ( 'NONE',  ( -1.194225721784776262, 0.05413385826771626580, -0.4176697321401330321 ) ) ;
#64017 = CARTESIAN_POINT ( 'NONE',  ( -0.2427821522309703550, -0.3162353388693405765, 0.4822834645669290543 ) ) ;
#64018 = CARTESIAN_POINT ( 'NONE',  ( 1.167979002624672580, 0.009842519685039144428, -0.3409548833797004797 ) ) ;
#64020 = CARTESIAN_POINT ( 'NONE',  ( 1.548556430446194954, -0.6046776061558807314, 0.2411417322834647770 ) ) ;
#64019 = FACE_OUTER_BOUND ( 'NONE', #31434, .T. ) ;
#64021 = CARTESIAN_POINT ( 'NONE',  ( 1.476377952755906442, -0.5400638737290844871, 0.3530559997133364547 ) ) ;
#64022 = CARTESIAN_POINT ( 'NONE',  ( 0.6962418744208975774, 2.409604939980833412E-17, -0.3464511005275205946 ) ) ;
#64024 = CONICAL_SURFACE ( 'NONE', #25023, 1.181102362204724310, 0.7853981633974621568 ) ;
#64023 = DIRECTION ( 'NONE',  ( 0.000000000000000000, 0.000000000000000000, 1.000000000000000000 ) ) ;
#64025 = CARTESIAN_POINT ( 'NONE',  ( -0.8070866141732276899, -0.5400638737290844871, 0.3530559997133364547 ) ) ;
#64026 = CARTESIAN_POINT ( 'NONE',  ( -1.157146581871515012E-16, 0.4724409448818898682, -0.4724409448818898127 ) ) ;
#64027 = CARTESIAN_POINT ( 'NONE',  ( 0.3996062992125986590, -0.1070741851644053111, -0.2690288713910760632 ) ) ;
#64028 = ORIENTED_EDGE ( 'NONE', *, *, #55811, .F. ) ;
#64029 = CARTESIAN_POINT ( 'NONE',  ( -0.1246719160104980823, -0.5511811023622048555, -0.09757992244046775898 ) ) ;
#64030 = CARTESIAN_POINT ( 'NONE',  ( 0.3917322834645669549, 0.1049643490035304660, -2.006561679790026531 ) ) ;
#64031 = CARTESIAN_POINT ( 'NONE',  ( 0.7349081364829402885, -0.6046776061558809534, -0.2411417322834644161 ) ) ;
#64032 = EDGE_CURVE ( 'NONE', #44871, #53395, #40836, .T. ) ;
#64033 = CARTESIAN_POINT ( 'NONE',  ( 0.4724409448818898682, 2.892866454678787531E-17, -2.952755905511811108 ) ) ;
#64034 = DIRECTION ( 'NONE',  ( -0.000000000000000000, -1.000000000000000000, -0.000000000000000000 ) ) ;
#64035 = CARTESIAN_POINT ( 'NONE',  ( -0.2493438320209966919, -0.3690944881889763329, 0.3153832671262228327 ) ) ;
#64036 = CARTESIAN_POINT ( 'NONE',  ( 0.4177787735907000366, 0.4110443821404751730, -1.559171609364239375 ) ) ;
#64037 = CARTESIAN_POINT ( 'NONE',  ( 1.391076115485564868, 0.2306618581243847221, -0.2411417322834647770 ) ) ;
#64038 = CARTESIAN_POINT ( 'NONE',  ( 0.8727034120734912248, -0.2845877964562161244, -0.3641732283464567121 ) ) ;
#64039 = CARTESIAN_POINT ( 'NONE',  ( 0.07217847769028949700, -0.3162353388693405765, 0.4822834645669290543 ) ) ;
#64040 = CARTESIAN_POINT ( 'NONE',  ( 0.2867679344610365999, 0.2867679344610365999, -0.8477497130895521593 ) ) ;
#64041 = CARTESIAN_POINT ( 'NONE',  ( -0.9842519685039360366, 0.2952755905511811885, 0.000000000000000000 ) ) ;
#64042 = CARTESIAN_POINT ( 'NONE',  ( -1.292650918635170010, -0.5511811023622046335, 0.09757992244046803654 ) ) ;
#64043 = CARTESIAN_POINT ( 'NONE',  ( -0.5774278215223089816, 0.2306618581243847221, -0.2411417322834647770 ) ) ;
#64044 = DIRECTION ( 'NONE',  ( -0.000000000000000000, -1.000000000000000000, -0.000000000000000000 ) ) ;
#64045 = CARTESIAN_POINT ( 'NONE',  ( 0.1742125984251973736, 0.1742125984251973736, -0.3937007874015748254 ) ) ;
#64046 = VERTEX_POINT ( 'NONE', #52198 ) ;
#64047 = CARTESIAN_POINT ( 'NONE',  ( -0.2867679344610365444, -0.2867679344610367664, -2.103037688485251522 ) ) ;
#64048 = CARTESIAN_POINT ( 'NONE',  ( 0.4002624671916016896, -0.05778040916215522460, 0.4822834645669289988 ) ) ;
#64049 = ORIENTED_EDGE ( 'NONE', *, *, #35375, .T. ) ;
#64050 = CARTESIAN_POINT ( 'NONE',  ( -0.7808398950131225646, -0.05778040916215522460, 0.4822834645669289988 ) ) ;
#64051 = CARTESIAN_POINT ( 'NONE',  ( 1.358267716535433323, -0.5400638737290845981, -0.3530559997133363437 ) ) ;
#64052 = EDGE_CURVE ( 'NONE', #5951, #54436, #22801, .T. ) ;
#64053 = CARTESIAN_POINT ( 'NONE',  ( 0.5314960629921264834, 0.1660481256975883668, -0.3530559997133364547 ) ) ;
#64054 = CARTESIAN_POINT ( 'NONE',  ( -0.1443569553805765515, -0.4281496062992127816, -0.4176697321401328100 ) ) ;
#64055 = CARTESIAN_POINT ( 'NONE',  ( 0.3392501089628018329, 0.1958661417322835607, -1.318241469816273215 ) ) ;
#64056 = CARTESIAN_POINT ( 'NONE',  ( -0.7874015748031489847, -0.1870078740157479769, 0.4822834645669291653 ) ) ;
#64057 = CARTESIAN_POINT ( 'NONE',  ( -0.3412073490813641308, 0.2306618581243847221, -0.2411417322834647770 ) ) ;
#64058 = EDGE_CURVE ( 'NONE', #45287, #27710, #65276, .T. ) ;
#64059 = CARTESIAN_POINT ( 'NONE',  ( -0.1181102362204717315, -0.5511811023622047445, 6.969142054262312111E-17 ) ) ;
#64060 = CARTESIAN_POINT ( 'NONE',  ( -0.02500110683994623273, 0.3941128856533804847, 9.485496803828530434E-13 ) ) ;
#64061 = CARTESIAN_POINT ( 'NONE',  ( 0.06561679790026316017, 0.05413385826771626580, -0.4176697321401330321 ) ) ;
#64062 = CARTESIAN_POINT ( 'NONE',  ( -1.220472440944882386, 0.000000000000000000, -0.3464511005275204836 ) ) ;
#64063 = CARTESIAN_POINT ( 'NONE',  ( 0.9448818897637802916, -0.1870078740157479769, 0.4822834645669291653 ) ) ;
#64064 = CARTESIAN_POINT ( 'NONE',  ( 0.4855643044619428750, 0.009842519685039463617, 0.3409548833797002576 ) ) ;
#64065 = ORIENTED_EDGE ( 'NONE', *, *, #32224, .T. ) ;
#64066 = ORIENTED_EDGE ( 'NONE', *, *, #48987, .T. ) ;
#64067 = CONICAL_SURFACE ( 'NONE', #70805, 3.444881889763779625, 0.7853981633974500554 ) ;
#64068 = CARTESIAN_POINT ( 'NONE',  ( 0.2427821522309719648, -0.05778040916215522460, 0.4822834645669289988 ) ) ;
#64069 = CARTESIAN_POINT ( 'NONE',  ( -0.3805774278215216522, -0.3690944881889765550, -0.3153832671262227771 ) ) ;
#64070 = VECTOR ( 'NONE', #59809, 39.37007874015748143 ) ;
#64071 = AXIS2_PLACEMENT_3D ( 'NONE', #17069, #23768, #60417 ) ;
#64073 = CARTESIAN_POINT ( 'NONE',  ( -0.3458507752293906723, -0.3458507752293910609, -0.3740157480314960092 ) ) ;
#64072 = CARTESIAN_POINT ( 'NONE',  ( 1.240157480314961314, 0.07958543189024071263, -0.2665933059059888421 ) ) ;
#64074 = CARTESIAN_POINT ( 'NONE',  ( -0.1958661417322834220, -0.3392501089628018884, -1.095144356955380704 ) ) ;
#64075 = CARTESIAN_POINT ( 'NONE',  ( 0.1265901696524989462, 0.4724409448818897572, -0.2276902887139107545 ) ) ;
#64076 = CARTESIAN_POINT ( 'NONE',  ( 1.437007874015748810, -0.4536011799217368745, -0.2665933059059886201 ) ) ;
#64077 = CARTESIAN_POINT ( 'NONE',  ( -1.463254593175852492, 0.2952755905511811885, 0.1292274648535926551 ) ) ;
#64078 = CARTESIAN_POINT ( 'NONE',  ( -0.3996062992125985480, -7.340648628747423112E-17, -2.793307086614173151 ) ) ;
#64079 = PRODUCT_DEFINITION_SHAPE ( 'NONE', 'NONE',  #83327 ) ;
#64080 = CARTESIAN_POINT ( 'NONE',  ( 0.1115485564304467270, -0.6692913385826773087, -0.1292274648535924053 ) ) ;
#64081 = CARTESIAN_POINT ( 'NONE',  ( -1.391076115485563314, -0.6046776061558809534, -0.2411417322834644161 ) ) ;
#64082 = CARTESIAN_POINT ( 'NONE',  ( -1.010498687664041384, -0.4281496062992127816, -0.4176697321401328100 ) ) ;
#64083 = CARTESIAN_POINT ( 'NONE',  ( 0.3871391076115492380, -0.05778040916215560624, -0.4822834645669293319 ) ) ;
#64084 = CARTESIAN_POINT ( 'NONE',  ( -9.674558042662122972E-17, 0.3949938075777409963, -0.2342519685039370914 ) ) ;
#64085 = CARTESIAN_POINT ( 'NONE',  ( -1.555118110236219930, -0.4536011799217368745, -0.2665933059059886201 ) ) ;
#64086 = CARTESIAN_POINT ( 'NONE',  ( 0.9120734908136489683, -0.6692913385826771977, 0.1292274648535927661 ) ) ;
#64087 = CARTESIAN_POINT ( 'NONE',  ( 0.7808398950131241190, -0.08942795157528024563, -0.3641732283464568787 ) ) ;
#64088 = CARTESIAN_POINT ( 'NONE',  ( 0.2151207158954171472, 1.080925587658431608, 0.2276473237265549121 ) ) ;
#64089 = CARTESIAN_POINT ( 'NONE',  ( 0.6233595800524942554, -0.08942795157528024563, -0.3641732283464568787 ) ) ;
#64090 = CARTESIAN_POINT ( 'NONE',  ( -1.456692913385826182, 0.2952755905511811885, 0.000000000000000000 ) ) ;
#64091 = ADVANCED_FACE ( 'NONE', ( #45881 ), #58847, .F. ) ;
#64092 = CARTESIAN_POINT ( 'NONE',  ( 0.1070741851644053388, 0.3996062992125986035, -1.015091863517060267 ) ) ;
#64093 = CARTESIAN_POINT ( 'NONE',  ( 1.259842519685040019, -0.1870078740157480879, -0.4822834645669291653 ) ) ;
#64094 = CARTESIAN_POINT ( 'NONE',  ( 0.3917322834645670104, -0.1049643490035303411, -0.2611548556430445256 ) ) ;
#64096 = CARTESIAN_POINT ( 'NONE',  ( -0.4567021909596216678, 1.408136488465067782, 2.130977159290117662 ) ) ;
#64095 = CARTESIAN_POINT ( 'NONE',  ( 0.6233595800524942554, -0.05778040916215560624, -0.4822834645669293319 ) ) ;
#64097 = CARTESIAN_POINT ( 'NONE',  ( -1.528871391076114250, 0.1771653543307087075, -0.09757992244046823083 ) ) ;
#64098 = CARTESIAN_POINT ( 'NONE',  ( 0.1115485564304470323, 0.2952755905511811885, 0.1292274648535926551 ) ) ;
#64099 = CARTESIAN_POINT ( 'NONE',  ( 0.4593175853018379162, -0.3690944881889763329, 0.3153832671262228327 ) ) ;
#64100 = EDGE_CURVE ( 'NONE', #68995, #67810, #80389, .T. ) ;
#64101 = CARTESIAN_POINT ( 'NONE',  ( 1.076115485564305141, 0.2306618581243847221, -0.2411417322834647770 ) ) ;
#64102 = FACE_OUTER_BOUND ( 'NONE', #34151, .T. ) ;
#64103 = CARTESIAN_POINT ( 'NONE',  ( -0.3149606299212590610, -0.1870078740157479769, 0.3641732283464567677 ) ) ;
#64104 = CARTESIAN_POINT ( 'NONE',  ( -0.6364829396325453192, -0.3162353388693405765, 0.4822834645669290543 ) ) ;
#64105 = CARTESIAN_POINT ( 'NONE',  ( -1.620734908136482577, 0.1771653543307087630, 0.09757992244046791164 ) ) ;
#64106 = CARTESIAN_POINT ( 'NONE',  ( -1.207349081364828880, 0.2306618581243847221, -0.2411417322834647770 ) ) ;
#64107 = CARTESIAN_POINT ( 'NONE',  ( 1.017060367454068803, -0.3162353388693405765, 0.4822834645669290543 ) ) ;
#64108 = CARTESIAN_POINT ( 'NONE',  ( 0.3917322834645670659, 2.398668435337828261E-17, -0.9022502869104481737 ) ) ;
#64109 = CARTESIAN_POINT ( 'NONE',  ( -1.240157480314959759, -0.4536011799217368745, -0.2665933059059886201 ) ) ;
#64110 = ADVANCED_FACE ( 'NONE', ( #39587 ), #15861, .F. ) ;
#64111 = CARTESIAN_POINT ( 'NONE',  ( 2.554262525012303442, 1.554943921348592717, 0.4744094488188975722 ) ) ;
#64112 = CARTESIAN_POINT ( 'NONE',  ( 0.8727034120734912248, -0.3162353388693409650, -0.4822834645669289433 ) ) ;
#64113 = CARTESIAN_POINT ( 'NONE',  ( 0.3458507752293908943, -0.3458507752293908943, -2.537401574803149984 ) ) ;
#64114 = CARTESIAN_POINT ( 'NONE',  ( -1.660104986876639543, -0.05778040916215560624, -0.4822834645669293319 ) ) ;
#64115 = CARTESIAN_POINT ( 'NONE',  ( -1.437007874015747477, 0.07958543189024071263, -0.2665933059059888421 ) ) ;
#64116 = CARTESIAN_POINT ( 'NONE',  ( -0.8267716535433065062, -0.5511811023622047445, 6.969142054262312111E-17 ) ) ;
#64117 = CARTESIAN_POINT ( 'NONE',  ( 1.660104986876641320, -0.08942795157527998196, 0.3641732283464567121 ) ) ;
#64118 = CARTESIAN_POINT ( 'NONE',  ( -0.4330708661417315697, -0.6692913385826771977, 8.415575281601705876E-17 ) ) ;
#64119 = CARTESIAN_POINT ( 'NONE',  ( -0.4658792650918627265, -0.2845877964562161244, -0.3641732283464567121 ) ) ;
#64120 = CARTESIAN_POINT ( 'NONE',  ( -1.430446194225721390, -0.3690944881889763329, 0.3153832671262228327 ) ) ;
#64121 = CARTESIAN_POINT ( 'NONE',  ( 0.9645669291338588858, 0.07958543189024085140, 0.2665933059059887866 ) ) ;
#64122 = CARTESIAN_POINT ( 'NONE',  ( 0.4265091863517067594, 0.2952755905511811885, 0.1292274648535926551 ) ) ;
#64123 = CARTESIAN_POINT ( 'NONE',  ( 0.1968503937007881344, -0.5511811023622047445, 6.969142054262312111E-17 ) ) ;
#64124 = CARTESIAN_POINT ( 'NONE',  ( 0.3412073490813655186, -0.6046776061558809534, -0.2411417322834644161 ) ) ;
#64125 = CARTESIAN_POINT ( 'NONE',  ( 0.5643044619422579178, -0.3690944881889765550, -0.3153832671262227771 ) ) ;
#64127 = CARTESIAN_POINT ( 'NONE',  ( -1.541994750656167090, -0.6692913385826773087, -0.1292274648535924053 ) ) ;
#64126 = AXIS2_PLACEMENT_3D ( 'NONE', #67470, #9804, #35476 ) ;
#64128 = CARTESIAN_POINT ( 'NONE',  ( -1.482939632545930975, 0.05413385826771666132, 0.4176697321401328100 ) ) ;
#64129 = CARTESIAN_POINT ( 'NONE',  ( -0.3937007874015740483, -0.1870078740157480879, -0.4822834645669291653 ) ) ;
#64130 = AXIS2_PLACEMENT_3D ( 'NONE', #21865, #73648, #22697 ) ;
#64131 = CARTESIAN_POINT ( 'NONE',  ( -0.1070741851644051862, -0.3996062992125986590, -0.3871391076115485719 ) ) ;
#64132 = CARTESIAN_POINT ( 'NONE',  ( -0.3996062992125984925, -0.1070741851644056858, -2.484908136482939955 ) ) ;
#64133 = CARTESIAN_POINT ( 'NONE',  ( 0.4396325459317590445, -0.6692913385826771977, 0.1292274648535927661 ) ) ;
#64134 = CARTESIAN_POINT ( 'NONE',  ( 1.062992125984252745, -0.5511811023622047445, 6.969142054262312111E-17 ) ) ;
#64135 =( GEOMETRIC_REPRESENTATION_CONTEXT ( 3 ) GLOBAL_UNCERTAINTY_ASSIGNED_CONTEXT ( ( #15894 ) ) GLOBAL_UNIT_ASSIGNED_CONTEXT ( ( #28354, #23279, #80143 ) ) REPRESENTATION_CONTEXT ( 'NONE', 'WORKASPACE' ) );
#64136 = CIRCLE ( 'NONE', #49350, 1.220472440944881942 ) ;
#64137 = CARTESIAN_POINT ( 'NONE',  ( -0.4855643044619415427, 0.05413385826771626580, -0.4176697321401330321 ) ) ;
#64138 = CARTESIAN_POINT ( 'NONE',  ( 0.3543307086614179147, 0.2952755905511811885, 0.000000000000000000 ) ) ;
#64139 = CARTESIAN_POINT ( 'NONE',  ( -0.2925321140481930704, -0.2925321140481933480, -2.263779527559055094 ) ) ;
#64140 = CARTESIAN_POINT ( 'NONE',  ( 0.3420746716998659953, 0.1974969037888705536, -2.020997375328084100 ) ) ;
#64141 = CARTESIAN_POINT ( 'NONE',  ( 0.1998031496062994405, -0.3460692066303958092, -2.926509186351706315 ) ) ;
#64142 = DIRECTION ( 'NONE',  ( 1.049727191138616477E-16, -0.5150380749100564870, 0.8571673007021107793 ) ) ;
#64143 = CARTESIAN_POINT ( 'NONE',  ( -0.3917322834645669549, -0.1049643490035306603, -0.9829396325459317518 ) ) ;
#64144 = CARTESIAN_POINT ( 'NONE',  ( -0.8398950131233589023, -0.5023911411419708095, -0.1820866141732282451 ) ) ;
#64145 = CARTESIAN_POINT ( 'NONE',  ( -1.154855643044618851, -0.6046776061558809534, -0.2411417322834644161 ) ) ;
#64146 = CARTESIAN_POINT ( 'NONE',  ( 0.3949938075777408852, 0.1058382717557500435, -2.721128608923885306 ) ) ;
#64147 = CARTESIAN_POINT ( 'NONE',  ( 1.056430446194226658, 0.2952755905511811885, 0.1292274648535926551 ) ) ;
#64148 = CARTESIAN_POINT ( 'NONE',  ( 1.246719160104987623, -0.4281496062992124485, 0.4176697321401328655 ) ) ;
#64149 = CARTESIAN_POINT ( 'NONE',  ( 0.5708661417322841158, -0.5400638737290845981, -0.3530559997133363437 ) ) ;
#64150 = CARTESIAN_POINT ( 'NONE',  ( -0.2362204724409451284, 0.4091458600556402425, -2.847769028871391050 ) ) ;
#64151 = CARTESIAN_POINT ( 'NONE',  ( 4.893765752498283924E-17, -0.3996062992125986035, -2.125984251968504157 ) ) ;
#64152 = CARTESIAN_POINT ( 'NONE',  ( -0.3917322834645670104, -0.1049643490035307020, -0.9875521241807894146 ) ) ;
#64153 = CARTESIAN_POINT ( 'NONE',  ( 1.660104986876641320, -0.05778040916215522460, 0.4822834645669289988 ) ) ;
#64154 = CARTESIAN_POINT ( 'NONE',  ( 0.5249343832021003964, 0.2306618581243847221, -0.2411417322834647770 ) ) ;
#64155 = EDGE_CURVE ( 'NONE', #19415, #66357, #26955, .T. ) ;
#64156 = CARTESIAN_POINT ( 'NONE',  ( 0.1181102362204730916, -0.6692913385826771977, 8.415575281601705876E-17 ) ) ;
#64157 = CARTESIAN_POINT ( 'NONE',  ( 0.6364829396325465405, -0.08942795157527998196, 0.3641732283464567121 ) ) ;
#64158 = CARTESIAN_POINT ( 'NONE',  ( 1.174540682414699111, -0.3162353388693405765, 0.4822834645669290543 ) ) ;
#64159 = CARTESIAN_POINT ( 'NONE',  ( -0.3392501089628019995, 0.1958661417322832277, -0.2683727034120735877 ) ) ;
#64160 = CARTESIAN_POINT ( 'NONE',  ( 0.3018372703412079971, -0.4281496062992124485, 0.4176697321401328655 ) ) ;
#64161 = CARTESIAN_POINT ( 'NONE',  ( 0.9645669291338591078, -0.5400638737290845981, -0.3530559997133363437 ) ) ;
#64162 = CARTESIAN_POINT ( 'NONE',  ( 0.3018372703412079971, 0.05413385826771626580, -0.4176697321401330321 ) ) ;
#64163 = CARTESIAN_POINT ( 'NONE',  ( 1.187664041994751285, -0.08942795157527998196, 0.3641732283464567121 ) ) ;
#64164 = CARTESIAN_POINT ( 'NONE',  ( -0.9908136482939626788, -0.6692913385826773087, -0.1292274648535924053 ) ) ;
#64165 = CARTESIAN_POINT ( 'NONE',  ( -0.9645669291338575535, -0.5400638737290844871, 0.3530559997133364547 ) ) ;
#64166 = CARTESIAN_POINT ( 'NONE',  ( 1.338582677165355062, -0.1870078740157480879, -0.4822834645669291653 ) ) ;
#64167 = CARTESIAN_POINT ( 'NONE',  ( 0.2867679344610365999, -0.2867679344610365444, -0.6555118110236222151 ) ) ;
#64168 = CARTESIAN_POINT ( 'NONE',  ( 0.3917322834645670104, -0.1049643490035303411, -1.678477690288713964 ) ) ;
#64169 = CARTESIAN_POINT ( 'NONE',  ( 0.1049643490035303689, 0.3917322834645670104, -2.820209973753280419 ) ) ;
#64170 = ORIENTED_EDGE ( 'NONE', *, *, #14676, .T. ) ;
#64171 = CARTESIAN_POINT ( 'NONE',  ( -0.1998031496062994683, 0.3460692066303958092, -0.01312335958005251234 ) ) ;
#64172 = VERTEX_POINT ( 'NONE', #72002 ) ;
#64173 = CARTESIAN_POINT ( 'NONE',  ( 1.397637795275591177, 0.1660481256975883668, -0.3530559997133364547 ) ) ;
#64174 = CARTESIAN_POINT ( 'NONE',  ( 0.8792650918635177559, -0.3690944881889765550, -0.3153832671262227771 ) ) ;
#64175 = CARTESIAN_POINT ( 'NONE',  ( -9.787531504996567848E-17, 0.3996062992125986035, -1.417322834645669216 ) ) ;
#64176 = CARTESIAN_POINT ( 'NONE',  ( 1.246719160104987623, -0.004921259842519870586, -0.3153832671262229437 ) ) ;
#64177 = CARTESIAN_POINT ( 'NONE',  ( 0.6188235755478038724, 2.084810923686589862E-15, -0.3954974714151459625 ) ) ;
#64178 = CARTESIAN_POINT ( 'NONE',  ( -0.1340670299283584221, 1.082026165109803317, 2.856419976764481117 ) ) ;
#64179 = DIRECTION ( 'NONE',  ( 0.000000000000000000, 0.000000000000000000, -1.000000000000000000 ) ) ;
#64180 = CARTESIAN_POINT ( 'NONE',  ( -0.3392501089628017219, -0.1958661417322836718, -0.7670603674540683592 ) ) ;
#64181 = CARTESIAN_POINT ( 'NONE',  ( -0.7808398950131222316, -0.2845877964562161244, -0.3641732283464567121 ) ) ;
#64182 = CARTESIAN_POINT ( 'NONE',  ( -1.430446194225721390, -0.3690944881889763329, 0.3153832671262228327 ) ) ;
#64183 = CARTESIAN_POINT ( 'NONE',  ( -1.227034120734907141, -0.6692913385826773087, -0.1292274648535924053 ) ) ;
#64184 = CARTESIAN_POINT ( 'NONE',  ( -0.04593175853018302557, -0.6692913385826773087, -0.1292274648535924053 ) ) ;
#64185 = CARTESIAN_POINT ( 'NONE',  ( 1.476377952755906220, 0.1660481256975883668, -0.3530559997133364547 ) ) ;
#64186 = VERTEX_POINT ( 'NONE', #27795 ) ;
#64187 = CARTESIAN_POINT ( 'NONE',  ( -1.128608923884513837, 0.1539470093639521697, -0.1968503937007875793 ) ) ;
#64188 = CARTESIAN_POINT ( 'NONE',  ( 0.4091458600556404646, -0.2362204724409448231, -1.994750656167979086 ) ) ;
#64189 = LINE ( 'NONE', #6524, #47863 ) ;
#64190 = DIRECTION ( 'NONE',  ( 0.000000000000000000, 0.000000000000000000, 1.000000000000000000 ) ) ;
#64191 = CARTESIAN_POINT ( 'NONE',  ( -0.8005249343832011588, -0.004921259842519870586, -0.3153832671262229437 ) ) ;
#64192 = CARTESIAN_POINT ( 'NONE',  ( -1.181102362204723644, -0.1870078740157479769, 0.4822834645669291653 ) ) ;
#64193 = CARTESIAN_POINT ( 'NONE',  ( 0.8727034120734913358, -0.05778040916215522460, 0.4822834645669289988 ) ) ;
#64194 = CONICAL_SURFACE ( 'NONE', #76282, 1.220472440944881942, 0.7853981633974621568 ) ;
#64195 = ORIENTED_EDGE ( 'NONE', *, *, #22408, .F. ) ;
#64197 = CARTESIAN_POINT ( 'NONE',  ( -0.3458507752293906723, -0.3458507752293910609, -2.655511811023621771 ) ) ;
#64196 = DIRECTION ( 'NONE',  ( -1.000000000000000000, 0.000000000000000000, 0.000000000000000000 ) ) ;
#64198 = CARTESIAN_POINT ( 'NONE',  ( 1.017060367454068803, -0.3162353388693405765, 0.4822834645669290543 ) ) ;
#64199 = CARTESIAN_POINT ( 'NONE',  ( -1.312335958005248715, -0.6046776061558809534, -0.2411417322834644161 ) ) ;
#64200 = CARTESIAN_POINT ( 'NONE',  ( -0.1958661417322836440, 0.3392501089628016664, -0.7230777970790532860 ) ) ;
#64201 = CARTESIAN_POINT ( 'NONE',  ( -0.5118110236220466680, -0.5511811023622047445, 6.969142054262312111E-17 ) ) ;
#64202 = CARTESIAN_POINT ( 'NONE',  ( -0.3917322834645669549, -0.1049643490035306603, -0.9179790026246720247 ) ) ;
#64203 = CARTESIAN_POINT ( 'NONE',  ( -0.6233595800524928121, -0.2845877964562161244, -0.3641732283464567121 ) ) ;
#64204 = CARTESIAN_POINT ( 'NONE',  ( 0.2362204724409456558, -0.1870078740157480601, -0.3641732283464567677 ) ) ;
#64205 = CARTESIAN_POINT ( 'NONE',  ( 0.1049868766404206816, -0.6046776061558809534, -0.2411417322834644161 ) ) ;
#64206 = CARTESIAN_POINT ( 'NONE',  ( -1.338582677165353729, -0.1870078740157479769, 0.3641732283464567677 ) ) ;
#64207 = CARTESIAN_POINT ( 'NONE',  ( -0.1958661417322836718, 0.3392501089628017219, -2.839895013123359568 ) ) ;
#64208 = CARTESIAN_POINT ( 'NONE',  ( 1.049868766404200127, -0.6046776061558809534, -0.2411417322834644161 ) ) ;
#64209 = CARTESIAN_POINT ( 'NONE',  ( -1.463254593175852492, 0.2952755905511811885, 0.1292274648535926551 ) ) ;
#64210 = CARTESIAN_POINT ( 'NONE',  ( -0.3458507752293906723, -0.3458507752293910609, -1.238188976377952999 ) ) ;
#64211 = CARTESIAN_POINT ( 'NONE',  ( -0.5380577427821514602, -0.4281496062992127816, -0.4176697321401328100 ) ) ;
#64212 = CARTESIAN_POINT ( 'NONE',  ( -0.8005249343832011588, 0.05413385826771626580, -0.4176697321401330321 ) ) ;
#64213 = CARTESIAN_POINT ( 'NONE',  ( 0.6299212598425204535, -0.1870078740157480601, -0.3641732283464567677 ) ) ;
#64214 = CARTESIAN_POINT ( 'NONE',  ( -0.2624671916010490880, 0.1283753931104746893, -0.1820866141732285504 ) ) ;
#64215 = CARTESIAN_POINT ( 'NONE',  ( -0.4396325459317579898, 0.2952755905511811885, 0.1292274648535926551 ) ) ;
#64216 = CARTESIAN_POINT ( 'NONE',  ( -1.345144356955379816, -0.3162353388693405765, 0.4822834645669290543 ) ) ;
#64217 = DIRECTION ( 'NONE',  ( 0.000000000000000000, 0.000000000000000000, -1.000000000000000000 ) ) ;
#64218 = CARTESIAN_POINT ( 'NONE',  ( 1.187664041994751285, -0.08942795157527998196, 0.3641732283464567121 ) ) ;
#64219 = CARTESIAN_POINT ( 'NONE',  ( -0.09842519685039295696, -0.5400638737290844871, 0.3530559997133364547 ) ) ;
#64220 = CARTESIAN_POINT ( 'NONE',  ( -1.528871391076114250, 0.2952755905511810774, -0.1292274648535930714 ) ) ;
#64221 = ORIENTED_EDGE ( 'NONE', *, *, #43859, .T. ) ;
#64222 = CARTESIAN_POINT ( 'NONE',  ( 0.1998031496062994128, -0.3460692066303957537, -2.215879265091863726 ) ) ;
#64223 = CARTESIAN_POINT ( 'NONE',  ( -0.8267716535433065062, 0.1771653543307087630, 0.000000000000000000 ) ) ;
#64224 = CARTESIAN_POINT ( 'NONE',  ( 0.9448818897637802916, -0.1870078740157479769, 0.4822834645669291653 ) ) ;
#64225 = CARTESIAN_POINT ( 'NONE',  ( -1.141732283464566011, -0.5511811023622047445, 6.969142054262312111E-17 ) ) ;
#64226 = CARTESIAN_POINT ( 'NONE',  ( -0.3460692066303960313, 0.1998031496062989965, -1.362860892388451539 ) ) ;
#64227 = CARTESIAN_POINT ( 'NONE',  ( -0.8398950131233589023, -0.6046776061558809534, -0.2411417322834644161 ) ) ;
#64228 = CARTESIAN_POINT ( 'NONE',  ( 0.7217847769028878924, 0.05413385826771666132, 0.4176697321401328100 ) ) ;
#64229 = CARTESIAN_POINT ( 'NONE',  ( 0.5708661417322842269, 0.1660481256975885056, 0.3530559997133364547 ) ) ;
#64230 = CARTESIAN_POINT ( 'NONE',  ( 1.430446194225722500, 0.05413385826771666132, 0.4176697321401328100 ) ) ;
#64231 = CARTESIAN_POINT ( 'NONE',  ( -1.515748031496062076, 0.07958543189024071263, -0.2665933059059888421 ) ) ;
#64232 = CARTESIAN_POINT ( 'NONE',  ( -0.1070741851644057135, 0.3996062992125984925, -0.7132545931758530466 ) ) ;
#64233 = CARTESIAN_POINT ( 'NONE',  ( 0.3996062992125986035, 2.446882876249141962E-17, -0.7480314960629921295 ) ) ;
#64234 = CARTESIAN_POINT ( 'NONE',  ( 0.3949938075777409963, 2.418639510665530435E-17, -0.1181102362204724948 ) ) ;
#64235 = CARTESIAN_POINT ( 'NONE',  ( 1.024278008493452630, 1.664615899758172368, 0.4581426849250264111 ) ) ;
#64236 = CARTESIAN_POINT ( 'NONE',  ( 1.056430446194226658, 0.1771653543307087630, 0.09757992244046791164 ) ) ;
#64237 = CARTESIAN_POINT ( 'NONE',  ( 0.4002624671916016896, -0.2845877964562161244, -0.3641732283464567121 ) ) ;
#64238 = CARTESIAN_POINT ( 'NONE',  ( 0.2755905511811031494, -0.6692913385826771977, 8.415575281601705876E-17 ) ) ;
#64239 = CARTESIAN_POINT ( 'NONE',  ( 1.174540682414699111, -0.05778040916215560624, -0.4822834645669293319 ) ) ;
#64240 = CARTESIAN_POINT ( 'NONE',  ( -9.674558042662122972E-17, 0.3949938075777409963, -1.179133858267716661 ) ) ;
#64241 = CARTESIAN_POINT ( 'NONE',  ( 0.3740157480314966754, -0.4536011799217367080, 0.2665933059059888421 ) ) ;
#64242 = CARTESIAN_POINT ( 'NONE',  ( -0.8267716535433065062, 0.2952755905511811885, 0.000000000000000000 ) ) ;
#64243 = CARTESIAN_POINT ( 'NONE',  ( -1.417322834645668772, -0.1870078740157480879, -0.4822834645669291653 ) ) ;
#64244 = CARTESIAN_POINT ( 'NONE',  ( 0.9383202099737538715, -0.05778040916215560624, -0.4822834645669293319 ) ) ;
#64245 = CARTESIAN_POINT ( 'NONE',  ( 5.785732909357575061E-17, -0.4724409448818898682, -1.496062992125984259 ) ) ;
#64246 = AXIS2_PLACEMENT_3D ( 'NONE', #13503, #34111, #26545 ) ;
#64247 = CARTESIAN_POINT ( 'NONE',  ( -0.3996062992125986590, 0.1070741851644051862, -2.552493438320209140 ) ) ;
#64248 = ORIENTED_EDGE ( 'NONE', *, *, #52608, .T. ) ;
#64249 = EDGE_LOOP ( 'NONE', ( #27110, #66763, #54910, #3074, #51608, #22150, #39421 ) ) ;
#64250 = CARTESIAN_POINT ( 'NONE',  ( -1.174540682414697335, -0.3162353388693409650, -0.4822834645669289433 ) ) ;
#64251 = CARTESIAN_POINT ( 'NONE',  ( -0.6561679790026240244, 0.2306618581243847221, -0.2411417322834647770 ) ) ;
#64253 = CARTESIAN_POINT ( 'NONE',  ( -0.7939632545931750718, -0.05778040916215560624, -0.4822834645669293319 ) ) ;
#64252 = CARTESIAN_POINT ( 'NONE',  ( -0.7939632545931750718, -0.08942795157528024563, -0.3641732283464568787 ) ) ;
#64254 = CARTESIAN_POINT ( 'NONE',  ( -0.1049643490035306742, 0.3917322834645668994, -1.976358636974066663 ) ) ;
#64255 = CARTESIAN_POINT ( 'NONE',  ( 0.1970133122064497144, -0.2199809220305531665, 0.1374248322900813446 ) ) ;
#64256 = CARTESIAN_POINT ( 'NONE',  ( 1.692913385826772421, 0.2952755905511811885, 0.000000000000000000 ) ) ;
#64257 = CARTESIAN_POINT ( 'NONE',  ( -1.135170603674539924, -0.6692913385826771977, 0.1292274648535927661 ) ) ;
#64258 = CARTESIAN_POINT ( 'NONE',  ( 0.4593175853018379162, -0.4281496062992124485, 0.4176697321401328655 ) ) ;
#64259 = CARTESIAN_POINT ( 'NONE',  ( -0.6955380577427815458, 0.05413385826771666132, 0.4176697321401328100 ) ) ;
#64260 = CARTESIAN_POINT ( 'NONE',  ( 0.3917322834645670104, -0.1049643490035303411, -1.520997375328083656 ) ) ;
#64261 = CARTESIAN_POINT ( 'NONE',  ( -0.7217847769028863381, -0.3690944881889763329, 0.3153832671262228327 ) ) ;
#64262 = VERTEX_POINT ( 'NONE', #42886 ) ;
#64263 = CARTESIAN_POINT ( 'NONE',  ( -0.1058382717557497937, -0.3949938075777411628, -1.804461942257217899 ) ) ;
#64264 = ORIENTED_EDGE ( 'NONE', *, *, #23392, .T. ) ;
#64265 = CARTESIAN_POINT ( 'NONE',  ( -1.515748031496062076, 0.07958543189024071263, -0.2665933059059888421 ) ) ;
#64266 = CARTESIAN_POINT ( 'NONE',  ( -1.220472440944881054, -0.6692913385826771977, 8.415575281601705876E-17 ) ) ;
#64267 = CARTESIAN_POINT ( 'NONE',  ( -0.9055118110236215490, -0.6692913385826771977, 8.415575281601705876E-17 ) ) ;
#64268 = CARTESIAN_POINT ( 'NONE',  ( 0.1070741851644054915, -0.3996062992125986035, -0.08530183727034119923 ) ) ;
#64269 = CARTESIAN_POINT ( 'NONE',  ( -1.148293963254592542, -0.6692913385826773087, -0.1292274648535924053 ) ) ;
#64270 = CARTESIAN_POINT ( 'NONE',  ( -1.345144356955379816, -0.05778040916215560624, -0.4822834645669293319 ) ) ;
#64271 = CARTESIAN_POINT ( 'NONE',  ( -0.8464566929133852113, 0.1660481256975885056, 0.3530559997133364547 ) ) ;
#64272 = CARTESIAN_POINT ( 'NONE',  ( 0.3543307086614181922, -0.5511811023622047445, 6.969142054262312111E-17 ) ) ;
#64273 = CARTESIAN_POINT ( 'NONE',  ( 1.614173228346456712, 0.4410134679336843999, 0.1372047244094478646 ) ) ;
#64274 = CARTESIAN_POINT ( 'NONE',  ( 4.797336870675656522E-17, -0.3917322834645670104, -0.3208661417322835607 ) ) ;
#64275 = CARTESIAN_POINT ( 'NONE',  ( -0.4461942257217840213, 0.1283753931104748280, 0.1820866141732283561 ) ) ;
#64276 = CARTESIAN_POINT ( 'NONE',  ( -0.6692913385826764205, 0.2952755905511811885, 0.000000000000000000 ) ) ;
#64277 = CARTESIAN_POINT ( 'NONE',  ( 1.207349081364829990, -0.6046776061558809534, -0.2411417322834644161 ) ) ;
#64278 = CARTESIAN_POINT ( 'NONE',  ( -0.6299212598425188991, -0.1870078740157480879, -0.4822834645669291653 ) ) ;
#64279 = EDGE_LOOP ( 'NONE', ( #60616, #15202, #27626, #5268, #41489, #80417, #82087, #33294, #26709, #16731, #28244, #67359, #10770, #57021, #13267, #50336, #71184, #9522, #31109, #74032, #28952, #59609, #58462, #5348, #62984, #73511, #49660, #18207, #75735, #77842 ) ) ;
#64280 = EDGE_LOOP ( 'NONE', ( #12281, #29598, #30422, #27833 ) ) ;
#64281 = CARTESIAN_POINT ( 'NONE',  ( -0.3460692066303957537, -0.1998031496062994405, -2.019028871391076230 ) ) ;
#64282 = CARTESIAN_POINT ( 'NONE',  ( -1.089238845144356427, -0.4281496062992127816, -0.4176697321401328100 ) ) ;
#64283 = CARTESIAN_POINT ( 'NONE',  ( 1.181102362204724976, -0.1870078740157480879, -0.4822834645669291653 ) ) ;
#64284 = CARTESIAN_POINT ( 'NONE',  ( -1.036745406824146176, -0.004921259842519870586, -0.3153832671262229437 ) ) ;
#64285 = CARTESIAN_POINT ( 'NONE',  ( -1.594488188976377563, -0.5400638737290844871, 0.3530559997133364547 ) ) ;
#64286 = CARTESIAN_POINT ( 'NONE',  ( -0.3458507752293909498, 0.3458507752293907833, -0.8070866141732284671 ) ) ;
#64287 = CARTESIAN_POINT ( 'NONE',  ( 1.895263394252414857, 1.111778211650222170, 0.2101609992702619945 ) ) ;
#64288 = CARTESIAN_POINT ( 'NONE',  ( 0.3917322834645670104, -0.1049643490035303411, -0.2611548556430445256 ) ) ;
#64289 = CARTESIAN_POINT ( 'NONE',  ( -0.1049643490035301885, -0.3917322834645671215, -2.046587926509185973 ) ) ;
#64290 = CARTESIAN_POINT ( 'NONE',  ( 0.2952755905511819101, 0.1660481256975883668, -0.3530559997133364547 ) ) ;
#64291 = CARTESIAN_POINT ( 'NONE',  ( -0.9645669291338575535, 0.07958543189024071263, -0.2665933059059888421 ) ) ;
#64292 = CARTESIAN_POINT ( 'NONE',  ( -0.7742782152230965886, 0.05413385826771666132, 0.4176697321401328100 ) ) ;
#64293 = CARTESIAN_POINT ( 'NONE',  ( 0.1265901696524990294, -0.4724409448818896462, -2.681758530183727895 ) ) ;
#64294 = CARTESIAN_POINT ( 'NONE',  ( -1.272965879265091305, -0.4281496062992124485, 0.4176697321401328655 ) ) ;
#64295 = CARTESIAN_POINT ( 'NONE',  ( -0.8530183727034112984, -0.4281496062992127816, -0.4176697321401328100 ) ) ;
#64296 = CARTESIAN_POINT ( 'NONE',  ( -0.1640419947506555343, -0.3162353388693405765, 0.4822834645669290543 ) ) ;
#64297 = CARTESIAN_POINT ( 'NONE',  ( -0.1974969037888706924, 0.3420746716998658843, -2.609580052493438718 ) ) ;
#64298 = CARTESIAN_POINT ( 'NONE',  ( 0.8530183727034126306, -0.004921259842519870586, -0.3153832671262229437 ) ) ;
#64299 = CARTESIAN_POINT ( 'NONE',  ( -0.6496062992125976043, -0.4536011799217367080, 0.2665933059059888421 ) ) ;
#64300 = CARTESIAN_POINT ( 'NONE',  ( -0.06112347087428735004, 1.066921639274551081, -1.448920818111165021 ) ) ;
#64301 = CARTESIAN_POINT ( 'NONE',  ( 0.5511811023622055217, -0.1870078740157479769, 0.3641732283464567677 ) ) ;
#64302 = CARTESIAN_POINT ( 'NONE',  ( 1.259842519685040019, -0.1870078740157479769, 0.3641732283464567677 ) ) ;
#64303 = CARTESIAN_POINT ( 'NONE',  ( 1.240157480314961314, -0.5400638737290844871, 0.3530559997133364547 ) ) ;
#64304 = CARTESIAN_POINT ( 'NONE',  ( 0.1377952755905518800, 0.07958543189024071263, -0.2665933059059888421 ) ) ;
#64305 = CARTESIAN_POINT ( 'NONE',  ( 0.3392501089628018884, -0.1958661417322834220, -1.356955380577427928 ) ) ;
#64306 = CARTESIAN_POINT ( 'NONE',  ( -0.9645669291338575535, 0.1660481256975883668, -0.3530559997133364547 ) ) ;
#64307 = CARTESIAN_POINT ( 'NONE',  ( 1.286089238845145033, 0.2306618581243848609, 0.2411417322834645549 ) ) ;
#64308 = CARTESIAN_POINT ( 'NONE',  ( -0.1265901696524986964, -0.4724409448818899238, -0.1489501312335958227 ) ) ;
#64309 = CARTESIAN_POINT ( 'NONE',  ( -0.4396325459317577122, -0.5511811023622048555, -0.09757992244046775898 ) ) ;
#64310 = DIRECTION ( 'NONE',  ( -0.000000000000000000, -1.000000000000000000, -0.000000000000000000 ) ) ;
#64311 = CARTESIAN_POINT ( 'NONE',  ( 0.3412073490813655186, -0.6046776061558809534, -0.2411417322834644161 ) ) ;
#64312 = DIRECTION ( 'NONE',  ( 0.000000000000000000, 1.224646799147351482E-16, 1.000000000000000000 ) ) ;
#64313 = CARTESIAN_POINT ( 'NONE',  ( 0.8464566929133865436, 0.07958543189024071263, -0.2665933059059888421 ) ) ;
#64314 = CARTESIAN_POINT ( 'NONE',  ( 0.2165354330708668673, 0.07958543189024071263, -0.2665933059059888421 ) ) ;
#64315 = CARTESIAN_POINT ( 'NONE',  ( -0.01968503937007793844, 0.1660481256975883668, -0.3530559997133364547 ) ) ;
#64316 = CARTESIAN_POINT ( 'NONE',  ( -1.174540682414697335, -0.3162353388693409650, -0.4822834645669289433 ) ) ;
#64317 = CARTESIAN_POINT ( 'NONE',  ( -0.9055118110236215490, -0.5511811023622047445, 6.969142054262312111E-17 ) ) ;
#64318 = CARTESIAN_POINT ( 'NONE',  ( 3.821484228344193657, 2.755905511811024056, -0.5314960629921260393 ) ) ;
#64319 = CARTESIAN_POINT ( 'NONE',  ( -0.5446194225721777693, -0.05778040916215522460, 0.4822834645669289988 ) ) ;
#64320 = CARTESIAN_POINT ( 'NONE',  ( -0.1998031496062991630, -0.3460692066303959202, -1.087270341207349000 ) ) ;
#64321 = CARTESIAN_POINT ( 'NONE',  ( 0.1958661417322834775, 0.3392501089628018884, -2.591207349081364519 ) ) ;
#64322 = CARTESIAN_POINT ( 'NONE',  ( 0.2755905511811031494, -0.5511811023622047445, 6.969142054262312111E-17 ) ) ;
#64323 = CARTESIAN_POINT ( 'NONE',  ( -0.6758530183727028406, 0.2952755905511811885, 0.1292274648535926551 ) ) ;
#64324 = CARTESIAN_POINT ( 'NONE',  ( -1.220472440944881054, -0.6692913385826771977, 8.415575281601705876E-17 ) ) ;
#64325 = CARTESIAN_POINT ( 'NONE',  ( -1.345144356955379816, -0.2845877964562159024, 0.3641732283464567677 ) ) ;
#64326 = CARTESIAN_POINT ( 'NONE',  ( 1.633858267716535639, -0.5400638737290844871, 0.3530559997133364547 ) ) ;
#64327 = CARTESIAN_POINT ( 'NONE',  ( -0.4461942257217840213, -0.6046776061558809534, -0.2411417322834644161 ) ) ;
#64328 = CARTESIAN_POINT ( 'NONE',  ( -0.7545931758530176614, -0.5511811023622048555, -0.09757992244046775898 ) ) ;
#64329 = CARTESIAN_POINT ( 'NONE',  ( -1.548556430446193399, 0.1283753931104748280, 0.1820866141732283561 ) ) ;
#64330 = CARTESIAN_POINT ( 'NONE',  ( 1.417322834645670104, -0.1870078740157479769, 0.4822834645669291653 ) ) ;
#64331 = FACE_OUTER_BOUND ( 'NONE', #32879, .T. ) ;
#64332 = CARTESIAN_POINT ( 'NONE',  ( -0.3917322834645671770, 0.1049643490035302024, -1.919310654364516200 ) ) ;
#64333 = ORIENTED_EDGE ( 'NONE', *, *, #43698, .T. ) ;
#64334 = CARTESIAN_POINT ( 'NONE',  ( -1.559171609364246924, 0.3937007874015748254, 0.5949441279213820710 ) ) ;
#64335 = CARTESIAN_POINT ( 'NONE',  ( -1.377952755905511140, 0.2952755905511811885, 0.000000000000000000 ) ) ;
#64336 = CARTESIAN_POINT ( 'NONE',  ( -0.8267716535433065062, -0.6692913385826771977, 8.415575281601705876E-17 ) ) ;
#64337 = CARTESIAN_POINT ( 'NONE',  ( -1.561679790026246017, -0.4281496062992127816, -0.4176697321401328100 ) ) ;
#64338 = CARTESIAN_POINT ( 'NONE',  ( -0.3917322834645670104, -7.196005306013484475E-17, -1.856299212598425230 ) ) ;
#64339 = CARTESIAN_POINT ( 'NONE',  ( 1.437007874015748810, -0.4536011799217368745, -0.2665933059059886201 ) ) ;
#64340 = ADVANCED_FACE ( 'NONE', ( #74496 ), #81223, .F. ) ;
#64341 = CARTESIAN_POINT ( 'NONE',  ( 0.4199475065616805614, 0.2306618581243848609, 0.2411417322834645549 ) ) ;
#64342 = CARTESIAN_POINT ( 'NONE',  ( -0.1312335958005241554, -0.6046776061558809534, -0.2411417322834644161 ) ) ;
#64343 = CARTESIAN_POINT ( 'NONE',  ( -0.6962418744208963561, -2.294479370626195693E-15, 0.3464511005275217603 ) ) ;
#64344 = CARTESIAN_POINT ( 'NONE',  ( -0.6415071261929207180, 0.02791078216816347476, -0.4328096321851898631 ) ) ;
#64345 = CARTESIAN_POINT ( 'NONE',  ( 0.8989501312335963501, -0.5511811023622048555, -0.09757992244046775898 ) ) ;
#64346 = CARTESIAN_POINT ( 'NONE',  ( 0.3996062992125986590, -0.1070741851644053111, -1.213910761154855189 ) ) ;
#64347 = VERTEX_POINT ( 'NONE', #28205 ) ;
#64348 = CARTESIAN_POINT ( 'NONE',  ( -0.1958661417322833942, -0.3392501089628018884, 0.09512504117354141087 ) ) ;
#64349 = ORIENTED_EDGE ( 'NONE', *, *, #40447, .T. ) ;
#64350 = CARTESIAN_POINT ( 'NONE',  ( -0.1246719160104980823, 0.2952755905511811885, 0.1292274648535926551 ) ) ;
#64351 = CARTESIAN_POINT ( 'NONE',  ( -0.6496062992125976043, -0.5400638737290844871, 0.3530559997133364547 ) ) ;
#64352 = CARTESIAN_POINT ( 'NONE',  ( -1.456692913385826182, 0.2952755905511811885, 0.000000000000000000 ) ) ;
#64353 = CARTESIAN_POINT ( 'NONE',  ( 0.7217847769028878924, 0.05413385826771666132, 0.4176697321401328100 ) ) ;
#64354 = CARTESIAN_POINT ( 'NONE',  ( 1.633858267716535639, -0.5400638737290844871, 0.3530559997133364547 ) ) ;
#64355 = CARTESIAN_POINT ( 'NONE',  ( 1.391076115485564868, -0.6046776061558807314, 0.2411417322834647770 ) ) ;
#64356 = CARTESIAN_POINT ( 'NONE',  ( -0.5380577427821514602, 0.05413385826771666132, 0.4176697321401328100 ) ) ;
#64357 = CARTESIAN_POINT ( 'NONE',  ( 0.4724409448818904789, -0.1870078740157479769, 0.4822834645669291653 ) ) ;
#64358 = CARTESIAN_POINT ( 'NONE',  ( 1.509186351706037543, -0.4281496062992127816, -0.4176697321401328100 ) ) ;
#64359 = CARTESIAN_POINT ( 'NONE',  ( 1.272965879265092637, 0.05413385826771666132, 0.4176697321401328100 ) ) ;
#64360 = CARTESIAN_POINT ( 'NONE',  ( 1.541994750656168645, 0.2952755905511810774, -0.1292274648535930714 ) ) ;
#64361 = CARTESIAN_POINT ( 'NONE',  ( -0.2559055118110230564, 0.1660481256975883668, -0.3530559997133364547 ) ) ;
#64362 = CARTESIAN_POINT ( 'NONE',  ( -0.1049643490035307020, 0.3917322834645669549, 0.001312335958005295946 ) ) ;
#64363 = CARTESIAN_POINT ( 'NONE',  ( 0.5643044619422579178, -0.004921259842519576551, 0.3153832671262227771 ) ) ;
#64364 = ORIENTED_EDGE ( 'NONE', *, *, #68219, .T. ) ;
#64365 = CARTESIAN_POINT ( 'NONE',  ( -0.2891555358219908833, -0.2891555358219912164, -0.5314960629921261503 ) ) ;
#64366 = ORIENTED_EDGE ( 'NONE', *, *, #4386, .F. ) ;
#64367 = CARTESIAN_POINT ( 'NONE',  ( -0.5052493438320203589, -0.5511811023622046335, 0.09757992244046803654 ) ) ;
#64368 = CARTESIAN_POINT ( 'NONE',  ( -0.4724409448818898682, -8.678599364036362592E-17, -1.218503937007874072 ) ) ;
#64369 = CARTESIAN_POINT ( 'NONE',  ( 0.2755905511811031494, -0.6692913385826771977, 8.415575281601705876E-17 ) ) ;
#64370 = CARTESIAN_POINT ( 'NONE',  ( 0.07217847769028949700, -0.05778040916215560624, -0.4822834645669293319 ) ) ;
#64371 = CARTESIAN_POINT ( 'NONE',  ( -0.9383202099737524282, -0.05778040916215522460, 0.4822834645669289988 ) ) ;
#64372 = CARTESIAN_POINT ( 'NONE',  ( -0.2867679344610365444, -0.2867679344610367664, -1.473116428642731401 ) ) ;
#64373 = CARTESIAN_POINT ( 'NONE',  ( -1.056430446194224881, -0.6692913385826771977, 0.1292274648535927661 ) ) ;
#64374 = DIRECTION ( 'NONE',  ( 0.000000000000000000, 1.000000000000000000, 0.000000000000000000 ) ) ;
#64375 = CARTESIAN_POINT ( 'NONE',  ( 0.8595800524934390507, -0.08942795157528024563, -0.3641732283464568787 ) ) ;
#64376 = CARTESIAN_POINT ( 'NONE',  ( 0.6692913385826778638, -0.6692913385826771977, 8.415575281601705876E-17 ) ) ;
#64377 = CARTESIAN_POINT ( 'NONE',  ( 0.8464566929133866546, -0.5400638737290844871, 0.3530559997133364547 ) ) ;
#64378 = EDGE_CURVE ( 'NONE', #73939, #72992, #62874, .T. ) ;
#64379 = CARTESIAN_POINT ( 'NONE',  ( 0.3460692066303959202, 0.1998031496062993295, -1.076115485564304475 ) ) ;
#64380 = CARTESIAN_POINT ( 'NONE',  ( -1.627296587926508442, -0.6046776061558809534, -0.2411417322834644161 ) ) ;
#64381 = CARTESIAN_POINT ( 'NONE',  ( -0.2925321140481930149, -0.2925321140481933480, -0.9232283464566929387 ) ) ;
#64382 = CARTESIAN_POINT ( 'NONE',  ( 0.1070741851644053388, 0.3996062992125986035, -0.2276902887139107545 ) ) ;
#64383 = CARTESIAN_POINT ( 'NONE',  ( 0.07217847769028949700, -0.05778040916215560624, -0.4822834645669293319 ) ) ;
#64384 = CARTESIAN_POINT ( 'NONE',  ( -0.1070741851644051862, -0.3996062992125987146, -2.749343832020996636 ) ) ;
#64385 = CARTESIAN_POINT ( 'NONE',  ( -0.3917322834645671215, 0.1049643490035301469, -1.534776902887139194 ) ) ;
#64386 = CARTESIAN_POINT ( 'NONE',  ( -1.318897637795274802, 0.07958543189024085140, 0.2665933059059887866 ) ) ;
#64387 = CARTESIAN_POINT ( 'NONE',  ( 1.148293963254593653, 0.2952755905511810774, -0.1292274648535930714 ) ) ;
#64388 = CARTESIAN_POINT ( 'NONE',  ( 1.410761154855643795, -0.05778040916215560624, -0.4822834645669293319 ) ) ;
#64389 = CARTESIAN_POINT ( 'NONE',  ( 0.3740157480314966754, -0.4536011799217367080, 0.2665933059059888421 ) ) ;
#64390 = CARTESIAN_POINT ( 'NONE',  ( 0.5052493438320215802, 0.2952755905511811885, 0.1292274648535926551 ) ) ;
#64391 = CARTESIAN_POINT ( 'NONE',  ( 0.2362204724409451007, -0.4091458600556402980, -1.428477690288713964 ) ) ;
#64392 = CARTESIAN_POINT ( 'NONE',  ( 0.3412073490813655186, -0.5023911411419708095, -0.1820866141732282451 ) ) ;
#64393 = CARTESIAN_POINT ( 'NONE',  ( -0.07874015748031421014, -0.1870078740157480879, -0.4822834645669291653 ) ) ;
#64394 = CARTESIAN_POINT ( 'NONE',  ( 0.3420746716998660508, 0.1974969037888705814, -1.310367454068241511 ) ) ;
#64395 = CARTESIAN_POINT ( 'NONE',  ( -1.148293963254592542, -0.6692913385826773087, -0.1292274648535924053 ) ) ;
#64396 = CARTESIAN_POINT ( 'NONE',  ( 0.5577427821522314977, -0.2845877964562161244, -0.3641732283464567121 ) ) ;
#64397 = CARTESIAN_POINT ( 'NONE',  ( 0.4849061582275022153, 1.805669738366188382, 0.4921425059946344938 ) ) ;
#64398 = CARTESIAN_POINT ( 'NONE',  ( -0.7020997375328076329, -0.3162353388693409650, -0.4822834645669289433 ) ) ;
#64399 = CARTESIAN_POINT ( 'NONE',  ( -0.4593175853018364174, -0.3690944881889765550, -0.3153832671262227771 ) ) ;
#64400 = CARTESIAN_POINT ( 'NONE',  ( 0.000000000000000000, 0.7086614173228346081, -0.1574803149606299746 ) ) ;
#64401 = CARTESIAN_POINT ( 'NONE',  ( -0.3477690288713905509, -0.6692913385826771977, 0.1292274648535927661 ) ) ;
#64402 = CARTESIAN_POINT ( 'NONE',  ( -0.2690288713910754526, -0.6692913385826771977, 0.1292274648535927661 ) ) ;
#64403 = CARTESIAN_POINT ( 'NONE',  ( 0.4265091863517067039, -0.5511811023622048555, -0.09757992244046775898 ) ) ;
#64404 = CARTESIAN_POINT ( 'NONE',  ( -0.1070741851644056997, 0.3996062992125984925, -1.973097112860892510 ) ) ;
#64405 = CARTESIAN_POINT ( 'NONE',  ( -0.1443569553805765515, -0.4281496062992127816, -0.4176697321401328100 ) ) ;
#64406 = EDGE_CURVE ( 'NONE', #57884, #65284, #9275, .T. ) ;
#64407 = CARTESIAN_POINT ( 'NONE',  ( 0.3917322834645668994, 0.1049643490035304522, -1.622027928312648859 ) ) ;
#64408 = CARTESIAN_POINT ( 'NONE',  ( 0.8792650918635177559, -0.004921259842519576551, 0.3153832671262227771 ) ) ;
#64409 = CARTESIAN_POINT ( 'NONE',  ( 1.332020997375328974, -0.05778040916215560624, -0.4822834645669293319 ) ) ;
#64410 = CARTESIAN_POINT ( 'NONE',  ( -0.8661417322834640276, -0.1870078740157480601, -0.3641732283464567677 ) ) ;
#64411 = CARTESIAN_POINT ( 'NONE',  ( -0.6889763779527552368, -0.4536011799217368745, -0.2665933059059886201 ) ) ;
#64412 = CARTESIAN_POINT ( 'NONE',  ( -0.7480314960629914633, -0.6692913385826771977, 8.415575281601705876E-17 ) ) ;
#64413 = CARTESIAN_POINT ( 'NONE',  ( 0.01312335958005323398, 0.05413385826771666132, 0.4176697321401328100 ) ) ;
#64414 = CARTESIAN_POINT ( 'NONE',  ( 0.7349081364829403995, 0.1283753931104748280, 0.1820866141732283561 ) ) ;
#64415 = CARTESIAN_POINT ( 'NONE',  ( 1.614173228346457156, 1.929133858267716661, -0.5309055118110239668 ) ) ;
#64416 = CARTESIAN_POINT ( 'NONE',  ( 1.207349081364829990, -0.5023911411419708095, -0.1820866141732282451 ) ) ;
#64417 = CARTESIAN_POINT ( 'NONE',  ( 0.6102362204724416372, 0.1660481256975883668, -0.3530559997133364547 ) ) ;
#64418 = FACE_OUTER_BOUND ( 'NONE', #14623, .T. ) ;
#64419 = CARTESIAN_POINT ( 'NONE',  ( -0.09842519685039295696, 0.1660481256975883668, -0.3530559997133364547 ) ) ;
#64420 = CARTESIAN_POINT ( 'NONE',  ( 0.1958661417322834775, 0.3392501089628018884, -0.8589238845144357981 ) ) ;
#64421 = CARTESIAN_POINT ( 'NONE',  ( 1.587926509186352142, -0.004921259842519576551, 0.3153832671262227771 ) ) ;
#64422 = CARTESIAN_POINT ( 'NONE',  ( 1.082677165354331228, 0.1660481256975883668, -0.3530559997133364547 ) ) ;
#64423 = B_SPLINE_CURVE_WITH_KNOTS ( 'NONE', 3,
 ( #28459, #66358, #79834, #54955 ),
 .UNSPECIFIED., .F., .F.,
 ( 4, 4 ),
 ( 2.888536477665436318E-07, 0.001436607511248042500 ),
 .UNSPECIFIED. ) ;
#64424 = CARTESIAN_POINT ( 'NONE',  ( 0.3412073490813655186, -0.6046776061558809534, -0.2411417322834644161 ) ) ;
#64425 = CARTESIAN_POINT ( 'NONE',  ( -3.937007874015748143, 1.724409448818897905, 0.4359958488159719758 ) ) ;
#64426 = CARTESIAN_POINT ( 'NONE',  ( 0.2624671916010504757, 0.1283753931104748280, 0.1820866141732283561 ) ) ;
#64427 = CARTESIAN_POINT ( 'NONE',  ( 0.9186351706036752773, 0.2306618581243847221, -0.2411417322834647770 ) ) ;
#64428 = CARTESIAN_POINT ( 'NONE',  ( -0.1509186351706028884, -0.08942795157527998196, 0.3641732283464567121 ) ) ;
#64429 = CARTESIAN_POINT ( 'NONE',  ( -0.7677165354330699465, -0.5400638737290845981, -0.3530559997133363437 ) ) ;
#64430 = CARTESIAN_POINT ( 'NONE',  ( 0.000000000000000000, 0.09842519685039372024, -1.432673802628665356E-17 ) ) ;
#64431 = CARTESIAN_POINT ( 'NONE',  ( -0.2559055118110230564, 0.1660481256975883668, -0.3530559997133364547 ) ) ;
#64432 = CARTESIAN_POINT ( 'NONE',  ( -1.404199475065615932, -0.4281496062992127816, -0.4176697321401328100 ) ) ;
#64433 = CARTESIAN_POINT ( 'NONE',  ( -0.7677165354330699465, 0.07958543189024085140, 0.2665933059059887866 ) ) ;
#64434 = CARTESIAN_POINT ( 'NONE',  ( 0.2099737532808405305, 0.2306618581243847221, -0.2411417322834647770 ) ) ;
#64435 = CARTESIAN_POINT ( 'NONE',  ( -1.108923884514435132, -0.3162353388693405765, 0.4822834645669290543 ) ) ;
#64436 = CARTESIAN_POINT ( 'NONE',  ( -0.2165354330708654795, 0.1660481256975885056, 0.3530559997133364547 ) ) ;
#64438 = CARTESIAN_POINT ( 'NONE',  ( 1.266404199475066328, -0.05778040916215522460, 0.4822834645669289988 ) ) ;
#64437 = DIRECTION ( 'NONE',  ( 0.000000000000000000, 0.000000000000000000, -1.000000000000000000 ) ) ;
#64439 = CARTESIAN_POINT ( 'NONE',  ( 1.338582677165355062, -0.1870078740157479769, 0.4822834645669291653 ) ) ;
#64440 = CARTESIAN_POINT ( 'NONE',  ( 0.1049643490035304799, -0.3917322834645669549, -2.439632545931758045 ) ) ;
#64441 = CARTESIAN_POINT ( 'NONE',  ( 0.4849061582275024929, 1.726086921369708538, -0.4921425059946356040 ) ) ;
#64442 = CARTESIAN_POINT ( 'NONE',  ( -0.9776902887139098386, -0.6692913385826771977, 0.1292274648535927661 ) ) ;
#64443 = CARTESIAN_POINT ( 'NONE',  ( -1.157146581871515012E-16, 0.4724409448818898682, -0.9448818897637796255 ) ) ;
#64444 = CARTESIAN_POINT ( 'NONE',  ( -0.1070741851644056997, 0.3996062992125986035, -0.1640419947506562004 ) ) ;
#64445 = EDGE_LOOP ( 'NONE', ( #12084, #51956, #65622, #66256 ) ) ;
#64446 = CARTESIAN_POINT ( 'NONE',  ( -0.2427821522309703550, -0.2845877964562159024, 0.3641732283464567677 ) ) ;
#64447 = CARTESIAN_POINT ( 'NONE',  ( 0.3917322834645670104, 2.398668435337828261E-17, -1.842519685039370136 ) ) ;
#64448 = ORIENTED_EDGE ( 'NONE', *, *, #42687, .T. ) ;
#64449 = CARTESIAN_POINT ( 'NONE',  ( 0.3937007874015754361, -0.1870078740157480879, -0.4822834645669291653 ) ) ;
#64450 = CARTESIAN_POINT ( 'NONE',  ( 0.6430446194225728496, 0.05413385826771666132, 0.4176697321401328100 ) ) ;
#64451 = DIRECTION ( 'NONE',  ( 0.000000000000000000, -1.000000000000000000, 0.000000000000000000 ) ) ;
#64452 = CARTESIAN_POINT ( 'NONE',  ( -0.5392480709929732274, -4.055231247046636510E-15, 0.3627989612356165572 ) ) ;
#64453 = CARTESIAN_POINT ( 'NONE',  ( -0.4330708661417315697, -0.5511811023622047445, 6.969142054262312111E-17 ) ) ;
#64454 = CARTESIAN_POINT ( 'NONE',  ( 0.3543307086614179147, 0.2952755905511811885, 0.000000000000000000 ) ) ;
#64455 = CARTESIAN_POINT ( 'NONE',  ( 0.8595800524934390507, -0.3162353388693405765, 0.4822834645669290543 ) ) ;
#64456 = CARTESIAN_POINT ( 'NONE',  ( 0.9055118110236227702, -0.5511811023622047445, 6.969142054262312111E-17 ) ) ;
#64457 = CARTESIAN_POINT ( 'NONE',  ( -0.6036745406824141069, -0.6046776061558809534, -0.2411417322834644161 ) ) ;
#64458 = CARTESIAN_POINT ( 'NONE',  ( -0.3917322834645670659, 0.1049643490035301607, -1.215203781331021915 ) ) ;
#64459 = CARTESIAN_POINT ( 'NONE',  ( -0.8464566929133852113, 0.1660481256975885056, 0.3530559997133364547 ) ) ;
#64460 = CARTESIAN_POINT ( 'NONE',  ( -1.213910761154854745, 0.1771653543307087075, -0.09757992244046823083 ) ) ;
#64461 = CARTESIAN_POINT ( 'NONE',  ( -1.010498687664041384, -0.4281496062992127816, -0.4176697321401328100 ) ) ;
#64462 = CARTESIAN_POINT ( 'NONE',  ( 1.200787401574803681, 0.1660481256975885056, 0.3530559997133364547 ) ) ;
#64463 = CARTESIAN_POINT ( 'NONE',  ( -0.4698620426709900766, 1.469755830210692560, -2.159222551273901836 ) ) ;
#64464 = ORIENTED_EDGE ( 'NONE', *, *, #37751, .F. ) ;
#64465 = CARTESIAN_POINT ( 'NONE',  ( -0.3917322834645670104, -0.1049643490035307020, -2.404874958826459075 ) ) ;
#64466 = CARTESIAN_POINT ( 'NONE',  ( 0.1968503937007881344, -0.6692913385826771977, 8.415575281601705876E-17 ) ) ;
#64467 = ORIENTED_EDGE ( 'NONE', *, *, #41459, .T. ) ;
#64468 = CARTESIAN_POINT ( 'NONE',  ( -0.9186351706036736120, 0.2306618581243848609, 0.2411417322834645549 ) ) ;
#64469 = CARTESIAN_POINT ( 'NONE',  ( 1.522309711286089939, -0.6046776061558809534, -0.2411417322834644161 ) ) ;
#64470 = CARTESIAN_POINT ( 'NONE',  ( 1.430446194225722500, 0.05413385826771666132, 0.4176697321401328100 ) ) ;
#64471 = CARTESIAN_POINT ( 'NONE',  ( 0.5971128608923890191, -0.6692913385826771977, 0.1292274648535927661 ) ) ;
#64472 = CARTESIAN_POINT ( 'NONE',  ( 0.1771653543307093182, -0.5400638737290845981, -0.3530559997133363437 ) ) ;
#64473 = CARTESIAN_POINT ( 'NONE',  ( 0.3917322834645670104, 2.398668435337828261E-17, -1.935039370078740273 ) ) ;
#64474 = CARTESIAN_POINT ( 'NONE',  ( -1.069553805774277722, 0.2952755905511811885, 0.1292274648535926551 ) ) ;
#64475 = CARTESIAN_POINT ( 'NONE',  ( -0.03280839895013062252, 0.2952755905511810774, -0.1292274648535930714 ) ) ;
#64476 = CARTESIAN_POINT ( 'NONE',  ( -0.2034120734908128059, 0.1771653543307087630, 0.09757992244046791164 ) ) ;
#64477 = CARTESIAN_POINT ( 'NONE',  ( 0.000000000000000000, 0.000000000000000000, -2.755905511811024056 ) ) ;
#64478 = EDGE_CURVE ( 'NONE', #64485, #4208, #74127, .T. ) ;
#64479 = CARTESIAN_POINT ( 'NONE',  ( -0.2230971128608915943, -0.4281496062992127816, -0.4176697321401328100 ) ) ;
#64480 = CARTESIAN_POINT ( 'NONE',  ( 0.2690288713910768403, 0.2066929133858267931, 0.1054918080437490802 ) ) ;
#64481 = CARTESIAN_POINT ( 'NONE',  ( 1.200787401574803681, -0.5400638737290845981, -0.3530559997133363437 ) ) ;
#64482 = FACE_OUTER_BOUND ( 'NONE', #54231, .T. ) ;
#64483 = ORIENTED_EDGE ( 'NONE', *, *, #52190, .F. ) ;
#64484 = ADVANCED_FACE ( 'NONE', ( #21892 ), #29852, .T. ) ;
#64485 = VERTEX_POINT ( 'NONE', #80815 ) ;
#64486 = CARTESIAN_POINT ( 'NONE',  ( 0.2099737532808405305, -0.6046776061558807314, 0.2411417322834647770 ) ) ;
#64487 = CARTESIAN_POINT ( 'NONE',  ( -0.4002624671916004129, -0.08942795157528024563, -0.3641732283464568787 ) ) ;
#64489 = LINE ( 'NONE', #12321, #3483 ) ;
#64488 = CARTESIAN_POINT ( 'NONE',  ( 1.515748031496063408, 0.07958543189024085140, 0.2665933059059887866 ) ) ;
#64490 = CARTESIAN_POINT ( 'NONE',  ( 0.4091458600556404646, -0.2362204724409448231, -0.1817585301837270351 ) ) ;
#64491 = CARTESIAN_POINT ( 'NONE',  ( 1.666666666666667185, -0.004921259842519576551, 0.3153832671262227771 ) ) ;
#64492 = CARTESIAN_POINT ( 'NONE',  ( 1.574803149606299746, -0.1870078740157479769, 0.4822834645669291653 ) ) ;
#64493 = CARTESIAN_POINT ( 'NONE',  ( 0.3996062992125986035, -0.1070741851644052972, -2.708005249343832688 ) ) ;
#64494 = CARTESIAN_POINT ( 'NONE',  ( 0.2493438320209980519, -0.4281496062992127816, -0.4176697321401328100 ) ) ;
#64495 = CARTESIAN_POINT ( 'NONE',  ( -1.559171609364246924, 0.3937007874015748254, 0.1028181436694137613 ) ) ;
#64496 = CARTESIAN_POINT ( 'NONE',  ( -1.417322834645668772, -0.1870078740157479769, 0.4822834645669291653 ) ) ;
#64497 = CARTESIAN_POINT ( 'NONE',  ( 0.3149606299212603933, -0.1870078740157479769, 0.4822834645669291653 ) ) ;
#64498 = CARTESIAN_POINT ( 'NONE',  ( 0.3420746716998660508, 0.1974969037888705814, 0.1069553805774278443 ) ) ;
#64499 = CARTESIAN_POINT ( 'NONE',  ( 1.522309711286089939, 0.2306618581243848609, 0.2411417322834645549 ) ) ;
#64500 = CARTESIAN_POINT ( 'NONE',  ( 0.8202099737532813073, 0.2952755905511811885, 0.1292274648535926551 ) ) ;
#64501 = CARTESIAN_POINT ( 'NONE',  ( 1.135170603674541256, -0.5511811023622048555, -0.09757992244046775898 ) ) ;
#64502 = DIRECTION ( 'NONE',  ( 0.000000000000000000, 0.000000000000000000, 1.000000000000000000 ) ) ;
#64503 = CARTESIAN_POINT ( 'NONE',  ( 0.9448818897637802916, -0.1870078740157480601, -0.3641732283464567677 ) ) ;
#64504 = CARTESIAN_POINT ( 'NONE',  ( -1.404199475065615932, -0.4281496062992127816, -0.4176697321401328100 ) ) ;
#64505 = CARTESIAN_POINT ( 'NONE',  ( -0.3996062992125985480, -7.340648628747423112E-17, -0.9035433070866141225 ) ) ;
#64506 = CARTESIAN_POINT ( 'NONE',  ( 0.9776902887139113929, -0.6692913385826773087, -0.1292274648535924053 ) ) ;
#64507 = ADVANCED_FACE ( 'NONE', ( #15597 ), #61018, .F. ) ;
#64508 = CARTESIAN_POINT ( 'NONE',  ( -9.594673741351313045E-17, 0.3917322834645670104, -0.4645669291338582751 ) ) ;
#64509 = EDGE_CURVE ( 'NONE', #22644, #8180, #3784, .T. ) ;
#64511 = CARTESIAN_POINT ( 'NONE',  ( -0.3812543623607988486, 1.253662731238188721, 2.019864340580467932 ) ) ;
#64510 = CARTESIAN_POINT ( 'NONE',  ( 0.5708661417322842269, 0.1660481256975885056, 0.3530559997133364547 ) ) ;
#64512 = CARTESIAN_POINT ( 'NONE',  ( -1.706036745406823485, 0.1283753931104748280, 0.1820866141732283561 ) ) ;
#64513 = CARTESIAN_POINT ( 'NONE',  ( 0.6364829396325465405, -0.08942795157527998196, 0.3641732283464567121 ) ) ;
#64514 = CARTESIAN_POINT ( 'NONE',  ( 0.5905511811023629321, 0.2952755905511811885, 0.000000000000000000 ) ) ;
#64515 = CARTESIAN_POINT ( 'NONE',  ( -0.2686849592492766003, 0.1228903193441466535, 0.1574803149606299191 ) ) ;
#64516 = CARTESIAN_POINT ( 'NONE',  ( -0.8267716535433065062, -0.5511811023622047445, 6.969142054262312111E-17 ) ) ;
#64517 = CARTESIAN_POINT ( 'NONE',  ( -0.5183727034120726440, -0.6692913385826773087, -0.1292274648535924053 ) ) ;
#64518 = CARTESIAN_POINT ( 'NONE',  ( -1.601049868766403650, 0.1283753931104746893, -0.1820866141732285504 ) ) ;
#64519 = CARTESIAN_POINT ( 'NONE',  ( -1.030183727034119867, -0.05778040916215560624, -0.4822834645669293319 ) ) ;
#64520 = CARTESIAN_POINT ( 'NONE',  ( 0.9120734908136490793, 0.2952755905511810774, -0.1292274648535930714 ) ) ;
#64521 = ADVANCED_BREP_SHAPE_REPRESENTATION ( '', ( #59000, #22098 ), #75874 ) ;
#64522 = CARTESIAN_POINT ( 'NONE',  ( -1.174540682414697335, -0.08942795157527998196, 0.3641732283464567121 ) ) ;
#64523 = CARTESIAN_POINT ( 'NONE',  ( -0.3973686378485497550, -0.03056273350765931207, -1.220472440944882386 ) ) ;
#64524 = CARTESIAN_POINT ( 'NONE',  ( 0.9973753280839902091, 0.2306618581243847221, -0.2411417322834647770 ) ) ;
#64525 = CARTESIAN_POINT ( 'NONE',  ( -0.4091458600556402980, -0.2362204724409451284, -2.491469816272966042 ) ) ;
#64526 = CARTESIAN_POINT ( 'NONE',  ( -1.699475065616797398, 0.2952755905511811885, 0.1292274648535926551 ) ) ;
#64527 = CARTESIAN_POINT ( 'NONE',  ( 1.292650918635171564, -0.6692913385826773087, -0.1292274648535924053 ) ) ;
#64528 = CARTESIAN_POINT ( 'NONE',  ( -1.115485564304461219, -0.3690944881889763329, 0.3153832671262228327 ) ) ;
#64529 = CARTESIAN_POINT ( 'NONE',  ( 1.666666666666667185, -0.004921259842519576551, 0.3153832671262227771 ) ) ;
#64530 = CARTESIAN_POINT ( 'NONE',  ( -1.161417322834644716, 0.07958543189024085140, 0.2665933059059887866 ) ) ;
#64531 = CARTESIAN_POINT ( 'NONE',  ( -0.4855643044619415427, -0.004921259842519870586, -0.3153832671262229437 ) ) ;
#64532 = CARTESIAN_POINT ( 'NONE',  ( -1.364829396325458521, 0.1283753931104746893, -0.1820866141732285504 ) ) ;
#64533 = CARTESIAN_POINT ( 'NONE',  ( 0.7742782152230978099, -0.3690944881889763329, 0.3153832671262228327 ) ) ;
#64534 = CARTESIAN_POINT ( 'NONE',  ( 0.3543307086614181922, -0.6692913385826771977, 8.415575281601705876E-17 ) ) ;
#64535 = CARTESIAN_POINT ( 'NONE',  ( 1.528871391076116026, -0.6692913385826773087, -0.1292274648535924053 ) ) ;
#64536 = CARTESIAN_POINT ( 'NONE',  ( -0.09186351706036663400, -0.4281496062992124485, 0.4176697321401328655 ) ) ;
#64537 = EDGE_CURVE ( 'NONE', #54535, #5751, #2547, .T. ) ;
#64538 = CARTESIAN_POINT ( 'NONE',  ( 0.6824146981627303710, 0.1283753931104746893, -0.1820866141732285504 ) ) ;
#64539 = CARTESIAN_POINT ( 'NONE',  ( -1.574803149606298192, -0.1870078740157480879, -0.4822834645669291653 ) ) ;
#64540 = CARTESIAN_POINT ( 'NONE',  ( -1.332020997375327642, -0.05778040916215522460, 0.4822834645669289988 ) ) ;
#64541 = CARTESIAN_POINT ( 'NONE',  ( -0.5774278215223089816, 0.2306618581243847221, -0.2411417322834647770 ) ) ;
#64542 = CARTESIAN_POINT ( 'NONE',  ( 0.1998031496062994405, -0.3460692066303958092, -0.2493438320209974135 ) ) ;
#64543 = CARTESIAN_POINT ( 'NONE',  ( -0.1265901696524993347, 0.4724409448818896462, -1.185695538057742748 ) ) ;
#64544 = CARTESIAN_POINT ( 'NONE',  ( 0.05249343832021075018, 0.2306618581243847221, -0.2411417322834647770 ) ) ;
#64545 = CARTESIAN_POINT ( 'NONE',  ( 1.108923884514436242, -0.08942795157527998196, 0.3641732283464567121 ) ) ;
#64546 = CARTESIAN_POINT ( 'NONE',  ( -0.4199475065616791736, -0.6046776061558807314, 0.2411417322834647770 ) ) ;
#64547 = CARTESIAN_POINT ( 'NONE',  ( 0.5511811023622054106, -0.1870078740157480879, -0.4822834645669291653 ) ) ;
#64548 = CARTESIAN_POINT ( 'NONE',  ( 0.1998031496062994405, -0.3460692066303958092, -2.769028871391076230 ) ) ;
#64549 = CARTESIAN_POINT ( 'NONE',  ( -0.3949938075777409963, -7.255918531996591613E-17, -1.771653543307086576 ) ) ;
#64550 = CARTESIAN_POINT ( 'NONE',  ( -9.594673741351313045E-17, 0.3917322834645670104, -0.4645669291338582751 ) ) ;
#64551 = CARTESIAN_POINT ( 'NONE',  ( 0.2524772379609335204, -0.1532855601034649740, 5.612412912560978739 ) ) ;
#64552 = CARTESIAN_POINT ( 'NONE',  ( -0.2867679344610364334, -0.2867679344610367109, -1.153543307086613900 ) ) ;
#64553 = CARTESIAN_POINT ( 'NONE',  ( -1.082677165354329896, 0.07958543189024085140, 0.2665933059059887866 ) ) ;
#64554 = CARTESIAN_POINT ( 'NONE',  ( 0.2867679344610365999, 0.2867679344610365999, -1.232283464566929387 ) ) ;
#64555 = CARTESIAN_POINT ( 'NONE',  ( -1.213910761154854745, 0.2952755905511810774, -0.1292274648535930714 ) ) ;
#64556 = CARTESIAN_POINT ( 'NONE',  ( 0.3917322834645668994, 0.1049643490035304522, 0.1102555362542800566 ) ) ;
#64557 = EDGE_CURVE ( 'NONE', #38656, #68129, #22982, .T. ) ;
#64558 = CARTESIAN_POINT ( 'NONE',  ( 0.5052493438320218022, -0.6692913385826773087, -0.1292274648535924053 ) ) ;
#64559 = CARTESIAN_POINT ( 'NONE',  ( 1.122047244094488860, 0.1660481256975885056, 0.3530559997133364547 ) ) ;
#64560 = CARTESIAN_POINT ( 'NONE',  ( 0.7086614173228352742, -0.1870078740157480879, -0.4822834645669291653 ) ) ;
#64561 = CARTESIAN_POINT ( 'NONE',  ( -0.1265901696524993347, 0.4724409448818895907, -2.841207349081364963 ) ) ;
#64562 = CARTESIAN_POINT ( 'NONE',  ( 0.2925321140481932369, -0.2925321140481932369, -2.460629921259842146 ) ) ;
#64563 = CARTESIAN_POINT ( 'NONE',  ( -0.1049643490035302301, -0.3917322834645671770, -1.013798843340894207 ) ) ;
#64564 = CARTESIAN_POINT ( 'NONE',  ( 1.220472440944882608, 0.2952755905511811885, 0.000000000000000000 ) ) ;
#64565 = CARTESIAN_POINT ( 'NONE',  ( 0.3871391076115492380, -0.05778040916215560624, -0.4822834645669293319 ) ) ;
#64566 = CARTESIAN_POINT ( 'NONE',  ( 0.2755905511811031494, -0.6692913385826771977, 8.415575281601705876E-17 ) ) ;
#64567 = CARTESIAN_POINT ( 'NONE',  ( 0.6299212598425204535, -0.1870078740157479769, 0.3641732283464567677 ) ) ;
#64568 = CARTESIAN_POINT ( 'NONE',  ( 1.148293963254593875, -0.6692913385826771977, 0.1292274648535927661 ) ) ;
#64569 = CARTESIAN_POINT ( 'NONE',  ( 0.2867679344610365999, 0.2867679344610365999, -0.06496062992125994917 ) ) ;
#64570 = CARTESIAN_POINT ( 'NONE',  ( -0.08530183727034056085, -0.05778040916215560624, -0.4822834645669293319 ) ) ;
#64571 = CARTESIAN_POINT ( 'NONE',  ( 0.9186351706036752773, 0.2306618581243847221, -0.2411417322834647770 ) ) ;
#64572 = CARTESIAN_POINT ( 'NONE',  ( 0.5905511811023629321, 0.2952755905511811885, 0.000000000000000000 ) ) ;
#64573 = CARTESIAN_POINT ( 'NONE',  ( 1.036745406824147731, -0.004921259842519576551, 0.3153832671262227771 ) ) ;
#64574 = CARTESIAN_POINT ( 'NONE',  ( -0.7808398950131225646, -0.05778040916215522460, 0.4822834645669289988 ) ) ;
#64575 = CARTESIAN_POINT ( 'NONE',  ( -1.135170603674539924, -0.6692913385826771977, 0.1292274648535927661 ) ) ;
#64576 = CARTESIAN_POINT ( 'NONE',  ( 1.154855643044620184, 0.2306618581243847221, -0.2411417322834647770 ) ) ;
#64577 = CARTESIAN_POINT ( 'NONE',  ( 0.3917322834645670104, -0.1049643490035303411, -0.5111548556430445256 ) ) ;
#64578 = CARTESIAN_POINT ( 'NONE',  ( 0.1958661417322836440, -0.3392501089628017219, -1.816272965879265122 ) ) ;
#64579 = CARTESIAN_POINT ( 'NONE',  ( 0.2867679344610365999, 0.2867679344610365999, -2.807086614173227357 ) ) ;
#64580 = EDGE_CURVE ( 'NONE', #66690, #21828, #35356, .T. ) ;
#64581 = ORIENTED_EDGE ( 'NONE', *, *, #50736, .F. ) ;
#64582 = CARTESIAN_POINT ( 'NONE',  ( -0.1070741851644056997, 0.3996062992125986035, -0.006561679790026264843 ) ) ;
#64583 = ORIENTED_EDGE ( 'NONE', *, *, #17800, .F. ) ;
#64584 = CARTESIAN_POINT ( 'NONE',  ( 1.548556430446194954, 0.2306618581243847221, -0.2411417322834647770 ) ) ;
#64585 = CARTESIAN_POINT ( 'NONE',  ( 1.108923884514436242, -0.08942795157527998196, 0.3641732283464567121 ) ) ;
#64586 = CARTESIAN_POINT ( 'NONE',  ( -0.3996062992125986035, -7.340648628747425578E-17, -1.929133858267716439 ) ) ;
#64587 = CARTESIAN_POINT ( 'NONE',  ( 1.305774278215223960, -0.5511811023622046335, 0.09757992244046803654 ) ) ;
#64588 = DIRECTION ( 'NONE',  ( -1.000000000000000000, -3.083952846180990281E-16, 0.000000000000000000 ) ) ;
#64589 = DIRECTION ( 'NONE',  ( 0.000000000000000000, 0.000000000000000000, 1.000000000000000000 ) ) ;
#64590 = CARTESIAN_POINT ( 'NONE',  ( 0.3951562584566663539, 0.01150853369506588293, -1.929133858268277546 ) ) ;
#64591 = CARTESIAN_POINT ( 'NONE',  ( 0.2867679344610365999, 0.2867679344610365999, -0.8523622047244096001 ) ) ;
#64592 = CARTESIAN_POINT ( 'NONE',  ( -0.9711286089238838626, 0.1283753931104746893, -0.1820866141732285504 ) ) ;
#64593 = CARTESIAN_POINT ( 'NONE',  ( 1.594488188976378673, 0.1660481256975885056, 0.3530559997133364547 ) ) ;
#64594 = CARTESIAN_POINT ( 'NONE',  ( -1.154855643044618851, 0.2306618581243848609, 0.2411417322834645549 ) ) ;
#64595 = CARTESIAN_POINT ( 'NONE',  ( 0.2165354330708668673, 0.1660481256975883668, -0.3530559997133364547 ) ) ;
#64596 = CARTESIAN_POINT ( 'NONE',  ( -1.607611548556429737, 0.2952755905511810774, -0.1292274648535930714 ) ) ;
#64597 = VERTEX_POINT ( 'NONE', #16426 ) ;
#64598 = AXIS2_PLACEMENT_3D ( 'NONE', #54440, #7029, #7454 ) ;
#64599 = CARTESIAN_POINT ( 'NONE',  ( -1.120392597725979655, 1.066916830561088103, -0.06289000371407697798 ) ) ;
#64600 = PRODUCT_CONTEXT ( 'NONE', #48197, 'mechanical' ) ;
#64601 = DIRECTION ( 'NONE',  ( -0.7071067811865376918, 0.000000000000000000, 0.7071067811865573427 ) ) ;
#64602 = CARTESIAN_POINT ( 'NONE',  ( -0.2017716535433071445, -0.2017716535433071445, -0.3937007874015748254 ) ) ;
#64603 = CARTESIAN_POINT ( 'NONE',  ( -0.9776902887139098386, 0.1771653543307087075, -0.09757992244046823083 ) ) ;
#64604 = CARTESIAN_POINT ( 'NONE',  ( 0.5774278215223104249, 0.2306618581243848609, 0.2411417322834645549 ) ) ;
#64605 = ORIENTED_EDGE ( 'NONE', *, *, #53516, .F. ) ;
#64607 = CARTESIAN_POINT ( 'NONE',  ( -1.220472440944881720, 0.8346805926620878280, 0.5309055118110233007 ) ) ;
#64606 = LINE ( 'NONE', #65459, #588 ) ;
#64608 = CARTESIAN_POINT ( 'NONE',  ( 1.272965879265092637, -0.4281496062992127816, -0.4176697321401328100 ) ) ;
#64609 = CARTESIAN_POINT ( 'NONE',  ( -1.679790026246718693, 0.2306618581243847221, -0.2411417322834647770 ) ) ;
#64610 = CARTESIAN_POINT ( 'NONE',  ( 0.1049643490035303689, 0.3917322834645668994, -0.8608730726696044444 ) ) ;
#64611 = CARTESIAN_POINT ( 'NONE',  ( -0.3346456692913377662, -0.4536011799217367080, 0.2665933059059888421 ) ) ;
#64612 = CARTESIAN_POINT ( 'NONE',  ( -1.292650918635170010, 0.1771653543307087075, -0.09757992244046823083 ) ) ;
#64613 = DIRECTION ( 'NONE',  ( -3.096699300667737957E-16, 1.000000000000000000, -0.000000000000000000 ) ) ;
#64614 = CARTESIAN_POINT ( 'NONE',  ( -0.4265091863517051496, -0.5511811023622046335, 0.09757992244046803654 ) ) ;
#64615 = CARTESIAN_POINT ( 'NONE',  ( 0.2034120734908142214, 0.1771653543307087075, -0.09757992244046823083 ) ) ;
#64616 = AXIS2_PLACEMENT_3D ( 'NONE', #16440, #66534, #8865 ) ;
#64617 = CARTESIAN_POINT ( 'NONE',  ( 0.03280839895013198948, 0.2952755905511811885, 0.1292274648535926551 ) ) ;
#64618 = CARTESIAN_POINT ( 'NONE',  ( -1.036745406824146176, -0.3690944881889763329, 0.3153832671262228327 ) ) ;
#64619 = CARTESIAN_POINT ( 'NONE',  ( -0.3392501089628019995, 0.1958661417322832277, -2.853018372703412187 ) ) ;
#64620 = CARTESIAN_POINT ( 'NONE',  ( 1.135170603674541256, 0.2952755905511811885, 0.1292274648535926551 ) ) ;
#64621 = CARTESIAN_POINT ( 'NONE',  ( -1.279527559055116948, 0.1660481256975883668, -0.3530559997133364547 ) ) ;
#64622 = CARTESIAN_POINT ( 'NONE',  ( -0.1265901696524986964, -0.4724409448818899238, -1.093832020997375087 ) ) ;
#64623 = CARTESIAN_POINT ( 'NONE',  ( -0.2427821522309703550, -0.05778040916215560624, -0.4822834645669293319 ) ) ;
#64624 = CARTESIAN_POINT ( 'NONE',  ( 0.4396325459317590445, -0.5511811023622046335, 0.09757992244046803654 ) ) ;
#64625 = ADVANCED_FACE ( 'NONE', ( #10521, #67767 ), #10103, .T. ) ;
#64626 = CARTESIAN_POINT ( 'NONE',  ( -1.069553805774277722, -0.6692913385826773087, -0.1292274648535924053 ) ) ;
#64627 = CARTESIAN_POINT ( 'NONE',  ( 0.6889763779527566800, -0.4536011799217367080, 0.2665933059059888421 ) ) ;
#64628 = CARTESIAN_POINT ( 'NONE',  ( -0.1640419947506555343, -0.2845877964562159024, 0.3641732283464567677 ) ) ;
#64629 = CARTESIAN_POINT ( 'NONE',  ( -0.8202099737532801971, -0.6692913385826771977, 0.1292274648535927661 ) ) ;
#64630 = CARTESIAN_POINT ( 'NONE',  ( -1.640419947506561060, 0.05413385826771666132, 0.4176697321401328100 ) ) ;
#64631 = CARTESIAN_POINT ( 'NONE',  ( -0.7402641841139966372, 2.388450810264987734, 0.4916013665244731712 ) ) ;
#64632 = CARTESIAN_POINT ( 'NONE',  ( 1.167979002624672580, -0.3690944881889763329, 0.3153832671262228327 ) ) ;
#64633 = ADVANCED_FACE ( 'NONE', ( #4189 ), #55515, .F. ) ;
#64634 = CARTESIAN_POINT ( 'NONE',  ( -1.338582677165353729, -0.1870078740157479769, 0.4822834645669291653 ) ) ;
#64635 = CARTESIAN_POINT ( 'NONE',  ( -1.430446194225721390, -0.4281496062992124485, 0.4176697321401328655 ) ) ;
#64636 = EDGE_LOOP ( 'NONE', ( #13665, #1141, #9193, #17052 ) ) ;
#64637 = CARTESIAN_POINT ( 'NONE',  ( 0.3996062992125984925, 0.1070741851644054637, -2.563648293963254776 ) ) ;
#64638 = CARTESIAN_POINT ( 'NONE',  ( -0.8202099737532799750, 0.1771653543307087075, -0.09757992244046823083 ) ) ;
#64639 = CARTESIAN_POINT ( 'NONE',  ( 0.6102362204724416372, -0.5400638737290844871, 0.3530559997133364547 ) ) ;
#64640 = CARTESIAN_POINT ( 'NONE',  ( -1.115485564304461219, -0.3690944881889763329, 0.3153832671262228327 ) ) ;
#64641 = CARTESIAN_POINT ( 'NONE',  ( -0.1070741851644051862, -0.3996062992125986590, -1.881233595800524849 ) ) ;
#64642 = CARTESIAN_POINT ( 'NONE',  ( -1.062992125984250968, 0.2952755905511811885, 0.000000000000000000 ) ) ;
#64643 = CARTESIAN_POINT ( 'NONE',  ( 0.6955380577427828781, -0.4281496062992124485, 0.4176697321401328655 ) ) ;
#64644 = CARTESIAN_POINT ( 'NONE',  ( 0.4199475065616805614, 0.2306618581243848609, 0.2411417322834645549 ) ) ;
#64645 = CARTESIAN_POINT ( 'NONE',  ( -0.1265901696524986964, -0.4724409448818899238, -0.07217847769028870597 ) ) ;
#64646 = CARTESIAN_POINT ( 'NONE',  ( -1.646981627296586703, -0.2845877964562161244, -0.3641732283464567121 ) ) ;
#64647 = CARTESIAN_POINT ( 'NONE',  ( 0.3996062992125984925, 0.1070741851644054499, -0.5164041994750655507 ) ) ;
#64648 = CARTESIAN_POINT ( 'NONE',  ( -0.2925321140481932924, 0.2925321140481931814, -0.9645669291338579976 ) ) ;
#64649 = CARTESIAN_POINT ( 'NONE',  ( -0.1058382717557497937, -0.3949938075777411628, -0.8595800524934383846 ) ) ;
#64650 = FACE_OUTER_BOUND ( 'NONE', #19032, .T. ) ;
#64651 = CARTESIAN_POINT ( 'NONE',  ( 1.200787401574803681, 0.07958543189024085140, 0.2665933059059887866 ) ) ;
#64652 = CARTESIAN_POINT ( 'NONE',  ( 0.2427821522309716595, -0.2845877964562161244, -0.3641732283464567121 ) ) ;
#64653 = CARTESIAN_POINT ( 'NONE',  ( 0.03937007874015806264, 0.2952755905511811885, 0.000000000000000000 ) ) ;
#64654 = CARTESIAN_POINT ( 'NONE',  ( 1.259842519685040019, -0.1870078740157479769, 0.4822834645669291653 ) ) ;
#64655 = CARTESIAN_POINT ( 'NONE',  ( -0.1974969037888706924, 0.3420746716998658843, -1.349737532808398921 ) ) ;
#64656 = CARTESIAN_POINT ( 'NONE',  ( 0.4790026246719168435, -0.2845877964562161244, -0.3641732283464567121 ) ) ;
#64657 = CARTESIAN_POINT ( 'NONE',  ( -0.8923884514435688198, -0.6046776061558807314, 0.2411417322834647770 ) ) ;
#64658 = CARTESIAN_POINT ( 'NONE',  ( -1.397637795275589623, -0.5400638737290845981, -0.3530559997133363437 ) ) ;
#64659 = CARTESIAN_POINT ( 'NONE',  ( 0.7939632545931766261, -0.3162353388693409650, -0.4822834645669289433 ) ) ;
#64660 = CARTESIAN_POINT ( 'NONE',  ( 0.4724409448818898682, 2.892866454678787531E-17, -1.692913385826771533 ) ) ;
#64661 = CARTESIAN_POINT ( 'NONE',  ( 0.1070741851644054915, -0.3996062992125985480, -2.604986876640420057 ) ) ;
#64662 = VERTEX_POINT ( 'NONE', #69815 ) ;
#64663 = EDGE_LOOP ( 'NONE', ( #36006, #31541, #78247, #52221, #37858, #76298, #33438 ) ) ;
#64664 = CARTESIAN_POINT ( 'NONE',  ( -1.194225721784776262, 0.05413385826771626580, -0.4176697321401330321 ) ) ;
#64665 = CARTESIAN_POINT ( 'NONE',  ( -0.7414698162729651543, -0.6692913385826771977, 0.1292274648535927661 ) ) ;
#64667 = CARTESIAN_POINT ( 'NONE',  ( -0.9317585301837263412, -0.4281496062992127816, -0.4176697321401328100 ) ) ;
#64666 = CARTESIAN_POINT ( 'NONE',  ( -0.6299212598425188991, -0.1870078740157480601, -0.3641732283464567677 ) ) ;
#64668 = CARTESIAN_POINT ( 'NONE',  ( 0.1958661417322836162, -0.3392501089628018329, -2.061660474244408014 ) ) ;
#64669 = CARTESIAN_POINT ( 'NONE',  ( 0.5314960629921393620, 2.755905511811024056, -3.821484228344191880 ) ) ;
#64670 = CARTESIAN_POINT ( 'NONE',  ( 1.555118110236221041, 0.1660481256975883668, -0.3530559997133364547 ) ) ;
#64671 = CARTESIAN_POINT ( 'NONE',  ( -1.246719160104986512, 0.05413385826771666132, 0.4176697321401328100 ) ) ;
#64672 = CARTESIAN_POINT ( 'NONE',  ( 0.1574803149606306130, -0.1870078740157479769, 0.4822834645669291653 ) ) ;
#64673 = CARTESIAN_POINT ( 'NONE',  ( -0.6692913385826764205, 0.2952755905511811885, 0.000000000000000000 ) ) ;
#64674 = CARTESIAN_POINT ( 'NONE',  ( 0.4921259842519691285, 0.1660481256975885056, 0.3530559997133364547 ) ) ;
#64675 = CARTESIAN_POINT ( 'NONE',  ( 0.3392501089628018884, -0.1958661417322834220, -1.356955380577427928 ) ) ;
#64676 = CARTESIAN_POINT ( 'NONE',  ( -1.023622047244093558, -0.1870078740157479769, 0.3641732283464567677 ) ) ;
#64677 = ORIENTED_EDGE ( 'NONE', *, *, #51203, .F. ) ;
#64678 = CARTESIAN_POINT ( 'NONE',  ( 0.1058382717557499880, 0.3949938075777411073, -1.725721784776902856 ) ) ;
#64679 = ORIENTED_EDGE ( 'NONE', *, *, #38011, .T. ) ;
#64680 = DIRECTION ( 'NONE',  ( -1.000000000000000000, -0.000000000000000000, -0.000000000000000000 ) ) ;
#64681 = CARTESIAN_POINT ( 'NONE',  ( -1.299212598425196097, -0.6692913385826771977, 8.415575281601705876E-17 ) ) ;
#64682 = CARTESIAN_POINT ( 'NONE',  ( -1.246719160104985846, -0.4281496062992127816, -0.4176697321401328100 ) ) ;
#64683 = CARTESIAN_POINT ( 'NONE',  ( 0.1998031496062992740, 0.3460692066303959757, 0.01312335958005248458 ) ) ;
#64684 = CARTESIAN_POINT ( 'NONE',  ( -0.9908136482939626788, -0.6692913385826773087, -0.1292274648535924053 ) ) ;
#64685 = CARTESIAN_POINT ( 'NONE',  ( -1.272965879265091305, -0.4281496062992124485, 0.4176697321401328655 ) ) ;
#64686 = CARTESIAN_POINT ( 'NONE',  ( -1.332020997375327642, -0.05778040916215522460, 0.4822834645669289988 ) ) ;
#64687 = CARTESIAN_POINT ( 'NONE',  ( -0.3833616679418195283, -1.094630224652485432E-15, 0.4281993546915541238 ) ) ;
#64688 = CARTESIAN_POINT ( 'NONE',  ( -0.1958661417322836718, 0.3392501089628017219, 0.2171916010498686767 ) ) ;
#64689 = CARTESIAN_POINT ( 'NONE',  ( -0.02624671916010428221, 0.1283753931104746893, -0.1820866141732285504 ) ) ;
#64690 = LINE ( 'NONE', #78591, #78072 ) ;
#64691 = CARTESIAN_POINT ( 'NONE',  ( -9.594673741351313045E-17, 0.3917322834645670104, -0.3996062992125985480 ) ) ;
#64692 = CARTESIAN_POINT ( 'NONE',  ( -0.3215223097112853146, -0.2845877964562159024, 0.3641732283464567677 ) ) ;
#64693 = CARTESIAN_POINT ( 'NONE',  ( -0.7939632545931750718, -0.05778040916215560624, -0.4822834645669293319 ) ) ;
#64694 = CARTESIAN_POINT ( 'NONE',  ( 1.345144356955381593, -0.3162353388693409650, -0.4822834645669289433 ) ) ;
#64695 = CARTESIAN_POINT ( 'NONE',  ( -0.6036745406824141069, -0.6046776061558809534, -0.2411417322834644161 ) ) ;
#64696 = VERTEX_POINT ( 'NONE', #18879 ) ;
#64697 = VERTEX_POINT ( 'NONE', #75730 ) ;
#64698 = CARTESIAN_POINT ( 'NONE',  ( -0.1070741851644051862, -0.3996062992125986590, -2.196194225721784576 ) ) ;
#64699 = CARTESIAN_POINT ( 'NONE',  ( -1.174540682414697335, -0.05778040916215522460, 0.4822834645669289988 ) ) ;
#64700 = CARTESIAN_POINT ( 'NONE',  ( 1.338582677165355062, -0.1870078740157480879, -0.4822834645669291653 ) ) ;
#64701 = CARTESIAN_POINT ( 'NONE',  ( -1.423884514435694859, -0.2845877964562159024, 0.3641732283464567677 ) ) ;
#64702 = CARTESIAN_POINT ( 'NONE',  ( -1.332020997375327642, -0.3162353388693409650, -0.4822834645669289433 ) ) ;
#64703 = CARTESIAN_POINT ( 'NONE',  ( 5.785732909357575061E-17, -0.4724409448818898682, -0.7086614173228346081 ) ) ;
#64704 = CARTESIAN_POINT ( 'NONE',  ( -0.4682703957577433740, 1.459763210197655647, 3.909061675276500392 ) ) ;
#64705 = CARTESIAN_POINT ( 'NONE',  ( 0.3917322834645670104, 2.398668435337828261E-17, -0.1102362204724409017 ) ) ;
#64706 = CARTESIAN_POINT ( 'NONE',  ( -0.1049643490035301885, -0.3917322834645671215, -2.204068241469816503 ) ) ;
#64707 = CARTESIAN_POINT ( 'NONE',  ( -0.07217847769028787330, -0.05778040916215522460, 0.4822834645669289988 ) ) ;
#64708 = CARTESIAN_POINT ( 'NONE',  ( -1.574803149606298192, -0.1870078740157480601, -0.3641732283464567677 ) ) ;
#64709 = CARTESIAN_POINT ( 'NONE',  ( -0.8530183727034112984, -0.4281496062992127816, -0.4176697321401328100 ) ) ;
#64710 = CARTESIAN_POINT ( 'NONE',  ( 0.3458507752293908943, -0.3458507752293908943, -2.852362204724409711 ) ) ;
#64712 = CARTESIAN_POINT ( 'NONE',  ( -0.2262115530851587786, -2.191421614605370878E-15, 0.4445507791589071167 ) ) ;
#64711 = CARTESIAN_POINT ( 'NONE',  ( -1.377952755905511140, 0.2952755905511811885, 0.000000000000000000 ) ) ;
#64713 = CARTESIAN_POINT ( 'NONE',  ( -1.056430446194224881, 0.2952755905511810774, -0.1292274648535930714 ) ) ;
#64714 = CARTESIAN_POINT ( 'NONE',  ( -0.3412073490813641308, -0.6046776061558807314, 0.2411417322834647770 ) ) ;
#64715 = CARTESIAN_POINT ( 'NONE',  ( -0.1974969037888706924, 0.3420746716998658843, -2.767060367454068803 ) ) ;
#64716 = CARTESIAN_POINT ( 'NONE',  ( 0.9711286089238851948, 0.1283753931104748280, 0.1820866141732283561 ) ) ;
#64717 = CARTESIAN_POINT ( 'NONE',  ( -0.05584411899101405369, 1.066260977814800670, -1.627668078129365314 ) ) ;
#64718 = CARTESIAN_POINT ( 'NONE',  ( 0.7414698162729663755, 0.1771653543307087630, 0.09757992244046791164 ) ) ;
#64719 = CARTESIAN_POINT ( 'NONE',  ( 1.292650918635171564, 0.1771653543307087630, 0.09757992244046791164 ) ) ;
#64720 = AXIS2_PLACEMENT_3D ( 'NONE', #69970, #29606, #55267 ) ;
#64721 = CARTESIAN_POINT ( 'NONE',  ( 1.437007874015748810, 0.1660481256975885056, 0.3530559997133364547 ) ) ;
#64722 = UNCERTAINTY_MEASURE_WITH_UNIT (LENGTH_MEASURE( 1.000000000000000082E-05 ), #2298, 'distance_accuracy_value', 'NONE');
#64723 = CARTESIAN_POINT ( 'NONE',  ( 0.2821522309711292364, 0.1771653543307087075, -0.09757992244046823083 ) ) ;
#64724 = CARTESIAN_POINT ( 'NONE',  ( 0.3917322834645669549, 0.1049643490035304660, -1.534120734908136052 ) ) ;
#64725 = CARTESIAN_POINT ( 'NONE',  ( -1.056430446194224881, -0.6692913385826771977, 0.1292274648535927661 ) ) ;
#64726 = CARTESIAN_POINT ( 'NONE',  ( 1.371391076115485719, -0.6692913385826773087, -0.1292274648535924053 ) ) ;
#64727 = CARTESIAN_POINT ( 'NONE',  ( 0.3458507752293908943, 0.3458507752293908943, -0.05708661417322836301 ) ) ;
#64728 = CARTESIAN_POINT ( 'NONE',  ( -0.5380577427821514602, -0.004921259842519576551, 0.3153832671262227771 ) ) ;
#64729 = DIRECTION ( 'NONE',  ( -0.000000000000000000, 1.000000000000000000, 0.000000000000000000 ) ) ;
#64730 = EDGE_CURVE ( 'NONE', #9834, #82476, #3761, .T. ) ;
#64731 = CARTESIAN_POINT ( 'NONE',  ( 0.2755905511811031494, 0.2952755905511811885, 0.000000000000000000 ) ) ;
#64732 = DIRECTION ( 'NONE',  ( -1.000000000000000000, -2.312964634635742464E-16, 0.000000000000000000 ) ) ;
#64733 = CARTESIAN_POINT ( 'NONE',  ( 0.7742782152230978099, -0.3690944881889763329, 0.3153832671262228327 ) ) ;
#64734 = CARTESIAN_POINT ( 'NONE',  ( 0.1049868766404206816, -0.5023911411419708095, -0.1820866141732282451 ) ) ;
#64735 = CARTESIAN_POINT ( 'NONE',  ( -0.2362204724409440182, -0.1870078740157479769, 0.4822834645669291653 ) ) ;
#64736 = CARTESIAN_POINT ( 'NONE',  ( -1.325459317585300889, -0.4281496062992127816, -0.4176697321401328100 ) ) ;
#64737 = CARTESIAN_POINT ( 'NONE',  ( -0.5839895013123351797, -0.5511811023622046335, 0.09757992244046803654 ) ) ;
#64738 = FACE_OUTER_BOUND ( 'NONE', #8379, .T. ) ;
#64739 = CARTESIAN_POINT ( 'NONE',  ( -0.9908136482939626788, 0.2952755905511811885, 0.1292274648535926551 ) ) ;
#64740 = CARTESIAN_POINT ( 'NONE',  ( -9.787531504996566615E-17, 0.3996062992125985480, -1.179133858267716661 ) ) ;
#64741 = CARTESIAN_POINT ( 'NONE',  ( -0.1958661417322834220, -0.3392501089628018884, -2.512467191601049699 ) ) ;
#64742 = CARTESIAN_POINT ( 'NONE',  ( -0.006561679790025524116, -0.2845877964562159024, 0.3641732283464567677 ) ) ;
#64743 = CARTESIAN_POINT ( 'NONE',  ( -0.7217847769028863381, -0.4281496062992124485, 0.4176697321401328655 ) ) ;
#64744 = CARTESIAN_POINT ( 'NONE',  ( -0.9186351706036736120, -0.6046776061558809534, -0.2411417322834644161 ) ) ;
#64745 = CARTESIAN_POINT ( 'NONE',  ( -1.286089238845143479, 0.1283753931104746893, -0.1820866141732285504 ) ) ;
#64746 = DIRECTION ( 'NONE',  ( 0.000000000000000000, 1.000000000000000000, 0.000000000000000000 ) ) ;
#64747 = CARTESIAN_POINT ( 'NONE',  ( -1.049868766404198794, -0.5023911411419708095, 0.1820866141732285504 ) ) ;
#64748 = CARTESIAN_POINT ( 'NONE',  ( -1.522309711286088607, 0.1283753931104746893, -0.1820866141732285504 ) ) ;
#64749 = CARTESIAN_POINT ( 'NONE',  ( 1.161417322834646271, 0.1660481256975883668, -0.3530559997133364547 ) ) ;
#64750 = CARTESIAN_POINT ( 'NONE',  ( 0.4724409448818898682, 2.892866454678787531E-17, -0.7480314960629921295 ) ) ;
#64751 = CARTESIAN_POINT ( 'NONE',  ( 0.1049643490035303967, 0.3917322834645670659, -2.509861835466878244 ) ) ;
#64752 = EDGE_LOOP ( 'NONE', ( #81179, #27392, #72342, #55378 ) ) ;
#64753 = DIRECTION ( 'NONE',  ( -0.000000000000000000, -1.000000000000000000, -0.000000000000000000 ) ) ;
#64754 = CARTESIAN_POINT ( 'NONE',  ( 1.541994750656168645, -0.5511811023622046335, 0.09757992244046803654 ) ) ;
#64755 = CARTESIAN_POINT ( 'NONE',  ( -1.227034120734907585, 0.2952755905511811885, 0.1292274648535926551 ) ) ;
#64756 = CARTESIAN_POINT ( 'NONE',  ( 1.443569553805774897, 0.2306618581243848609, 0.2411417322834645549 ) ) ;
#64757 = CARTESIAN_POINT ( 'NONE',  ( -0.1958661417322836718, 0.3392501089628017219, -1.987532808398950079 ) ) ;
#64758 = CARTESIAN_POINT ( 'NONE',  ( 1.587926509186352586, -0.3690944881889765550, -0.3153832671262227771 ) ) ;
#64759 = CARTESIAN_POINT ( 'NONE',  ( 0.5839895013123367340, 0.2952755905511811885, 0.1292274648535926551 ) ) ;
#64760 = CARTESIAN_POINT ( 'NONE',  ( 0.1574803149606306130, -0.1870078740157480879, -0.4822834645669291653 ) ) ;
#64761 = CARTESIAN_POINT ( 'NONE',  ( 0.03098326503090165565, 1.062992125984251635, -3.937007874015749920 ) ) ;
#64762 = CARTESIAN_POINT ( 'NONE',  ( -0.3996062992125986035, 0.1070741851644051584, -2.629265091863516979 ) ) ;
#64763 = CARTESIAN_POINT ( 'NONE',  ( 0.8923884514435701520, -0.5023911411419708095, -0.1820866141732282451 ) ) ;
#64764 = CARTESIAN_POINT ( 'NONE',  ( 0.3996062992125986590, -0.1070741851644053111, -1.371391076115485053 ) ) ;
#64765 = ORIENTED_EDGE ( 'NONE', *, *, #40849, .T. ) ;
#64766 = CARTESIAN_POINT ( 'NONE',  ( 0.3392501089628018884, -0.1958661417322833942, -0.1017253525272460019 ) ) ;
#64767 = ORIENTED_EDGE ( 'NONE', *, *, #57587, .T. ) ;
#64768 = CARTESIAN_POINT ( 'NONE',  ( 0.1574803149606306130, -0.1870078740157479769, 0.4822834645669291653 ) ) ;
#64769 = CARTESIAN_POINT ( 'NONE',  ( -1.555118110236219930, -0.5400638737290845981, -0.3530559997133363437 ) ) ;
#64770 = CARTESIAN_POINT ( 'NONE',  ( 0.6824146981627303710, -0.6046776061558807314, 0.2411417322834647770 ) ) ;
#64771 = CARTESIAN_POINT ( 'NONE',  ( 1.384514435695538559, 0.2952755905511810774, -0.1292274648535930714 ) ) ;
#64772 = CARTESIAN_POINT ( 'NONE',  ( 1.469816272965879911, 0.2306618581243847221, -0.2411417322834647770 ) ) ;
#64773 = CARTESIAN_POINT ( 'NONE',  ( -0.4461942257217840213, -0.6046776061558809534, -0.2411417322834644161 ) ) ;
#64774 = CARTESIAN_POINT ( 'NONE',  ( -0.01968503937007793844, -0.5400638737290844871, 0.3530559997133364547 ) ) ;
#64775 = CARTESIAN_POINT ( 'NONE',  ( 1.607611548556431069, 0.2952755905511811885, 0.1292274648535926551 ) ) ;
#64776 = AXIS2_PLACEMENT_3D ( 'NONE', #75430, #50956, #76653 ) ;
#64777 = CARTESIAN_POINT ( 'NONE',  ( 1.404199475065617264, -0.4281496062992124485, 0.4176697321401328655 ) ) ;
#64778 = CARTESIAN_POINT ( 'NONE',  ( 1.371391076115485941, 0.2952755905511811885, 0.1292274648535926551 ) ) ;
#64779 = CARTESIAN_POINT ( 'NONE',  ( -0.3280839895013117347, -0.4281496062992124485, 0.4176697321401328655 ) ) ;
#64780 = CARTESIAN_POINT ( 'NONE',  ( -0.2867679344610364334, -0.2867679344610367109, -0.3661417322834645827 ) ) ;
#64781 = CARTESIAN_POINT ( 'NONE',  ( 0.3871391076115493490, -0.2845877964562159024, 0.3641732283464567677 ) ) ;
#64782 = VERTEX_POINT ( 'NONE', #62258 ) ;
#64783 = CARTESIAN_POINT ( 'NONE',  ( 0.1974969037888704704, 0.3420746716998660508, -0.6167979002624671692 ) ) ;
#64784 = ORIENTED_EDGE ( 'NONE', *, *, #16008, .F. ) ;
#64785 = CARTESIAN_POINT ( 'NONE',  ( -0.5643044619422565855, -0.004921259842519870586, -0.3153832671262229437 ) ) ;
#64786 = DIRECTION ( 'NONE',  ( 0.000000000000000000, 0.000000000000000000, 1.000000000000000000 ) ) ;
#64787 = CARTESIAN_POINT ( 'NONE',  ( 0.05905511811023681640, 0.1660481256975883668, -0.3530559997133364547 ) ) ;
#64788 = CARTESIAN_POINT ( 'NONE',  ( 0.1049868766404206816, -0.6046776061558809534, -0.2411417322834644161 ) ) ;
#64789 = CARTESIAN_POINT ( 'NONE',  ( -1.056430446194224881, 0.2952755905511810774, -0.1292274648535930714 ) ) ;
#64790 = CARTESIAN_POINT ( 'NONE',  ( -0.2867679344610365444, -0.2867679344610367664, -1.630596743603361265 ) ) ;
#64791 = CARTESIAN_POINT ( 'NONE',  ( -1.561679790026246017, -0.4281496062992127816, -0.4176697321401328100 ) ) ;
#64792 = DIRECTION ( 'NONE',  ( 0.000000000000000000, 0.000000000000000000, 1.000000000000000000 ) ) ;
#64793 = CARTESIAN_POINT ( 'NONE',  ( 0.7874015748031503170, -0.1870078740157479769, 0.3641732283464567677 ) ) ;
#64794 = CARTESIAN_POINT ( 'NONE',  ( 0.3018372703412079971, 0.05413385826771626580, -0.4176697321401330321 ) ) ;
#64795 = CARTESIAN_POINT ( 'NONE',  ( 0.8727034120734913358, -0.05778040916215522460, 0.4822834645669289988 ) ) ;
#64796 = CARTESIAN_POINT ( 'NONE',  ( 0.1998031496062992740, 0.3460692066303959757, -1.246719160104986734 ) ) ;
#64797 = CARTESIAN_POINT ( 'NONE',  ( -1.673228346456691717, 0.1660481256975883668, -0.3530559997133364547 ) ) ;
#64798 = CARTESIAN_POINT ( 'NONE',  ( 0.3996062992125984925, 0.1070741851644054637, -0.6738845144356955252 ) ) ;
#64799 = CARTESIAN_POINT ( 'NONE',  ( 0.1070741851644054776, -0.3996062992125984925, -0.3195538057742782212 ) ) ;
#64800 = CARTESIAN_POINT ( 'NONE',  ( -0.1837270341207343505, -0.6046776061558807314, 0.2411417322834647770 ) ) ;
#64801 = CARTESIAN_POINT ( 'NONE',  ( 0.1070741851644053527, 0.3996062992125986590, -2.670603674540682260 ) ) ;
#64802 = CARTESIAN_POINT ( 'NONE',  ( 0.3917322834645670104, 2.398668435337828261E-17, -2.092519685039370358 ) ) ;
#64803 = CARTESIAN_POINT ( 'NONE',  ( -1.259842519685038686, -0.1870078740157480601, -0.3641732283464567677 ) ) ;
#64804 = CARTESIAN_POINT ( 'NONE',  ( 1.167979002624672580, 0.05413385826771626580, -0.4176697321401330321 ) ) ;
#64805 = CARTESIAN_POINT ( 'NONE',  ( 1.358267716535433323, 0.1660481256975885056, 0.3530559997133364547 ) ) ;
#64806 = CARTESIAN_POINT ( 'NONE',  ( 0.1837270341207357105, -0.5023911411419708095, -0.1820866141732282451 ) ) ;
#64807 = CARTESIAN_POINT ( 'NONE',  ( 0.3477690288713918276, 0.2952755905511811885, 0.1292274648535926551 ) ) ;
#64808 = CARTESIAN_POINT ( 'NONE',  ( -0.2362204724409447953, -0.4091458600556404646, -1.559711286089238591 ) ) ;
#64809 = CARTESIAN_POINT ( 'NONE',  ( 0.3871391076115493490, -0.2845877964562159024, 0.3641732283464567677 ) ) ;
#64810 = CARTESIAN_POINT ( 'NONE',  ( -0.1377952755905504645, 0.1660481256975885056, 0.3530559997133364547 ) ) ;
#64811 = CARTESIAN_POINT ( 'NONE',  ( -0.3949938075777409963, -7.255918531996591613E-17, -1.375984251968503713 ) ) ;
#64812 = CARTESIAN_POINT ( 'NONE',  ( -1.423884514435694859, -0.3162353388693405765, 0.4822834645669290543 ) ) ;
#64813 = CARTESIAN_POINT ( 'NONE',  ( 0.6561679790026253567, 0.1283753931104748280, 0.1820866141732283561 ) ) ;
#64814 = DIRECTION ( 'NONE',  ( -0.000000000000000000, -1.000000000000000000, -0.000000000000000000 ) ) ;
#64815 = CARTESIAN_POINT ( 'NONE',  ( -0.7283464566929126471, 0.1660481256975883668, -0.3530559997133364547 ) ) ;
#64816 = CARTESIAN_POINT ( 'NONE',  ( -0.1181102362204717315, -0.5511811023622047445, 6.969142054262312111E-17 ) ) ;
#64817 = DIRECTION ( 'NONE',  ( -1.000000000000000000, -0.000000000000000000, -0.000000000000000000 ) ) ;
#64818 = CARTESIAN_POINT ( 'NONE',  ( -0.9383202099737524282, -0.05778040916215522460, 0.4822834645669289988 ) ) ;
#64819 = CARTESIAN_POINT ( 'NONE',  ( -0.2230971128608915943, 0.05413385826771666132, 0.4176697321401328100 ) ) ;
#64820 = CARTESIAN_POINT ( 'NONE',  ( 0.2230971128608929543, -0.004921259842519870586, -0.3153832671262229437 ) ) ;
#64821 = B_SPLINE_CURVE_WITH_KNOTS ( 'NONE', 3,
 ( #6988, #72229, #33082, #65074, #685, #57900, #77707, #14158, #53259, #44843, #70540, #39814 ),
 .UNSPECIFIED., .F., .F.,
 ( 4, 2, 2, 2, 2, 4 ),
 ( 0.007992874908874613230, 0.009303755029336854485, 0.01061463514979909574, 0.01192551527026133873, 0.01258095533049245415, 0.01323639539072356958 ),
 .UNSPECIFIED. ) ;
#64822 = CARTESIAN_POINT ( 'NONE',  ( -0.3996062992125986590, 0.1070741851644051723, -2.314304461942256808 ) ) ;
#64823 = CARTESIAN_POINT ( 'NONE',  ( -0.02624671916010428221, 0.2306618581243847221, -0.2411417322834647770 ) ) ;
#64824 =( BOUNDED_CURVE ( )  B_SPLINE_CURVE ( 2, ( #12029, #57856, #14111, #19994, #51957, #70929, #44802, #40184, #71340, #224, #51125, #27131, #13274 ),
 .UNSPECIFIED., .F., .F. ) 
 B_SPLINE_CURVE_WITH_KNOTS ( ( 3, 2, 2, 2, 2, 2, 3 ),
 ( 0.8625000000000000444, 0.8666666666666666963, 0.8708333333333333481, 0.8750000000000001110, 0.8791666666666667629, 0.8833333333333334147, 0.8875000000000000666 ),
 .UNSPECIFIED. ) 
 CURVE ( )  GEOMETRIC_REPRESENTATION_ITEM ( )  RATIONAL_B_SPLINE_CURVE ( ( 1.000000000000000000, 0.9659258262890683122, 1.000000000000000000, 0.9659258262890683122, 1.000000000000000000, 0.9659258262890683122, 1.000000000000000000, 0.9659258262890683122, 1.000000000000000000, 0.9659258262890683122, 1.000000000000000000, 0.9659258262890674240, 1.000000000000000888 ) ) 
 REPRESENTATION_ITEM ( '' )  );
#64825 = EDGE_CURVE ( 'NONE', #1879, #9013, #49621, .T. ) ;
#64826 = CARTESIAN_POINT ( 'NONE',  ( -0.1049643490035306742, 0.3917322834645668994, -1.976358636974066663 ) ) ;
#64827 = CARTESIAN_POINT ( 'NONE',  ( 0.7939632545931766261, -0.2845877964562161244, -0.3641732283464567121 ) ) ;
#64828 = CARTESIAN_POINT ( 'NONE',  ( 1.555118110236221041, -0.5400638737290844871, 0.3530559997133364547 ) ) ;
#64829 = CARTESIAN_POINT ( 'NONE',  ( -0.7808398950131225646, -0.08942795157527998196, 0.3641732283464567121 ) ) ;
#64830 = CARTESIAN_POINT ( 'NONE',  ( -1.351706036745406347, -0.004921259842519870586, -0.3153832671262229437 ) ) ;
#64831 = EDGE_CURVE ( 'NONE', #48423, #80, #31503, .T. ) ;
#64832 = CARTESIAN_POINT ( 'NONE',  ( -0.7742782152230962556, -0.4281496062992127816, -0.4176697321401328100 ) ) ;
#64833 = CARTESIAN_POINT ( 'NONE',  ( -0.1312335958005241554, 0.2306618581243848609, 0.2411417322834645549 ) ) ;
#64834 = CARTESIAN_POINT ( 'NONE',  ( 0.3608923884514443348, -0.5511811023622046335, 0.09757992244046803654 ) ) ;
#64835 = CARTESIAN_POINT ( 'NONE',  ( -0.4724409448818898682, -8.678599364036362592E-17, -2.401574803149606474 ) ) ;
#64836 = CARTESIAN_POINT ( 'NONE',  ( 0.9973753280839902091, 0.1283753931104746893, -0.1820866141732285504 ) ) ;
#64837 = CARTESIAN_POINT ( 'NONE',  ( 0.1377952755905518800, 0.1660481256975883668, -0.3530559997133364547 ) ) ;
#64838 = CARTESIAN_POINT ( 'NONE',  ( -1.436417322834644850, 0.4405861044731111953, 0.3149606299212598381 ) ) ;
#64839 = CARTESIAN_POINT ( 'NONE',  ( -0.3477690288713905509, -0.6692913385826771977, 0.1292274648535927661 ) ) ;
#64840 = CARTESIAN_POINT ( 'NONE',  ( 0.1958661417322836440, -0.3392501089628017219, -1.436351706036745446 ) ) ;
#64841 = CARTESIAN_POINT ( 'NONE',  ( 1.469816272965879911, 0.1283753931104746893, -0.1820866141732285504 ) ) ;
#64842 = CARTESIAN_POINT ( 'NONE',  ( 0.6561679790026253567, -0.6046776061558809534, -0.2411417322834644161 ) ) ;
#64843 = CARTESIAN_POINT ( 'NONE',  ( 0.2034120734908144990, -0.6692913385826771977, 0.1292274648535927661 ) ) ;
#64844 = CARTESIAN_POINT ( 'NONE',  ( 1.114295247146197099, 1.650914051239646151E-16, 0.3627985898453514046 ) ) ;
#64845 = CARTESIAN_POINT ( 'NONE',  ( 0.006561679790026889343, -0.2845877964562161244, -0.3641732283464567121 ) ) ;
#64846 = CARTESIAN_POINT ( 'NONE',  ( 0.8464566929133866546, -0.5400638737290844871, 0.3530559997133364547 ) ) ;
#64847 = CARTESIAN_POINT ( 'NONE',  ( -0.3805774278215216522, -0.3690944881889765550, -0.3153832671262227771 ) ) ;
#64848 = CARTESIAN_POINT ( 'NONE',  ( -0.6364829396325453192, -0.05778040916215560624, -0.4822834645669293319 ) ) ;
#64849 = CARTESIAN_POINT ( 'NONE',  ( 0.8136482939632553313, 0.2306618581243848609, 0.2411417322834645549 ) ) ;
#64850 = CARTESIAN_POINT ( 'NONE',  ( -0.2755905511811018171, 0.2952755905511811885, 0.000000000000000000 ) ) ;
#64851 = VERTEX_POINT ( 'NONE', #63496 ) ;
#64852 = CARTESIAN_POINT ( 'NONE',  ( -1.141732283464566011, 0.2952755905511811885, 0.000000000000000000 ) ) ;
#64853 = CARTESIAN_POINT ( 'NONE',  ( -0.8136482939632537770, -0.5023911411419708095, 0.1820866141732285504 ) ) ;
#64854 = CARTESIAN_POINT ( 'NONE',  ( 0.1377952755905518800, -0.5400638737290844871, 0.3530559997133364547 ) ) ;
#64855 = CARTESIAN_POINT ( 'NONE',  ( -1.213910761154854745, 0.2952755905511810774, -0.1292274648535930714 ) ) ;
#64856 = CARTESIAN_POINT ( 'NONE',  ( -0.7349081364829387342, -0.6046776061558807314, 0.2411417322834647770 ) ) ;
#64857 = CARTESIAN_POINT ( 'NONE',  ( -1.881759086957760285, 2.742776672516394232, 0.5314960629921260393 ) ) ;
#64859 = CARTESIAN_POINT ( 'NONE',  ( 1.437007874015748810, 0.1660481256975885056, 0.3530559997133364547 ) ) ;
#64858 = CARTESIAN_POINT ( 'NONE',  ( 0.000000000000000000, 0.000000000000000000, 0.000000000000000000 ) ) ;
#64860 = CARTESIAN_POINT ( 'NONE',  ( 1.181102362204725198, -0.1870078740157479769, 0.4822834645669291653 ) ) ;
#64861 = CARTESIAN_POINT ( 'NONE',  ( 0.3917322834645669549, 0.1049643490035304660, -2.479002624671915900 ) ) ;
#64862 = DIRECTION ( 'NONE',  ( -3.096699300667737957E-16, 1.000000000000000000, -0.000000000000000000 ) ) ;
#64863 = CARTESIAN_POINT ( 'NONE',  ( -1.279527559055116948, -0.5400638737290844871, 0.3530559997133364547 ) ) ;
#64864 = CARTESIAN_POINT ( 'NONE',  ( -0.4091458600556405756, 0.2362204724409446288, -0.9711286089238845287 ) ) ;
#64865 = CARTESIAN_POINT ( 'NONE',  ( 0.3460692066303959202, 0.1998031496062993295, -0.1312335958005249603 ) ) ;
#64866 = VERTEX_POINT ( 'NONE', #5426 ) ;
#64867 = CARTESIAN_POINT ( 'NONE',  ( -0.1115485564304453947, -0.5511811023622046335, 0.09757992244046803654 ) ) ;
#64868 = CARTESIAN_POINT ( 'NONE',  ( 0.1049643490035304938, -0.3917322834645669549, -1.967191601049868899 ) ) ;
#64869 = EDGE_LOOP ( 'NONE', ( #64767, #63293, #71489 ) ) ;
#64870 = CARTESIAN_POINT ( 'NONE',  ( 0.2887139107611556010, -0.6046776061558807314, 0.2411417322834647770 ) ) ;
#64871 = CARTESIAN_POINT ( 'NONE',  ( 0.4068241469816279987, -0.4281496062992127816, -0.4176697321401328100 ) ) ;
#64872 = CARTESIAN_POINT ( 'NONE',  ( 0.2362204724409451007, -0.4091458600556402980, -2.926509186351706315 ) ) ;
#64873 = FACE_OUTER_BOUND ( 'NONE', #76489, .T. ) ;
#64874 = CARTESIAN_POINT ( 'NONE',  ( -0.9317585301837263412, -0.3690944881889765550, -0.3153832671262227771 ) ) ;
#64875 = DIRECTION ( 'NONE',  ( -0.000000000000000000, -1.000000000000000000, -0.000000000000000000 ) ) ;
#64876 = CARTESIAN_POINT ( 'NONE',  ( 0.6233595800524942554, -0.05778040916215560624, -0.4822834645669293319 ) ) ;
#64877 = CARTESIAN_POINT ( 'NONE',  ( 0.9186351706036751663, -0.5023911411419708095, 0.1820866141732285504 ) ) ;
#64878 = CARTESIAN_POINT ( 'NONE',  ( -0.3083989501312330295, -0.3162353388693409650, -0.4822834645669289433 ) ) ;
#64879 = CARTESIAN_POINT ( 'NONE',  ( 0.3392501089628018329, 0.1958661417322835052, -1.313628978181415441 ) ) ;
#64880 = CARTESIAN_POINT ( 'NONE',  ( -0.9448818897637790704, -0.1870078740157480879, -0.4822834645669291653 ) ) ;
#64881 = FACE_OUTER_BOUND ( 'NONE', #59362, .T. ) ;
#64882 = CARTESIAN_POINT ( 'NONE',  ( -0.8530183727034112984, -0.4281496062992127816, -0.4176697321401328100 ) ) ;
#64883 = CARTESIAN_POINT ( 'NONE',  ( 1.292650918635171564, -0.6692913385826773087, -0.1292274648535924053 ) ) ;
#64884 = CARTESIAN_POINT ( 'NONE',  ( 1.640419947506562393, -0.3690944881889763329, 0.3153832671262228327 ) ) ;
#64885 = ORIENTED_EDGE ( 'NONE', *, *, #24432, .T. ) ;
#64886 = CARTESIAN_POINT ( 'NONE',  ( -0.1958661417322833942, -0.3392501089628018884, -2.424559998196537336 ) ) ;
#64887 = CARTESIAN_POINT ( 'NONE',  ( -0.2099737532808391705, 0.2306618581243848609, 0.2411417322834645549 ) ) ;
#64888 = ORIENTED_EDGE ( 'NONE', *, *, #60494, .T. ) ;
#64889 = CARTESIAN_POINT ( 'NONE',  ( -0.7545931758530177724, 0.2952755905511811885, 0.1292274648535926551 ) ) ;
#64890 = CARTESIAN_POINT ( 'NONE',  ( 1.587926509186352142, 0.05413385826771666132, 0.4176697321401328100 ) ) ;
#64891 = CARTESIAN_POINT ( 'NONE',  ( 1.384514435695538337, -0.6692913385826771977, 0.1292274648535927661 ) ) ;
#64892 = CARTESIAN_POINT ( 'NONE',  ( 0.3083989501312343062, -0.3162353388693405765, 0.4822834645669290543 ) ) ;
#64893 = AXIS2_PLACEMENT_3D ( 'NONE', #42752, #68036, #54136 ) ;
#64894 = ADVANCED_FACE ( 'NONE', ( #5830 ), #31981, .F. ) ;
#64895 = CARTESIAN_POINT ( 'NONE',  ( -0.3412073490813641308, 0.2306618581243847221, -0.2411417322834647770 ) ) ;
#64896 = CARTESIAN_POINT ( 'NONE',  ( 0.1049643490035303689, 0.3917322834645670104, -1.967847769028871374 ) ) ;
#64897 = CARTESIAN_POINT ( 'NONE',  ( -1.358267716535432434, 0.1660481256975883668, -0.3530559997133364547 ) ) ;
#64898 = CARTESIAN_POINT ( 'NONE',  ( -0.01312335958005186876, 0.05413385826771626580, -0.4176697321401330321 ) ) ;
#64899 = CARTESIAN_POINT ( 'NONE',  ( -0.2755905511811015396, -0.5511811023622047445, 6.969142054262312111E-17 ) ) ;
#64900 = CARTESIAN_POINT ( 'NONE',  ( 1.601049868766404982, -0.6046776061558809534, -0.2411417322834644161 ) ) ;
#64901 = CARTESIAN_POINT ( 'NONE',  ( 1.410761154855643795, -0.05778040916215560624, -0.4822834645669293319 ) ) ;
#64902 = CARTESIAN_POINT ( 'NONE',  ( -0.3280839895013117347, -0.4281496062992124485, 0.4176697321401328655 ) ) ;
#64903 = CARTESIAN_POINT ( 'NONE',  ( -0.5314960629921393620, 2.755905511811024056, 3.826707563893390951 ) ) ;
#64904 = CARTESIAN_POINT ( 'NONE',  ( 1.233595800524935227, -0.6046776061558807314, 0.2411417322834647770 ) ) ;
#64905 = CARTESIAN_POINT ( 'NONE',  ( 3.908320185825791881, 1.537401574803149984, -0.4744094488188970171 ) ) ;
#64906 = ORIENTED_EDGE ( 'NONE', *, *, #42986, .T. ) ;
#64907 =( BOUNDED_SURFACE ( )  B_SPLINE_SURFACE ( 1, 2, ( 
 ( #19650, #71007, #64688, #7027, #32696, #53298, #53711, #66791, #21330, #33954, #54127, #21738, #79010, #3219, #22575, #60040, #54544, #22981, #73092, #79841, #15868, #41920, #48648, #80259, #3632, #29300, #47402, #28053, #22158, #47817, #1972, #74343, #16275, #54962, #34375, #9126, #28466, #2396, #80669, #16689, #60865, #9944, #79418, #35616, #73519, #9533, #46982, #15442, #41516, #35204, #72676, #42328, #15025, #40681, #67201, #28881, #34796, #59618, #8704, #66366, #41103, #48236, #60456, #73932, #2807, #27636, #67613, #61279, #8288, #30119, #43148, #81076, #10371, #30537, #81489, #55371, #62943, #82307, #36438, #30940, #82710, #49478, #56201, #75584, #18333, #25030, #56607, #63345, #5680, #23805, #4454, #81902, #24213, #61703, #50703, #75991, #31348, #10778, #68845, #4863, #62111, #57014, #76401, #37267, #69670, #55781, #12013, #49884, #69261, #23393, #75171, #17923, #11608, #49060, #18733, #74759, #29708, #43560, #5277, #11191, #36029, #68438, #17107, #17516, #24626, #36852, #50293, #62525, #4043, #43973, #37667, #68027, #42742, #65010, #19136, #58260, #207, #1049, #70911, #38497, #51942, #51108, #83123, #26703, #13261, #52779, #38079, #19979, #6094, #44375, #78488, #52358, #64180, #76805, #39325, #39748, #78065, #77647, #26281, #63754, #625, #45211, #25860, #38911, #20395, #64591, #45630, #6927, #70067, #65444, #25442, #12422, #71324, #51519, #7776, #44785, #31769, #58684, #33014, #57430, #77223, #46048, #32598, #27116, #71741, #70482, #59104, #12839, #1459, #33444, #13673, #6514, #32184, #57839, #19552, #7346, #14096, #21225, #33852, #40581, #60356, #46880, #3115, #14921, #14516, #54025, #22052, #72574, #67098, #41414, #78904, #34693, #59935, #60765, #47297, #66261, #28363, #27534, #59517, #28781, #72986, #29198, #40169, #79736, #65853, #20812, #54865, #54444, #8601, #53191, #15761, #16171, #80155, #47713, #2703, #8186, #73413, #21637, #2290, #15338, #22473, #41002, #9429, #66684, #46467, #41816, #1872, #72161, #35098, #27951, #67507, #34273, #53610, #48133, #73831, #79318, #9020, #9843, #35514, #3532, #61178, #82106, #13053, #74243, #38706, #45001, #37880, #17720, #48544, #64385, #18127, #70700, #43347, #43759, #56811, #11398, #22881, #44179, #11817, #69049, #76606, #12631, #50089, #44584, #6721, #63143, #69871, #5889, #31979, #32391, #70278, #77019, #19352, #37470, #69465, #12223, #63555, #37055, #80570, #6303, #62739, #24419, #82510, #18535, #75785, #5075, #30744, #50905, #2, #5484, #25654, #31561, #82920, #56407, #31145, #57218, #25240, #24826, #50494, #76197, #18936, #38290, #63966, #57639, #51316, #1673, #13464, #47098, #39121, #19772, #65663, #7990, #1266, #26076, #58481, #71121, #77861, #14315, #846, #40382, #52156, #51736, #33654, #59317, #26503, #21027, #78703, #32814, #71961, #13887, #14730, #26914, #20190, #27330, #64802, #7141, #66065, #52574, #66478, #77438, #52990, #45425, #58054, #8813, #8401, #45841, #71540, #46687, #53415, #34068, #72380, #39974, #39546, #59732, #58906, #65235, #78283, #2086, #20614, #27751, #46266, #420, #79124, #7572, #33245, #21441, #72787, #15137, #40793, #60155, #48757, #23090, #28166, #41622, #74456, #60978, #17219, #36138, #34906, #49170, #53823, #74875, #81186, #74038, #79537, #2507, #42851, #54240, #23503, #21850, #79957, #9646, #47514, #73206, #80369, #47929, #15556, #29407, #16803, #2920, #80774, #68544, #15975, #22682, #42032, #68139, #34489, #42439, #29815, #55476, #73633, #22270, #48341, #16385, #41215, #66903, #10484, #9234, #60569, #35315, #54658, #28584, #67311, #3328, #3743, #61810, #28992, #4150, #67726, #35724, #10061, #61394, #55066, #50813, #44087, #76101, #30230, #50404, #11724, #49996, #63051, #76514, #31051, #18445, #5389, #36545, #6205, #49586, #62221, #69781, #75693, #31883, #75281, #4559, #25145 ),
 ( #55892, #81604, #25555, #30650, #57543, #23920, #56314, #69370, #17624, #43256, #56720, #24326, #68953, #5794, #18843, #62639, #57126, #51222, #18034, #82417, #12126, #44489, #76920, #82820, #83234, #19248, #43668, #82012, #24736, #37783, #11303, #44900, #70180, #10885, #36962, #37380, #63460, #4983, #31464, #12533, #38193, #63868, #64705, #14630, #1167, #71863, #25976, #7045, #26818, #14213, #51634, #59632, #77339, #32294, #78184, #20515, #13789, #38610, #71024, #322, #32714, #52476, #13368, #52893, #58381, #64288, #46167, #39871, #39021, #33555, #7894, #45329, #65560, #26400, #27234, #39446, #742, #59218, #19667, #52057, #78606, #65134, #79026, #6623, #1579, #57954, #70598, #21345, #20929, #77763, #20095, #46585, #65967, #33138, #72284, #40286, #45746, #71441, #7470, #8304, #58810, #33971, #1988, #27651, #53313, #12952, #46998, #34810, #9960, #21752, #22995, #29313, #8717, #60881, #61292, #53725, #74358, #15457, #79855, #79433, #67214, #9547, #22587, #35217, #47415, #54141, #3647, #41528, #66804, #34388, #41115, #60053, #48248, #2820, #9139, #54558, #2409, #3232, #28067, #41933, #60469, #28481, #73106, #80681, #73533, #54974, #22172, #16289, #35631, #48660, #72692, #73944, #15039, #47830, #15880, #28896, #40695, #67628, #80272, #66380, #26670, #72542, #45596, #46432, #72124, #14889, #26247, #34238, #78867, #40136, #33409, #8568, #52325, #51906, #39290, #71290, #40549, #14482, #21193, #8154, #1839, #59899, #77613, #46011, #46847, #65821, #58224, #19946, #59485, #66230, #59071, #72953, #64976, #1017, #33819, #13637, #78031, #27499, #7313, #38876, #53576, #53155, #2251, #27917, #65406, #32982, #21603, #20361, #32561, #47263, #27082, #79285, #71707, #64554, #58650, #14061, #6892, #591, #52744, #39715, #7744, #1426, #78452, #20778, #31336, #51507, #32171, #30524, #83111, #63332, #63743, #44363, #24200, #43547, #62929, #6082, #69247, #70055, #50690, #57001, #17911, #82698, #17503, #56594, #76793, #11594, #57827, #38484, #62511, #76388, #44773, #49871, #25847, #37254, #69656, #75571, #25017, #18721, #31756, #12409, #5263, #18318, #70470, #38067, #30927, #4849, #82294, #56187, #57418, #24613, #50280, #25430, #81889, #51095, #75978, #19124, #43960, #12000, #37654, #6501, #5669, #64168, #12827, #195, #43135, #68831, #11178, #36838, #72565, #45620, #77637, #33005, #8592, #33843, #45197, #14912, #65001, #27524, #615, #1450, #27107, #53180, #64578, #40572, #59509, #78478, #71732, #46871, #7337, #6916, #19969, #26271, #78895, #52770, #1863, #46458, #40160, #66253, #32587, #1040, #21216, #20802, #13250, #58250, #14507, #34264, #14087, #27942, #71314, #39314, #72152, #51932, #58675, #65844, #13662, #77211, #59924, #8177, #2279, #19540, #20386, #26694, #70900, #52349, #38899, #78056, #65435, #46037, #39739, #7768, #33434, #59095, #67917, #80144, #36328, #55258, #54017, #68333, #47288, #10672, #16993, #9833, #72977, #21627, #62003, #73401, #42636, #15329, #15752, #28772, #66674, #79309, #16159, #67088, #40994, #48532, #10254, #22045, #16577, #4339, #35089, #41806, #61168, #3938, #53600, #42222, #48951, #74652, #9420, #41405, #67498, #35504, #9012, #34684, #61592, #60348, #79728, #54434, #73822, #47705, #2695, #28355, #22871, #80967, #60756, #23281, #3519, #54855, #3107, #22465, #29188, #80560, #48125, #74233, #35925, #29597, #37562, #63236, #56498, #81378, #30421, #43039, #49774, #69560, #56089, #12315, #24105, #23691, #5576, #31242, #81794, #76297, #50589, #4748, #43857, #69146, #69961, #82200, #75474, #56908, #36734, #68735, #37973, #24518, #38387, #49365, #50184, #11077, #75061, #75881, #63648, #17815, #62409, #24922, #25335, #5987, #82604, #11908, #17409, #18627, #30833, #11496, #18222, #31658, #44270, #57316, #83013, #55669, #50998, #43448, #37150, #76696, #62835, #19030, #5169 ) ),
 .UNSPECIFIED., .F., .F., .F. ) 
 B_SPLINE_SURFACE_WITH_KNOTS ( ( 2, 2 ),
 ( 3, 2, 2, 2, 2, 2, 2, 2, 2, 2, 2, 2, 2, 2, 2, 2, 2, 2, 2, 2, 2, 2, 2, 2, 2, 2, 2, 2, 2, 2, 2, 2, 2, 2, 2, 2, 2, 2, 2, 2, 2, 2, 2, 2, 2, 2, 2, 2, 2, 2, 2, 2, 2, 2, 2, 2, 2, 2, 2, 2, 2, 2, 2, 2, 2, 2, 2, 2, 2, 2, 2, 2, 2, 2, 2, 2, 2, 2, 2, 2, 2, 2, 2, 2, 2, 2, 2, 2, 2, 2, 2, 2, 2, 2, 2, 2, 2, 2, 2, 2, 2, 2, 2, 2, 2, 2, 2, 2, 2, 2, 2, 2, 2, 2, 2, 2, 2, 2, 2, 2, 2, 2, 2, 2, 2, 2, 2, 2, 2, 2, 2, 2, 2, 2, 2, 2, 2, 2, 2, 2, 2, 2, 2, 2, 2, 2, 2, 2, 2, 2, 2, 2, 2, 2, 2, 2, 2, 2, 2, 2, 2, 2, 2, 2, 2, 2, 2, 2, 2, 2, 2, 2, 2, 2, 2, 2, 2, 2, 2, 2, 2, 2, 2, 2, 2, 2, 2, 2, 2, 2, 2, 2, 2, 2, 2, 2, 2, 2, 2, 2, 2, 2, 2, 2, 2, 2, 2, 2, 2, 2, 2, 2, 2, 2, 2, 2, 2, 2, 2, 2, 2, 2, 2, 2, 2, 2, 2, 2, 2, 2, 2, 2, 2, 2, 2, 2, 2, 3 ),
 ( 0.000000000000000000, 1.000000000000000000 ),
 ( 0.000000000000000000, 0.004166666666666666609, 0.008333333333333333218, 0.01250000000000000069, 0.01666666666666666644, 0.02083333333333333218, 0.02500000000000000139, 0.02916666666666666713, 0.03333333333333333287, 0.03749999999999999861, 0.04166666666666666435, 0.04583333333333333010, 0.05000000000000000278, 0.05416666666666666852, 0.05833333333333333426, 0.06250000000000000000, 0.06666666666666666574, 0.07083333333333333148, 0.07499999999999999722, 0.07916666666666666297, 0.08333333333333332871, 0.08749999999999999445, 0.09166666666666666019, 0.09583333333333333981, 0.1000000000000000056, 0.1041666666666666713, 0.1083333333333333370, 0.1125000000000000028, 0.1166666666666666685, 0.1208333333333333343, 0.1250000000000000000, 0.1291666666666666796, 0.1333333333333333315, 0.1375000000000000111, 0.1416666666666666630, 0.1458333333333333426, 0.1499999999999999944, 0.1541666666666666741, 0.1583333333333333259, 0.1625000000000000056, 0.1666666666666666574, 0.1708333333333333370, 0.1749999999999999889, 0.1791666666666666685, 0.1833333333333333204, 0.1875000000000000000, 0.1916666666666666796, 0.1958333333333333315, 0.2000000000000000111, 0.2041666666666666630, 0.2083333333333333426, 0.2124999999999999944, 0.2166666666666666741, 0.2208333333333333259, 0.2250000000000000056, 0.2291666666666666574, 0.2333333333333333370, 0.2374999999999999889, 0.2416666666666666685, 0.2458333333333333204, 0.2500000000000000000, 0.2541666666666666519, 0.2583333333333333592, 0.2625000000000000111, 0.2666666666666666630, 0.2708333333333333148, 0.2750000000000000222, 0.2791666666666666741, 0.2833333333333333259, 0.2874999999999999778, 0.2916666666666666852, 0.2958333333333333370, 0.2999999999999999889, 0.3041666666666666408, 0.3083333333333333481, 0.3125000000000000000, 0.3166666666666666519, 0.3208333333333333592, 0.3250000000000000111, 0.3291666666666666630, 0.3333333333333333148, 0.3375000000000000222, 0.3416666666666666741, 0.3458333333333333259, 0.3499999999999999778, 0.3541666666666666852, 0.3583333333333333370, 0.3624999999999999889, 0.3666666666666666408, 0.3708333333333333481, 0.3750000000000000000, 0.3791666666666666519, 0.3833333333333333592, 0.3875000000000000111, 0.3916666666666666630, 0.3958333333333333148, 0.4000000000000000222, 0.4041666666666666741, 0.4083333333333333259, 0.4124999999999999778, 0.4166666666666666852, 0.4208333333333333370, 0.4249999999999999889, 0.4291666666666666408, 0.4333333333333333481, 0.4375000000000000000, 0.4416666666666666519, 0.4458333333333333592, 0.4500000000000000111, 0.4541666666666666630, 0.4583333333333333148, 0.4625000000000000222, 0.4666666666666666741, 0.4708333333333333259, 0.4749999999999999778, 0.4791666666666666852, 0.4833333333333333370, 0.4874999999999999889, 0.4916666666666666408, 0.4958333333333333481, 0.5000000000000000000, 0.5041666666666666519, 0.5083333333333333037, 0.5124999999999999556, 0.5166666666666667185, 0.5208333333333333703, 0.5250000000000000222, 0.5291666666666666741, 0.5333333333333333259, 0.5374999999999999778, 0.5416666666666666297, 0.5458333333333332815, 0.5500000000000000444, 0.5541666666666666963, 0.5583333333333333481, 0.5625000000000000000, 0.5666666666666666519, 0.5708333333333333037, 0.5749999999999999556, 0.5791666666666667185, 0.5833333333333333703, 0.5875000000000000222, 0.5916666666666666741, 0.5958333333333333259, 0.5999999999999999778, 0.6041666666666666297, 0.6083333333333332815, 0.6125000000000000444, 0.6166666666666666963, 0.6208333333333333481, 0.6250000000000000000, 0.6291666666666666519, 0.6333333333333333037, 0.6374999999999999556, 0.6416666666666667185, 0.6458333333333333703, 0.6500000000000000222, 0.6541666666666666741, 0.6583333333333333259, 0.6624999999999999778, 0.6666666666666666297, 0.6708333333333332815, 0.6750000000000000444, 0.6791666666666666963, 0.6833333333333333481, 0.6875000000000000000, 0.6916666666666666519, 0.6958333333333333037, 0.6999999999999999556, 0.7041666666666667185, 0.7083333333333333703, 0.7125000000000000222, 0.7166666666666666741, 0.7208333333333333259, 0.7249999999999999778, 0.7291666666666666297, 0.7333333333333332815, 0.7375000000000000444, 0.7416666666666666963, 0.7458333333333333481, 0.7500000000000000000, 0.7541666666666666519, 0.7583333333333333037, 0.7624999999999999556, 0.7666666666666667185, 0.7708333333333333703, 0.7750000000000000222, 0.7791666666666666741, 0.7833333333333333259, 0.7874999999999999778, 0.7916666666666666297, 0.7958333333333332815, 0.8000000000000000444, 0.8041666666666666963, 0.8083333333333333481, 0.8125000000000000000, 0.8166666666666666519, 0.8208333333333333037, 0.8249999999999999556, 0.8291666666666667185, 0.8333333333333333703, 0.8375000000000000222, 0.8416666666666666741, 0.8458333333333333259, 0.8499999999999999778, 0.8541666666666666297, 0.8583333333333332815, 0.8625000000000000444, 0.8666666666666666963, 0.8708333333333333481, 0.8750000000000000000, 0.8791666666666666519, 0.8833333333333333037, 0.8874999999999999556, 0.8916666666666667185, 0.8958333333333333703, 0.9000000000000000222, 0.9041666666666666741, 0.9083333333333333259, 0.9124999999999999778, 0.9166666666666666297, 0.9208333333333332815, 0.9250000000000000444, 0.9291666666666666963, 0.9333333333333333481, 0.9375000000000000000, 0.9416666666666666519, 0.9458333333333333037, 0.9499999999999999556, 0.9541666666666667185, 0.9583333333333333703, 0.9625000000000000222, 0.9666666666666666741, 0.9708333333333333259, 0.9749999999999999778, 0.9791666666666666297, 0.9833333333333332815, 0.9875000000000000444 ),
 .UNSPECIFIED. ) 
 GEOMETRIC_REPRESENTATION_ITEM ( )  RATIONAL_B_SPLINE_SURFACE ( (
 ( 1.000000000000000000, 0.9659258262890683122, 1.000000000000000000, 0.9659258262890683122, 1.000000000000000000, 0.9659258262890683122, 1.000000000000000000, 0.9659258262890683122, 1.000000000000000000, 0.9659258262890683122, 1.000000000000000000, 0.9659258262890683122, 1.000000000000000000, 0.9659258262890683122, 1.000000000000000000, 0.9659258262890683122, 1.000000000000000000, 0.9659258262890683122, 1.000000000000000000, 0.9659258262890683122, 1.000000000000000000, 0.9659258262890683122, 1.000000000000000000, 0.9659258262890683122, 1.000000000000000000, 0.9659258262890683122, 1.000000000000000000, 0.9659258262890683122, 1.000000000000000000, 0.9659258262890683122, 1.000000000000000000, 0.9659258262890683122, 1.000000000000000000, 0.9659258262890683122, 1.000000000000000000, 0.9659258262890683122, 1.000000000000000000, 0.9659258262890683122, 1.000000000000000000, 0.9659258262890683122, 1.000000000000000000, 0.9659258262890683122, 1.000000000000000000, 0.9659258262890683122, 1.000000000000000000, 0.9659258262890683122, 1.000000000000000000, 0.9659258262890683122, 1.000000000000000000, 0.9659258262890683122, 1.000000000000000000, 0.9659258262890683122, 1.000000000000000000, 0.9659258262890683122, 1.000000000000000000, 0.9659258262890683122, 1.000000000000000000, 0.9659258262890683122, 1.000000000000000000, 0.9659258262890683122, 1.000000000000000000, 0.9659258262890683122, 1.000000000000000000, 0.9659258262890683122, 1.000000000000000000, 0.9659258262890683122, 1.000000000000000000, 0.9659258262890683122, 1.000000000000000000, 0.9659258262890683122, 1.000000000000000000, 0.9659258262890683122, 1.000000000000000000, 0.9659258262890683122, 1.000000000000000000, 0.9659258262890683122, 1.000000000000000000, 0.9659258262890683122, 1.000000000000000000, 0.9659258262890683122, 1.000000000000000000, 0.9659258262890683122, 1.000000000000000000, 0.9659258262890683122, 1.000000000000000000, 0.9659258262890683122, 1.000000000000000000, 0.9659258262890683122, 1.000000000000000000, 0.9659258262890683122, 1.000000000000000000, 0.9659258262890683122, 1.000000000000000000, 0.9659258262890683122, 1.000000000000000000, 0.9659258262890683122, 1.000000000000000000, 0.9659258262890683122, 1.000000000000000000, 0.9659258262890683122, 1.000000000000000000, 0.9659258262890683122, 1.000000000000000000, 0.9659258262890683122, 1.000000000000000000, 0.9659258262890683122, 1.000000000000000000, 0.9659258262890683122, 1.000000000000000000, 0.9659258262890683122, 1.000000000000000000, 0.9659258262890683122, 1.000000000000000000, 0.9659258262890683122, 1.000000000000000000, 0.9659258262890683122, 1.000000000000000000, 0.9659258262890683122, 1.000000000000000000, 0.9659258262890683122, 1.000000000000000000, 0.9659258262890683122, 1.000000000000000000, 0.9659258262890683122, 1.000000000000000000, 0.9659258262890683122, 1.000000000000000000, 0.9659258262890683122, 1.000000000000000000, 0.9659258262890683122, 1.000000000000000000, 0.9659258262890683122, 1.000000000000000000, 0.9659258262890683122, 1.000000000000000000, 0.9659258262890683122, 1.000000000000000000, 0.9659258262890683122, 1.000000000000000000, 0.9659258262890683122, 1.000000000000000000, 0.9659258262890683122, 1.000000000000000000, 0.9659258262890683122, 1.000000000000000000, 0.9659258262890683122, 1.000000000000000000, 0.9659258262890683122, 1.000000000000000000, 0.9659258262890683122, 1.000000000000000000, 0.9659258262890683122, 1.000000000000000000, 0.9659258262890683122, 1.000000000000000000, 0.9659258262890683122, 1.000000000000000000, 0.9659258262890683122, 1.000000000000000000, 0.9659258262890683122, 1.000000000000000000, 0.9659258262890683122, 1.000000000000000000, 0.9659258262890683122, 1.000000000000000000, 0.9659258262890683122, 1.000000000000000000, 0.9659258262890683122, 1.000000000000000000, 0.9659258262890683122, 1.000000000000000000, 0.9659258262890683122, 1.000000000000000000, 0.9659258262890683122, 1.000000000000000000, 0.9659258262890683122, 1.000000000000000000, 0.9659258262890683122, 1.000000000000000000, 0.9659258262890683122, 1.000000000000000000, 0.9659258262890683122, 1.000000000000000000, 0.9659258262890683122, 1.000000000000000000, 0.9659258262890683122, 1.000000000000000000, 0.9659258262890683122, 1.000000000000000000, 0.9659258262890683122, 1.000000000000000000, 0.9659258262890683122, 1.000000000000000000, 0.9659258262890683122, 1.000000000000000000, 0.9659258262890683122, 1.000000000000000000, 0.9659258262890683122, 1.000000000000000000, 0.9659258262890683122, 1.000000000000000000, 0.9659258262890683122, 1.000000000000000000, 0.9659258262890683122, 1.000000000000000000, 0.9659258262890683122, 1.000000000000000000, 0.9659258262890683122, 1.000000000000000000, 0.9659258262890683122, 1.000000000000000000, 0.9659258262890683122, 1.000000000000000000, 0.9659258262890683122, 1.000000000000000000, 0.9659258262890683122, 1.000000000000000000, 0.9659258262890683122, 1.000000000000000000, 0.9659258262890683122, 1.000000000000000000, 0.9659258262890683122, 1.000000000000000000, 0.9659258262890683122, 1.000000000000000000, 0.9659258262890683122, 1.000000000000000000, 0.9659258262890683122, 1.000000000000000000, 0.9659258262890683122, 1.000000000000000000, 0.9659258262890683122, 1.000000000000000000, 0.9659258262890683122, 1.000000000000000000, 0.9659258262890683122, 1.000000000000000000, 0.9659258262890683122, 1.000000000000000000, 0.9659258262890683122, 1.000000000000000000, 0.9659258262890683122, 1.000000000000000000, 0.9659258262890683122, 1.000000000000000000, 0.9659258262890683122, 1.000000000000000000, 0.9659258262890683122, 1.000000000000000000, 0.9659258262890683122, 1.000000000000000000, 0.9659258262890683122, 1.000000000000000000, 0.9659258262890683122, 1.000000000000000000, 0.9659258262890683122, 1.000000000000000000, 0.9659258262890683122, 1.000000000000000000, 0.9659258262890683122, 1.000000000000000000, 0.9659258262890683122, 1.000000000000000000, 0.9659258262890683122, 1.000000000000000000, 0.9659258262890683122, 1.000000000000000000, 0.9659258262890683122, 1.000000000000000000, 0.9659258262890683122, 1.000000000000000000, 0.9659258262890683122, 1.000000000000000000, 0.9659258262890683122, 1.000000000000000000, 0.9659258262890683122, 1.000000000000000000, 0.9659258262890683122, 1.000000000000000000, 0.9659258262890683122, 1.000000000000000000, 0.9659258262890683122, 1.000000000000000000, 0.9659258262890683122, 1.000000000000000000, 0.9659258262890683122, 1.000000000000000000, 0.9659258262890683122, 1.000000000000000000, 0.9659258262890683122, 1.000000000000000000, 0.9659258262890683122, 1.000000000000000000, 0.9659258262890683122, 1.000000000000000000, 0.9659258262890683122, 1.000000000000000000, 0.9659258262890683122, 1.000000000000000000, 0.9659258262890683122, 1.000000000000000000, 0.9659258262890683122, 1.000000000000000000, 0.9659258262890683122, 1.000000000000000000, 0.9659258262890683122, 1.000000000000000000, 0.9659258262890683122, 1.000000000000000000, 0.9659258262890683122, 1.000000000000000000, 0.9659258262890683122, 1.000000000000000000, 0.9659258262890683122, 1.000000000000000000, 0.9659258262890683122, 1.000000000000000000, 0.9659258262890683122, 1.000000000000000000, 0.9659258262890683122, 1.000000000000000000, 0.9659258262890683122, 1.000000000000000000, 0.9659258262890683122, 1.000000000000000000, 0.9659258262890683122, 1.000000000000000000, 0.9659258262890683122, 1.000000000000000000, 0.9659258262890683122, 1.000000000000000000, 0.9659258262890683122, 1.000000000000000000, 0.9659258262890683122, 1.000000000000000000, 0.9659258262890683122, 1.000000000000000000, 0.9659258262890683122, 1.000000000000000000, 0.9659258262890683122, 1.000000000000000000, 0.9659258262890683122, 1.000000000000000000, 0.9659258262890683122, 1.000000000000000000, 0.9659258262890683122, 1.000000000000000000, 0.9659258262890683122, 1.000000000000000000, 0.9659258262890683122, 1.000000000000000000, 0.9659258262890683122, 1.000000000000000000, 0.9659258262890683122, 1.000000000000000000, 0.9659258262890683122, 1.000000000000000000, 0.9659258262890683122, 1.000000000000000000, 0.9659258262890683122, 1.000000000000000000, 0.9659258262890683122, 1.000000000000000000, 0.9659258262890683122, 1.000000000000000000, 0.9659258262890683122, 1.000000000000000000, 0.9659258262890683122, 1.000000000000000000, 0.9659258262890683122, 1.000000000000000000, 0.9659258262890683122, 1.000000000000000000, 0.9659258262890683122, 1.000000000000000000, 0.9659258262890683122, 1.000000000000000000, 0.9659258262890683122, 1.000000000000000000, 0.9659258262890683122, 1.000000000000000000, 0.9659258262890683122, 1.000000000000000000, 0.9659258262890683122, 1.000000000000000000, 0.9659258262890683122, 1.000000000000000000, 0.9659258262890683122, 1.000000000000000000, 0.9659258262890683122, 1.000000000000000000, 0.9659258262890683122, 1.000000000000000000, 0.9659258262890683122, 1.000000000000000000, 0.9659258262890683122, 1.000000000000000000, 0.9659258262890683122, 1.000000000000000000, 0.9659258262890683122, 1.000000000000000000, 0.9659258262890683122, 1.000000000000000000, 0.9659258262890683122, 1.000000000000000000, 0.9659258262890683122, 1.000000000000000000, 0.9659258262890683122, 1.000000000000000000, 0.9659258262890683122, 1.000000000000000000, 0.9659258262890683122, 1.000000000000000000, 0.9659258262890683122, 1.000000000000000000, 0.9659258262890683122, 1.000000000000000000, 0.9659258262890683122, 1.000000000000000000, 0.9659258262890683122, 1.000000000000000000, 0.9659258262890683122, 1.000000000000000000, 0.9659258262890683122, 1.000000000000000000, 0.9659258262890683122, 1.000000000000000000, 0.9659258262890683122, 1.000000000000000000, 0.9659258262890683122, 1.000000000000000000, 0.9659258262890683122, 1.000000000000000000, 0.9659258262890683122, 1.000000000000000000, 0.9659258262890683122, 1.000000000000000000, 0.9659258262890683122, 1.000000000000000000, 0.9659258262890683122, 1.000000000000000000, 0.9659258262890683122, 1.000000000000000000, 0.9659258262890683122, 1.000000000000000000, 0.9659258262890683122, 1.000000000000000000, 0.9659258262890683122, 1.000000000000000000, 0.9659258262890683122, 1.000000000000000000, 0.9659258262890683122, 1.000000000000000000, 0.9659258262890683122, 1.000000000000000000, 0.9659258262890683122, 1.000000000000000000, 0.9659258262890683122, 1.000000000000000000, 0.9659258262890683122, 1.000000000000000000, 0.9659258262890683122, 1.000000000000000000, 0.9659258262890683122, 1.000000000000000000, 0.9659258262890683122, 1.000000000000000000, 0.9659258262890683122, 1.000000000000000000, 0.9659258262890683122, 1.000000000000000000, 0.9659258262890683122, 1.000000000000000000, 0.9659258262890683122, 1.000000000000000000),
 ( 1.000000000000000000, 0.9659258262890683122, 1.000000000000000000, 0.9659258262890683122, 1.000000000000000000, 0.9659258262890683122, 1.000000000000000000, 0.9659258262890683122, 1.000000000000000000, 0.9659258262890683122, 1.000000000000000000, 0.9659258262890683122, 1.000000000000000000, 0.9659258262890683122, 1.000000000000000000, 0.9659258262890683122, 1.000000000000000000, 0.9659258262890683122, 1.000000000000000000, 0.9659258262890683122, 1.000000000000000000, 0.9659258262890683122, 1.000000000000000000, 0.9659258262890683122, 1.000000000000000000, 0.9659258262890683122, 1.000000000000000000, 0.9659258262890683122, 1.000000000000000000, 0.9659258262890683122, 1.000000000000000000, 0.9659258262890683122, 1.000000000000000000, 0.9659258262890683122, 1.000000000000000000, 0.9659258262890683122, 1.000000000000000000, 0.9659258262890683122, 1.000000000000000000, 0.9659258262890683122, 1.000000000000000000, 0.9659258262890683122, 1.000000000000000000, 0.9659258262890683122, 1.000000000000000000, 0.9659258262890683122, 1.000000000000000000, 0.9659258262890683122, 1.000000000000000000, 0.9659258262890683122, 1.000000000000000000, 0.9659258262890683122, 1.000000000000000000, 0.9659258262890683122, 1.000000000000000000, 0.9659258262890683122, 1.000000000000000000, 0.9659258262890683122, 1.000000000000000000, 0.9659258262890683122, 1.000000000000000000, 0.9659258262890683122, 1.000000000000000000, 0.9659258262890683122, 1.000000000000000000, 0.9659258262890683122, 1.000000000000000000, 0.9659258262890683122, 1.000000000000000000, 0.9659258262890683122, 1.000000000000000000, 0.9659258262890683122, 1.000000000000000000, 0.9659258262890683122, 1.000000000000000000, 0.9659258262890683122, 1.000000000000000000, 0.9659258262890683122, 1.000000000000000000, 0.9659258262890683122, 1.000000000000000000, 0.9659258262890683122, 1.000000000000000000, 0.9659258262890683122, 1.000000000000000000, 0.9659258262890683122, 1.000000000000000000, 0.9659258262890683122, 1.000000000000000000, 0.9659258262890683122, 1.000000000000000000, 0.9659258262890683122, 1.000000000000000000, 0.9659258262890683122, 1.000000000000000000, 0.9659258262890683122, 1.000000000000000000, 0.9659258262890683122, 1.000000000000000000, 0.9659258262890683122, 1.000000000000000000, 0.9659258262890683122, 1.000000000000000000, 0.9659258262890683122, 1.000000000000000000, 0.9659258262890683122, 1.000000000000000000, 0.9659258262890683122, 1.000000000000000000, 0.9659258262890683122, 1.000000000000000000, 0.9659258262890683122, 1.000000000000000000, 0.9659258262890683122, 1.000000000000000000, 0.9659258262890683122, 1.000000000000000000, 0.9659258262890683122, 1.000000000000000000, 0.9659258262890683122, 1.000000000000000000, 0.9659258262890683122, 1.000000000000000000, 0.9659258262890683122, 1.000000000000000000, 0.9659258262890683122, 1.000000000000000000, 0.9659258262890683122, 1.000000000000000000, 0.9659258262890683122, 1.000000000000000000, 0.9659258262890683122, 1.000000000000000000, 0.9659258262890683122, 1.000000000000000000, 0.9659258262890683122, 1.000000000000000000, 0.9659258262890683122, 1.000000000000000000, 0.9659258262890683122, 1.000000000000000000, 0.9659258262890683122, 1.000000000000000000, 0.9659258262890683122, 1.000000000000000000, 0.9659258262890683122, 1.000000000000000000, 0.9659258262890683122, 1.000000000000000000, 0.9659258262890683122, 1.000000000000000000, 0.9659258262890683122, 1.000000000000000000, 0.9659258262890683122, 1.000000000000000000, 0.9659258262890683122, 1.000000000000000000, 0.9659258262890683122, 1.000000000000000000, 0.9659258262890683122, 1.000000000000000000, 0.9659258262890683122, 1.000000000000000000, 0.9659258262890683122, 1.000000000000000000, 0.9659258262890683122, 1.000000000000000000, 0.9659258262890683122, 1.000000000000000000, 0.9659258262890683122, 1.000000000000000000, 0.9659258262890683122, 1.000000000000000000, 0.9659258262890683122, 1.000000000000000000, 0.9659258262890683122, 1.000000000000000000, 0.9659258262890683122, 1.000000000000000000, 0.9659258262890683122, 1.000000000000000000, 0.9659258262890683122, 1.000000000000000000, 0.9659258262890683122, 1.000000000000000000, 0.9659258262890683122, 1.000000000000000000, 0.9659258262890683122, 1.000000000000000000, 0.9659258262890683122, 1.000000000000000000, 0.9659258262890683122, 1.000000000000000000, 0.9659258262890683122, 1.000000000000000000, 0.9659258262890683122, 1.000000000000000000, 0.9659258262890683122, 1.000000000000000000, 0.9659258262890683122, 1.000000000000000000, 0.9659258262890683122, 1.000000000000000000, 0.9659258262890683122, 1.000000000000000000, 0.9659258262890683122, 1.000000000000000000, 0.9659258262890683122, 1.000000000000000000, 0.9659258262890683122, 1.000000000000000000, 0.9659258262890683122, 1.000000000000000000, 0.9659258262890683122, 1.000000000000000000, 0.9659258262890683122, 1.000000000000000000, 0.9659258262890683122, 1.000000000000000000, 0.9659258262890683122, 1.000000000000000000, 0.9659258262890683122, 1.000000000000000000, 0.9659258262890683122, 1.000000000000000000, 0.9659258262890683122, 1.000000000000000000, 0.9659258262890683122, 1.000000000000000000, 0.9659258262890683122, 1.000000000000000000, 0.9659258262890683122, 1.000000000000000000, 0.9659258262890683122, 1.000000000000000000, 0.9659258262890683122, 1.000000000000000000, 0.9659258262890683122, 1.000000000000000000, 0.9659258262890683122, 1.000000000000000000, 0.9659258262890683122, 1.000000000000000000, 0.9659258262890683122, 1.000000000000000000, 0.9659258262890683122, 1.000000000000000000, 0.9659258262890683122, 1.000000000000000000, 0.9659258262890683122, 1.000000000000000000, 0.9659258262890683122, 1.000000000000000000, 0.9659258262890683122, 1.000000000000000000, 0.9659258262890683122, 1.000000000000000000, 0.9659258262890683122, 1.000000000000000000, 0.9659258262890683122, 1.000000000000000000, 0.9659258262890683122, 1.000000000000000000, 0.9659258262890683122, 1.000000000000000000, 0.9659258262890683122, 1.000000000000000000, 0.9659258262890683122, 1.000000000000000000, 0.9659258262890683122, 1.000000000000000000, 0.9659258262890683122, 1.000000000000000000, 0.9659258262890683122, 1.000000000000000000, 0.9659258262890683122, 1.000000000000000000, 0.9659258262890683122, 1.000000000000000000, 0.9659258262890683122, 1.000000000000000000, 0.9659258262890683122, 1.000000000000000000, 0.9659258262890683122, 1.000000000000000000, 0.9659258262890683122, 1.000000000000000000, 0.9659258262890683122, 1.000000000000000000, 0.9659258262890683122, 1.000000000000000000, 0.9659258262890683122, 1.000000000000000000, 0.9659258262890683122, 1.000000000000000000, 0.9659258262890683122, 1.000000000000000000, 0.9659258262890683122, 1.000000000000000000, 0.9659258262890683122, 1.000000000000000000, 0.9659258262890683122, 1.000000000000000000, 0.9659258262890683122, 1.000000000000000000, 0.9659258262890683122, 1.000000000000000000, 0.9659258262890683122, 1.000000000000000000, 0.9659258262890683122, 1.000000000000000000, 0.9659258262890683122, 1.000000000000000000, 0.9659258262890683122, 1.000000000000000000, 0.9659258262890683122, 1.000000000000000000, 0.9659258262890683122, 1.000000000000000000, 0.9659258262890683122, 1.000000000000000000, 0.9659258262890683122, 1.000000000000000000, 0.9659258262890683122, 1.000000000000000000, 0.9659258262890683122, 1.000000000000000000, 0.9659258262890683122, 1.000000000000000000, 0.9659258262890683122, 1.000000000000000000, 0.9659258262890683122, 1.000000000000000000, 0.9659258262890683122, 1.000000000000000000, 0.9659258262890683122, 1.000000000000000000, 0.9659258262890683122, 1.000000000000000000, 0.9659258262890683122, 1.000000000000000000, 0.9659258262890683122, 1.000000000000000000, 0.9659258262890683122, 1.000000000000000000, 0.9659258262890683122, 1.000000000000000000, 0.9659258262890683122, 1.000000000000000000, 0.9659258262890683122, 1.000000000000000000, 0.9659258262890683122, 1.000000000000000000, 0.9659258262890683122, 1.000000000000000000, 0.9659258262890683122, 1.000000000000000000, 0.9659258262890683122, 1.000000000000000000, 0.9659258262890683122, 1.000000000000000000, 0.9659258262890683122, 1.000000000000000000, 0.9659258262890683122, 1.000000000000000000, 0.9659258262890683122, 1.000000000000000000, 0.9659258262890683122, 1.000000000000000000, 0.9659258262890683122, 1.000000000000000000, 0.9659258262890683122, 1.000000000000000000, 0.9659258262890683122, 1.000000000000000000, 0.9659258262890683122, 1.000000000000000000, 0.9659258262890683122, 1.000000000000000000, 0.9659258262890683122, 1.000000000000000000, 0.9659258262890683122, 1.000000000000000000, 0.9659258262890683122, 1.000000000000000000, 0.9659258262890683122, 1.000000000000000000, 0.9659258262890683122, 1.000000000000000000, 0.9659258262890683122, 1.000000000000000000, 0.9659258262890683122, 1.000000000000000000, 0.9659258262890683122, 1.000000000000000000, 0.9659258262890683122, 1.000000000000000000, 0.9659258262890683122, 1.000000000000000000, 0.9659258262890683122, 1.000000000000000000, 0.9659258262890683122, 1.000000000000000000, 0.9659258262890683122, 1.000000000000000000, 0.9659258262890683122, 1.000000000000000000, 0.9659258262890683122, 1.000000000000000000, 0.9659258262890683122, 1.000000000000000000, 0.9659258262890683122, 1.000000000000000000, 0.9659258262890683122, 1.000000000000000000, 0.9659258262890683122, 1.000000000000000000, 0.9659258262890683122, 1.000000000000000000, 0.9659258262890683122, 1.000000000000000000, 0.9659258262890683122, 1.000000000000000000, 0.9659258262890683122, 1.000000000000000000, 0.9659258262890683122, 1.000000000000000000, 0.9659258262890683122, 1.000000000000000000, 0.9659258262890683122, 1.000000000000000000, 0.9659258262890683122, 1.000000000000000000, 0.9659258262890683122, 1.000000000000000000, 0.9659258262890683122, 1.000000000000000000, 0.9659258262890683122, 1.000000000000000000, 0.9659258262890683122, 1.000000000000000000, 0.9659258262890683122, 1.000000000000000000, 0.9659258262890683122, 1.000000000000000000, 0.9659258262890683122, 1.000000000000000000, 0.9659258262890683122, 1.000000000000000000, 0.9659258262890683122, 1.000000000000000000, 0.9659258262890683122, 1.000000000000000000, 0.9659258262890683122, 1.000000000000000000, 0.9659258262890683122, 1.000000000000000000, 0.9659258262890683122, 1.000000000000000000, 0.9659258262890683122, 1.000000000000000000, 0.9659258262890683122, 1.000000000000000000, 0.9659258262890683122, 1.000000000000000000, 0.9659258262890683122, 1.000000000000000000, 0.9659258262890683122, 1.000000000000000000, 0.9659258262890683122, 1.000000000000000000, 0.9659258262890683122, 1.000000000000000000, 0.9659258262890683122, 1.000000000000000000) ) ) 
 REPRESENTATION_ITEM ( '' )  SURFACE ( )  );
#64908 = EDGE_LOOP ( 'NONE', ( #45506, #28873, #16346, #27685, #30305, #29969 ) ) ;
#64909 = CARTESIAN_POINT ( 'NONE',  ( 0.07874015748031558404, -0.1870078740157479769, 0.4822834645669291653 ) ) ;
#64910 = CARTESIAN_POINT ( 'NONE',  ( -0.2099737532808391705, -0.5023911411419708095, -0.1820866141732282451 ) ) ;
#64912 = CARTESIAN_POINT ( 'NONE',  ( -0.4724409448818896462, -0.1265901696524993070, -0.3608923884514435576 ) ) ;
#64911 = CARTESIAN_POINT ( 'NONE',  ( 1.496062992125985147, -0.1870078740157479769, 0.3641732283464567677 ) ) ;
#64913 = CARTESIAN_POINT ( 'NONE',  ( -0.1265901696524993347, 0.4724409448818895907, -0.2408136482939632061 ) ) ;
#64914 = LINE ( 'NONE', #13163, #63204 ) ;
#64915 = CARTESIAN_POINT ( 'NONE',  ( 1.240157480314961314, -0.5400638737290844871, 0.3530559997133364547 ) ) ;
#64916 = CARTESIAN_POINT ( 'NONE',  ( -0.3949938075777411073, 0.1058382717557497660, 0.04790026246719160385 ) ) ;
#64917 = CARTESIAN_POINT ( 'NONE',  ( -0.03937007874015669567, -0.6692913385826771977, 8.415575281601705876E-17 ) ) ;
#64918 = CARTESIAN_POINT ( 'NONE',  ( -1.627296587926508442, 0.2306618581243848609, 0.2411417322834645549 ) ) ;
#64919 = CARTESIAN_POINT ( 'NONE',  ( -1.437007874015747477, -0.5400638737290844871, 0.3530559997133364547 ) ) ;
#64920 = CARTESIAN_POINT ( 'NONE',  ( -0.1443569553805768291, 0.05413385826771666132, 0.4176697321401328100 ) ) ;
#64921 = CARTESIAN_POINT ( 'NONE',  ( -0.3420746716998662729, 0.1974969037888702206, 0.05446194225721785048 ) ) ;
#64922 = CARTESIAN_POINT ( 'NONE',  ( 1.666666666666667185, 0.05413385826771666132, 0.4176697321401328100 ) ) ;
#64923 = CARTESIAN_POINT ( 'NONE',  ( 0.7020997375328090762, -0.05778040916215560624, -0.4822834645669293319 ) ) ;
#64924 = CARTESIAN_POINT ( 'NONE',  ( 1.036745406824147731, -0.004921259842519576551, 0.3153832671262227771 ) ) ;
#64925 = CARTESIAN_POINT ( 'NONE',  ( 0.3061702621670817082, 1.250678700630301510, 0.06534988725049302449 ) ) ;
#64926 = CARTESIAN_POINT ( 'NONE',  ( 0.9711286089238851948, -0.5023911411419708095, -0.1820866141732282451 ) ) ;
#64927 = CARTESIAN_POINT ( 'NONE',  ( -1.122047244094487306, 0.1660481256975883668, -0.3530559997133364547 ) ) ;
#64928 = CARTESIAN_POINT ( 'NONE',  ( 0.3996062992125986035, -0.1070741851644052972, -0.9757217847769029673 ) ) ;
#64929 = CARTESIAN_POINT ( 'NONE',  ( 1.076115485564305141, 0.2306618581243847221, -0.2411417322834647770 ) ) ;
#64930 = CARTESIAN_POINT ( 'NONE',  ( -0.3917322834645671215, 0.1049643490035301469, -0.6548556430446192955 ) ) ;
#64932 = DIRECTION ( 'NONE',  ( -1.000000000000000000, 0.000000000000000000, -3.491481338843132961E-15 ) ) ;
#64931 = CARTESIAN_POINT ( 'NONE',  ( 0.8727034120734913358, -0.05778040916215522460, 0.4822834645669289988 ) ) ;
#64933 = CARTESIAN_POINT ( 'NONE',  ( 0.2887139107611556010, -0.5023911411419708095, 0.1820866141732285504 ) ) ;
#64934 = CARTESIAN_POINT ( 'NONE',  ( 0.5446194225721792126, -0.3162353388693405765, 0.4822834645669290543 ) ) ;
#64935 = LINE ( 'NONE', #65786, #61313 ) ;
#64936 = CARTESIAN_POINT ( 'NONE',  ( -1.135170603674539924, -0.5511811023622046335, 0.09757992244046803654 ) ) ;
#64937 = CARTESIAN_POINT ( 'NONE',  ( -1.056430446194224881, 0.2952755905511810774, -0.1292274648535930714 ) ) ;
#64938 = CARTESIAN_POINT ( 'NONE',  ( 1.305774278215223960, -0.6692913385826771977, 0.1292274648535927661 ) ) ;
#64939 = CARTESIAN_POINT ( 'NONE',  ( -1.404199475065615932, 0.05413385826771666132, 0.4176697321401328100 ) ) ;
#64940 = CARTESIAN_POINT ( 'NONE',  ( 1.043307086614173818, 0.1660481256975885056, 0.3530559997133364547 ) ) ;
#64941 = CARTESIAN_POINT ( 'NONE',  ( -1.456692913385826182, 0.1771653543307087630, 0.000000000000000000 ) ) ;
#64942 = CARTESIAN_POINT ( 'NONE',  ( -0.3969271875946644434, -0.02899565511876312993, -1.220472440944881942 ) ) ;
#64943 = CARTESIAN_POINT ( 'NONE',  ( 1.003937007874016185, 0.1660481256975883668, -0.3530559997133364547 ) ) ;
#64944 = CARTESIAN_POINT ( 'NONE',  ( -0.4724409448818895907, -0.1265901696524993070, -2.484908136482939955 ) ) ;
#64945 = CARTESIAN_POINT ( 'NONE',  ( 1.614173228346457378, -0.6692913385826771977, 8.415575281601705876E-17 ) ) ;
#64946 = CARTESIAN_POINT ( 'NONE',  ( 1.187664041994751285, -0.05778040916215522460, 0.4822834645669289988 ) ) ;
#64947 = CARTESIAN_POINT ( 'NONE',  ( -1.325459317585300889, -0.3690944881889765550, -0.3153832671262227771 ) ) ;
#64948 = CARTESIAN_POINT ( 'NONE',  ( 1.371391076115485941, 0.1771653543307087630, 0.09757992244046791164 ) ) ;
#64949 = CARTESIAN_POINT ( 'NONE',  ( -1.318897637795274802, 0.07958543189024085140, 0.2665933059059887866 ) ) ;
#64950 = CARTESIAN_POINT ( 'NONE',  ( -0.5643044619422565855, -0.3690944881889763329, 0.3153832671262228327 ) ) ;
#64951 = CARTESIAN_POINT ( 'NONE',  ( -1.437007874015747477, -0.4536011799217367080, 0.2665933059059888421 ) ) ;
#64953 = B_SPLINE_CURVE_WITH_KNOTS ( 'NONE', 3,
 ( #50106, #75803, #18145, #44913, #40297, #39885, #65147 ),
 .UNSPECIFIED., .F., .F.,
 ( 4, 3, 4 ),
 ( 5.551115123125782702E-17, 0.001246230184515582365, 0.002492489877932689731 ),
 .UNSPECIFIED. ) ;
#64952 = CARTESIAN_POINT ( 'NONE',  ( 0.8398950131233602345, 0.1283753931104746893, -0.1820866141732285504 ) ) ;
#64954 = CONICAL_SURFACE ( 'NONE', #28671, 3.582677165354330562, 0.7853981633974415066 ) ;
#64955 = CARTESIAN_POINT ( 'NONE',  ( 0.5971128608923891301, 0.2952755905511810774, -0.1292274648535930714 ) ) ;
#64956 = CARTESIAN_POINT ( 'NONE',  ( 1.043307086614173818, -0.5400638737290845981, -0.3530559997133363437 ) ) ;
#64957 = CARTESIAN_POINT ( 'NONE',  ( 0.1640419947506569498, -0.3162353388693409650, -0.4822834645669289433 ) ) ;
#64958 = ADVANCED_FACE ( 'NONE', ( #31920 ), #44528, .F. ) ;
#64959 = CARTESIAN_POINT ( 'NONE',  ( 0.4527559055118117182, -0.4536011799217367080, 0.2665933059059888421 ) ) ;
#64960 = CARTESIAN_POINT ( 'NONE',  ( -1.456692913385826182, 0.2952755905511811885, 0.000000000000000000 ) ) ;
#64961 = EDGE_CURVE ( 'NONE', #51378, #55951, #48706, .T. ) ;
#64962 = EDGE_CURVE ( 'NONE', #82322, #23151, #12993, .T. ) ;
#64963 = CARTESIAN_POINT ( 'NONE',  ( 2.795275590551181910, 1.568468489416428469, 0.000000000000000000 ) ) ;
#64964 = CARTESIAN_POINT ( 'NONE',  ( -0.4265091863517051496, 0.2952755905511810774, -0.1292274648535930714 ) ) ;
#64965 = CARTESIAN_POINT ( 'NONE',  ( 0.2925321140481932369, -0.2925321140481931814, -0.5708661417322833387 ) ) ;
#64966 = CARTESIAN_POINT ( 'NONE',  ( 0.01241954290193841674, 0.000000000000000000, 0.3464511005275205946 ) ) ;
#64967 = CARTESIAN_POINT ( 'NONE',  ( 0.1443569553805781891, -0.4281496062992124485, 0.4176697321401328655 ) ) ;
#64968 = CARTESIAN_POINT ( 'NONE',  ( -0.5905511811023613777, -0.6692913385826771977, 8.415575281601705876E-17 ) ) ;
#64969 = CARTESIAN_POINT ( 'NONE',  ( 0.02624671916010564918, 0.2306618581243848609, 0.2411417322834645549 ) ) ;
#64970 = CARTESIAN_POINT ( 'NONE',  ( 0.3996062992125986590, -0.1070741851644053111, -2.788713910761154047 ) ) ;
#64971 = CARTESIAN_POINT ( 'NONE',  ( -0.3420746716998659953, -0.1974969037888706647, -1.784776902887138972 ) ) ;
#64972 = CARTESIAN_POINT ( 'NONE',  ( -0.3917322834645670104, -7.196005306013484475E-17, -0.6614173228346454936 ) ) ;
#64973 = CARTESIAN_POINT ( 'NONE',  ( -1.519422763189357539, 0.2755905511811023723, 0.7302211324797359682 ) ) ;
#64974 = CARTESIAN_POINT ( 'NONE',  ( 4.797336870675656522E-17, -0.3917322834645670104, -1.173228346456692828 ) ) ;
#64975 = CARTESIAN_POINT ( 'NONE',  ( -0.8923884514435688198, 0.1283753931104746893, -0.1820866141732285504 ) ) ;
#64976 = CARTESIAN_POINT ( 'NONE',  ( -9.594673741351313045E-17, 0.3917322834645670104, -1.094488188976378007 ) ) ;
#64977 = CARTESIAN_POINT ( 'NONE',  ( -1.259842519685038686, -0.1870078740157479769, 0.4822834645669291653 ) ) ;
#64978 = B_SPLINE_CURVE_WITH_KNOTS ( 'NONE', 3,
 ( #20655, #64844, #1715, #65702, #7182, #32853, #58522 ),
 .UNSPECIFIED., .F., .F.,
 ( 4, 3, 4 ),
 ( 7.703719777548943412E-34, 0.001246230184515573257, 0.002492489877932650266 ),
 .UNSPECIFIED. ) ;
#64979 = CARTESIAN_POINT ( 'NONE',  ( -0.3392501089628019439, 0.1958661417322832554, 0.05120041814404382302 ) ) ;
#64980 = CARTESIAN_POINT ( 'NONE',  ( 0.6299212598425204535, -0.1870078740157480879, -0.4822834645669291653 ) ) ;
#64981 = CARTESIAN_POINT ( 'NONE',  ( -0.09186351706036689768, -0.004921259842519870586, -0.3153832671262229437 ) ) ;
#64982 = EDGE_CURVE ( 'NONE', #50071, #72444, #2027, .T. ) ;
#64983 = CARTESIAN_POINT ( 'NONE',  ( 1.266404199475066328, -0.05778040916215522460, 0.4822834645669289988 ) ) ;
#64984 = CARTESIAN_POINT ( 'NONE',  ( 0.5314960629921264834, 0.1660481256975883668, -0.3530559997133364547 ) ) ;
#64985 = CARTESIAN_POINT ( 'NONE',  ( 0.3855990896080964681, 1.260602825228276602, 1.053749523914724318 ) ) ;
#64986 = CARTESIAN_POINT ( 'NONE',  ( -0.3460692066303958092, -0.1998031496062994683, -2.572178477690288734 ) ) ;
#64987 = CARTESIAN_POINT ( 'NONE',  ( -0.1958661417322833942, -0.3392501089628018884, -1.007237163550868120 ) ) ;
#64988 = CARTESIAN_POINT ( 'NONE',  ( 1.318897637795276356, -0.5400638737290844871, 0.3530559997133364547 ) ) ;
#64989 = CARTESIAN_POINT ( 'NONE',  ( 0.3149606299212603933, -0.1870078740157479769, 0.4822834645669291653 ) ) ;
#64990 = CARTESIAN_POINT ( 'NONE',  ( 0.2887139107611556010, -0.6046776061558807314, 0.2411417322834647770 ) ) ;
#64991 = CARTESIAN_POINT ( 'NONE',  ( 1.404199475065617708, 0.05413385826771626580, -0.4176697321401330321 ) ) ;
#64992 = CARTESIAN_POINT ( 'NONE',  ( -0.3917322834645671215, 0.1049643490035301469, -0.7473753280839893209 ) ) ;
#64993 = CARTESIAN_POINT ( 'NONE',  ( 0.1377952755905518800, -0.5400638737290844871, 0.3530559997133364547 ) ) ;
#64994 = CARTESIAN_POINT ( 'NONE',  ( 1.181102362204725198, -0.1870078740157479769, 0.4822834645669291653 ) ) ;
#64995 = CARTESIAN_POINT ( 'NONE',  ( 0.3740157480314966754, -0.5400638737290844871, 0.3530559997133364547 ) ) ;
#64996 = VECTOR ( 'NONE', #32325, 39.37007874015748143 ) ;
#64997 = CARTESIAN_POINT ( 'NONE',  ( 1.318897637795276356, -0.4536011799217367080, 0.2665933059059888421 ) ) ;
#64998 = CARTESIAN_POINT ( 'NONE',  ( -1.003937007874015297, -0.5400638737290845981, -0.3530559997133363437 ) ) ;
#64999 = CARTESIAN_POINT ( 'NONE',  ( -1.391076115485563758, 0.2306618581243848609, 0.2411417322834645549 ) ) ;
#65000 = CARTESIAN_POINT ( 'NONE',  ( 0.9251968503937015864, -0.5400638737290844871, 0.3530559997133364547 ) ) ;
#65001 = CARTESIAN_POINT ( 'NONE',  ( -0.3392501089628017219, -0.1958661417322836718, -1.776902887139107490 ) ) ;
#65002 = ORIENTED_EDGE ( 'NONE', *, *, #29379, .F. ) ;
#65003 = CARTESIAN_POINT ( 'NONE',  ( -0.3996062992125986035, -7.340648628747425578E-17, -0.03937007874015750059 ) ) ;
#65004 = ORIENTED_EDGE ( 'NONE', *, *, #18159, .T. ) ;
#65005 = CARTESIAN_POINT ( 'NONE',  ( 1.692913385826772421, 0.2952755905511811885, 0.000000000000000000 ) ) ;
#65006 = CARTESIAN_POINT ( 'NONE',  ( 0.9055118110236227702, -0.5511811023622047445, 6.969142054262312111E-17 ) ) ;
#65007 = DIRECTION ( 'NONE',  ( -3.096699300667737957E-16, 1.000000000000000000, -0.000000000000000000 ) ) ;
#65008 = DIRECTION ( 'NONE',  ( -1.000000000000000000, 0.000000000000000000, 0.000000000000000000 ) ) ;
#65009 = DIRECTION ( 'NONE',  ( -0.000000000000000000, -1.000000000000000000, -0.000000000000000000 ) ) ;
#65010 = CARTESIAN_POINT ( 'NONE',  ( 0.1049643490035304938, -0.3917322834645669549, -0.6423884514435697080 ) ) ;
#65011 = VECTOR ( 'NONE', #65246, 39.37007874015748143 ) ;
#65012 = CARTESIAN_POINT ( 'NONE',  ( -1.102362204724408601, -0.1870078740157480601, -0.3641732283464567677 ) ) ;
#65013 = CARTESIAN_POINT ( 'NONE',  ( 1.581364829396326277, -0.05778040916215522460, 0.4822834645669289988 ) ) ;
#65014 = CARTESIAN_POINT ( 'NONE',  ( -1.653543307086613234, -0.1870078740157479769, 0.4822834645669291653 ) ) ;
#65015 = CARTESIAN_POINT ( 'NONE',  ( -0.3280839895013117347, -0.4281496062992124485, 0.4176697321401328655 ) ) ;
#65016 = CARTESIAN_POINT ( 'NONE',  ( -1.614173228346455824, 0.2952755905511811885, 0.000000000000000000 ) ) ;
#65017 = VERTEX_POINT ( 'NONE', #58850 ) ;
#65018 = CARTESIAN_POINT ( 'NONE',  ( -1.430446194225721390, -0.4281496062992124485, 0.4176697321401328655 ) ) ;
#65019 = CARTESIAN_POINT ( 'NONE',  ( -3.937007874015748143, 2.165354330708661568, 0.3149606299212595606 ) ) ;
#65020 = DIRECTION ( 'NONE',  ( 1.047444401652940007E-14, 0.000000000000000000, -1.000000000000000000 ) ) ;
#65021 = DIRECTION ( 'NONE',  ( -1.000000000000000000, -0.000000000000000000, -0.000000000000000000 ) ) ;
#65022 = DIRECTION ( 'NONE',  ( 0.000000000000000000, -0.000000000000000000, 1.000000000000000000 ) ) ;
#65023 = CARTESIAN_POINT ( 'NONE',  ( -0.7480314960629914633, -0.5511811023622047445, 6.969142054262312111E-17 ) ) ;
#65024 = CARTESIAN_POINT ( 'NONE',  ( -1.646981627296586703, -0.05778040916215522460, 0.4822834645669289988 ) ) ;
#65025 = CARTESIAN_POINT ( 'NONE',  ( 0.5577427821522316087, -0.05778040916215522460, 0.4822834645669289988 ) ) ;
#65026 = ORIENTED_EDGE ( 'NONE', *, *, #43993, .T. ) ;
#65028 = CARTESIAN_POINT ( 'NONE',  ( 1.586052503253845503, 0.4724409448818907564, 0.1653254495020587411 ) ) ;
#65027 = CARTESIAN_POINT ( 'NONE',  ( -1.854472803289052507, 2.716535433070866645, -0.5314960629921260393 ) ) ;
#65029 = CARTESIAN_POINT ( 'NONE',  ( 1.220472440944882608, 0.2952755905511811885, 0.000000000000000000 ) ) ;
#65030 = CARTESIAN_POINT ( 'NONE',  ( 1.548556430446194954, -0.5023911411419708095, 0.1820866141732285504 ) ) ;
#65031 = CARTESIAN_POINT ( 'NONE',  ( 0.3392501089628018329, -0.1958661417322834497, -0.8149413141394206139 ) ) ;
#65032 = CARTESIAN_POINT ( 'NONE',  ( -0.4724409448818890911, -0.1870078740157479769, 0.3641732283464567677 ) ) ;
#65033 = CARTESIAN_POINT ( 'NONE',  ( -1.561679790026246017, -0.3690944881889765550, -0.3153832671262227771 ) ) ;
#65034 = CARTESIAN_POINT ( 'NONE',  ( 0.1049643490035303689, 0.3917322834645670104, -1.180446194225721834 ) ) ;
#65035 = CARTESIAN_POINT ( 'NONE',  ( 0.2952755905511816326, -0.5400638737290844871, 0.3530559997133364547 ) ) ;
#65036 = CARTESIAN_POINT ( 'NONE',  ( -0.9317585301837263412, -0.3690944881889765550, -0.3153832671262227771 ) ) ;
#65037 = CARTESIAN_POINT ( 'NONE',  ( 0.2624671916010504757, -0.5023911411419708095, -0.1820866141732282451 ) ) ;
#65038 = CARTESIAN_POINT ( 'NONE',  ( 0.09842519685039434474, -0.5400638737290845981, -0.3530559997133363437 ) ) ;
#65039 = CARTESIAN_POINT ( 'NONE',  ( -1.240157480314959759, -0.4536011799217368745, -0.2665933059059886201 ) ) ;
#65040 = CARTESIAN_POINT ( 'NONE',  ( 0.1958661417322834775, 0.3392501089628018884, -0.1410954312674034816 ) ) ;
#65041 = CARTESIAN_POINT ( 'NONE',  ( 0.7414698162729663755, -0.6692913385826773087, -0.1292274648535924053 ) ) ;
#65042 = EDGE_CURVE ( 'NONE', #29487, #80970, #32755, .T. ) ;
#65043 = CARTESIAN_POINT ( 'NONE',  ( -1.633858267716534529, 0.1660481256975885056, 0.3530559997133364547 ) ) ;
#65044 = CARTESIAN_POINT ( 'NONE',  ( 0.4724409448818897572, -0.1265901696524988906, -1.290682414698162583 ) ) ;
#65045 = CARTESIAN_POINT ( 'NONE',  ( -0.4855643044619415427, -0.4281496062992124485, 0.4176697321401328655 ) ) ;
#65046 = CARTESIAN_POINT ( 'NONE',  ( 0.1509186351706042484, -0.2845877964562159024, 0.3641732283464567677 ) ) ;
#65047 = CARTESIAN_POINT ( 'NONE',  ( -1.062992125984250968, -0.6692913385826771977, 8.415575281601705876E-17 ) ) ;
#65048 = CARTESIAN_POINT ( 'NONE',  ( 0.8923884514435703741, 0.1283753931104748280, 0.1820866141732283561 ) ) ;
#65049 = CARTESIAN_POINT ( 'NONE',  ( -0.2099737532808391705, -0.5023911411419708095, -0.1820866141732282451 ) ) ;
#65050 = CARTESIAN_POINT ( 'NONE',  ( -0.5643044619422565855, 0.05413385826771626580, -0.4176697321401330321 ) ) ;
#65051 = CARTESIAN_POINT ( 'NONE',  ( -1.318897637795274802, -0.5400638737290845981, -0.3530559997133363437 ) ) ;
#65052 = CARTESIAN_POINT ( 'NONE',  ( 1.679790026246720025, 0.2306618581243848609, 0.2411417322834645549 ) ) ;
#65053 = CARTESIAN_POINT ( 'NONE',  ( 1.062992125984252523, 0.2066929133858268208, 0.000000000000000000 ) ) ;
#65054 = CARTESIAN_POINT ( 'NONE',  ( 1.253280839895013710, -0.08942795157528024563, -0.3641732283464568787 ) ) ;
#65055 = AXIS2_PLACEMENT_3D ( 'NONE', #61271, #72668, #73084 ) ;
#65056 = CARTESIAN_POINT ( 'NONE',  ( 0.3083989501312343062, -0.05778040916215560624, -0.4822834645669293319 ) ) ;
#65057 = CARTESIAN_POINT ( 'NONE',  ( -1.627296587926508442, 0.2306618581243848609, 0.2411417322834645549 ) ) ;
#65058 = CARTESIAN_POINT ( 'NONE',  ( -1.437007874015747477, -0.5400638737290844871, 0.3530559997133364547 ) ) ;
#65059 = ORIENTED_EDGE ( 'NONE', *, *, #61531, .T. ) ;
#65060 = CARTESIAN_POINT ( 'NONE',  ( 4.893765752498283308E-17, -0.3996062992125985480, -2.202755905511811108 ) ) ;
#65061 = CARTESIAN_POINT ( 'NONE',  ( -0.6955380577427815458, -0.004921259842519576551, 0.3153832671262227771 ) ) ;
#65062 = CARTESIAN_POINT ( 'NONE',  ( 0.8530183727034126306, 0.05413385826771626580, -0.4176697321401330321 ) ) ;
#65063 = CARTESIAN_POINT ( 'NONE',  ( -0.9055118110236215490, 0.1771653543307087630, 0.000000000000000000 ) ) ;
#65064 = CARTESIAN_POINT ( 'NONE',  ( -0.1998031496062991630, -0.3460692066303959202, -1.717191601049869121 ) ) ;
#65065 = CARTESIAN_POINT ( 'NONE',  ( -1.200787401574802349, 0.1660481256975883668, -0.3530559997133364547 ) ) ;
#65066 = CARTESIAN_POINT ( 'NONE',  ( 0.7611548556430454138, 0.2306618581243847221, -0.2411417322834647770 ) ) ;
#65067 = CARTESIAN_POINT ( 'NONE',  ( 0.5183727034120741983, -0.6692913385826771977, 0.1292274648535927661 ) ) ;
#65068 = CARTESIAN_POINT ( 'NONE',  ( 5.785732909357575061E-17, -0.4724409448818898682, -0.07874015748031495954 ) ) ;
#65069 = CARTESIAN_POINT ( 'NONE',  ( -1.712598425196849572, 0.07958543189024085140, 0.2665933059059887866 ) ) ;
#65070 = CARTESIAN_POINT ( 'NONE',  ( 0.3996062992125985480, -0.1070741851644052972, -1.133202099737532720 ) ) ;
#65071 = CARTESIAN_POINT ( 'NONE',  ( -0.1998031496062991907, -0.3460692066303959757, -1.325459317585301777 ) ) ;
#65072 = VECTOR ( 'NONE', #9794, 39.37007874015748143 ) ;
#65073 = CARTESIAN_POINT ( 'NONE',  ( -0.3949938075777409408, -0.1058382717557502933, -0.6758530183727035068 ) ) ;
#65074 = CARTESIAN_POINT ( 'NONE',  ( 0.4562095852119599781, 1.668416680336031188, 2.594411373832410828 ) ) ;
#65075 = CARTESIAN_POINT ( 'NONE',  ( 0.8727034120734913358, -0.08942795157527998196, 0.3641732283464567121 ) ) ;
#65076 = CARTESIAN_POINT ( 'NONE',  ( 0.2034120734908142214, 0.1771653543307087075, -0.09757992244046823083 ) ) ;
#65077 = CARTESIAN_POINT ( 'NONE',  ( 0.03280839895013198948, 0.2952755905511811885, 0.1292274648535926551 ) ) ;
#65078 = CARTESIAN_POINT ( 'NONE',  ( 1.115485564304462551, 0.05413385826771666132, 0.4176697321401328100 ) ) ;
#65079 = CARTESIAN_POINT ( 'NONE',  ( -0.1058382717557503072, 0.3949938075777408852, -1.815616797900262869 ) ) ;
#65080 = CARTESIAN_POINT ( 'NONE',  ( 0.5839895013123367340, 0.1771653543307087630, 0.09757992244046791164 ) ) ;
#65081 = CARTESIAN_POINT ( 'NONE',  ( -0.6692913385826764205, 0.2952755905511811885, 0.000000000000000000 ) ) ;
#65082 = CARTESIAN_POINT ( 'NONE',  ( 1.430446194225722500, 0.05413385826771666132, 0.4176697321401328100 ) ) ;
#65083 = CARTESIAN_POINT ( 'NONE',  ( 0.9776902887139113929, -0.6692913385826773087, -0.1292274648535924053 ) ) ;
#65084 = CARTESIAN_POINT ( 'NONE',  ( 0.4091458600556404646, -0.2362204724409448231, -2.152230971128608950 ) ) ;
#65085 = CARTESIAN_POINT ( 'NONE',  ( 1.171093442848939681, -8.644661201599092366E-16, -0.4445507791589066171 ) ) ;
#65086 = VERTEX_POINT ( 'NONE', #14255 ) ;
#65087 = ORIENTED_EDGE ( 'NONE', *, *, #71325, .F. ) ;
#65088 = CARTESIAN_POINT ( 'NONE',  ( -1.332020997375327642, -0.3162353388693409650, -0.4822834645669289433 ) ) ;
#65089 = CARTESIAN_POINT ( 'NONE',  ( -1.181102362204723644, -0.1870078740157479769, 0.4822834645669291653 ) ) ;
#65091 = CARTESIAN_POINT ( 'NONE',  ( -0.5708661417322825615, -0.5400638737290844871, 0.3530559997133364547 ) ) ;
#65090 = CARTESIAN_POINT ( 'NONE',  ( -0.8595800524934373854, -0.08942795157527998196, 0.3641732283464567121 ) ) ;
#65092 = CARTESIAN_POINT ( 'NONE',  ( -0.1049643490035301746, -0.3917322834645670659, -2.356936064795589036 ) ) ;
#65093 = DIRECTION ( 'NONE',  ( 0.000000000000000000, -1.000000000000000000, 0.000000000000000000 ) ) ;
#65094 = CARTESIAN_POINT ( 'NONE',  ( 1.601049868766404982, -0.6046776061558809534, -0.2411417322834644161 ) ) ;
#65095 = CARTESIAN_POINT ( 'NONE',  ( -1.437007874015747477, -0.5400638737290844871, 0.3530559997133364547 ) ) ;
#65096 = CARTESIAN_POINT ( 'NONE',  ( 0.4330708661417329575, -0.6692913385826771977, 8.415575281601705876E-17 ) ) ;
#65097 = B_SPLINE_CURVE_WITH_KNOTS ( 'NONE', 3,
 ( #53959, #3049, #54378, #68278 ),
 .UNSPECIFIED., .F., .F.,
 ( 4, 4 ),
 ( 1.999999999910059834E-07, 0.006970199999999934261 ),
 .UNSPECIFIED. ) ;
#65098 = CARTESIAN_POINT ( 'NONE',  ( -0.9055118110236215490, -0.6692913385826771977, 8.415575281601705876E-17 ) ) ;
#65099 = CARTESIAN_POINT ( 'NONE',  ( -0.2867679344610364334, -0.2867679344610367109, 0.1712598425196849850 ) ) ;
#65100 = CARTESIAN_POINT ( 'NONE',  ( 0.5577427821522314977, -0.3162353388693409650, -0.4822834645669289433 ) ) ;
#65101 = CARTESIAN_POINT ( 'NONE',  ( 0.3917322834645669549, 0.1049643490035304660, -2.006561679790026531 ) ) ;
#65102 = CARTESIAN_POINT ( 'NONE',  ( -0.6889763779527552368, 0.07958543189024085140, 0.2665933059059887866 ) ) ;
#65103 = ORIENTED_EDGE ( 'NONE', *, *, #37312, .F. ) ;
#65104 = CARTESIAN_POINT ( 'NONE',  ( 4.837279021331060870E-17, -0.3949938075777409963, -1.811023622047243986 ) ) ;
#65105 = EDGE_LOOP ( 'NONE', ( #12298, #25204, #62294, #27539 ) ) ;
#65106 = CARTESIAN_POINT ( 'NONE',  ( -1.555118110236219930, 0.07958543189024085140, 0.2665933059059887866 ) ) ;
#65107 = CARTESIAN_POINT ( 'NONE',  ( -1.174540682414697335, -0.3162353388693409650, -0.4822834645669289433 ) ) ;
#65108 = CARTESIAN_POINT ( 'NONE',  ( -1.213910761154854745, -0.6692913385826771977, 0.1292274648535927661 ) ) ;
#65109 = CARTESIAN_POINT ( 'NONE',  ( -0.2925321140481932924, 0.2925321140481931814, -0.6496062992125984925 ) ) ;
#65110 = CARTESIAN_POINT ( 'NONE',  ( -0.9251968503937002541, 0.1660481256975885056, 0.3530559997133364547 ) ) ;
#65111 = CARTESIAN_POINT ( 'NONE',  ( -1.240157480314959759, 0.1660481256975885056, 0.3530559997133364547 ) ) ;
#65112 = CARTESIAN_POINT ( 'NONE',  ( -1.627296587926508442, 0.2306618581243848609, 0.2411417322834645549 ) ) ;
#65113 = DIRECTION ( 'NONE',  ( 0.000000000000000000, -1.000000000000000000, 0.000000000000000000 ) ) ;
#65114 = EDGE_CURVE ( 'NONE', #44445, #60047, #46209, .T. ) ;
#65115 = LINE ( 'NONE', #724, #25402 ) ;
#65116 = CARTESIAN_POINT ( 'NONE',  ( 0.1837270341207357105, -0.5023911411419708095, -0.1820866141732282451 ) ) ;
#65117 = FACE_OUTER_BOUND ( 'NONE', #75120, .T. ) ;
#65118 = CARTESIAN_POINT ( 'NONE',  ( 0.2867679344610365999, -0.2867679344610365444, -0.4980314960629922405 ) ) ;
#65119 = CARTESIAN_POINT ( 'NONE',  ( -0.2493438320209966919, -0.004921259842519870586, -0.3153832671262229437 ) ) ;
#65120 =( GEOMETRIC_REPRESENTATION_CONTEXT ( 3 ) GLOBAL_UNCERTAINTY_ASSIGNED_CONTEXT ( ( #20112 ) ) GLOBAL_UNIT_ASSIGNED_CONTEXT ( ( #1164, #11202, #60466 ) ) REPRESENTATION_CONTEXT ( 'NONE', 'WORKASPACE' ) );
#65121 = CARTESIAN_POINT ( 'NONE',  ( -0.9120734908136475250, -0.6692913385826773087, -0.1292274648535924053 ) ) ;
#65122 = ADVANCED_FACE ( 'NONE', ( #59259 ), #13830, .F. ) ;
#65123 = CARTESIAN_POINT ( 'NONE',  ( 0.8530183727034126306, 0.05413385826771626580, -0.4176697321401330321 ) ) ;
#65124 = CARTESIAN_POINT ( 'NONE',  ( -0.3346456692913377662, 0.1660481256975883668, -0.3530559997133364547 ) ) ;
#65125 = ORIENTED_EDGE ( 'NONE', *, *, #78984, .T. ) ;
#65126 = ORIENTED_EDGE ( 'NONE', *, *, #8539, .T. ) ;
#65127 = CARTESIAN_POINT ( 'NONE',  ( 4.893765752498283308E-17, -0.3996062992125985480, -1.887795275590550936 ) ) ;
#65128 = CARTESIAN_POINT ( 'NONE',  ( -0.9383202099737524282, -0.3162353388693409650, -0.4822834645669289433 ) ) ;
#65129 = CARTESIAN_POINT ( 'NONE',  ( 1.200787401574803681, -0.5400638737290845981, -0.3530559997133363437 ) ) ;
#65130 = CARTESIAN_POINT ( 'NONE',  ( -1.384514435695537005, 0.1771653543307087630, 0.09757992244046791164 ) ) ;
#65131 = CARTESIAN_POINT ( 'NONE',  ( -1.620734908136482577, -0.6692913385826773087, -0.1292274648535924053 ) ) ;
#65132 = CARTESIAN_POINT ( 'NONE',  ( 0.4091458600556404646, -0.2362204724409448231, -0.8923884514435694859 ) ) ;
#65133 = CARTESIAN_POINT ( 'NONE',  ( 0.000000000000000000, -1.268531780058464091E-17, 0.000000000000000000 ) ) ;
#65134 = CARTESIAN_POINT ( 'NONE',  ( -0.2867679344610364334, -0.2867679344610367109, -0.3661417322834645827 ) ) ;
#65135 = CARTESIAN_POINT ( 'NONE',  ( 0.2867679344610366554, -0.2867679344610365444, -2.072834645669292097 ) ) ;
#65136 = CARTESIAN_POINT ( 'NONE',  ( -0.2427821522309703550, -0.3162353388693405765, 0.4822834645669290543 ) ) ;
#65137 = CARTESIAN_POINT ( 'NONE',  ( 1.692913385826772421, 0.2952755905511811885, 0.000000000000000000 ) ) ;
#65138 = CARTESIAN_POINT ( 'NONE',  ( -0.6692913385826764205, -0.6692913385826771977, 8.415575281601705876E-17 ) ) ;
#65139 = CARTESIAN_POINT ( 'NONE',  ( -0.3460692066303957537, -0.1998031496062994405, -0.1292650918635170898 ) ) ;
#65141 = CARTESIAN_POINT ( 'NONE',  ( 5.785732909357575061E-17, -0.4724409448818898682, -1.100393700787401619 ) ) ;
#65140 = CARTESIAN_POINT ( 'NONE',  ( -1.167979002624671470, -0.4281496062992127816, -0.4176697321401328100 ) ) ;
#65142 = CARTESIAN_POINT ( 'NONE',  ( -1.102362204724408601, -0.1870078740157479769, 0.4822834645669291653 ) ) ;
#65143 = CARTESIAN_POINT ( 'NONE',  ( -0.5052493438320203589, -0.6692913385826771977, 0.1292274648535927661 ) ) ;
#65144 = AXIS2_PLACEMENT_3D ( 'NONE', #79908, #66857, #29363 ) ;
#65145 = CARTESIAN_POINT ( 'NONE',  ( -0.1058382717557497660, -0.3949938075777411073, -2.511154855643044748 ) ) ;
#65146 = CARTESIAN_POINT ( 'NONE',  ( 0.8333333333333340365, 0.1771653543307087075, -0.09757992244046823083 ) ) ;
#65147 = CARTESIAN_POINT ( 'NONE',  ( -1.112371124080194340, -2.567464376874931580E-15, -0.4445507791589072832 ) ) ;
#65148 = CARTESIAN_POINT ( 'NONE',  ( 0.6036745406824154392, 0.1283753931104746893, -0.1820866141732285504 ) ) ;
#65149 = CARTESIAN_POINT ( 'NONE',  ( 1.351706036745407458, -0.3690944881889765550, -0.3153832671262227771 ) ) ;
#65150 = CARTESIAN_POINT ( 'NONE',  ( 1.220472440944882386, -0.6692913385826771977, 8.415575281601705876E-17 ) ) ;
#65151 = CARTESIAN_POINT ( 'NONE',  ( 0.07874015748031558404, -0.1870078740157479769, 0.3641732283464567677 ) ) ;
#65152 = CARTESIAN_POINT ( 'NONE',  ( 0.3392501089628018884, -0.1958661417322834220, -1.829396325459317518 ) ) ;
#65153 = CARTESIAN_POINT ( 'NONE',  ( -1.095800524934382292, -0.3162353388693409650, -0.4822834645669289433 ) ) ;
#65154 = CARTESIAN_POINT ( 'NONE',  ( 1.227034120734908917, -0.6692913385826771977, 0.1292274648535927661 ) ) ;
#65155 =( BOUNDED_CURVE ( )  B_SPLINE_CURVE ( 1, ( #42274, #3990 ),
 .UNSPECIFIED., .F., .F. ) 
 B_SPLINE_CURVE_WITH_KNOTS ( ( 2, 2 ),
 ( 4.770489558936219510E-18, 0.002000000000000006981 ),
 .UNSPECIFIED. ) 
 CURVE ( )  GEOMETRIC_REPRESENTATION_ITEM ( )  RATIONAL_B_SPLINE_CURVE ( ( 0.9875488213027530104, 0.9875488213027530104 ) ) 
 REPRESENTATION_ITEM ( '' )  );
#65156 = CARTESIAN_POINT ( 'NONE',  ( -0.3458507752293906723, -0.3458507752293910609, 0.02165354330708659653 ) ) ;
#65157 = CARTESIAN_POINT ( 'NONE',  ( -0.6889763779527552368, 0.07958543189024085140, 0.2665933059059887866 ) ) ;
#65158 = CARTESIAN_POINT ( 'NONE',  ( 0.01000891935578606708, -2.191421614605370878E-15, 0.4445507791589071167 ) ) ;
#65159 = CARTESIAN_POINT ( 'NONE',  ( 0.4068241469816281097, 0.05413385826771666132, 0.4176697321401328100 ) ) ;
#65160 = CYLINDRICAL_SURFACE ( 'NONE', #53250, 2.362204724409449064 ) ;
#65161 = EDGE_CURVE ( 'NONE', #63010, #45388, #48149, .T. ) ;
#65162 = CARTESIAN_POINT ( 'NONE',  ( 0.7611548556430451917, -0.5023911411419708095, 0.1820866141732285504 ) ) ;
#65163 = CARTESIAN_POINT ( 'NONE',  ( 0.3215223097112867578, -0.08942795157527998196, 0.3641732283464567121 ) ) ;
#65164 = CARTESIAN_POINT ( 'NONE',  ( -0.4593175853018364174, -0.4281496062992127816, -0.4176697321401328100 ) ) ;
#65165 = CARTESIAN_POINT ( 'NONE',  ( -1.181102362204723644, -0.1870078740157480879, -0.4822834645669291653 ) ) ;
#65166 = CARTESIAN_POINT ( 'NONE',  ( -0.8464566929133852113, 0.07958543189024085140, 0.2665933059059887866 ) ) ;
#65167 = CARTESIAN_POINT ( 'NONE',  ( -2.583694225513480713, 2.755905511811024056, -0.5314960629921260393 ) ) ;
#65168 = CARTESIAN_POINT ( 'NONE',  ( 0.5774278215223104249, 0.2306618581243848609, 0.2411417322834645549 ) ) ;
#65169 = CARTESIAN_POINT ( 'NONE',  ( -0.7414698162729651543, -0.6692913385826771977, 0.1292274648535927661 ) ) ;
#65170 = CARTESIAN_POINT ( 'NONE',  ( -0.3460692066303957537, -0.1998031496062994405, -1.231627296587926468 ) ) ;
#65171 = CARTESIAN_POINT ( 'NONE',  ( -0.3917322834645670104, -7.196005306013484475E-17, -2.801181102362204633 ) ) ;
#65172 = CARTESIAN_POINT ( 'NONE',  ( 0.1246719160104994284, -0.5511811023622046335, 0.09757992244046803654 ) ) ;
#65173 = CARTESIAN_POINT ( 'NONE',  ( -0.6496062992125976043, 0.1660481256975883668, -0.3530559997133364547 ) ) ;
#65174 = CARTESIAN_POINT ( 'NONE',  ( -1.292650918635170010, 0.2952755905511810774, -0.1292274648535930714 ) ) ;
#65175 = CARTESIAN_POINT ( 'NONE',  ( -1.069553805774277722, -0.5511811023622048555, -0.09757992244046775898 ) ) ;
#65176 = CARTESIAN_POINT ( 'NONE',  ( 1.348312163386739426, 0.2755905511811023723, 0.8577811012195456497 ) ) ;
#65177 = CARTESIAN_POINT ( 'NONE',  ( -0.8858267716535425107, -0.4536011799217367080, 0.2665933059059888421 ) ) ;
#65178 = CARTESIAN_POINT ( 'NONE',  ( -0.7283464566929126471, 0.1012011053420775880, -0.2882089793578257453 ) ) ;
#65179 = CARTESIAN_POINT ( 'NONE',  ( 1.286089238845145033, 0.2306618581243848609, 0.2411417322834645549 ) ) ;
#65180 = CARTESIAN_POINT ( 'NONE',  ( 0.3460692066303959202, 0.1998031496062993295, 0.02624671916010497957 ) ) ;
#65181 = CARTESIAN_POINT ( 'NONE',  ( 0.3917322834645670659, -0.1049643490035303273, -2.313011441766091192 ) ) ;
#65182 = VERTEX_POINT ( 'NONE', #65176 ) ;
#65183 =( GEOMETRIC_REPRESENTATION_CONTEXT ( 3 ) GLOBAL_UNCERTAINTY_ASSIGNED_CONTEXT ( ( #25993 ) ) GLOBAL_UNIT_ASSIGNED_CONTEXT ( ( #57438, #81911, #24223 ) ) REPRESENTATION_CONTEXT ( 'NONE', 'WORKASPACE' ) );
#65184 = CARTESIAN_POINT ( 'NONE',  ( 0.02707642104390755797, -0.3965571307776183940, -3.856971560569892101E-17 ) ) ;
#65185 = CARTESIAN_POINT ( 'NONE',  ( -1.601049868766403650, -0.6046776061558807314, 0.2411417322834647770 ) ) ;
#65186 = CARTESIAN_POINT ( 'NONE',  ( -1.220472440944881054, 0.2952755905511811885, 0.000000000000000000 ) ) ;
#65187 = CARTESIAN_POINT ( 'NONE',  ( 1.069553805774278610, -0.6692913385826771977, 0.1292274648535927661 ) ) ;
#65188 = CARTESIAN_POINT ( 'NONE',  ( -0.3917322834645669549, -0.1049643490035306603, -2.335301837270341352 ) ) ;
#65189 = CARTESIAN_POINT ( 'NONE',  ( 1.620734908136483465, -0.5511811023622046335, 0.09757992244046803654 ) ) ;
#65190 = CARTESIAN_POINT ( 'NONE',  ( 0.4002624671916016896, -0.05778040916215522460, 0.4822834645669289988 ) ) ;
#65191 = CARTESIAN_POINT ( 'NONE',  ( -0.1049868766404193215, -0.6046776061558807314, 0.2411417322834647770 ) ) ;
#65192 = CARTESIAN_POINT ( 'NONE',  ( 0.4116952507455398091, 1.299637793558053644, -3.915461318743572505 ) ) ;
#65193 = CARTESIAN_POINT ( 'NONE',  ( -0.1998031496062991907, -0.3460692066303959757, -1.955380577427821454 ) ) ;
#65194 = CARTESIAN_POINT ( 'NONE',  ( 0.7808398950131240079, -0.2845877964562159024, 0.3641732283464567677 ) ) ;
#65195 = CARTESIAN_POINT ( 'NONE',  ( 0.3996062992125986035, 0.1070741851644054776, -1.384514435695537671 ) ) ;
#65196 = VERTEX_POINT ( 'NONE', #79067 ) ;
#65198 = CARTESIAN_POINT ( 'NONE',  ( -0.1049643490035302301, -0.3917322834645671770, -0.06891695357711476178 ) ) ;
#65197 = CIRCLE ( 'NONE', #28904, 1.889763779527559251 ) ;
#65199 = VERTEX_POINT ( 'NONE', #40327 ) ;
#65200 = CARTESIAN_POINT ( 'NONE',  ( -0.05905511811023545637, -0.5400638737290845981, -0.3530559997133363437 ) ) ;
#65201 = CARTESIAN_POINT ( 'NONE',  ( 1.463254593175853824, 0.2952755905511810774, -0.1292274648535930714 ) ) ;
#65202 = CARTESIAN_POINT ( 'NONE',  ( 0.5183727034120741983, -0.6692913385826771977, 0.1292274648535927661 ) ) ;
#65203 = CARTESIAN_POINT ( 'NONE',  ( 1.174540682414699111, -0.3162353388693405765, 0.4822834645669290543 ) ) ;
#65204 = CARTESIAN_POINT ( 'NONE',  ( -0.3412073490813641308, 0.2306618581243847221, -0.2411417322834647770 ) ) ;
#65205 = CARTESIAN_POINT ( 'NONE',  ( 0.1509186351706042484, -0.3162353388693405765, 0.4822834645669290543 ) ) ;
#65206 = CARTESIAN_POINT ( 'NONE',  ( -1.496062992125983815, -0.1870078740157479769, 0.4822834645669291653 ) ) ;
#65207 = CARTESIAN_POINT ( 'NONE',  ( 1.391076115485564868, -0.6046776061558807314, 0.2411417322834647770 ) ) ;
#65208 = CARTESIAN_POINT ( 'NONE',  ( 1.272965879265092637, -0.4281496062992127816, -0.4176697321401328100 ) ) ;
#65209 = CARTESIAN_POINT ( 'NONE',  ( -0.1958661417322834220, -0.3392501089628018884, -0.2152230971128608339 ) ) ;
#65210 = CARTESIAN_POINT ( 'NONE',  ( 0.2427821522309719648, -0.08942795157527998196, 0.3641732283464567121 ) ) ;
#65211 = VERTEX_POINT ( 'NONE', #39913 ) ;
#65212 = CARTESIAN_POINT ( 'NONE',  ( 0.3949938075777409963, 2.418639510665530435E-17, -0.5905511811023622659 ) ) ;
#65213 = ORIENTED_EDGE ( 'NONE', *, *, #35790, .T. ) ;
#65214 = CARTESIAN_POINT ( 'NONE',  ( -0.4265091863517051496, 0.1771653543307087075, -0.09757992244046823083 ) ) ;
#65215 = CARTESIAN_POINT ( 'NONE',  ( 0.03280839895013198948, -0.6692913385826773087, -0.1292274648535924053 ) ) ;
#65216 = CARTESIAN_POINT ( 'NONE',  ( 2.872985923768004213, 1.064103292658513666, 0.03357545743407176764 ) ) ;
#65217 = CARTESIAN_POINT ( 'NONE',  ( -0.04593175853018302557, -0.6692913385826773087, -0.1292274648535924053 ) ) ;
#65218 = CARTESIAN_POINT ( 'NONE',  ( 0.09842519685039434474, -0.5400638737290845981, -0.3530559997133363437 ) ) ;
#65219 = CARTESIAN_POINT ( 'NONE',  ( -0.6889763779527552368, 0.1660481256975885056, 0.3530559997133364547 ) ) ;
#65220 = ADVANCED_FACE ( 'NONE', ( #72323 ), #28882, .F. ) ;
#65221 = CARTESIAN_POINT ( 'NONE',  ( -1.082677165354329896, 0.1660481256975885056, 0.3530559997133364547 ) ) ;
#65222 = CARTESIAN_POINT ( 'NONE',  ( 1.489501312335958172, -0.2845877964562159024, 0.3641732283464567677 ) ) ;
#65223 = DIRECTION ( 'NONE',  ( -3.491481338843132961E-15, -0.000000000000000000, 1.000000000000000000 ) ) ;
#65224 = FACE_OUTER_BOUND ( 'NONE', #1125, .T. ) ;
#65225 = CARTESIAN_POINT ( 'NONE',  ( 0.9514435695538062676, -0.08942795157527998196, 0.3641732283464567121 ) ) ;
#65226 = CARTESIAN_POINT ( 'NONE',  ( 0.5183727034120741983, -0.6692913385826771977, 0.1292274648535927661 ) ) ;
#65227 = CARTESIAN_POINT ( 'NONE',  ( 0.6758530183727039509, -0.6692913385826771977, 0.1292274648535927661 ) ) ;
#65228 = CARTESIAN_POINT ( 'NONE',  ( -0.3460692066303958092, -0.1998031496062994683, -1.469816272965879245 ) ) ;
#65229 = CARTESIAN_POINT ( 'NONE',  ( -1.633858267716534529, -0.5400638737290845981, -0.3530559997133363437 ) ) ;
#65230 = CARTESIAN_POINT ( 'NONE',  ( -0.1998031496062991630, -0.3460692066303959202, -0.6148293963254594097 ) ) ;
#65231 = B_SPLINE_CURVE_WITH_KNOTS ( 'NONE', 3,
 ( #78183, #12951, #12531, #19247, #321, #71862, #14212, #27233, #31882, #25975, #39020, #51221, #39870, #65559, #38609, #52892, #38192, #25554, #52056, #57542, #83233, #20094, #64287, #51633, #77337, #8302, #65966, #1987, #53724, #48247, #21344, #41114, #3645, #8716, #66803, #2408, #21750, #47829, #9138, #34809, #22170, #9958, #72690, #73532, #46997, #33970, #73104, #59631, #41932, #15038, #60468, #27650, #79431, #46584, #14629, #72283, #22586, #40693, #80680, #67627 ),
 .UNSPECIFIED., .F., .F.,
 ( 4, 2, 2, 2, 2, 2, 2, 2, 2, 2, 2, 2, 2, 2, 2, 2, 2, 2, 2, 2, 2, 2, 2, 2, 2, 2, 2, 2, 2, 4 ),
 ( 0.01323639539072356784, 0.01388181161316722097, 0.01452722783561087409, 0.01581806028049817514, 0.01710889272538547792, 0.01839972517027278071, 0.02098139006004740015, 0.02356305494982201612, 0.02485388739470933625, 0.02614471983959665291, 0.02743555228448397304, 0.02872638472937128623, 0.03130804961914591955, 0.03259888206403323274, 0.03388971450892054593, 0.03453513073136420253, 0.03518054695380785912, 0.03647137939869517925, 0.03776221184358249244, 0.03905304428846980563, 0.04034387673335712576, 0.04163470917824443895, 0.04421637406801907921, 0.04679803895779371253, 0.04937970384756834585, 0.05067053629245565904, 0.05196136873734297223, 0.05325220118223029236, 0.05389761740467396284, 0.05454303362711762637 ),
 .UNSPECIFIED. ) ;
#65232 = CARTESIAN_POINT ( 'NONE',  ( 4.893765752498283308E-17, -0.3996062992125985480, 0.001968503937007844932 ) ) ;
#65233 = CARTESIAN_POINT ( 'NONE',  ( -0.3805774278215216522, -0.4281496062992127816, -0.4176697321401328100 ) ) ;
#65234 = CARTESIAN_POINT ( 'NONE',  ( -0.1998031496062994683, 0.3460692066303958092, -2.690288713910760965 ) ) ;
#65235 = CARTESIAN_POINT ( 'NONE',  ( 0.2867679344610365999, -0.2867679344610365444, -2.230314960629921295 ) ) ;
#65236 = CARTESIAN_POINT ( 'NONE',  ( -1.194225721784776262, -0.3690944881889763329, 0.3153832671262228327 ) ) ;
#65237 = CARTESIAN_POINT ( 'NONE',  ( 1.496062992125984703, -0.1870078740157480879, -0.4822834645669291653 ) ) ;
#65238 = CARTESIAN_POINT ( 'NONE',  ( 0.8136482939632553313, -0.6046776061558809534, -0.2411417322834644161 ) ) ;
#65239 = CARTESIAN_POINT ( 'NONE',  ( -0.2559055118110227234, -0.4536011799217367080, 0.2665933059059888421 ) ) ;
#65240 = CARTESIAN_POINT ( 'NONE',  ( 0.4133858267716541968, -0.5400638737290845981, -0.3530559997133363437 ) ) ;
#65241 = CARTESIAN_POINT ( 'NONE',  ( -0.2362204724409451284, 0.4091458600556402425, -1.507217847769029007 ) ) ;
#65242 = CARTESIAN_POINT ( 'NONE',  ( 0.3018372703412079971, -0.004921259842519870586, -0.3153832671262229437 ) ) ;
#65243 = CARTESIAN_POINT ( 'NONE',  ( -0.1902887139107604098, -0.6692913385826771977, 0.1292274648535927661 ) ) ;
#65244 = CARTESIAN_POINT ( 'NONE',  ( -0.3420746716998662729, 0.1974969037888702206, -1.520341207349081181 ) ) ;
#65245 = CARTESIAN_POINT ( 'NONE',  ( -1.062992125984250968, 0.2952755905511811885, 0.000000000000000000 ) ) ;
#65246 = DIRECTION ( 'NONE',  ( -0.000000000000000000, -0.000000000000000000, -1.000000000000000000 ) ) ;
#65247 = CARTESIAN_POINT ( 'NONE',  ( 0.5643044619422579178, -0.3690944881889765550, -0.3153832671262227771 ) ) ;
#65248 = CARTESIAN_POINT ( 'NONE',  ( 0.3346456692913390985, 0.1012011053420777407, 0.2882089793578257453 ) ) ;
#65249 = CARTESIAN_POINT ( 'NONE',  ( -0.8727034120734901146, -0.05778040916215560624, -0.4822834645669293319 ) ) ;
#65250 = CARTESIAN_POINT ( 'NONE',  ( -0.2427821522309703550, -0.2845877964562159024, 0.3641732283464567677 ) ) ;
#65251 = CARTESIAN_POINT ( 'NONE',  ( -1.614173228346456712, 0.4410134679336886188, -0.1372047244094478091 ) ) ;
#65252 = CARTESIAN_POINT ( 'NONE',  ( -0.7742782152230965886, 0.05413385826771666132, 0.4176697321401328100 ) ) ;
#65253 = CARTESIAN_POINT ( 'NONE',  ( -0.7480314960629914633, -0.6692913385826771977, 8.415575281601705876E-17 ) ) ;
#65254 = CARTESIAN_POINT ( 'NONE',  ( 0.5249343832021003964, 0.1283753931104746893, -0.1820866141732285504 ) ) ;
#65255 = CARTESIAN_POINT ( 'NONE',  ( 0.2925321140481932369, -0.2925321140481931814, -2.064960629921259727 ) ) ;
#65256 = CARTESIAN_POINT ( 'NONE',  ( -0.1640419947506553400, -0.05778040916215560624, -0.4822834645669293319 ) ) ;
#65257 = CARTESIAN_POINT ( 'NONE',  ( -0.3917322834645668994, -0.1049643490035306742, -2.173209030674854159 ) ) ;
#65258 = AXIS2_PLACEMENT_3D ( 'NONE', #26904, #78272, #20603 ) ;
#65259 = CYLINDRICAL_SURFACE ( 'NONE', #8602, 0.4744094488188972947 ) ;
#65260 = CARTESIAN_POINT ( 'NONE',  ( 0.8267716535433078384, -0.5511811023622047445, 6.969142054262312111E-17 ) ) ;
#65261 = CARTESIAN_POINT ( 'NONE',  ( 1.345144356955381593, -0.3162353388693409650, -0.4822834645669289433 ) ) ;
#65262 = CARTESIAN_POINT ( 'NONE',  ( -0.7939632545931754048, -0.2845877964562159024, 0.3641732283464567677 ) ) ;
#65263 = CARTESIAN_POINT ( 'NONE',  ( -1.161417322834644716, -0.4536011799217368745, -0.2665933059059886201 ) ) ;
#65264 = CARTESIAN_POINT ( 'NONE',  ( -0.8005249343832011588, 0.05413385826771626580, -0.4176697321401330321 ) ) ;
#65265 = CARTESIAN_POINT ( 'NONE',  ( -0.2165354330708654795, -0.5400638737290845981, -0.3530559997133363437 ) ) ;
#65266 = CARTESIAN_POINT ( 'NONE',  ( 0.5446194225721792126, -0.2845877964562159024, 0.3641732283464567677 ) ) ;
#65267 = CARTESIAN_POINT ( 'NONE',  ( -0.2362235781738432072, 0.1771612133531280942, 5.714029142339813738 ) ) ;
#65268 = CARTESIAN_POINT ( 'NONE',  ( 1.036745406824147508, -0.3690944881889765550, -0.3153832671262227771 ) ) ;
#65269 = CARTESIAN_POINT ( 'NONE',  ( 0.4265091863517067594, 0.2952755905511811885, 0.1292274648535926551 ) ) ;
#65270 = CARTESIAN_POINT ( 'NONE',  ( -0.3460692066303957537, -0.1998031496062994405, 0.02821522309711285356 ) ) ;
#65271 = CARTESIAN_POINT ( 'NONE',  ( -0.5314960629921254842, -0.5400638737290845981, -0.3530559997133363437 ) ) ;
#65272 = CARTESIAN_POINT ( 'NONE',  ( -0.1958661417322836718, 0.3392501089628017219, -1.357611548556430625 ) ) ;
#65273 = CARTESIAN_POINT ( 'NONE',  ( 1.522309711286089939, -0.5023911411419708095, -0.1820866141732282451 ) ) ;
#65274 = CARTESIAN_POINT ( 'NONE',  ( 0.5643044619422579178, 0.05413385826771666132, 0.4176697321401328100 ) ) ;
#65275 = CARTESIAN_POINT ( 'NONE',  ( 0.1246719160104994284, 0.2952755905511810774, -0.1292274648535930714 ) ) ;
#65276 = LINE ( 'NONE', #79163, #11818 ) ;
#65277 = CARTESIAN_POINT ( 'NONE',  ( 0.09842519685039434474, 0.07958543189024085140, 0.2665933059059887866 ) ) ;
#65278 = CARTESIAN_POINT ( 'NONE',  ( 0.7939632545931766261, -0.3162353388693409650, -0.4822834645669289433 ) ) ;
#65279 = CARTESIAN_POINT ( 'NONE',  ( -0.6299212598425188991, -0.1870078740157479769, 0.3641732283464567677 ) ) ;
#65280 = CARTESIAN_POINT ( 'NONE',  ( -0.6758530183727028406, 0.2952755905511811885, 0.1292274648535926551 ) ) ;
#65281 = CARTESIAN_POINT ( 'NONE',  ( -0.03443470937339728616, 0.000000000000000000, -1.537015892239756099 ) ) ;
#65282 = CARTESIAN_POINT ( 'NONE',  ( -0.3543307086614165824, -0.6692913385826771977, 8.415575281601705876E-17 ) ) ;
#65283 = B_SPLINE_CURVE_WITH_KNOTS ( 'NONE', 3,
 ( #55331, #10742, #66751, #42706, #3594, #47778, #61240, #54923, #41879, #80630 ),
 .UNSPECIFIED., .F., .F.,
 ( 4, 2, 2, 2, 4 ),
 ( 4.336808689942017736E-19, 0.0007778963758021331535, 0.001555792751604265873, 0.002333689127406398701, 0.003111585503208531313 ),
 .UNSPECIFIED. ) ;
#65284 = VERTEX_POINT ( 'NONE', #76743 ) ;
#65285 = CARTESIAN_POINT ( 'NONE',  ( -1.181102362204723644, -0.1870078740157479769, 0.4822834645669291653 ) ) ;
#65286 = CARTESIAN_POINT ( 'NONE',  ( -1.286089238845143479, -0.5023911411419708095, 0.1820866141732285504 ) ) ;
#65287 = CARTESIAN_POINT ( 'NONE',  ( -0.1246719160104980823, 0.2952755905511811885, 0.1292274648535926551 ) ) ;
#65288 = CARTESIAN_POINT ( 'NONE',  ( 0.3986795681651734702, 0.0008564280371857875508, -1.220472440944881720 ) ) ;
#65289 = CARTESIAN_POINT ( 'NONE',  ( -0.7152230971128602510, -0.3162353388693405765, 0.4822834645669290543 ) ) ;
#65290 = DIRECTION ( 'NONE',  ( 0.000000000000000000, 1.000000000000000000, 0.000000000000000000 ) ) ;
#65292 = CARTESIAN_POINT ( 'NONE',  ( 0.8464566929133865436, 0.1660481256975883668, -0.3530559997133364547 ) ) ;
#65291 = CARTESIAN_POINT ( 'NONE',  ( 1.082677165354331228, 0.1660481256975883391, -0.3530559997133364547 ) ) ;
#65293 = CARTESIAN_POINT ( 'NONE',  ( 1.404199475065617708, 0.05413385826771626580, -0.4176697321401330321 ) ) ;
#65294 = CARTESIAN_POINT ( 'NONE',  ( -0.1958661417322834220, -0.3392501089628018884, -2.419947506561679784 ) ) ;
#65295 = DIRECTION ( 'NONE',  ( 0.000000000000000000, 1.000000000000000000, -0.000000000000000000 ) ) ;
#65296 = CARTESIAN_POINT ( 'NONE',  ( -1.384514435695537005, 0.2952755905511811885, 0.1292274648535926551 ) ) ;
#65297 = B_SPLINE_CURVE_WITH_KNOTS ( 'NONE', 3,
 ( #13935, #76646, #25698, #7620 ),
 .UNSPECIFIED., .F., .F.,
 ( 4, 4 ),
 ( 0.05218731980467056220, 0.05362944292333609447 ),
 .UNSPECIFIED. ) ;
#65298 = CARTESIAN_POINT ( 'NONE',  ( -0.4091458600556405756, 0.2362204724409446288, -0.6561679790026246906 ) ) ;
#65299 = CARTESIAN_POINT ( 'NONE',  ( -0.2925321140481930704, -0.2925321140481933480, -0.2165354330708662012 ) ) ;
#65300 = ORIENTED_EDGE ( 'NONE', *, *, #14652, .T. ) ;
#65301 = CARTESIAN_POINT ( 'NONE',  ( -0.1574803149606292529, -0.1870078740157480601, -0.3641732283464567677 ) ) ;
#65302 = CARTESIAN_POINT ( 'NONE',  ( 0.3917322834645670104, 2.398668435337828261E-17, -2.000000000000000000 ) ) ;
#65303 = ORIENTED_EDGE ( 'NONE', *, *, #79432, .T. ) ;
#65304 = CARTESIAN_POINT ( 'NONE',  ( 0.07874015748031558404, -0.1870078740157480879, -0.4822834645669291653 ) ) ;
#65305 = CARTESIAN_POINT ( 'NONE',  ( -0.1443569553805768291, 0.05413385826771666132, 0.4176697321401328100 ) ) ;
#65306 = CARTESIAN_POINT ( 'NONE',  ( -0.6036745406824141069, -0.6046776061558809534, -0.2411417322834644161 ) ) ;
#65307 = DIRECTION ( 'NONE',  ( 1.000000000000000000, 0.000000000000000000, 0.000000000000000000 ) ) ;
#65308 = CARTESIAN_POINT ( 'NONE',  ( -0.7283464566929126471, -0.4536011799217367080, 0.2665933059059888421 ) ) ;
#65309 = CARTESIAN_POINT ( 'NONE',  ( -1.559171609364246924, 1.299212598425196985, 0.4177787735906735578 ) ) ;
#65310 = CARTESIAN_POINT ( 'NONE',  ( 0.9514435695538062676, -0.3162353388693409650, -0.4822834645669289433 ) ) ;
#65311 = CARTESIAN_POINT ( 'NONE',  ( 0.5839895013123367340, -0.5511811023622048555, -0.09757992244046775898 ) ) ;
#65312 = CARTESIAN_POINT ( 'NONE',  ( -0.4724409448818890911, -0.1870078740157480879, -0.4822834645669291653 ) ) ;
#65313 = CARTESIAN_POINT ( 'NONE',  ( -0.1958661417322836440, 0.3392501089628016664, -1.195518741960943210 ) ) ;
#65314 = CARTESIAN_POINT ( 'NONE',  ( -0.8005249343832011588, 0.05413385826771626580, -0.4176697321401330321 ) ) ;
#65315 = CARTESIAN_POINT ( 'NONE',  ( 0.000000000000000000, 2.755905511811024056, 0.000000000000000000 ) ) ;
#65316 = ADVANCED_FACE ( 'NONE', ( #77585 ), #57361, .T. ) ;
#65317 = CARTESIAN_POINT ( 'NONE',  ( 1.509186351706037543, 0.05413385826771666132, 0.4176697321401328100 ) ) ;
#65318 = CARTESIAN_POINT ( 'NONE',  ( -0.3129921259842521897, 1.496062992125984259, 0.4921259842519685179 ) ) ;
#65319 = ORIENTED_EDGE ( 'NONE', *, *, #46418, .F. ) ;
#65320 = CARTESIAN_POINT ( 'NONE',  ( 0.3917322834645670104, 0.1049643490035304660, -2.326134801346143366 ) ) ;
#65321 = CARTESIAN_POINT ( 'NONE',  ( -0.05249343832020911260, 0.2306618581243848609, 0.2411417322834645549 ) ) ;
#65322 = EDGE_LOOP ( 'NONE', ( #69685, #36127, #18007, #57619 ) ) ;
#65323 = CIRCLE ( 'NONE', #29013, 0.5120078740157480990 ) ;
#65324 = CARTESIAN_POINT ( 'NONE',  ( -0.8398950131233589023, -0.6046776061558809534, -0.2411417322834644161 ) ) ;
#65325 = CARTESIAN_POINT ( 'NONE',  ( 1.272965879265092637, 0.05413385826771666132, 0.4176697321401328100 ) ) ;
#65326 = CARTESIAN_POINT ( 'NONE',  ( 1.410761154855643795, -0.3162353388693405765, 0.4822834645669290543 ) ) ;
#65327 = CARTESIAN_POINT ( 'NONE',  ( 0.1640419947506569498, -0.05778040916215522460, 0.4822834645669289988 ) ) ;
#65328 = CARTESIAN_POINT ( 'NONE',  ( -0.1968503937007867743, 0.2952755905511811885, 0.000000000000000000 ) ) ;
#65329 = CARTESIAN_POINT ( 'NONE',  ( 0.3392501089628018884, -0.1958661417322834220, -1.921916010498687877 ) ) ;
#65330 = CARTESIAN_POINT ( 'NONE',  ( -1.397637795275589623, 0.1660481256975885056, 0.3530559997133364547 ) ) ;
#65331 = CARTESIAN_POINT ( 'NONE',  ( -0.2034120734908128059, 0.2952755905511811885, 0.1292274648535926551 ) ) ;
#65332 = CARTESIAN_POINT ( 'NONE',  ( -0.3215223097112853146, -0.08942795157528024563, -0.3641732283464568787 ) ) ;
#65333 = CARTESIAN_POINT ( 'NONE',  ( -1.603475055217291612, 0.7166759647713525361, -0.04573490813648263542 ) ) ;
#65334 = CARTESIAN_POINT ( 'NONE',  ( 1.358267716535433323, 0.1660481256975885056, 0.3530559997133364547 ) ) ;
#65335 = CARTESIAN_POINT ( 'NONE',  ( -0.6167979002624665030, 0.05413385826771666132, 0.4176697321401328100 ) ) ;
#65336 = CARTESIAN_POINT ( 'NONE',  ( 0.2952755905511819101, 0.1012011053420775880, -0.2882089793578256898 ) ) ;
#65337 = CARTESIAN_POINT ( 'NONE',  ( 1.174540682414699111, -0.05778040916215560624, -0.4822834645669293319 ) ) ;
#65338 = CARTESIAN_POINT ( 'NONE',  ( -0.3049517105654738214, -2.191421614605370878E-15, 0.4445507791589071167 ) ) ;
#65339 =( BOUNDED_SURFACE ( )  B_SPLINE_SURFACE ( 1, 2, ( 
 ( #18103, #76174, #70672, #58030, #63941, #76994, #37855, #76582, #5458, #44154, #44977, #82081, #82487, #13028, #5051, #12606, #83306, #18910, #44561, #6278, #38264, #12197, #82896, #64360, #30720, #69846, #31538, #31120, #56787, #70251, #57194, #23989, #50882, #31954, #6697, #19325, #24802, #49656, #25628, #56383, #24396, #50066, #75761, #43736, #51291, #69441, #11793, #20999, #59704, #64778, #8376, #26889, #1239, #393, #65635, #59291, #40358, #7965, #79097, #52128, #77837, #39520, #1648, #8787, #65208, #32787, #26051, #52548, #34041, #34460, #7545, #15111, #2059, #27305, #21416, #78257, #51710, #66451, #33627, #39096, #52964, #33218, #47070, #71097, #27723, #78678, #20166, #816, #71515, #26478, #66037, #39949, #77411, #46661, #53390, #58881, #72761, #19746, #72355, #20588, #14703, #45401, #40766, #13440, #7116, #58456, #45816, #13861, #46240, #71936, #14285, #41593, #22242, #61362, #53795, #28139, #74010, #67283, #54211, #10454, #79507, #2480, #21823, #3299, #60540, #29378, #28963, #60949, #47897, #73178, #4121, #80341, #2891, #47485, #36109, #79926, #61780, #15528, #54628, #28555, #34879, #9206, #67696, #41186, #60129, #74425, #66876, #73605, #9616, #15947, #35287, #22654, #48313, #16357, #35696, #42002, #10032, #42410, #3715, #55039, #80746, #23060, #48728, #16772, #68107, #20441, #33897, #9066, #77690, #34738, #66729, #46094, #1918, #60398, #2749, #59149, #71367, #71787, #20857, #15382, #51985, #8647, #21681, #65896, #21271, #33487, #46509, #73032, #26745, #27159, #41044, #33061, #40625, #2338, #46926, #72619, #34318, #66307, #40214, #27580, #20020, #45671, #72210, #14562, #7820, #1506, #8232, #13716, #59562, #53237, #39370, #65056, #78953, #14967, #7393, #59979, #27994, #53654, #79362, #58732, #47343, #1094, #52400, #78109, #14141, #39793, #65488, #52822, #78533, #26933, #21868, #15575, #72806, #41639, #40812, #41233, #8419, #60587, #67330, #79555, #27769, #47533, #1284, #8831, #2937, #53842, #66497, #66920, #52594, #8009, #15155, #21459, #59750, #14748, #73224, #78301, #20633, #34508, #2104, #46705, #47948, #46284, #71980, #14334, #47117, #1692, #9252, #60171, #79142, #40402, #39992, #33263, #2526, #27350, #65682, #73650, #21046, #15992, #33673, #28184, #78721, #59335, #53008, #34924, #72399, #58925, #66083, #34087, #53434, #28601, #79974, #54258, #22287, #62658, #23519, #62238, #74473, #61827, #30667, #67745, #68156, #82029, #74056, #81622, #43273, #4576, #30247, #49603, #23935, #81204, #68560, #56330, #60996, #4167, #29831, #48774, #16820, #49188, #18051, #74891, #17237, #50012, #24343, #55494, #55910, #48358, #42867, #10903, #36561, #68970, #3345, #75297, #17641, #43684, #4999, #75710, #9663, #29009, #55082, #80387, #11319, #36978, #35333, #54675, #16403, #22699, #42049, #10078, #35742, #23106, #61410, #42456, #3759, #29424, #80791, #10500, #36154, #82839, #44507, #57142, #25161, #19689, #25574, #51239, #5405, #31067, #56736, #12551, #45347, #77358, #6640, #70196, #6223, #50419, #76938, #71043, #20115, #82433, #24751, #76119, #5811, #12142, #13388, #7064, #31481, #70616, #38210, #50829, #63885, #76531, #31899, #39040, #32733, #18460, #44919, #11741, #44103, #18859, #57560, #83251, #19266, #12971, #69387, #38628, #37799, #64306, #26421, #37396, #52074, #760, #63476, #32312, #77781, #57975, #340, #25996, #63068, #69796, #51653, #64725, #58400, #79043, #2837, #54158, #52910, #65153, #39891, #14647, #9156, #79873, #2428, #15475, #59650, #15056, #27251, #40304, #66823, #20533, #20948, #34829, #26836, #34405, #79450, #40712, #66397, #28084, #60073, #33988, #21362, #60487, #13808, #65984, #8322, #1596, #78624, #2006, #45762, #27668, #53334, #28500, #71461, #47015, #8735, #1185, #72709, #53742, #21770, #47432, #39467, #73125, #41132, #7490, #33159, #58828, #52494, #78203, #7912, #46185, #71882, #14231, #65578, #33573, #59235, #46605, #72301, #54577, #48264, #35648, #49506, #61309, #23838, #17139, #73961, #42771, #75199, #3666, #80698, #9979, #29329, #55810, #61732, #4069, #41545, #67234, #9564, #48679, #81517, #30149, #68467, #23011, #42358 ),
 ( #54990, #16718, #41950, #68056, #17543, #68872, #28913, #81105, #47847, #80290, #74374, #10403, #36060, #29736, #55399, #56233, #35235, #43175, #23422, #30568, #49088, #11220, #60898, #36880, #74788, #10805, #36465, #22190, #62140, #4479, #62558, #4893, #73553, #15897, #3250, #22604, #16307, #67645, #24654, #43588, #57044, #25057, #31795, #19164, #57871, #62971, #6542, #50732, #82738, #81931, #63784, #57458, #38525, #6123, #77253, #50322, #76019, #37698, #83151, #6957, #63373, #30968, #24242, #76431, #32212, #32627, #5708, #13287, #237, #25471, #19582, #18759, #49915, #64620, #51137, #37296, #76832, #31379, #45242, #69289, #25889, #44814, #75613, #17951, #11636, #70510, #64208, #38108, #5309, #12868, #51549, #44403, #70942, #56635, #38939, #70095, #82336, #18361, #44005, #69698, #12042, #12449, #66294, #26312, #33046, #14548, #46495, #1492, #39779, #14953, #77678, #51970, #59549, #27145, #71773, #73018, #20008, #45659, #71355, #72191, #26733, #8633, #40200, #20843, #65473, #13701, #9049, #65883, #52387, #39357, #15369, #46080, #41030, #65041, #8219, #20427, #1080, #58715, #78934, #7378, #58290, #21257, #655, #66716, #78096, #33883, #7807, #21668, #14126, #2321, #1904, #33472, #59134, #52809, #46911, #40611, #27565, #78519, #53224, #34304, #72606, #27981, #59965, #53640, #79347, #47327, #2733, #11428, #5508, #56431, #67953, #43787, #28394, #9457, #74272, #22907, #61205, #16201, #75812, #54053, #79767, #37083, #3562, #48165, #50521, #22084, #47743, #73441, #48575, #3147, #69493, #16616, #80599, #41848, #15791, #69894, #42258, #28810, #41443, #76227, #22502, #18561, #67127, #62769, #80187, #60794, #35130, #82133, #54474, #34724, #24447, #60384, #44204, #73860, #56837, #5103, #67538, #30770, #37495, #9875, #31171, #50115, #18155, #54894, #35544, #11842, #63170, #29227, #82535, #24853, #46295, #71151, #78311, #5915, #25266, #38319, #57244, #70729, #38736, #45453, #32842, #71568, #76630, #20221, #64413, #13083, #12248, #77467, #13492, #52186, #19804, #7601, #63993, #6334, #51342, #39148, #20642, #77046, #44609, #37904, #6748, #45870, #63581, #19378, #26943, #13919, #64833, #33275, #32420, #31589, #82948, #7171, #45030, #50932, #32007, #58082, #58935, #18961, #77890, #65265, #26103, #58511, #448, #51765, #1293, #70305, #874, #52604, #12658, #26533, #39575, #57667, #29, #25682, #60597, #60183, #47543, #9673, #40003, #66507, #8841, #27780, #79152, #28193, #80397, #53851, #79564, #29020, #61006, #40822, #9263, #27358, #2535, #21879, #73233, #22296, #65691, #15584, #28611, #22710, #41649, #35344, #54686, #8019, #34096, #59344, #41243, #16002, #54268, #34934, #78732, #3355, #66930, #21055, #14756, #2114, #67340, #53443, #73661, #2946, #40411, #79983, #71990, #21468, #47126, #59759, #72816, #47957, #14343, #33682, #1701, #53017, #46715, #15166, #72407, #66092, #8428, #34517, #68568, #29434, #4583, #82036, #82441, #10089, #67755, #61420, #68166, #74483, #75718, #69396, #10509, #49609, #49197, #36162, #42875, #61836, #10910, #50019, #11748, #55093, #23942, #74067, #80801, #4177, #36568, #62246, #30254, #55918, #48368, #81631, #16830, #75304, #5414, #16413, #31075, #63076, #42466, #17648, #56743, #42060, #35754, #3770, #43280, #29840, #55504, #48786, #68979, #23118, #81212, #11327, #23527, #74898, #17246, #37404, #36987, #62666, #5006, #18058, #30676, #43691, #56337, #24350, #44929, #24758, #51664, #64316, #65165, #20125, #57570, #58838, #350, #7501, #18468, #37807, #50840, #69803, #83262, #51248, #57985, #45357, #770, #5819, #32744, #76950, #25584, #50426, #6650, #26007, #64736, #32323, #45772, #76540, #18868, #63895, #77368, #33170, #6233, #57151, #76126, #19277, #58411, #44111, #31909, #39478, #26432, #19700, #71471, #70626, #12151, #63485, #71054, #31490, #13398, #12982, #13819, #82850, #52083, #39051, #25171, #44517, #70204, #7074, #77792, #12562, #38220, #38638, #9166, #59661, #28511, #9574, #47442, #79056, #73136, #52504, #60085, #54168, #21780, #34417, #34838, #78213, #59246, #40723, #72720, #27681, #65995, #41143, #20545, #46197, #2439, #53346, #14659 ) ),
 .UNSPECIFIED., .F., .F., .F. ) 
 B_SPLINE_SURFACE_WITH_KNOTS ( ( 2, 2 ),
 ( 3, 2, 2, 2, 2, 2, 2, 2, 2, 2, 2, 2, 2, 2, 2, 2, 2, 2, 2, 2, 2, 2, 2, 2, 2, 2, 2, 2, 2, 2, 2, 2, 2, 2, 2, 2, 2, 2, 2, 2, 2, 2, 2, 2, 2, 2, 2, 2, 2, 2, 2, 2, 2, 2, 2, 2, 2, 2, 2, 2, 2, 2, 2, 2, 2, 2, 2, 2, 2, 2, 2, 2, 2, 2, 2, 2, 2, 2, 2, 2, 2, 2, 2, 2, 2, 2, 2, 2, 2, 2, 2, 2, 2, 2, 2, 2, 2, 2, 2, 2, 2, 2, 2, 2, 2, 2, 2, 2, 2, 2, 2, 2, 2, 2, 2, 2, 2, 2, 2, 2, 2, 2, 2, 2, 2, 2, 2, 2, 2, 2, 2, 2, 2, 2, 2, 2, 2, 2, 2, 2, 2, 2, 2, 2, 2, 2, 2, 2, 2, 2, 2, 2, 2, 2, 2, 2, 2, 2, 2, 2, 2, 2, 2, 2, 2, 2, 2, 2, 2, 2, 2, 2, 2, 2, 2, 2, 2, 2, 2, 2, 2, 2, 2, 2, 2, 2, 2, 2, 2, 2, 2, 2, 2, 2, 2, 2, 2, 2, 2, 2, 2, 2, 2, 2, 2, 2, 2, 2, 2, 2, 2, 2, 2, 2, 2, 2, 2, 2, 2, 2, 2, 2, 2, 2, 2, 2, 2, 2, 2, 2, 2, 2, 2, 2, 2, 2, 2, 2, 2, 2, 2, 2, 2, 2, 2, 2, 2, 2, 2, 2, 2, 2, 2, 2, 2, 3 ),
 ( 0.000000000000000000, 1.000000000000000000 ),
 ( 0.000000000000000000, 0.003787878787878787984, 0.007575757575757575968, 0.01136363636363636395, 0.01515151515151515194, 0.01893939393939393992, 0.02272727272727272790, 0.02651515151515151589, 0.03030303030303030387, 0.03409090909090908839, 0.03787878787878787984, 0.04166666666666666435, 0.04545454545454545581, 0.04924242424242424032, 0.05303030303030303177, 0.05681818181818181629, 0.06060606060606060774, 0.06439393939393939226, 0.06818181818181817677, 0.07196969696969697516, 0.07575757575757575968, 0.07954545454545454419, 0.08333333333333332871, 0.08712121212121212710, 0.09090909090909091161, 0.09469696969696969613, 0.09848484848484848064, 0.1022727272727272790, 0.1060606060606060635, 0.1098484848484848481, 0.1136363636363636326, 0.1174242424242424310, 0.1212121212121212155, 0.1250000000000000000, 0.1287878787878787845, 0.1325757575757575690, 0.1363636363636363535, 0.1401515151515151381, 0.1439393939393939503, 0.1477272727272727348, 0.1515151515151515194, 0.1553030303030303039, 0.1590909090909090884, 0.1628787878787878729, 0.1666666666666666574, 0.1704545454545454419, 0.1742424242424242542, 0.1780303030303030387, 0.1818181818181818232, 0.1856060606060606077, 0.1893939393939393923, 0.1931818181818181768, 0.1969696969696969613, 0.2007575757575757458, 0.2045454545454545581, 0.2083333333333333426, 0.2121212121212121271, 0.2159090909090909116, 0.2196969696969696961, 0.2234848484848484806, 0.2272727272727272652, 0.2310606060606060497, 0.2348484848484848619, 0.2386363636363636465, 0.2424242424242424310, 0.2462121212121212155, 0.2500000000000000000, 0.2537878787878787845, 0.2575757575757575690, 0.2613636363636363535, 0.2651515151515151381, 0.2689393939393939226, 0.2727272727272727071, 0.2765151515151514916, 0.2803030303030302761, 0.2840909090909091161, 0.2878787878787879007, 0.2916666666666666852, 0.2954545454545454697, 0.2992424242424242542, 0.3030303030303030387, 0.3068181818181818232, 0.3106060606060606077, 0.3143939393939393923, 0.3181818181818181768, 0.3219696969696969613, 0.3257575757575757458, 0.3295454545454545303, 0.3333333333333333148, 0.3371212121212120993, 0.3409090909090908839, 0.3446969696969697239, 0.3484848484848485084, 0.3522727272727272929, 0.3560606060606060774, 0.3598484848484848619, 0.3636363636363636465, 0.3674242424242424310, 0.3712121212121212155, 0.3750000000000000000, 0.3787878787878787845, 0.3825757575757575690, 0.3863636363636363535, 0.3901515151515151381, 0.3939393939393939226, 0.3977272727272727071, 0.4015151515151514916, 0.4053030303030302761, 0.4090909090909091161, 0.4128787878787879007, 0.4166666666666666852, 0.4204545454545454697, 0.4242424242424242542, 0.4280303030303030387, 0.4318181818181818232, 0.4356060606060606077, 0.4393939393939393923, 0.4431818181818181768, 0.4469696969696969613, 0.4507575757575757458, 0.4545454545454545303, 0.4583333333333333148, 0.4621212121212120993, 0.4659090909090908839, 0.4696969696969697239, 0.4734848484848485084, 0.4772727272727272929, 0.4810606060606060774, 0.4848484848484848619, 0.4886363636363636465, 0.4924242424242424310, 0.4962121212121212155, 0.5000000000000000000, 0.5037878787878787845, 0.5075757575757575690, 0.5113636363636363535, 0.5151515151515151381, 0.5189393939393939226, 0.5227272727272727071, 0.5265151515151514916, 0.5303030303030302761, 0.5340909090909090606, 0.5378787878787878451, 0.5416666666666666297, 0.5454545454545454142, 0.5492424242424241987, 0.5530303030303029832, 0.5568181818181817677, 0.5606060606060605522, 0.5643939393939394478, 0.5681818181818182323, 0.5719696969696970168, 0.5757575757575758013, 0.5795454545454545858, 0.5833333333333333703, 0.5871212121212121549, 0.5909090909090909394, 0.5946969696969697239, 0.5984848484848485084, 0.6022727272727272929, 0.6060606060606060774, 0.6098484848484848619, 0.6136363636363636465, 0.6174242424242424310, 0.6212121212121212155, 0.6250000000000000000, 0.6287878787878787845, 0.6325757575757575690, 0.6363636363636363535, 0.6401515151515151381, 0.6439393939393939226, 0.6477272727272727071, 0.6515151515151514916, 0.6553030303030302761, 0.6590909090909090606, 0.6628787878787878451, 0.6666666666666666297, 0.6704545454545454142, 0.6742424242424241987, 0.6780303030303029832, 0.6818181818181817677, 0.6856060606060605522, 0.6893939393939394478, 0.6931818181818182323, 0.6969696969696970168, 0.7007575757575758013, 0.7045454545454545858, 0.7083333333333333703, 0.7121212121212121549, 0.7159090909090909394, 0.7196969696969697239, 0.7234848484848485084, 0.7272727272727272929, 0.7310606060606060774, 0.7348484848484848619, 0.7386363636363636465, 0.7424242424242424310, 0.7462121212121212155, 0.7500000000000000000, 0.7537878787878787845, 0.7575757575757575690, 0.7613636363636363535, 0.7651515151515151381, 0.7689393939393939226, 0.7727272727272727071, 0.7765151515151514916, 0.7803030303030302761, 0.7840909090909090606, 0.7878787878787878451, 0.7916666666666666297, 0.7954545454545454142, 0.7992424242424241987, 0.8030303030303029832, 0.8068181818181817677, 0.8106060606060605522, 0.8143939393939394478, 0.8181818181818182323, 0.8219696969696970168, 0.8257575757575758013, 0.8295454545454545858, 0.8333333333333333703, 0.8371212121212121549, 0.8409090909090909394, 0.8446969696969697239, 0.8484848484848485084, 0.8522727272727272929, 0.8560606060606060774, 0.8598484848484848619, 0.8636363636363636465, 0.8674242424242424310, 0.8712121212121212155, 0.8750000000000000000, 0.8787878787878787845, 0.8825757575757575690, 0.8863636363636363535, 0.8901515151515151381, 0.8939393939393939226, 0.8977272727272727071, 0.9015151515151514916, 0.9053030303030302761, 0.9090909090909090606, 0.9128787878787878451, 0.9166666666666666297, 0.9204545454545454142, 0.9242424242424241987, 0.9280303030303029832, 0.9318181818181817677, 0.9356060606060605522, 0.9393939393939394478, 0.9431818181818182323, 0.9469696969696970168, 0.9507575757575758013, 0.9545454545454545858, 0.9583333333333333703, 0.9621212121212121549, 0.9659090909090909394 ),
 .UNSPECIFIED. ) 
 GEOMETRIC_REPRESENTATION_ITEM ( )  RATIONAL_B_SPLINE_SURFACE ( (
 ( 1.000000000000000000, 0.9659258262890683122, 1.000000000000000000, 0.9659258262890683122, 1.000000000000000000, 0.9659258262890683122, 1.000000000000000000, 0.9659258262890683122, 1.000000000000000000, 0.9659258262890683122, 1.000000000000000000, 0.9659258262890683122, 1.000000000000000000, 0.9659258262890683122, 1.000000000000000000, 0.9659258262890683122, 1.000000000000000000, 0.9659258262890683122, 1.000000000000000000, 0.9659258262890683122, 1.000000000000000000, 0.9659258262890683122, 1.000000000000000000, 0.9659258262890683122, 1.000000000000000000, 0.9659258262890683122, 1.000000000000000000, 0.9659258262890683122, 1.000000000000000000, 0.9659258262890683122, 1.000000000000000000, 0.9659258262890683122, 1.000000000000000000, 0.9659258262890683122, 1.000000000000000000, 0.9659258262890683122, 1.000000000000000000, 0.9659258262890683122, 1.000000000000000000, 0.9659258262890683122, 1.000000000000000000, 0.9659258262890683122, 1.000000000000000000, 0.9659258262890683122, 1.000000000000000000, 0.9659258262890683122, 1.000000000000000000, 0.9659258262890683122, 1.000000000000000000, 0.9659258262890683122, 1.000000000000000000, 0.9659258262890683122, 1.000000000000000000, 0.9659258262890683122, 1.000000000000000000, 0.9659258262890683122, 1.000000000000000000, 0.9659258262890683122, 1.000000000000000000, 0.9659258262890683122, 1.000000000000000000, 0.9659258262890683122, 1.000000000000000000, 0.9659258262890683122, 1.000000000000000000, 0.9659258262890683122, 1.000000000000000000, 0.9659258262890683122, 1.000000000000000000, 0.9659258262890683122, 1.000000000000000000, 0.9659258262890683122, 1.000000000000000000, 0.9659258262890683122, 1.000000000000000000, 0.9659258262890683122, 1.000000000000000000, 0.9659258262890683122, 1.000000000000000000, 0.9659258262890683122, 1.000000000000000000, 0.9659258262890683122, 1.000000000000000000, 0.9659258262890683122, 1.000000000000000000, 0.9659258262890683122, 1.000000000000000000, 0.9659258262890683122, 1.000000000000000000, 0.9659258262890683122, 1.000000000000000000, 0.9659258262890683122, 1.000000000000000000, 0.9659258262890683122, 1.000000000000000000, 0.9659258262890683122, 1.000000000000000000, 0.9659258262890683122, 1.000000000000000000, 0.9659258262890683122, 1.000000000000000000, 0.9659258262890683122, 1.000000000000000000, 0.9659258262890683122, 1.000000000000000000, 0.9659258262890683122, 1.000000000000000000, 0.9659258262890683122, 1.000000000000000000, 0.9659258262890683122, 1.000000000000000000, 0.9659258262890683122, 1.000000000000000000, 0.9659258262890683122, 1.000000000000000000, 0.9659258262890683122, 1.000000000000000000, 0.9659258262890683122, 1.000000000000000000, 0.9659258262890683122, 1.000000000000000000, 0.9659258262890683122, 1.000000000000000000, 0.9659258262890683122, 1.000000000000000000, 0.9659258262890683122, 1.000000000000000000, 0.9659258262890683122, 1.000000000000000000, 0.9659258262890683122, 1.000000000000000000, 0.9659258262890683122, 1.000000000000000000, 0.9659258262890683122, 1.000000000000000000, 0.9659258262890683122, 1.000000000000000000, 0.9659258262890683122, 1.000000000000000000, 0.9659258262890683122, 1.000000000000000000, 0.9659258262890683122, 1.000000000000000000, 0.9659258262890683122, 1.000000000000000000, 0.9659258262890683122, 1.000000000000000000, 0.9659258262890683122, 1.000000000000000000, 0.9659258262890683122, 1.000000000000000000, 0.9659258262890683122, 1.000000000000000000, 0.9659258262890683122, 1.000000000000000000, 0.9659258262890683122, 1.000000000000000000, 0.9659258262890683122, 1.000000000000000000, 0.9659258262890683122, 1.000000000000000000, 0.9659258262890683122, 1.000000000000000000, 0.9659258262890683122, 1.000000000000000000, 0.9659258262890683122, 1.000000000000000000, 0.9659258262890683122, 1.000000000000000000, 0.9659258262890683122, 1.000000000000000000, 0.9659258262890683122, 1.000000000000000000, 0.9659258262890683122, 1.000000000000000000, 0.9659258262890683122, 1.000000000000000000, 0.9659258262890683122, 1.000000000000000000, 0.9659258262890683122, 1.000000000000000000, 0.9659258262890683122, 1.000000000000000000, 0.9659258262890683122, 1.000000000000000000, 0.9659258262890683122, 1.000000000000000000, 0.9659258262890683122, 1.000000000000000000, 0.9659258262890683122, 1.000000000000000000, 0.9659258262890683122, 1.000000000000000000, 0.9659258262890683122, 1.000000000000000000, 0.9659258262890683122, 1.000000000000000000, 0.9659258262890683122, 1.000000000000000000, 0.9659258262890683122, 1.000000000000000000, 0.9659258262890683122, 1.000000000000000000, 0.9659258262890683122, 1.000000000000000000, 0.9659258262890683122, 1.000000000000000000, 0.9659258262890683122, 1.000000000000000000, 0.9659258262890683122, 1.000000000000000000, 0.9659258262890683122, 1.000000000000000000, 0.9659258262890683122, 1.000000000000000000, 0.9659258262890683122, 1.000000000000000000, 0.9659258262890683122, 1.000000000000000000, 0.9659258262890683122, 1.000000000000000000, 0.9659258262890683122, 1.000000000000000000, 0.9659258262890683122, 1.000000000000000000, 0.9659258262890683122, 1.000000000000000000, 0.9659258262890683122, 1.000000000000000000, 0.9659258262890683122, 1.000000000000000000, 0.9659258262890683122, 1.000000000000000000, 0.9659258262890683122, 1.000000000000000000, 0.9659258262890683122, 1.000000000000000000, 0.9659258262890683122, 1.000000000000000000, 0.9659258262890683122, 1.000000000000000000, 0.9659258262890683122, 1.000000000000000000, 0.9659258262890683122, 1.000000000000000000, 0.9659258262890683122, 1.000000000000000000, 0.9659258262890683122, 1.000000000000000000, 0.9659258262890683122, 1.000000000000000000, 0.9659258262890683122, 1.000000000000000000, 0.9659258262890683122, 1.000000000000000000, 0.9659258262890683122, 1.000000000000000000, 0.9659258262890683122, 1.000000000000000000, 0.9659258262890683122, 1.000000000000000000, 0.9659258262890683122, 1.000000000000000000, 0.9659258262890683122, 1.000000000000000000, 0.9659258262890683122, 1.000000000000000000, 0.9659258262890683122, 1.000000000000000000, 0.9659258262890683122, 1.000000000000000000, 0.9659258262890683122, 1.000000000000000000, 0.9659258262890683122, 1.000000000000000000, 0.9659258262890683122, 1.000000000000000000, 0.9659258262890683122, 1.000000000000000000, 0.9659258262890683122, 1.000000000000000000, 0.9659258262890683122, 1.000000000000000000, 0.9659258262890683122, 1.000000000000000000, 0.9659258262890683122, 1.000000000000000000, 0.9659258262890683122, 1.000000000000000000, 0.9659258262890683122, 1.000000000000000000, 0.9659258262890683122, 1.000000000000000000, 0.9659258262890683122, 1.000000000000000000, 0.9659258262890683122, 1.000000000000000000, 0.9659258262890683122, 1.000000000000000000, 0.9659258262890683122, 1.000000000000000000, 0.9659258262890683122, 1.000000000000000000, 0.9659258262890683122, 1.000000000000000000, 0.9659258262890683122, 1.000000000000000000, 0.9659258262890683122, 1.000000000000000000, 0.9659258262890683122, 1.000000000000000000, 0.9659258262890683122, 1.000000000000000000, 0.9659258262890683122, 1.000000000000000000, 0.9659258262890683122, 1.000000000000000000, 0.9659258262890683122, 1.000000000000000000, 0.9659258262890683122, 1.000000000000000000, 0.9659258262890683122, 1.000000000000000000, 0.9659258262890683122, 1.000000000000000000, 0.9659258262890683122, 1.000000000000000000, 0.9659258262890683122, 1.000000000000000000, 0.9659258262890683122, 1.000000000000000000, 0.9659258262890683122, 1.000000000000000000, 0.9659258262890683122, 1.000000000000000000, 0.9659258262890683122, 1.000000000000000000, 0.9659258262890683122, 1.000000000000000000, 0.9659258262890683122, 1.000000000000000000, 0.9659258262890683122, 1.000000000000000000, 0.9659258262890683122, 1.000000000000000000, 0.9659258262890683122, 1.000000000000000000, 0.9659258262890683122, 1.000000000000000000, 0.9659258262890683122, 1.000000000000000000, 0.9659258262890683122, 1.000000000000000000, 0.9659258262890683122, 1.000000000000000000, 0.9659258262890683122, 1.000000000000000000, 0.9659258262890683122, 1.000000000000000000, 0.9659258262890683122, 1.000000000000000000, 0.9659258262890683122, 1.000000000000000000, 0.9659258262890683122, 1.000000000000000000, 0.9659258262890683122, 1.000000000000000000, 0.9659258262890683122, 1.000000000000000000, 0.9659258262890683122, 1.000000000000000000, 0.9659258262890683122, 1.000000000000000000, 0.9659258262890683122, 1.000000000000000000, 0.9659258262890683122, 1.000000000000000000, 0.9659258262890683122, 1.000000000000000000, 0.9659258262890683122, 1.000000000000000000, 0.9659258262890683122, 1.000000000000000000, 0.9659258262890683122, 1.000000000000000000, 0.9659258262890683122, 1.000000000000000000, 0.9659258262890683122, 1.000000000000000000, 0.9659258262890683122, 1.000000000000000000, 0.9659258262890683122, 1.000000000000000000, 0.9659258262890683122, 1.000000000000000000, 0.9659258262890683122, 1.000000000000000000, 0.9659258262890683122, 1.000000000000000000, 0.9659258262890683122, 1.000000000000000000, 0.9659258262890683122, 1.000000000000000000, 0.9659258262890683122, 1.000000000000000000, 0.9659258262890683122, 1.000000000000000000, 0.9659258262890683122, 1.000000000000000000, 0.9659258262890683122, 1.000000000000000000, 0.9659258262890683122, 1.000000000000000000, 0.9659258262890683122, 1.000000000000000000, 0.9659258262890683122, 1.000000000000000000, 0.9659258262890683122, 1.000000000000000000, 0.9659258262890683122, 1.000000000000000000, 0.9659258262890683122, 1.000000000000000000, 0.9659258262890683122, 1.000000000000000000, 0.9659258262890683122, 1.000000000000000000, 0.9659258262890683122, 1.000000000000000000, 0.9659258262890683122, 1.000000000000000000, 0.9659258262890683122, 1.000000000000000000, 0.9659258262890683122, 1.000000000000000000, 0.9659258262890683122, 1.000000000000000000, 0.9659258262890683122, 1.000000000000000000, 0.9659258262890683122, 1.000000000000000000, 0.9659258262890683122, 1.000000000000000000, 0.9659258262890683122, 1.000000000000000000, 0.9659258262890683122, 1.000000000000000000, 0.9659258262890683122, 1.000000000000000000, 0.9659258262890683122, 1.000000000000000000, 0.9659258262890683122, 1.000000000000000000, 0.9659258262890683122, 1.000000000000000000, 0.9659258262890683122, 1.000000000000000000, 0.9659258262890683122, 1.000000000000000000, 0.9659258262890683122, 1.000000000000000000, 0.9659258262890683122, 1.000000000000000000, 0.9659258262890683122, 1.000000000000000000, 0.9659258262890683122, 1.000000000000000000, 0.9659258262890683122, 1.000000000000000000, 0.9659258262890683122, 1.000000000000000000, 0.9659258262890683122, 1.000000000000000000, 0.9659258262890683122, 1.000000000000000000, 0.9659258262890683122, 1.000000000000000000, 0.9659258262890683122, 1.000000000000000000, 0.9659258262890683122, 1.000000000000000000, 0.9659258262890683122, 1.000000000000000000, 0.9659258262890683122, 1.000000000000000000, 0.9659258262890683122, 1.000000000000000000, 0.9659258262890683122, 1.000000000000000000, 0.9659258262890683122, 1.000000000000000000, 0.9659258262890683122, 1.000000000000000000, 0.9659258262890683122, 1.000000000000000000, 0.9659258262890683122, 1.000000000000000000, 0.9659258262890683122, 1.000000000000000000, 0.9659258262890683122, 1.000000000000000000, 0.9659258262890683122, 1.000000000000000000, 0.9659258262890683122, 1.000000000000000000, 0.9659258262890683122, 1.000000000000000000, 0.9659258262890683122, 1.000000000000000000, 0.9659258262890683122, 1.000000000000000000),
 ( 1.000000000000000000, 0.9659258262890683122, 1.000000000000000000, 0.9659258262890683122, 1.000000000000000000, 0.9659258262890683122, 1.000000000000000000, 0.9659258262890683122, 1.000000000000000000, 0.9659258262890683122, 1.000000000000000000, 0.9659258262890683122, 1.000000000000000000, 0.9659258262890683122, 1.000000000000000000, 0.9659258262890683122, 1.000000000000000000, 0.9659258262890683122, 1.000000000000000000, 0.9659258262890683122, 1.000000000000000000, 0.9659258262890683122, 1.000000000000000000, 0.9659258262890683122, 1.000000000000000000, 0.9659258262890683122, 1.000000000000000000, 0.9659258262890683122, 1.000000000000000000, 0.9659258262890683122, 1.000000000000000000, 0.9659258262890683122, 1.000000000000000000, 0.9659258262890683122, 1.000000000000000000, 0.9659258262890683122, 1.000000000000000000, 0.9659258262890683122, 1.000000000000000000, 0.9659258262890683122, 1.000000000000000000, 0.9659258262890683122, 1.000000000000000000, 0.9659258262890683122, 1.000000000000000000, 0.9659258262890683122, 1.000000000000000000, 0.9659258262890683122, 1.000000000000000000, 0.9659258262890683122, 1.000000000000000000, 0.9659258262890683122, 1.000000000000000000, 0.9659258262890683122, 1.000000000000000000, 0.9659258262890683122, 1.000000000000000000, 0.9659258262890683122, 1.000000000000000000, 0.9659258262890683122, 1.000000000000000000, 0.9659258262890683122, 1.000000000000000000, 0.9659258262890683122, 1.000000000000000000, 0.9659258262890683122, 1.000000000000000000, 0.9659258262890683122, 1.000000000000000000, 0.9659258262890683122, 1.000000000000000000, 0.9659258262890683122, 1.000000000000000000, 0.9659258262890683122, 1.000000000000000000, 0.9659258262890683122, 1.000000000000000000, 0.9659258262890683122, 1.000000000000000000, 0.9659258262890683122, 1.000000000000000000, 0.9659258262890683122, 1.000000000000000000, 0.9659258262890683122, 1.000000000000000000, 0.9659258262890683122, 1.000000000000000000, 0.9659258262890683122, 1.000000000000000000, 0.9659258262890683122, 1.000000000000000000, 0.9659258262890683122, 1.000000000000000000, 0.9659258262890683122, 1.000000000000000000, 0.9659258262890683122, 1.000000000000000000, 0.9659258262890683122, 1.000000000000000000, 0.9659258262890683122, 1.000000000000000000, 0.9659258262890683122, 1.000000000000000000, 0.9659258262890683122, 1.000000000000000000, 0.9659258262890683122, 1.000000000000000000, 0.9659258262890683122, 1.000000000000000000, 0.9659258262890683122, 1.000000000000000000, 0.9659258262890683122, 1.000000000000000000, 0.9659258262890683122, 1.000000000000000000, 0.9659258262890683122, 1.000000000000000000, 0.9659258262890683122, 1.000000000000000000, 0.9659258262890683122, 1.000000000000000000, 0.9659258262890683122, 1.000000000000000000, 0.9659258262890683122, 1.000000000000000000, 0.9659258262890683122, 1.000000000000000000, 0.9659258262890683122, 1.000000000000000000, 0.9659258262890683122, 1.000000000000000000, 0.9659258262890683122, 1.000000000000000000, 0.9659258262890683122, 1.000000000000000000, 0.9659258262890683122, 1.000000000000000000, 0.9659258262890683122, 1.000000000000000000, 0.9659258262890683122, 1.000000000000000000, 0.9659258262890683122, 1.000000000000000000, 0.9659258262890683122, 1.000000000000000000, 0.9659258262890683122, 1.000000000000000000, 0.9659258262890683122, 1.000000000000000000, 0.9659258262890683122, 1.000000000000000000, 0.9659258262890683122, 1.000000000000000000, 0.9659258262890683122, 1.000000000000000000, 0.9659258262890683122, 1.000000000000000000, 0.9659258262890683122, 1.000000000000000000, 0.9659258262890683122, 1.000000000000000000, 0.9659258262890683122, 1.000000000000000000, 0.9659258262890683122, 1.000000000000000000, 0.9659258262890683122, 1.000000000000000000, 0.9659258262890683122, 1.000000000000000000, 0.9659258262890683122, 1.000000000000000000, 0.9659258262890683122, 1.000000000000000000, 0.9659258262890683122, 1.000000000000000000, 0.9659258262890683122, 1.000000000000000000, 0.9659258262890683122, 1.000000000000000000, 0.9659258262890683122, 1.000000000000000000, 0.9659258262890683122, 1.000000000000000000, 0.9659258262890683122, 1.000000000000000000, 0.9659258262890683122, 1.000000000000000000, 0.9659258262890683122, 1.000000000000000000, 0.9659258262890683122, 1.000000000000000000, 0.9659258262890683122, 1.000000000000000000, 0.9659258262890683122, 1.000000000000000000, 0.9659258262890683122, 1.000000000000000000, 0.9659258262890683122, 1.000000000000000000, 0.9659258262890683122, 1.000000000000000000, 0.9659258262890683122, 1.000000000000000000, 0.9659258262890683122, 1.000000000000000000, 0.9659258262890683122, 1.000000000000000000, 0.9659258262890683122, 1.000000000000000000, 0.9659258262890683122, 1.000000000000000000, 0.9659258262890683122, 1.000000000000000000, 0.9659258262890683122, 1.000000000000000000, 0.9659258262890683122, 1.000000000000000000, 0.9659258262890683122, 1.000000000000000000, 0.9659258262890683122, 1.000000000000000000, 0.9659258262890683122, 1.000000000000000000, 0.9659258262890683122, 1.000000000000000000, 0.9659258262890683122, 1.000000000000000000, 0.9659258262890683122, 1.000000000000000000, 0.9659258262890683122, 1.000000000000000000, 0.9659258262890683122, 1.000000000000000000, 0.9659258262890683122, 1.000000000000000000, 0.9659258262890683122, 1.000000000000000000, 0.9659258262890683122, 1.000000000000000000, 0.9659258262890683122, 1.000000000000000000, 0.9659258262890683122, 1.000000000000000000, 0.9659258262890683122, 1.000000000000000000, 0.9659258262890683122, 1.000000000000000000, 0.9659258262890683122, 1.000000000000000000, 0.9659258262890683122, 1.000000000000000000, 0.9659258262890683122, 1.000000000000000000, 0.9659258262890683122, 1.000000000000000000, 0.9659258262890683122, 1.000000000000000000, 0.9659258262890683122, 1.000000000000000000, 0.9659258262890683122, 1.000000000000000000, 0.9659258262890683122, 1.000000000000000000, 0.9659258262890683122, 1.000000000000000000, 0.9659258262890683122, 1.000000000000000000, 0.9659258262890683122, 1.000000000000000000, 0.9659258262890683122, 1.000000000000000000, 0.9659258262890683122, 1.000000000000000000, 0.9659258262890683122, 1.000000000000000000, 0.9659258262890683122, 1.000000000000000000, 0.9659258262890683122, 1.000000000000000000, 0.9659258262890683122, 1.000000000000000000, 0.9659258262890683122, 1.000000000000000000, 0.9659258262890683122, 1.000000000000000000, 0.9659258262890683122, 1.000000000000000000, 0.9659258262890683122, 1.000000000000000000, 0.9659258262890683122, 1.000000000000000000, 0.9659258262890683122, 1.000000000000000000, 0.9659258262890683122, 1.000000000000000000, 0.9659258262890683122, 1.000000000000000000, 0.9659258262890683122, 1.000000000000000000, 0.9659258262890683122, 1.000000000000000000, 0.9659258262890683122, 1.000000000000000000, 0.9659258262890683122, 1.000000000000000000, 0.9659258262890683122, 1.000000000000000000, 0.9659258262890683122, 1.000000000000000000, 0.9659258262890683122, 1.000000000000000000, 0.9659258262890683122, 1.000000000000000000, 0.9659258262890683122, 1.000000000000000000, 0.9659258262890683122, 1.000000000000000000, 0.9659258262890683122, 1.000000000000000000, 0.9659258262890683122, 1.000000000000000000, 0.9659258262890683122, 1.000000000000000000, 0.9659258262890683122, 1.000000000000000000, 0.9659258262890683122, 1.000000000000000000, 0.9659258262890683122, 1.000000000000000000, 0.9659258262890683122, 1.000000000000000000, 0.9659258262890683122, 1.000000000000000000, 0.9659258262890683122, 1.000000000000000000, 0.9659258262890683122, 1.000000000000000000, 0.9659258262890683122, 1.000000000000000000, 0.9659258262890683122, 1.000000000000000000, 0.9659258262890683122, 1.000000000000000000, 0.9659258262890683122, 1.000000000000000000, 0.9659258262890683122, 1.000000000000000000, 0.9659258262890683122, 1.000000000000000000, 0.9659258262890683122, 1.000000000000000000, 0.9659258262890683122, 1.000000000000000000, 0.9659258262890683122, 1.000000000000000000, 0.9659258262890683122, 1.000000000000000000, 0.9659258262890683122, 1.000000000000000000, 0.9659258262890683122, 1.000000000000000000, 0.9659258262890683122, 1.000000000000000000, 0.9659258262890683122, 1.000000000000000000, 0.9659258262890683122, 1.000000000000000000, 0.9659258262890683122, 1.000000000000000000, 0.9659258262890683122, 1.000000000000000000, 0.9659258262890683122, 1.000000000000000000, 0.9659258262890683122, 1.000000000000000000, 0.9659258262890683122, 1.000000000000000000, 0.9659258262890683122, 1.000000000000000000, 0.9659258262890683122, 1.000000000000000000, 0.9659258262890683122, 1.000000000000000000, 0.9659258262890683122, 1.000000000000000000, 0.9659258262890683122, 1.000000000000000000, 0.9659258262890683122, 1.000000000000000000, 0.9659258262890683122, 1.000000000000000000, 0.9659258262890683122, 1.000000000000000000, 0.9659258262890683122, 1.000000000000000000, 0.9659258262890683122, 1.000000000000000000, 0.9659258262890683122, 1.000000000000000000, 0.9659258262890683122, 1.000000000000000000, 0.9659258262890683122, 1.000000000000000000, 0.9659258262890683122, 1.000000000000000000, 0.9659258262890683122, 1.000000000000000000, 0.9659258262890683122, 1.000000000000000000, 0.9659258262890683122, 1.000000000000000000, 0.9659258262890683122, 1.000000000000000000, 0.9659258262890683122, 1.000000000000000000, 0.9659258262890683122, 1.000000000000000000, 0.9659258262890683122, 1.000000000000000000, 0.9659258262890683122, 1.000000000000000000, 0.9659258262890683122, 1.000000000000000000, 0.9659258262890683122, 1.000000000000000000, 0.9659258262890683122, 1.000000000000000000, 0.9659258262890683122, 1.000000000000000000, 0.9659258262890683122, 1.000000000000000000, 0.9659258262890683122, 1.000000000000000000, 0.9659258262890683122, 1.000000000000000000, 0.9659258262890683122, 1.000000000000000000, 0.9659258262890683122, 1.000000000000000000, 0.9659258262890683122, 1.000000000000000000, 0.9659258262890683122, 1.000000000000000000, 0.9659258262890683122, 1.000000000000000000, 0.9659258262890683122, 1.000000000000000000, 0.9659258262890683122, 1.000000000000000000, 0.9659258262890683122, 1.000000000000000000, 0.9659258262890683122, 1.000000000000000000, 0.9659258262890683122, 1.000000000000000000, 0.9659258262890683122, 1.000000000000000000, 0.9659258262890683122, 1.000000000000000000, 0.9659258262890683122, 1.000000000000000000, 0.9659258262890683122, 1.000000000000000000, 0.9659258262890683122, 1.000000000000000000, 0.9659258262890683122, 1.000000000000000000, 0.9659258262890683122, 1.000000000000000000, 0.9659258262890683122, 1.000000000000000000, 0.9659258262890683122, 1.000000000000000000, 0.9659258262890683122, 1.000000000000000000, 0.9659258262890683122, 1.000000000000000000, 0.9659258262890683122, 1.000000000000000000, 0.9659258262890683122, 1.000000000000000000, 0.9659258262890683122, 1.000000000000000000, 0.9659258262890683122, 1.000000000000000000, 0.9659258262890683122, 1.000000000000000000, 0.9659258262890683122, 1.000000000000000000, 0.9659258262890683122, 1.000000000000000000, 0.9659258262890683122, 1.000000000000000000, 0.9659258262890683122, 1.000000000000000000, 0.9659258262890683122, 1.000000000000000000, 0.9659258262890683122, 1.000000000000000000, 0.9659258262890683122, 1.000000000000000000, 0.9659258262890683122, 1.000000000000000000, 0.9659258262890683122, 1.000000000000000000, 0.9659258262890683122, 1.000000000000000000, 0.9659258262890683122, 1.000000000000000000, 0.9659258262890683122, 1.000000000000000000) ) ) 
 REPRESENTATION_ITEM ( '' )  SURFACE ( )  );
#65340 = ORIENTED_EDGE ( 'NONE', *, *, #22702, .F. ) ;
#65341 = CARTESIAN_POINT ( 'NONE',  ( -0.01968503937007793844, 0.1660481256975883668, -0.3530559997133364547 ) ) ;
#65342 = CARTESIAN_POINT ( 'NONE',  ( -0.2493438320209966919, -0.004921259842519870586, -0.3153832671262229437 ) ) ;
#65344 = CARTESIAN_POINT ( 'NONE',  ( -1.603475055217291612, 0.7793870273546337213, -0.04573490813648262154 ) ) ;
#65343 = CARTESIAN_POINT ( 'NONE',  ( 1.010498687664042716, -0.3690944881889763329, 0.3153832671262228327 ) ) ;
#65345 = CARTESIAN_POINT ( 'NONE',  ( 0.2362204724409449064, 0.4091458600556404646, -0.3786089238845143923 ) ) ;
#65346 = CARTESIAN_POINT ( 'NONE',  ( 1.692913385826772421, 0.1771653543307087630, 0.000000000000000000 ) ) ;
#65347 = CARTESIAN_POINT ( 'NONE',  ( 1.036745406824147508, -0.4281496062992127816, -0.4176697321401328100 ) ) ;
#65348 = CARTESIAN_POINT ( 'NONE',  ( -0.3949938075777409963, -7.255918531996591613E-17, -0.1161417322834646104 ) ) ;
#65349 = CARTESIAN_POINT ( 'NONE',  ( 0.01312335958005323398, 0.05413385826771666132, 0.4176697321401328100 ) ) ;
#65350 = FACE_OUTER_BOUND ( 'NONE', #3304, .T. ) ;
#65351 = CARTESIAN_POINT ( 'NONE',  ( -1.404199475065615932, 0.05413385826771666132, 0.4176697321401328100 ) ) ;
#65352 = CARTESIAN_POINT ( 'NONE',  ( -0.1181102362204717315, 0.2952755905511811885, 0.000000000000000000 ) ) ;
#65353 = CARTESIAN_POINT ( 'NONE',  ( 0.2891555358219910499, 0.2891555358219910499, 0.1003937007874015630 ) ) ;
#65354 = CARTESIAN_POINT ( 'NONE',  ( 1.627296587926509996, -0.6046776061558807314, 0.2411417322834647770 ) ) ;
#65355 = CARTESIAN_POINT ( 'NONE',  ( 0.5446194225721792126, -0.05778040916215560624, -0.4822834645669293319 ) ) ;
#65356 = CARTESIAN_POINT ( 'NONE',  ( 1.154855643044620184, -0.5023911411419708095, 0.1820866141732285504 ) ) ;
#65357 = CARTESIAN_POINT ( 'NONE',  ( 0.3123753919909370014, 1.356452634660756384, 0.02004157963777108628 ) ) ;
#65358 = CARTESIAN_POINT ( 'NONE',  ( 0.2230971128608932319, -0.3690944881889763329, 0.3153832671262228327 ) ) ;
#65359 = CARTESIAN_POINT ( 'NONE',  ( -1.351706036745406347, -0.4281496062992124485, 0.4176697321401328655 ) ) ;
#65360 = CARTESIAN_POINT ( 'NONE',  ( -0.2925321140481930149, -0.2925321140481933480, -0.9232283464566929387 ) ) ;
#65361 = CARTESIAN_POINT ( 'NONE',  ( 0.9908136482939640111, -0.6692913385826771977, 0.1292274648535927661 ) ) ;
#65362 = CONICAL_SURFACE ( 'NONE', #46517, 1.220472440944883497, 0.7853981633974691512 ) ;
#65363 = CARTESIAN_POINT ( 'NONE',  ( -0.3392501089628019995, 0.1958661417322832277, -0.8057742782152230721 ) ) ;
#65364 = AXIS2_PLACEMENT_3D ( 'NONE', #71050, #59242, #21369 ) ;
#65365 = AXIS2_PLACEMENT_3D ( 'NONE', #43070, #51031, #62444 ) ;
#65367 = DIRECTION ( 'NONE',  ( 0.000000000000000000, 0.000000000000000000, 1.000000000000000000 ) ) ;
#65366 = CARTESIAN_POINT ( 'NONE',  ( 0.7152230971128616943, -0.05778040916215522460, 0.4822834645669289988 ) ) ;
#65368 = CYLINDRICAL_SURFACE ( 'NONE', #44613, 0.09842519685039351207 ) ;
#65369 = CARTESIAN_POINT ( 'NONE',  ( 0.4199475065616803948, -0.5023911411419708095, -0.1820866141732282451 ) ) ;
#65370 = CARTESIAN_POINT ( 'NONE',  ( 0.7217847769028878924, 0.05413385826771666132, 0.4176697321401328100 ) ) ;
#65371 = CARTESIAN_POINT ( 'NONE',  ( -0.2140388612101736809, 0.2035438835850314210, 0.1320934087364890874 ) ) ;
#65372 = CARTESIAN_POINT ( 'NONE',  ( -1.141732283464566011, -0.5511811023622047445, 6.969142054262312111E-17 ) ) ;
#65373 = CARTESIAN_POINT ( 'NONE',  ( -1.122047244094487306, -0.5400638737290844871, 0.3530559997133364547 ) ) ;
#65374 = CARTESIAN_POINT ( 'NONE',  ( -1.358267716535432434, 0.1660481256975883668, -0.3530559997133364547 ) ) ;
#65375 = CARTESIAN_POINT ( 'NONE',  ( 0.9776902887139113929, -0.6692913385826773087, -0.1292274648535924053 ) ) ;
#65376 = CARTESIAN_POINT ( 'NONE',  ( 1.476377952755906442, -0.5400638737290844871, 0.3530559997133364547 ) ) ;
#65377 = CARTESIAN_POINT ( 'NONE',  ( 1.016821367227983774, 1.537401574803149984, -0.4744094488188970171 ) ) ;
#65378 = CARTESIAN_POINT ( 'NONE',  ( 0.5380577427821529035, 0.05413385826771626580, -0.4176697321401330321 ) ) ;
#65379 = CARTESIAN_POINT ( 'NONE',  ( 0.1265901696524990294, -0.4724409448818896462, -2.839238845144356649 ) ) ;
#65380 = CARTESIAN_POINT ( 'NONE',  ( 0.1229937836670168122, 1.078949693266341603, 3.935114318630247077 ) ) ;
#65381 = CARTESIAN_POINT ( 'NONE',  ( 1.410761154855643795, -0.05778040916215560624, -0.4822834645669293319 ) ) ;
#65382 = CARTESIAN_POINT ( 'NONE',  ( -1.371391076115484831, 0.1771653543307087075, -0.09757992244046823083 ) ) ;
#65383 = CARTESIAN_POINT ( 'NONE',  ( 1.423884514435696413, -0.2845877964562161244, -0.3641732283464567121 ) ) ;
#65384 = CARTESIAN_POINT ( 'NONE',  ( -1.220472440944881054, -0.5511811023622047445, 6.969142054262312111E-17 ) ) ;
#65385 = CARTESIAN_POINT ( 'NONE',  ( -0.3215223097112853146, -0.08942795157528024563, -0.3641732283464568787 ) ) ;
#65386 = CARTESIAN_POINT ( 'NONE',  ( -0.4724409448818882584, 0.1265901696525017217, -2.080052493438319772 ) ) ;
#65387 = CARTESIAN_POINT ( 'NONE',  ( 0.9448818897637802916, -0.1870078740157479769, 0.3641732283464567677 ) ) ;
#65388 = CARTESIAN_POINT ( 'NONE',  ( 0.5314960629921267055, -0.5400638737290844871, 0.3530559997133364547 ) ) ;
#65389 = CARTESIAN_POINT ( 'NONE',  ( 1.148293963254593653, 0.2952755905511810774, -0.1292274648535930714 ) ) ;
#65390 = CARTESIAN_POINT ( 'NONE',  ( 0.1509186351706045259, -0.05778040916215560624, -0.4822834645669293319 ) ) ;
#65391 = CARTESIAN_POINT ( 'NONE',  ( 0.4986876640419954376, 0.1283753931104748280, 0.1820866141732283561 ) ) ;
#65392 = B_SPLINE_CURVE_WITH_KNOTS ( 'NONE', 3,
 ( #58257, #12010, #5677, #34270, #73409, #46464, #14093 ),
 .UNSPECIFIED., .F., .F.,
 ( 4, 3, 4 ),
 ( 1.561251128379126385E-17, 0.001246230184515555693, 0.002492489877932649398 ),
 .UNSPECIFIED. ) ;
#65393 = CARTESIAN_POINT ( 'NONE',  ( 1.069553805774278610, -0.6692913385826771977, 0.1292274648535927661 ) ) ;
#65394 = CARTESIAN_POINT ( 'NONE',  ( -1.535433070866141225, -0.6692913385826771977, 8.415575281601705876E-17 ) ) ;
#65395 = CARTESIAN_POINT ( 'NONE',  ( -0.6758530183727028406, -0.6692913385826773087, -0.1292274648535924053 ) ) ;
#65396 = CARTESIAN_POINT ( 'NONE',  ( 0.3996062992125985480, 0.1070741851644054637, -0.5971128608923884640 ) ) ;
#65397 = CARTESIAN_POINT ( 'NONE',  ( 0.05905511811023680946, 0.1012011053420775880, -0.2882089793578257453 ) ) ;
#65398 = CARTESIAN_POINT ( 'NONE',  ( 0.1246719160104994284, -0.6692913385826771977, 0.1292274648535927661 ) ) ;
#65399 = CARTESIAN_POINT ( 'NONE',  ( -0.1902887139107604098, 0.2952755905511810774, -0.1292274648535930714 ) ) ;
#65400 = CARTESIAN_POINT ( 'NONE',  ( 0.1246719160104994284, -0.6692913385826771977, 0.1292274648535927661 ) ) ;
#65401 = CARTESIAN_POINT ( 'NONE',  ( 0.2925321140481932369, 0.2925321140481932369, -2.814960629921259727 ) ) ;
#65402 = CARTESIAN_POINT ( 'NONE',  ( 0.1974969037888704704, 0.3420746716998660508, -1.719160104986876769 ) ) ;
#65403 = CARTESIAN_POINT ( 'NONE',  ( 0.3917322834645670104, 2.398668435337828261E-17, -0.4251968503937007537 ) ) ;
#65404 = CARTESIAN_POINT ( 'NONE',  ( 0.3917322834645670104, 2.398668435337828261E-17, -1.212598425196850238 ) ) ;
#65405 = CARTESIAN_POINT ( 'NONE',  ( -0.9908136482939626788, -0.5511811023622048555, -0.09757992244046775898 ) ) ;
#65406 = CARTESIAN_POINT ( 'NONE',  ( 4.797336870675656522E-17, -0.3917322834645670104, -1.173228346456692828 ) ) ;
#65407 = CARTESIAN_POINT ( 'NONE',  ( -1.108923884514435132, -0.3162353388693405765, 0.4822834645669290543 ) ) ;
#65408 = CARTESIAN_POINT ( 'NONE',  ( -0.3392501089628018329, -0.1958661417322836440, 0.1824340139445687625 ) ) ;
#65409 = CARTESIAN_POINT ( 'NONE',  ( 0.4002624671916016896, -0.05778040916215522460, 0.4822834645669289988 ) ) ;
#65410 = CARTESIAN_POINT ( 'NONE',  ( -0.6364829396325453192, -0.2845877964562159024, 0.3641732283464567677 ) ) ;
#65412 = EDGE_CURVE ( 'NONE', #82979, #44891, #82854, .T. ) ;
#65411 = CARTESIAN_POINT ( 'NONE',  ( 1.404199475065617264, -0.4281496062992124485, 0.4176697321401328655 ) ) ;
#65413 = CARTESIAN_POINT ( 'NONE',  ( 0.3674540682414705883, 0.2306618581243847221, -0.2411417322834647770 ) ) ;
#65414 = CARTESIAN_POINT ( 'NONE',  ( 0.4437891188668303677, 1.369016496689889895, 1.030574033111541166 ) ) ;
#65415 = AXIS2_PLACEMENT_3D ( 'NONE', #9022, #78068, #34695 ) ;
#65416 = CARTESIAN_POINT ( 'NONE',  ( -0.1998031496062994683, 0.3460692066303958092, -2.690288713910760965 ) ) ;
#65417 = CARTESIAN_POINT ( 'NONE',  ( -0.1958661417322836995, 0.3392501089628017219, -1.269704355151917818 ) ) ;
#65418 = CARTESIAN_POINT ( 'NONE',  ( 1.259842519685040019, -0.1870078740157480879, -0.4822834645669291653 ) ) ;
#65419 = CIRCLE ( 'NONE', #29118, 0.009842519685039378616 ) ;
#65420 = AXIS2_PLACEMENT_3D ( 'NONE', #21235, #77657, #45222 ) ;
#65421 = CARTESIAN_POINT ( 'NONE',  ( 0.2821522309711292364, -0.6692913385826771977, 0.1292274648535927661 ) ) ;
#65422 = CARTESIAN_POINT ( 'NONE',  ( 0.3740157480314966754, 0.1660481256975883668, -0.3530559997133364547 ) ) ;
#65423 = CARTESIAN_POINT ( 'NONE',  ( 1.522309711286089939, -0.6046776061558809534, -0.2411417322834644161 ) ) ;
#65424 = CARTESIAN_POINT ( 'NONE',  ( 0.8136482939632553313, -0.6046776061558809534, -0.2411417322834644161 ) ) ;
#65425 = APPLICATION_CONTEXT ( 'automotive_design' ) ;
#65426 = CARTESIAN_POINT ( 'NONE',  ( -0.3392501089628019995, 0.1958661417322832277, -0.7408136482939633449 ) ) ;
#65427 = CARTESIAN_POINT ( 'NONE',  ( -0.1377952755905504645, 0.1660481256975885056, 0.3530559997133364547 ) ) ;
#65428 = CARTESIAN_POINT ( 'NONE',  ( 1.030183727034121421, -0.05778040916215522460, 0.4822834645669289988 ) ) ;
#65429 = CARTESIAN_POINT ( 'NONE',  ( 0.5971128608923891301, 0.2952755905511810774, -0.1292274648535930714 ) ) ;
#65430 = CARTESIAN_POINT ( 'NONE',  ( 1.076115485564305141, 0.1283753931104746893, -0.1820866141732285504 ) ) ;
#65431 = CARTESIAN_POINT ( 'NONE',  ( -0.7480314960629914633, 0.2952755905511811885, 0.000000000000000000 ) ) ;
#65432 = CARTESIAN_POINT ( 'NONE',  ( -1.358267716535432434, 0.1660481256975883668, -0.3530559997133364547 ) ) ;
#65433 = CARTESIAN_POINT ( 'NONE',  ( 0.9055118110236227702, -0.6692913385826771977, 8.415575281601705876E-17 ) ) ;
#65434 = CARTESIAN_POINT ( 'NONE',  ( 0.4724409448818898682, 2.892866454678787531E-17, -0.5098425196850393526 ) ) ;
#65435 = CARTESIAN_POINT ( 'NONE',  ( -0.1958661417322834220, -0.3392501089628018884, -2.104986876640420057 ) ) ;
#65436 = ORIENTED_EDGE ( 'NONE', *, *, #58210, .T. ) ;
#65437 = CARTESIAN_POINT ( 'NONE',  ( 0.3460692066303959757, -0.1998031496062991907, -0.5774278215223097588 ) ) ;
#65438 = ORIENTED_EDGE ( 'NONE', *, *, #56216, .F. ) ;
#65439 = CARTESIAN_POINT ( 'NONE',  ( 1.338582677165355062, -0.1870078740157479769, 0.4822834645669291653 ) ) ;
#65440 = CARTESIAN_POINT ( 'NONE',  ( 0.7874015748031503170, -0.1870078740157479769, 0.3641732283464567677 ) ) ;
#65441 = CARTESIAN_POINT ( 'NONE',  ( 0.5971128608923891301, 0.2952755905511810219, -0.1292274648535930437 ) ) ;
#65442 = CARTESIAN_POINT ( 'NONE',  ( -0.08874907683609993547, 8.471767977567108961E-16, -0.4445507791589058955 ) ) ;
#65443 = CARTESIAN_POINT ( 'NONE',  ( 1.968503937007874072, 0.000000000000000000, 5.879133660591329580 ) ) ;
#65444 = CARTESIAN_POINT ( 'NONE',  ( -0.1049643490035307020, 0.3917322834645669549, -0.8786089238845143923 ) ) ;
#65445 = CARTESIAN_POINT ( 'NONE',  ( 1.122047244094488860, 0.1660481256975885056, 0.3530559997133364547 ) ) ;
#65446 = DIRECTION ( 'NONE',  ( 0.000000000000000000, 0.000000000000000000, -1.000000000000000000 ) ) ;
#65447 = CARTESIAN_POINT ( 'NONE',  ( -0.4396325459317579898, 0.2952755905511811885, 0.1292274648535926551 ) ) ;
#65448 = CARTESIAN_POINT ( 'NONE',  ( 1.272965879265092637, 0.05413385826771666132, 0.4176697321401328100 ) ) ;
#65449 = ORIENTED_EDGE ( 'NONE', *, *, #19008, .T. ) ;
#65450 = EDGE_CURVE ( 'NONE', #39649, #48388, #19637, .T. ) ;
#65451 = CARTESIAN_POINT ( 'NONE',  ( -1.673228346456691717, 0.1660481256975883668, -0.3530559997133364547 ) ) ;
#65452 = CARTESIAN_POINT ( 'NONE',  ( 0.3492006680983059663, 0.3045572308828553565, -0.01849200668098333403 ) ) ;
#65453 = DIRECTION ( 'NONE',  ( 0.000000000000000000, 0.000000000000000000, 1.000000000000000000 ) ) ;
#65454 = CARTESIAN_POINT ( 'NONE',  ( 1.614173228346456712, 1.496062992125984037, -0.1372047244094476703 ) ) ;
#65455 = CARTESIAN_POINT ( 'NONE',  ( -0.9645669291338575535, 0.07958543189024071263, -0.2665933059059888421 ) ) ;
#65456 = CARTESIAN_POINT ( 'NONE',  ( 0.9120734908136490793, 0.2066929133858267098, -0.1054918080437494132 ) ) ;
#65457 = CARTESIAN_POINT ( 'NONE',  ( 0.6889763779527566800, -0.5400638737290844871, 0.3530559997133364547 ) ) ;
#65458 = VERTEX_POINT ( 'NONE', #45984 ) ;
#65460 = CARTESIAN_POINT ( 'NONE',  ( 0.3503937007874015630, -0.3733313776025731778, -0.01968503937007957602 ) ) ;
#65459 = CARTESIAN_POINT ( 'NONE',  ( -1.614173228346456712, 2.401574803149606474, 0.1372047244094477536 ) ) ;
#65461 = CARTESIAN_POINT ( 'NONE',  ( 0.8792650918635177559, 0.05413385826771666132, 0.4176697321401328100 ) ) ;
#65462 = CARTESIAN_POINT ( 'NONE',  ( -1.509186351706035767, 0.05413385826771626580, -0.4176697321401330321 ) ) ;
#65463 = CARTESIAN_POINT ( 'NONE',  ( 0.1958661417322836162, -0.3392501089628018329, -0.9592982695199985255 ) ) ;
#65464 = CARTESIAN_POINT ( 'NONE',  ( -0.8923884514435688198, 0.1283753931104746893, -0.1820866141732285504 ) ) ;
#65465 = CARTESIAN_POINT ( 'NONE',  ( 1.686351706036745890, 0.2952755905511811885, 0.1292274648535926551 ) ) ;
#65466 = CARTESIAN_POINT ( 'NONE',  ( 0.1049643490035304799, -0.3917322834645669549, -1.114829396325459410 ) ) ;
#65467 = CARTESIAN_POINT ( 'NONE',  ( 0.2755905511811031494, -0.6692913385826771977, 8.415575281601705876E-17 ) ) ;
#65468 = CARTESIAN_POINT ( 'NONE',  ( -0.9711286089238838626, 0.1283753931104746893, -0.1820866141732285504 ) ) ;
#65469 = CARTESIAN_POINT ( 'NONE',  ( 0.1902887139107617975, 0.1771653543307087630, 0.09757992244046791164 ) ) ;
#65470 = CARTESIAN_POINT ( 'NONE',  ( -0.4527559055118102749, 0.1660481256975885056, 0.3530559997133364547 ) ) ;
#65471 = CARTESIAN_POINT ( 'NONE',  ( -1.299212598425196097, 0.1771653543307087630, 0.000000000000000000 ) ) ;
#65472 = CARTESIAN_POINT ( 'NONE',  ( -0.2867679344610365444, -0.2867679344610367664, -0.2132739089576921876 ) ) ;
#65473 = CARTESIAN_POINT ( 'NONE',  ( 0.8005249343832027131, 0.05413385826771666132, 0.4176697321401328100 ) ) ;
#65474 = EDGE_CURVE ( 'NONE', #49008, #16433, #11869, .T. ) ;
#65475 = CARTESIAN_POINT ( 'NONE',  ( -1.338582677165353729, -0.1870078740157479769, 0.4822834645669291653 ) ) ;
#65476 = VECTOR ( 'NONE', #2694, 39.37007874015748143 ) ;
#65477 = CARTESIAN_POINT ( 'NONE',  ( 0.2362204724409451007, -0.4091458600556402980, -1.428477690288713964 ) ) ;
#65478 = CARTESIAN_POINT ( 'NONE',  ( -0.6692913385826764205, -0.6692913385826771977, 8.415575281601705876E-17 ) ) ;
#65479 = CARTESIAN_POINT ( 'NONE',  ( -0.2952755905511804668, 0.07958543189024085140, 0.2665933059059887866 ) ) ;
#65480 = CARTESIAN_POINT ( 'NONE',  ( -1.227034120734907141, -0.6692913385826773087, -0.1292274648535924053 ) ) ;
#65481 = CARTESIAN_POINT ( 'NONE',  ( 0.8989501312335964611, 0.1771653543307087630, 0.09757992244046791164 ) ) ;
#65482 = CARTESIAN_POINT ( 'NONE',  ( -0.4265091863517051496, 0.1771653543307087075, -0.09757992244046823083 ) ) ;
#65483 = CARTESIAN_POINT ( 'NONE',  ( -1.187664041994750175, -0.05778040916215560624, -0.4822834645669293319 ) ) ;
#65484 = CARTESIAN_POINT ( 'NONE',  ( -0.9711286089238838626, -0.6046776061558807314, 0.2411417322834647770 ) ) ;
#65485 = CARTESIAN_POINT ( 'NONE',  ( 1.686351706036745890, 0.2952755905511811885, 0.1292274648535926551 ) ) ;
#65486 = CARTESIAN_POINT ( 'NONE',  ( 1.036041590146032698, 3.421639014772782816E-16, 0.3464511005275203726 ) ) ;
#65487 = CARTESIAN_POINT ( 'NONE',  ( 0.9120734908136490793, 0.1771653543307087075, -0.09757992244046823083 ) ) ;
#65488 = CARTESIAN_POINT ( 'NONE',  ( 0.2099737532808405305, -0.6046776061558807314, 0.2411417322834647770 ) ) ;
#65489 = CARTESIAN_POINT ( 'NONE',  ( -1.305774278215222184, 0.2952755905511811885, 0.1292274648535926551 ) ) ;
#65490 = CARTESIAN_POINT ( 'NONE',  ( -1.384514435695537005, 0.2952755905511811885, 0.1292274648535926551 ) ) ;
#65491 = VERTEX_POINT ( 'NONE', #28300 ) ;
#65492 = CARTESIAN_POINT ( 'NONE',  ( 0.2925321140481932369, -0.2925321140481931814, -2.537401574803149984 ) ) ;
#65493 = CARTESIAN_POINT ( 'NONE',  ( -0.7545931758530176614, -0.5511811023622048555, -0.09757992244046775898 ) ) ;
#65494 = CARTESIAN_POINT ( 'NONE',  ( 0.5643044619422579178, -0.4281496062992127816, -0.4176697321401328100 ) ) ;
#65495 = CARTESIAN_POINT ( 'NONE',  ( -1.259842519685038686, -0.1870078740157479769, 0.3641732283464567677 ) ) ;
#65496 = CARTESIAN_POINT ( 'NONE',  ( -0.1070741851644056997, 0.3996062992125984925, -1.973097112860892510 ) ) ;
#65497 = CARTESIAN_POINT ( 'NONE',  ( -1.574803149606298636, -0.1870078740157479769, 0.4822834645669291653 ) ) ;
#65498 = CARTESIAN_POINT ( 'NONE',  ( 1.017060367454068803, -0.3162353388693405765, 0.4822834645669290543 ) ) ;
#65499 = CARTESIAN_POINT ( 'NONE',  ( 0.4855643044619430415, -0.4281496062992127816, -0.4176697321401328100 ) ) ;
#65500 = CARTESIAN_POINT ( 'NONE',  ( 1.233595800524935227, -0.6046776061558807314, 0.2411417322834647770 ) ) ;
#65501 = CARTESIAN_POINT ( 'NONE',  ( -0.3996062992125986035, -0.01591673448991143269, -1.219479340321616867 ) ) ;
#65502 = CARTESIAN_POINT ( 'NONE',  ( 0.3460692066303959757, -0.1998031496062991907, -1.522309711286089273 ) ) ;
#65503 = CARTESIAN_POINT ( 'NONE',  ( 4.837279021331060870E-17, -0.3949938075777409963, -0.5511811023622048555 ) ) ;
#65504 = CARTESIAN_POINT ( 'NONE',  ( 1.112371124080195450, -4.927456884911482678E-16, 0.4445507791589062840 ) ) ;
#65505 = CARTESIAN_POINT ( 'NONE',  ( 0.1574803149606306130, -0.1870078740157479769, 0.3641732283464567677 ) ) ;
#65506 = CARTESIAN_POINT ( 'NONE',  ( 0.01968503937007930540, 0.1660481256975885056, 0.3530559997133364547 ) ) ;
#65507 = CARTESIAN_POINT ( 'NONE',  ( 1.089238845144357537, -0.4281496062992124485, 0.4176697321401328655 ) ) ;
#65508 = CARTESIAN_POINT ( 'NONE',  ( -0.3420746716998662729, 0.1974969037888702206, -1.677821522309711710 ) ) ;
#65509 = CARTESIAN_POINT ( 'NONE',  ( 0.3805774278215230400, -0.3690944881889763329, 0.3153832671262228327 ) ) ;
#65510 = CARTESIAN_POINT ( 'NONE',  ( -0.5774278215223089816, -0.6046776061558807314, 0.2411417322834647770 ) ) ;
#65511 = CARTESIAN_POINT ( 'NONE',  ( -1.555118110236219930, -0.5400638737290845981, -0.3530559997133363437 ) ) ;
#65512 = CARTESIAN_POINT ( 'NONE',  ( 0.8727034120734913358, -0.05778040916215522460, 0.4822834645669289988 ) ) ;
#65513 = CARTESIAN_POINT ( 'NONE',  ( 0.3458507752293908943, 0.3458507752293908943, -1.870078740157480546 ) ) ;
#65514 = DIRECTION ( 'NONE',  ( -0.000000000000000000, 1.000000000000000000, -0.000000000000000000 ) ) ;
#65515 = B_SPLINE_CURVE_WITH_KNOTS ( 'NONE', 3,
 ( #45729, #39429, #65545, #72267 ),
 .UNSPECIFIED., .F., .F.,
 ( 4, 4 ),
 ( 3.210432057730626195E-07, 0.001287787053611998828 ),
 .UNSPECIFIED. ) ;
#65516 =( BOUNDED_CURVE ( )  B_SPLINE_CURVE ( 1, ( #75432, #56866 ),
 .UNSPECIFIED., .F., .F. ) 
 B_SPLINE_CURVE_WITH_KNOTS ( ( 2, 2 ),
 ( 0.000000000000000000, 0.002000000000000011317 ),
 .UNSPECIFIED. ) 
 CURVE ( )  GEOMETRIC_REPRESENTATION_ITEM ( )  RATIONAL_B_SPLINE_CURVE ( ( 0.9875488213027514561, 0.9875488213027514561 ) ) 
 REPRESENTATION_ITEM ( '' )  );
#65517 = ORIENTED_EDGE ( 'NONE', *, *, #54718, .T. ) ;
#65518 = ORIENTED_EDGE ( 'NONE', *, *, #80096, .T. ) ;
#65519 = CARTESIAN_POINT ( 'NONE',  ( -1.423884514435694859, -0.3162353388693405765, 0.4822834645669290543 ) ) ;
#65521 = CARTESIAN_POINT ( 'NONE',  ( -1.023622047244093558, -0.1870078740157479769, 0.4822834645669291653 ) ) ;
#65520 = CARTESIAN_POINT ( 'NONE',  ( -1.115485564304461219, -0.004921259842519870586, -0.3153832671262229437 ) ) ;
#65522 = CARTESIAN_POINT ( 'NONE',  ( 0.3917322834645668994, -0.1049643490035303134, -2.553786458496376088 ) ) ;
#65523 = CARTESIAN_POINT ( 'NONE',  ( -0.1070741851644051862, -0.3996062992125986590, -2.826115485564304475 ) ) ;
#65524 = CARTESIAN_POINT ( 'NONE',  ( 1.522309711286089939, 0.2306618581243848609, 0.2411417322834645549 ) ) ;
#65525 = CARTESIAN_POINT ( 'NONE',  ( -1.095800524934382292, -0.05778040916215522460, 0.4822834645669289988 ) ) ;
#65526 = CARTESIAN_POINT ( 'NONE',  ( 0.3477690288713918276, 0.2952755905511811885, 0.1292274648535926551 ) ) ;
#65527 = CARTESIAN_POINT ( 'NONE',  ( -1.161417322834644716, 0.1660481256975885056, 0.3530559997133364547 ) ) ;
#65528 = CARTESIAN_POINT ( 'NONE',  ( 0.2867679344610365999, 0.2867679344610365999, -2.737513492617110522 ) ) ;
#65529 = CARTESIAN_POINT ( 'NONE',  ( 0.7152230971128614723, -0.3162353388693409650, -0.4822834645669289433 ) ) ;
#65530 = CARTESIAN_POINT ( 'NONE',  ( 0.3917322834645669549, 0.1049643490035304660, -1.691601049868766360 ) ) ;
#65531 = CARTESIAN_POINT ( 'NONE',  ( -0.7742782152230962556, -0.3690944881889765550, -0.3153832671262227771 ) ) ;
#65532 = EDGE_LOOP ( 'NONE', ( #46063, #7769, #72566, #83015 ) ) ;
#65533 = CARTESIAN_POINT ( 'NONE',  ( -0.1974969037888706647, 0.3420746716998658843, -2.060367454068241067 ) ) ;
#65534 = AXIS2_PLACEMENT_3D ( 'NONE', #53747, #79457, #81007 ) ;
#65535 = VERTEX_POINT ( 'NONE', #47236 ) ;
#65536 = CARTESIAN_POINT ( 'NONE',  ( -1.522309711286088607, 0.1283753931104746893, -0.1820866141732285504 ) ) ;
#65537 = CIRCLE ( 'NONE', #46708, 1.122047244094488194 ) ;
#65538 = CARTESIAN_POINT ( 'NONE',  ( -0.9908136482939626788, -0.6692913385826773087, -0.1292274648535924053 ) ) ;
#65539 = CARTESIAN_POINT ( 'NONE',  ( -1.502624671916009680, -0.3162353388693405765, 0.4822834645669290543 ) ) ;
#65540 = CARTESIAN_POINT ( 'NONE',  ( 0.3996062992125986035, 2.446882876249141962E-17, -0.7480314960629921295 ) ) ;
#65541 = CARTESIAN_POINT ( 'NONE',  ( -1.522309711286088607, 0.2306618581243847221, -0.2411417322834647770 ) ) ;
#65542 = CARTESIAN_POINT ( 'NONE',  ( -1.233595800524933894, 0.2306618581243848609, 0.2411417322834645549 ) ) ;
#65543 = CARTESIAN_POINT ( 'NONE',  ( -1.463254593175852492, 0.2952755905511811885, 0.1292274648535926551 ) ) ;
#65544 = CARTESIAN_POINT ( 'NONE',  ( -1.614173228346457378, 1.818966223839196372, 0.1372047244094476981 ) ) ;
#65545 = CARTESIAN_POINT ( 'NONE',  ( -1.604771003085130321, 0.7270283685441725208, -0.1466069496707743391 ) ) ;
#65546 = CARTESIAN_POINT ( 'NONE',  ( 0.2034120734908144990, -0.5511811023622046335, 0.09757992244046803654 ) ) ;
#65547 = CARTESIAN_POINT ( 'NONE',  ( 2.795275590551181910, 1.900312960331935086, 0.000000000000000000 ) ) ;
#65548 = CARTESIAN_POINT ( 'NONE',  ( -0.1049643490035302024, -0.3917322834645671215, -0.3143044619422573072 ) ) ;
#65549 = CARTESIAN_POINT ( 'NONE',  ( -0.5118110236220466680, -0.5511811023622047445, 6.969142054262312111E-17 ) ) ;
#65550 = CARTESIAN_POINT ( 'NONE',  ( -0.6233595800524928121, -0.3162353388693409650, -0.4822834645669289433 ) ) ;
#65551 = CARTESIAN_POINT ( 'NONE',  ( 0.9251968503937015864, -0.5400638737290844871, 0.3530559997133364547 ) ) ;
#65552 = CARTESIAN_POINT ( 'NONE',  ( -0.9973753280839886548, 0.2306618581243848609, 0.2411417322834645549 ) ) ;
#65553 = ORIENTED_EDGE ( 'NONE', *, *, #72539, .T. ) ;
#65554 = ORIENTED_EDGE ( 'NONE', *, *, #81347, .T. ) ;
#65555 = CARTESIAN_POINT ( 'NONE',  ( -0.9317585301837263412, -0.4281496062992127816, -0.4176697321401328100 ) ) ;
#65556 = CARTESIAN_POINT ( 'NONE',  ( 0.7677165354330716118, -0.5400638737290844871, 0.3530559997133364547 ) ) ;
#65557 = CARTESIAN_POINT ( 'NONE',  ( -1.522309711286088607, 0.1283753931104746893, -0.1820866141732285504 ) ) ;
#65558 = CARTESIAN_POINT ( 'NONE',  ( 0.4091458600556404646, -0.2362204724409448231, -1.207349081364829324 ) ) ;
#65559 = CARTESIAN_POINT ( 'NONE',  ( 2.020039340939663752, 1.253873987468406392, 0.3814095263789863965 ) ) ;
#65560 = CARTESIAN_POINT ( 'NONE',  ( -9.594673741351313045E-17, 0.3917322834645670104, -0.3070866141732283006 ) ) ;
#65561 = CARTESIAN_POINT ( 'NONE',  ( 0.3392501089628018329, 0.1958661417322835607, -2.263123359580052618 ) ) ;
#65562 = CARTESIAN_POINT ( 'NONE',  ( -0.1443569553805765515, -0.4281496062992127816, -0.4176697321401328100 ) ) ;
#65563 = CARTESIAN_POINT ( 'NONE',  ( -1.404199475065615932, -0.3690944881889765550, -0.3153832671262227771 ) ) ;
#65564 = CARTESIAN_POINT ( 'NONE',  ( -0.7152230971128602510, -0.05778040916215560624, -0.4822834645669293319 ) ) ;
#65565 = CARTESIAN_POINT ( 'NONE',  ( 0.3996062992125984925, 0.1070741851644054637, 0.1135170603674540285 ) ) ;
#65567 = DIRECTION ( 'NONE',  ( 0.000000000000000000, 0.000000000000000000, 1.000000000000000000 ) ) ;
#65566 = CARTESIAN_POINT ( 'NONE',  ( -1.463254593175852492, -0.6692913385826773087, -0.1292274648535924053 ) ) ;
#65568 = CARTESIAN_POINT ( 'NONE',  ( -1.154855643044618851, -0.6046776061558809534, -0.2411417322834644161 ) ) ;
#65569 = CARTESIAN_POINT ( 'NONE',  ( -0.4133858267716528645, 0.1660481256975883668, -0.3530559997133364547 ) ) ;
#65570 = CARTESIAN_POINT ( 'NONE',  ( -0.2891555358219909388, -0.2891555358219912164, -2.655511811023621771 ) ) ;
#65571 = CARTESIAN_POINT ( 'NONE',  ( 0.2624671916010504757, -0.5023911411419708095, -0.1820866141732282451 ) ) ;
#65572 = CARTESIAN_POINT ( 'NONE',  ( 2.362204724409448620, 1.724409448818900570, 8.247593713802677664E-15 ) ) ;
#65573 = CARTESIAN_POINT ( 'NONE',  ( 0.5183727034120741983, -0.5511811023622046335, 0.09757992244046803654 ) ) ;
#65574 = CARTESIAN_POINT ( 'NONE',  ( 1.509186351706037543, -0.3690944881889765550, -0.3153832671262227771 ) ) ;
#65575 = CARTESIAN_POINT ( 'NONE',  ( 0.9842519685039375910, 0.2952755905511811885, 0.000000000000000000 ) ) ;
#65576 = CARTESIAN_POINT ( 'NONE',  ( 0.2887139107611556010, 0.1283753931104746893, -0.1820866141732285504 ) ) ;
#65577 = CARTESIAN_POINT ( 'NONE',  ( 0.3917322834645670104, 2.398668435337828261E-17, -2.000000000000000000 ) ) ;
#65578 = CARTESIAN_POINT ( 'NONE',  ( -1.456692913385826182, 0.2952755905511811885, 0.000000000000000000 ) ) ;
#65579 = CARTESIAN_POINT ( 'NONE',  ( -0.1706036745406816491, -0.3690944881889763329, 0.3153832671262228327 ) ) ;
#65580 = CARTESIAN_POINT ( 'NONE',  ( -1.157146581871515012E-16, 0.4724409448818898682, -0.07677165354330710290 ) ) ;
#65581 = CARTESIAN_POINT ( 'NONE',  ( -0.5118110236220466680, 0.1771653543307087630, 0.000000000000000000 ) ) ;
#65582 = ADVANCED_FACE ( 'NONE', ( #26644 ), #946, .F. ) ;
#65583 = CARTESIAN_POINT ( 'NONE',  ( -0.4624320255261038515, -2.191421614605370878E-15, 0.4445507791589071167 ) ) ;
#65584 = CARTESIAN_POINT ( 'NONE',  ( -0.2559055118110227234, -0.5400638737290844871, 0.3530559997133364547 ) ) ;
#65585 = FACE_OUTER_BOUND ( 'NONE', #80616, .T. ) ;
#65586 = CARTESIAN_POINT ( 'NONE',  ( 1.115485564304462551, -0.004921259842519576551, 0.3153832671262227771 ) ) ;
#65587 = CARTESIAN_POINT ( 'NONE',  ( 0.2427821522309716595, -0.2845877964562161244, -0.3641732283464567121 ) ) ;
#65588 = CARTESIAN_POINT ( 'NONE',  ( -0.3543307086614165824, 0.2952755905511811885, 0.000000000000000000 ) ) ;
#65589 = DIRECTION ( 'NONE',  ( 0.000000000000000000, -1.000000000000000000, 0.000000000000000000 ) ) ;
#65590 = CARTESIAN_POINT ( 'NONE',  ( -0.8923884514435688198, -0.5023911411419708095, 0.1820866141732285504 ) ) ;
#65591 = CARTESIAN_POINT ( 'NONE',  ( -1.646051170424378096, 0.8346805926620876059, 0.5309055118110233007 ) ) ;
#65592 = CARTESIAN_POINT ( 'NONE',  ( 0.7152230971128616943, -0.05778040916215522460, 0.4822834645669289988 ) ) ;
#65593 = CARTESIAN_POINT ( 'NONE',  ( -0.7480314960629914633, -0.6692913385826771977, 8.415575281601705876E-17 ) ) ;
#65594 = CARTESIAN_POINT ( 'NONE',  ( 0.2925321140481932369, -0.2925321140481931814, -1.277559055118109965 ) ) ;
#65595 = CARTESIAN_POINT ( 'NONE',  ( -0.1958661417322836718, 0.3392501089628017219, -2.774934383202099841 ) ) ;
#65596 = CARTESIAN_POINT ( 'NONE',  ( 0.05249343832021075018, 0.1283753931104746893, -0.1820866141732285504 ) ) ;
#65598 = VECTOR ( 'NONE', #29033, 39.37007874015748143 ) ;
#65597 = CARTESIAN_POINT ( 'NONE',  ( -0.6167979002624665030, -0.4281496062992127816, -0.4176697321401328100 ) ) ;
#65599 = CARTESIAN_POINT ( 'NONE',  ( -1.167979002624671470, 0.05413385826771666132, 0.4176697321401328100 ) ) ;
#65600 = CARTESIAN_POINT ( 'NONE',  ( -1.371391076115484609, -0.5511811023622046335, 0.09757992244046803654 ) ) ;
#65601 = CARTESIAN_POINT ( 'NONE',  ( -3.908320185825792326, 1.521933560353155857, -0.4744094488188975722 ) ) ;
#65602 = EDGE_CURVE ( 'NONE', #1230, #33111, #8129, .T. ) ;
#65603 = CARTESIAN_POINT ( 'NONE',  ( -0.8202099737532799750, 0.1771653543307087075, -0.09757992244046823083 ) ) ;
#65604 = DIRECTION ( 'NONE',  ( 0.000000000000000000, 0.000000000000000000, 1.000000000000000000 ) ) ;
#65605 = CARTESIAN_POINT ( 'NONE',  ( 0.7545931758530188826, -0.6692913385826771977, 0.1292274648535927661 ) ) ;
#65606 = CARTESIAN_POINT ( 'NONE',  ( -0.3996062992125986035, -0.1070741851644056997, -0.2034120734908136108 ) ) ;
#65607 = CARTESIAN_POINT ( 'NONE',  ( 0.3392501089628018329, 0.1958661417322835607, -2.490176796096799539 ) ) ;
#65608 = ORIENTED_EDGE ( 'NONE', *, *, #31972, .T. ) ;
#65609 = ADVANCED_FACE ( 'NONE', ( #1810 ), #57365, .F. ) ;
#65610 = CARTESIAN_POINT ( 'NONE',  ( 1.141392835773559211, 1.299212598425196985, 1.141392835773562764 ) ) ;
#65611 = CARTESIAN_POINT ( 'NONE',  ( 1.417322834645670104, -0.1870078740157479769, 0.3641732283464567677 ) ) ;
#65612 = CARTESIAN_POINT ( 'NONE',  ( -1.207349081364828880, 0.2306618581243847221, -0.2411417322834647770 ) ) ;
#65613 = CARTESIAN_POINT ( 'NONE',  ( 1.246719160104987623, -0.4281496062992124485, 0.4176697321401328655 ) ) ;
#65614 = CARTESIAN_POINT ( 'NONE',  ( -0.1958661417322836718, 0.3392501089628017219, -2.459973753280839670 ) ) ;
#65615 = CARTESIAN_POINT ( 'NONE',  ( 1.522309711286089939, 0.1283753931104748280, 0.1820866141732283561 ) ) ;
#65616 = CARTESIAN_POINT ( 'NONE',  ( 0.6692913385826778638, -0.6692913385826771977, 8.415575281601705876E-17 ) ) ;
#65617 = CARTESIAN_POINT ( 'NONE',  ( -0.2427821522309703550, -0.3162353388693405765, 0.4822834645669290543 ) ) ;
#65618 = CARTESIAN_POINT ( 'NONE',  ( -3.911372956956467029, 1.694725607269298218, 0.4487278785265438885 ) ) ;
#65619 = CARTESIAN_POINT ( 'NONE',  ( -0.2925321140481930704, -0.2925321140481933480, -1.948818897637795144 ) ) ;
#65620 = CARTESIAN_POINT ( 'NONE',  ( 0.6299212598425204535, -0.1870078740157479769, 0.3641732283464567677 ) ) ;
#65621 = CARTESIAN_POINT ( 'NONE',  ( 0.1070741851644054915, -0.3996062992125986035, -1.817585301837270517 ) ) ;
#65622 = ORIENTED_EDGE ( 'NONE', *, *, #76445, .F. ) ;
#65623 = CARTESIAN_POINT ( 'NONE',  ( 0.1049643490035303967, 0.3917322834645670659, 0.009823203903200209905 ) ) ;
#65624 = EDGE_LOOP ( 'NONE', ( #61771, #20695, #17191, #71927, #40786 ) ) ;
#65625 = CARTESIAN_POINT ( 'NONE',  ( -0.08530183727034056085, -0.05778040916215560624, -0.4822834645669293319 ) ) ;
#65626 = CARTESIAN_POINT ( 'NONE',  ( 1.299212598425197429, 0.2952755905511811885, 0.000000000000000000 ) ) ;
#65627 = CARTESIAN_POINT ( 'NONE',  ( 0.2296587926509192634, -0.3162353388693405765, 0.4822834645669290543 ) ) ;
#65628 = CARTESIAN_POINT ( 'NONE',  ( -0.5380577427821514602, -0.004921259842519576551, 0.3153832671262227771 ) ) ;
#65629 = CARTESIAN_POINT ( 'NONE',  ( 1.391076115485564868, 0.2306618581243847221, -0.2411417322834647770 ) ) ;
#65630 = CARTESIAN_POINT ( 'NONE',  ( -0.3149606299212590610, -0.1870078740157480879, -0.4822834645669291653 ) ) ;
#65631 = CARTESIAN_POINT ( 'NONE',  ( -0.01312335958005186876, -0.4281496062992124485, 0.4176697321401328655 ) ) ;
#65632 = CARTESIAN_POINT ( 'NONE',  ( -1.515748031496062076, -0.5400638737290844871, 0.3530559997133364547 ) ) ;
#65633 = CARTESIAN_POINT ( 'NONE',  ( 1.469816272965879911, 0.2306618581243847221, -0.2411417322834647770 ) ) ;
#65634 = EDGE_CURVE ( 'NONE', #80735, #21338, #76216, .T. ) ;
#65635 = CARTESIAN_POINT ( 'NONE',  ( 1.338582677165355062, -0.1870078740157479769, 0.4822834645669291653 ) ) ;
#65636 = CARTESIAN_POINT ( 'NONE',  ( 0.3392501089628018329, 0.1958661417322835607, -0.7532808398950130435 ) ) ;
#65637 = CARTESIAN_POINT ( 'NONE',  ( 0.4921259842519691285, -0.4536011799217368745, -0.2665933059059886201 ) ) ;
#65638 = ORIENTED_EDGE ( 'NONE', *, *, #34659, .F. ) ;
#65639 = CARTESIAN_POINT ( 'NONE',  ( -0.2891555358219911054, 0.2891555358219909388, -0.8070866141732284671 ) ) ;
#65640 = ORIENTED_EDGE ( 'NONE', *, *, #69856, .F. ) ;
#65641 = CARTESIAN_POINT ( 'NONE',  ( -0.2755905511811018171, 0.1771653543307087630, 0.000000000000000000 ) ) ;
#65642 = CARTESIAN_POINT ( 'NONE',  ( 0.01312335958005323398, -0.4281496062992127816, -0.4176697321401328100 ) ) ;
#65643 = CARTESIAN_POINT ( 'NONE',  ( 2.829418903715935407, 1.111478976311908617, 0.2095522481616418631 ) ) ;
#65644 = CARTESIAN_POINT ( 'NONE',  ( -0.1377952755905504645, 0.1660481256975885056, 0.3530559997133364547 ) ) ;
#65645 = CARTESIAN_POINT ( 'NONE',  ( -0.05905511811023545637, -0.5400638737290845981, -0.3530559997133363437 ) ) ;
#65646 = CARTESIAN_POINT ( 'NONE',  ( -0.9908136482939626788, 0.2952755905511811885, 0.1292274648535926551 ) ) ;
#65647 = CARTESIAN_POINT ( 'NONE',  ( -0.8464566929133852113, -0.5400638737290845981, -0.3530559997133363437 ) ) ;
#65648 = EDGE_CURVE ( 'NONE', #17964, #400, #2458, .T. ) ;
#65649 = CARTESIAN_POINT ( 'NONE',  ( 1.233595800524935227, 0.1283753931104746893, -0.1820866141732285504 ) ) ;
#65650 = CARTESIAN_POINT ( 'NONE',  ( -1.515748031496062076, -0.5400638737290844871, 0.3530559997133364547 ) ) ;
#65651 = CARTESIAN_POINT ( 'NONE',  ( 5.785732909357575061E-17, -0.4724409448818898682, -2.755905511811023612 ) ) ;
#65652 = CARTESIAN_POINT ( 'NONE',  ( 1.102362204724410155, -0.1870078740157479769, 0.3641732283464567677 ) ) ;
#65653 = CARTESIAN_POINT ( 'NONE',  ( 0.3805774278215230400, -0.4281496062992124485, 0.4176697321401328655 ) ) ;
#65654 = CARTESIAN_POINT ( 'NONE',  ( 0.3740157480314966754, -0.5400638737290844871, 0.3530559997133364547 ) ) ;
#65655 = CARTESIAN_POINT ( 'NONE',  ( 0.3460692066303959757, -0.1998031496062991907, -1.364829396325459188 ) ) ;
#65656 = CARTESIAN_POINT ( 'NONE',  ( -1.653543307086613234, -0.1870078740157480879, -0.4822834645669291653 ) ) ;
#65657 = CARTESIAN_POINT ( 'NONE',  ( -0.3996062992125986590, 0.1070741851644051723, -0.5820209973753280863 ) ) ;
#65658 = CARTESIAN_POINT ( 'NONE',  ( 0.3460692066303959202, -0.1998031496062991630, -0.3392388451443569819 ) ) ;
#65659 = CARTESIAN_POINT ( 'NONE',  ( -0.5577427821522301654, -0.05778040916215560624, -0.4822834645669293319 ) ) ;
#65660 = CARTESIAN_POINT ( 'NONE',  ( 0.4091458600556404646, -0.2362204724409448231, 0.05249343832020997302 ) ) ;
#65661 =( BOUNDED_CURVE ( )  B_SPLINE_CURVE ( 2, ( #28754, #4321, #41388, #73805, #10653, #48107, #35072 ),
 .UNSPECIFIED., .F., .F. ) 
 B_SPLINE_CURVE_WITH_KNOTS ( ( 3, 2, 2, 3 ),
 ( 0.05000000000000000278, 0.05416666666666666852, 0.05833333333333333426, 0.06250000000000000000 ),
 .UNSPECIFIED. ) 
 CURVE ( )  GEOMETRIC_REPRESENTATION_ITEM ( )  RATIONAL_B_SPLINE_CURVE ( ( 1.000000000000000000, 0.9659258262890683122, 1.000000000000000000, 0.9659258262890683122, 1.000000000000000000, 0.9659258262890683122, 1.000000000000000000 ) ) 
 REPRESENTATION_ITEM ( '' )  );
#65662 = EDGE_CURVE ( 'NONE', #58992, #64597, #47874, .T. ) ;
#65663 = CARTESIAN_POINT ( 'NONE',  ( 0.3917322834645670104, 2.398668435337828261E-17, -1.935039370078740273 ) ) ;
#65664 = CARTESIAN_POINT ( 'NONE',  ( -1.095800524934382292, -0.2845877964562161244, -0.3641732283464567121 ) ) ;
#65665 = CARTESIAN_POINT ( 'NONE',  ( 0.9973753280839902091, 0.2306618581243847221, -0.2411417322834647770 ) ) ;
#65666 = AXIS2_PLACEMENT_3D ( 'NONE', #44125, #5832, #57165 ) ;
#65667 = CARTESIAN_POINT ( 'NONE',  ( 1.049868766404200349, 0.2306618581243848609, 0.2411417322834645549 ) ) ;
#65668 = CARTESIAN_POINT ( 'NONE',  ( -0.06561679790026180015, -0.004921259842519576551, 0.3153832671262227771 ) ) ;
#65669 = CARTESIAN_POINT ( 'NONE',  ( 0.5249343832021003964, 0.2306618581243847221, -0.2411417322834647770 ) ) ;
#65670 = CARTESIAN_POINT ( 'NONE',  ( -0.2362204724409447953, -0.4091458600556404646, -1.717191601049868677 ) ) ;
#65671 = CARTESIAN_POINT ( 'NONE',  ( -0.2690288713910754526, -0.5511811023622046335, 0.09757992244046803654 ) ) ;
#65672 = CARTESIAN_POINT ( 'NONE',  ( 0.05905511811023681640, 0.1660481256975883668, -0.3530559997133364547 ) ) ;
#65673 = CARTESIAN_POINT ( 'NONE',  ( 4.837279021331061486E-17, -0.3949938075777409963, -1.415354330708661346 ) ) ;
#65674 = CARTESIAN_POINT ( 'NONE',  ( -1.305774278215222184, -0.6692913385826773087, -0.1292274648535924053 ) ) ;
#65675 = CARTESIAN_POINT ( 'NONE',  ( 0.6496062992125991586, 0.07958543189024085140, 0.2665933059059887866 ) ) ;
#65676 = CARTESIAN_POINT ( 'NONE',  ( 1.482939632545932307, -0.3690944881889763329, 0.3153832671262228327 ) ) ;
#65677 = CARTESIAN_POINT ( 'NONE',  ( -0.8661417322834640276, -0.1870078740157480879, -0.4822834645669291653 ) ) ;
#65678 = CARTESIAN_POINT ( 'NONE',  ( -0.2230971128608915943, -0.004921259842519576551, 0.3153832671262227771 ) ) ;
#65679 = CARTESIAN_POINT ( 'NONE',  ( -0.4724409448818898682, -8.678599364036362592E-17, -2.005905511811023612 ) ) ;
#65680 = CARTESIAN_POINT ( 'NONE',  ( -0.7217847769028863381, 0.05413385826771626580, -0.4176697321401330321 ) ) ;
#65681 = CARTESIAN_POINT ( 'NONE',  ( -0.5971128608923877978, -0.6692913385826773087, -0.1292274648535924053 ) ) ;
#65682 = CARTESIAN_POINT ( 'NONE',  ( -0.1049868766404193215, -0.6046776061558807314, 0.2411417322834647770 ) ) ;
#65683 = CARTESIAN_POINT ( 'NONE',  ( -0.2925321140481930149, -0.2925321140481933480, -2.498031496062992574 ) ) ;
#65684 = CARTESIAN_POINT ( 'NONE',  ( -0.3917322834645670659, 0.1049643490035301607, -2.160085671094801540 ) ) ;
#65685 = CARTESIAN_POINT ( 'NONE',  ( -1.574803149606298636, -0.1870078740157479769, 0.3641732283464567677 ) ) ;
#65686 = CARTESIAN_POINT ( 'NONE',  ( 0.8595800524934390507, -0.2845877964562159024, 0.3641732283464567677 ) ) ;
#65687 = CARTESIAN_POINT ( 'NONE',  ( 1.384514435695538337, -0.6692913385826771977, 0.1292274648535927661 ) ) ;
#65688 = CARTESIAN_POINT ( 'NONE',  ( -0.6496062992125976043, -0.4536011799217367080, 0.2665933059059888421 ) ) ;
#65689 = CARTESIAN_POINT ( 'NONE',  ( -1.200787401574802349, 0.07958543189024071263, -0.2665933059059888421 ) ) ;
#65690 = CARTESIAN_POINT ( 'NONE',  ( -0.6889763779527552368, 0.1660481256975885056, 0.3530559997133364547 ) ) ;
#65691 = CARTESIAN_POINT ( 'NONE',  ( -0.4593175853018366950, 0.05413385826771666132, 0.4176697321401328100 ) ) ;
#65692 = CARTESIAN_POINT ( 'NONE',  ( 0.5118110236220480003, -0.5511811023622047445, 6.969142054262312111E-17 ) ) ;
#65693 = CARTESIAN_POINT ( 'NONE',  ( 1.266404199475066328, -0.08942795157527998196, 0.3641732283464567121 ) ) ;
#65694 = CARTESIAN_POINT ( 'NONE',  ( 0.4396325459317593221, 0.2952755905511810774, -0.1292274648535930714 ) ) ;
#65695 = CYLINDRICAL_SURFACE ( 'NONE', #19567, 0.3937007874015748254 ) ;
#65696 = CARTESIAN_POINT ( 'NONE',  ( -0.4855643044619415427, -0.4281496062992124485, 0.4176697321401328655 ) ) ;
#65697 = CARTESIAN_POINT ( 'NONE',  ( -0.1049643490035302024, -0.3917322834645671215, -1.574146981627296604 ) ) ;
#65698 = CARTESIAN_POINT ( 'NONE',  ( 1.568241469816273437, -0.2845877964562159024, 0.3641732283464567677 ) ) ;
#65699 = CARTESIAN_POINT ( 'NONE',  ( 0.5971128608923891301, 0.2952755905511810774, -0.1292274648535930714 ) ) ;
#65700 = CARTESIAN_POINT ( 'NONE',  ( 0.3215223097112867578, -0.3162353388693409650, -0.4822834645669289433 ) ) ;
#65701 = CARTESIAN_POINT ( 'NONE',  ( 0.07874015748031558404, -0.1870078740157479769, 0.3641732283464567677 ) ) ;
#65702 = CARTESIAN_POINT ( 'NONE',  ( 1.113459889019126514, -1.206088964116209378E-16, 0.3954974714151466841 ) ) ;
#65703 = CARTESIAN_POINT ( 'NONE',  ( 0.01312335958005323398, -0.3690944881889765550, -0.3153832671262227771 ) ) ;
#65704 = CARTESIAN_POINT ( 'NONE',  ( 0.7020997375328090762, -0.3162353388693405765, 0.4822834645669290543 ) ) ;
#65705 = EDGE_CURVE ( 'NONE', #53888, #30109, #71904, .T. ) ;
#65706 = CARTESIAN_POINT ( 'NONE',  ( -0.5708661417322828946, 0.07958543189024071263, -0.2665933059059888421 ) ) ;
#65707 = CARTESIAN_POINT ( 'NONE',  ( -0.8989501312335946848, -0.6692913385826771977, 0.1292274648535927661 ) ) ;
#65708 = DIRECTION ( 'NONE',  ( 0.000000000000000000, 0.000000000000000000, -1.000000000000000000 ) ) ;
#65709 = ORIENTED_EDGE ( 'NONE', *, *, #75114, .T. ) ;
#65710 = CARTESIAN_POINT ( 'NONE',  ( -1.076115485564303809, -0.6046776061558809534, -0.2411417322834644161 ) ) ;
#65711 = CARTESIAN_POINT ( 'NONE',  ( -1.095800524934382292, -0.08942795157527998196, 0.3641732283464567121 ) ) ;
#65712 = CARTESIAN_POINT ( 'NONE',  ( -0.1837270341207343505, -0.6046776061558807314, 0.2411417322834647770 ) ) ;
#65713 = CARTESIAN_POINT ( 'NONE',  ( -1.666666666666665853, 0.05413385826771626580, -0.4176697321401330321 ) ) ;
#65714 = CARTESIAN_POINT ( 'NONE',  ( -0.6496062992125976043, 0.1660481256975883668, -0.3530559997133364547 ) ) ;
#65715 = CYLINDRICAL_SURFACE ( 'NONE', #71351, 0.4744094488188972947 ) ;
#65717 = CARTESIAN_POINT ( 'NONE',  ( 0.8136482939632553313, 0.2306618581243848609, 0.2411417322834645549 ) ) ;
#65716 = CARTESIAN_POINT ( 'NONE',  ( 1.627296587926509996, -0.6046776061558807314, 0.2411417322834647770 ) ) ;
#65718 = CARTESIAN_POINT ( 'NONE',  ( 0.8202099737532814183, -0.6692913385826773087, -0.1292274648535924053 ) ) ;
#65719 = CARTESIAN_POINT ( 'NONE',  ( 0.3392501089628018884, -0.1958661417322834220, -2.301837270341207553 ) ) ;
#65720 = CARTESIAN_POINT ( 'NONE',  ( -1.154855643044618851, -0.6046776061558809534, -0.2411417322834644161 ) ) ;
#65721 = CARTESIAN_POINT ( 'NONE',  ( -9.787531504996567848E-17, 0.3996062992125986035, -0.1574803149606299746 ) ) ;
#65722 = ORIENTED_EDGE ( 'NONE', *, *, #67683, .T. ) ;
#65723 = CARTESIAN_POINT ( 'NONE',  ( -0.5774278215223089816, -0.5023911411419708095, 0.1820866141732285504 ) ) ;
#65724 = CARTESIAN_POINT ( 'NONE',  ( 0.3917322834645670104, -0.1049643490035303411, -1.835958005249343827 ) ) ;
#65725 = VERTEX_POINT ( 'NONE', #74404 ) ;
#65726 = CARTESIAN_POINT ( 'NONE',  ( 0.2296587926509192634, -0.05778040916215560624, -0.4822834645669293319 ) ) ;
#65727 = CARTESIAN_POINT ( 'NONE',  ( -0.1706036745406816491, -0.4281496062992124485, 0.4176697321401328655 ) ) ;
#65728 = CARTESIAN_POINT ( 'NONE',  ( -0.6824146981627288167, 0.2306618581243848609, 0.2411417322834645549 ) ) ;
#65729 = CARTESIAN_POINT ( 'NONE',  ( 1.535433070866142558, 0.2952755905511811885, 0.000000000000000000 ) ) ;
#65730 = CARTESIAN_POINT ( 'NONE',  ( -1.003937007874014853, 0.07958543189024085140, 0.2665933059059887866 ) ) ;
#65731 = CARTESIAN_POINT ( 'NONE',  ( 0.01715078996012292523, 1.063284142118728903, -1.620408976207265761 ) ) ;
#65732 = CARTESIAN_POINT ( 'NONE',  ( 0.6758530183727039509, -0.6692913385826771977, 0.1292274648535927661 ) ) ;
#65733 = CARTESIAN_POINT ( 'NONE',  ( 0.6561679790026253567, 0.1283753931104748280, 0.1820866141732283561 ) ) ;
#65734 = CARTESIAN_POINT ( 'NONE',  ( -0.4133858267716528645, -0.5400638737290844871, 0.3530559997133364547 ) ) ;
#65735 = CARTESIAN_POINT ( 'NONE',  ( 0.3917322834645668994, 0.1049643490035304522, -1.307067298391389354 ) ) ;
#65736 = CARTESIAN_POINT ( 'NONE',  ( -0.8923884514435688198, -0.6046776061558807314, 0.2411417322834647770 ) ) ;
#65737 = CARTESIAN_POINT ( 'NONE',  ( -1.568241469816272105, -0.08942795157527998196, 0.3641732283464567121 ) ) ;
#65738 = CARTESIAN_POINT ( 'NONE',  ( 1.358267716535433323, 0.1660481256975885056, 0.3530559997133364547 ) ) ;
#65739 = CARTESIAN_POINT ( 'NONE',  ( 1.601049868766404982, -0.5023911411419708095, -0.1820866141732282451 ) ) ;
#65740 = EDGE_LOOP ( 'NONE', ( #31659, #21302, #26287, #41909 ) ) ;
#65741 = CARTESIAN_POINT ( 'NONE',  ( 4.797336870675656522E-17, -0.3917322834645670659, -2.280203042815959869 ) ) ;
#65742 = CARTESIAN_POINT ( 'NONE',  ( 0.09186351706036827158, 0.05413385826771666132, 0.4176697321401328100 ) ) ;
#65743 = VERTEX_POINT ( 'NONE', #21797 ) ;
#65744 = CARTESIAN_POINT ( 'NONE',  ( -1.056430446194224881, 0.2952755905511810774, -0.1292274648535930714 ) ) ;
#65745 = CARTESIAN_POINT ( 'NONE',  ( 1.384514435695538337, -0.6692913385826771977, 0.1292274648535927661 ) ) ;
#65746 = CARTESIAN_POINT ( 'NONE',  ( 1.174540682414699111, -0.05778040916215560624, -0.4822834645669293319 ) ) ;
#65747 = CARTESIAN_POINT ( 'NONE',  ( 0.3477690288713918276, 0.2952755905511811885, 0.1292274648535926551 ) ) ;
#65748 = CARTESIAN_POINT ( 'NONE',  ( -0.4593175853018364174, -0.4281496062992127816, -0.4176697321401328100 ) ) ;
#65749 = CARTESIAN_POINT ( 'NONE',  ( 0.2867679344610365999, 0.2867679344610365999, -1.954724409448818978 ) ) ;
#65750 = CARTESIAN_POINT ( 'NONE',  ( -1.227034120734907585, 0.2952755905511811885, 0.1292274648535926551 ) ) ;
#65751 = CARTESIAN_POINT ( 'NONE',  ( -0.4002624671916004129, -0.3162353388693405765, 0.4822834645669290543 ) ) ;
#65752 = CARTESIAN_POINT ( 'NONE',  ( -0.5971128608923877978, -0.5511811023622048555, -0.09757992244046775898 ) ) ;
#65753 = CARTESIAN_POINT ( 'NONE',  ( -2.795275590551185907, 0.4724409448818907564, -3.981376139758521912E-16 ) ) ;
#65754 = CARTESIAN_POINT ( 'NONE',  ( -0.4790026246719154557, -0.3162353388693405765, 0.4822834645669290543 ) ) ;
#65755 = CARTESIAN_POINT ( 'NONE',  ( -0.5314960629921393620, 2.751923335154144556, 3.846978723397334488 ) ) ;
#65756 = CARTESIAN_POINT ( 'NONE',  ( 0.5905511811023629321, -0.6692913385826771977, 8.415575281601705876E-17 ) ) ;
#65757 = CARTESIAN_POINT ( 'NONE',  ( 3.927301751045197964, 1.151648106155687801, -0.2765835404858998925 ) ) ;
#65758 = CARTESIAN_POINT ( 'NONE',  ( 0.07217847769028949700, -0.3162353388693405765, 0.4822834645669290543 ) ) ;
#65759 = CARTESIAN_POINT ( 'NONE',  ( -0.3018372703412066094, -0.004921259842519576551, 0.3153832671262227771 ) ) ;
#65761 = CARTESIAN_POINT ( 'NONE',  ( -0.8858267716535425107, 0.1012011053420775880, -0.2882089793578257453 ) ) ;
#65760 = CARTESIAN_POINT ( 'NONE',  ( 1.174540682414699111, -0.2845877964562159024, 0.3641732283464567677 ) ) ;
#65762 = CARTESIAN_POINT ( 'NONE',  ( -0.1265901696524986964, -0.4724409448818899238, -0.4639107611548556331 ) ) ;
#65763 = CARTESIAN_POINT ( 'NONE',  ( 0.9776902887139113929, -0.5511811023622048555, -0.09757992244046775898 ) ) ;
#65764 = AXIS2_PLACEMENT_3D ( 'NONE', #46811, #52285, #53118 ) ;
#65765 = CARTESIAN_POINT ( 'NONE',  ( 1.312335958005249825, 0.2306618581243847221, -0.2411417322834647770 ) ) ;
#65766 = CARTESIAN_POINT ( 'NONE',  ( 0.1058382717557500852, -0.3949938075777408852, -0.004593175853018378711 ) ) ;
#65767 = CARTESIAN_POINT ( 'NONE',  ( 0.06561679790026316017, 0.05413385826771626580, -0.4176697321401330321 ) ) ;
#65768 = CARTESIAN_POINT ( 'NONE',  ( -0.03443470937339728616, 1.062992125984252079, -1.537015892239756099 ) ) ;
#65769 = CARTESIAN_POINT ( 'NONE',  ( 1.568241469816273437, -0.2845877964562159024, 0.3641732283464567677 ) ) ;
#65770 = CARTESIAN_POINT ( 'NONE',  ( -0.3477690288713905509, -0.6692913385826771977, 0.1292274648535927661 ) ) ;
#65771 = CARTESIAN_POINT ( 'NONE',  ( -0.1058382717557503072, 0.3949938075777408852, -0.2408136482939632617 ) ) ;
#65772 = CARTESIAN_POINT ( 'NONE',  ( -1.522309711286088607, -0.5023911411419708095, 0.1820866141732285504 ) ) ;
#65773 = CARTESIAN_POINT ( 'NONE',  ( 0.6496062992125991586, 0.1660481256975885056, 0.3530559997133364547 ) ) ;
#65774 = CARTESIAN_POINT ( 'NONE',  ( 0.9580052493438327987, -0.3690944881889765550, -0.3153832671262227771 ) ) ;
#65775 = CARTESIAN_POINT ( 'NONE',  ( 0.8070866141732288002, 0.1012011053420777407, 0.2882089793578257453 ) ) ;
#65776 = CARTESIAN_POINT ( 'NONE',  ( 0.5774278215223104249, 0.1283753931104748280, 0.1820866141732283561 ) ) ;
#65777 = CARTESIAN_POINT ( 'NONE',  ( -1.312335958005248715, 0.2306618581243848609, 0.2411417322834645549 ) ) ;
#65778 = CARTESIAN_POINT ( 'NONE',  ( -0.3996062992125984925, -0.1070741851644056858, -1.067585301837270517 ) ) ;
#65779 = CARTESIAN_POINT ( 'NONE',  ( 1.207349081364829990, 0.2306618581243848609, 0.2411417322834645549 ) ) ;
#65780 = CARTESIAN_POINT ( 'NONE',  ( 0.1049643490035304938, -0.3917322834645669549, -0.5498687664041993495 ) ) ;
#65782 = CARTESIAN_POINT ( 'NONE',  ( -0.3458507752293906723, -0.3458507752293910609, -0.4507874015748031815 ) ) ;
#65781 = CARTESIAN_POINT ( 'NONE',  ( 0.2952755905511819101, 0.1660481256975883668, -0.3530559997133364547 ) ) ;
#65783 = CARTESIAN_POINT ( 'NONE',  ( -0.8478501267249378692, 2.401574803149606474, 0.8478501267249375362 ) ) ;
#65784 = CARTESIAN_POINT ( 'NONE',  ( 0.3149606299212603933, -0.1870078740157479769, 0.3641732283464567677 ) ) ;
#65785 = CARTESIAN_POINT ( 'NONE',  ( 0.4199475065616805614, 0.2306618581243848609, 0.2411417322834645549 ) ) ;
#65786 = CARTESIAN_POINT ( 'NONE',  ( 3.833048052449394218E-17, 0.000000000000000000, 0.3129921259842520787 ) ) ;
#65787 = CARTESIAN_POINT ( 'NONE',  ( -1.069553805774277722, 0.1771653543307087630, 0.09757992244046791164 ) ) ;
#65788 = CARTESIAN_POINT ( 'NONE',  ( -1.200787401574802349, 0.1660481256975883668, -0.3530559997133364547 ) ) ;
#65789 = CARTESIAN_POINT ( 'NONE',  ( -1.364829396325458521, 0.2306618581243847221, -0.2411417322834647770 ) ) ;
#65790 = CARTESIAN_POINT ( 'NONE',  ( 0.6496062992125991586, -0.5400638737290845981, -0.3530559997133363437 ) ) ;
#65791 = CARTESIAN_POINT ( 'NONE',  ( -1.574803149606298192, -0.1870078740157480601, -0.3641732283464567677 ) ) ;
#65792 = CYLINDRICAL_SURFACE ( 'NONE', #50436, 0.4744094488188972947 ) ;
#65793 = CARTESIAN_POINT ( 'NONE',  ( 0.7349081364829402885, -0.6046776061558809534, -0.2411417322834644161 ) ) ;
#65794 = CARTESIAN_POINT ( 'NONE',  ( -0.2925321140481932369, 0.2925321140481931259, 0.2185039370078740162 ) ) ;
#65795 = CARTESIAN_POINT ( 'NONE',  ( 0.06179341360373440117, 1.065997766574747319, 3.936642186895995987 ) ) ;
#65796 = CARTESIAN_POINT ( 'NONE',  ( 1.443569553805774897, -0.6046776061558809534, -0.2411417322834644161 ) ) ;
#65797 = CARTESIAN_POINT ( 'NONE',  ( -1.299212598425196097, -0.5511811023622047445, 6.969142054262312111E-17 ) ) ;
#65798 = CARTESIAN_POINT ( 'NONE',  ( 1.095800524934383846, -0.08942795157528024563, -0.3641732283464568787 ) ) ;
#65799 = CARTESIAN_POINT ( 'NONE',  ( -1.345144356955379816, -0.2845877964562159024, 0.3641732283464567677 ) ) ;
#65800 = CARTESIAN_POINT ( 'NONE',  ( -0.7545931758530176614, -0.5511811023622048555, -0.09757992244046775898 ) ) ;
#65801 = EDGE_CURVE ( 'NONE', #64662, #35562, #28940, .T. ) ;
#65802 = CARTESIAN_POINT ( 'NONE',  ( -3.224202737261815166, 2.716535433070866645, 0.5314960629921260393 ) ) ;
#65803 = CARTESIAN_POINT ( 'NONE',  ( 0.3083989501312343062, -0.2845877964562159024, 0.3641732283464567677 ) ) ;
#65804 = CARTESIAN_POINT ( 'NONE',  ( 0.5708661417322842269, 0.1660481256975885056, 0.3530559997133364547 ) ) ;
#65805 = CARTESIAN_POINT ( 'NONE',  ( 1.253280839895013710, -0.3162353388693405765, 0.4822834645669290543 ) ) ;
#65806 = CARTESIAN_POINT ( 'NONE',  ( -0.1049868766404193215, -0.6046776061558807314, 0.2411417322834647770 ) ) ;
#65807 = CARTESIAN_POINT ( 'NONE',  ( -0.04593175853018302557, -0.5511811023622048555, -0.09757992244046775898 ) ) ;
#65808 = CARTESIAN_POINT ( 'NONE',  ( 1.404199475065617264, -0.4281496062992124485, 0.4176697321401328655 ) ) ;
#65809 = CARTESIAN_POINT ( 'NONE',  ( -1.607611548556429737, 0.2952755905511810774, -0.1292274648535930714 ) ) ;
#65810 = CARTESIAN_POINT ( 'NONE',  ( -1.062992125984250968, 0.2952755905511811885, 0.000000000000000000 ) ) ;
#65811 = CARTESIAN_POINT ( 'NONE',  ( -0.3996062992125986035, -7.340648628747425578E-17, -0.9842519685039369248 ) ) ;
#65812 = CARTESIAN_POINT ( 'NONE',  ( 0.05249343832021075018, 0.1539470093639521697, -0.1968503937007875793 ) ) ;
#65813 = CARTESIAN_POINT ( 'NONE',  ( 0.006561679790026889343, -0.05778040916215522460, 0.4822834645669289988 ) ) ;
#65814 = CARTESIAN_POINT ( 'NONE',  ( -0.9186351706036736120, -0.6046776061558809534, -0.2411417322834644161 ) ) ;
#65815 = CARTESIAN_POINT ( 'NONE',  ( 0.1312335958005255154, -0.6046776061558807314, 0.2411417322834647770 ) ) ;
#65816 = CARTESIAN_POINT ( 'NONE',  ( -0.3460692066303960868, 0.1998031496062990242, -2.545931758530183497 ) ) ;
#65817 = CARTESIAN_POINT ( 'NONE',  ( -0.2891555358219911054, 0.2891555358219909388, -1.751968503937008093 ) ) ;
#65818 = CARTESIAN_POINT ( 'NONE',  ( 0.3392501089628018884, -0.1958661417322834220, -0.7270341207349080292 ) ) ;
#65819 = CARTESIAN_POINT ( 'NONE',  ( 0.1958661417322836440, -0.3392501089628017219, -1.028871391076115360 ) ) ;
#65820 = CARTESIAN_POINT ( 'NONE',  ( -0.8070866141732276899, -0.4536011799217367080, 0.2665933059059888421 ) ) ;
#65821 = CARTESIAN_POINT ( 'NONE',  ( 0.3917322834645670104, -0.1049643490035303411, -1.048556430446194287 ) ) ;
#65822 = CARTESIAN_POINT ( 'NONE',  ( 1.614173228346457378, 0.1771653543307087630, 0.000000000000000000 ) ) ;
#65823 = CARTESIAN_POINT ( 'NONE',  ( 0.3917322834645668994, -0.1049643490035303134, -0.03410141912629739008 ) ) ;
#65824 = CARTESIAN_POINT ( 'NONE',  ( 0.5577427821522316087, -0.05778040916215522460, 0.4822834645669289988 ) ) ;
#65825 = CARTESIAN_POINT ( 'NONE',  ( -0.3674540682414692561, -0.5023911411419708095, -0.1820866141732282451 ) ) ;
#65826 = CARTESIAN_POINT ( 'NONE',  ( 1.017060367454068581, -0.05778040916215560624, -0.4822834645669293319 ) ) ;
#65827 = CARTESIAN_POINT ( 'NONE',  ( 0.4986876640419954376, 0.2306618581243848609, 0.2411417322834645549 ) ) ;
#65828 = CARTESIAN_POINT ( 'NONE',  ( -0.4418045515502812548, 1.710866862483978013, -2.103588674771180500 ) ) ;
#65829 = CARTESIAN_POINT ( 'NONE',  ( 0.3996062992125986590, -0.1070741851644053111, -2.788713910761154047 ) ) ;
#65830 = CARTESIAN_POINT ( 'NONE',  ( 0.1049643490035304799, -0.3917322834645670104, -1.184402517881576911 ) ) ;
#65831 = CARTESIAN_POINT ( 'NONE',  ( 1.423884514435696413, -0.3162353388693409650, -0.4822834645669289433 ) ) ;
#65832 = CARTESIAN_POINT ( 'NONE',  ( -0.09842519685039295696, 0.1660481256975883668, -0.3530559997133364547 ) ) ;
#65833 = CARTESIAN_POINT ( 'NONE',  ( -1.548556430446193399, -0.6046776061558809534, -0.2411417322834644161 ) ) ;
#65834 = CARTESIAN_POINT ( 'NONE',  ( 0.9645669291338591078, -0.5400638737290845981, -0.3530559997133363437 ) ) ;
#65835 = CARTESIAN_POINT ( 'NONE',  ( 0.1049643490035304938, -0.3917322834645669549, -0.6423884514435697080 ) ) ;
#65836 = CARTESIAN_POINT ( 'NONE',  ( -0.03280839895013062252, -0.6692913385826771977, 0.1292274648535927661 ) ) ;
#65837 = CARTESIAN_POINT ( 'NONE',  ( 0.8398950131233602345, -0.6046776061558807314, 0.2411417322834647770 ) ) ;
#65838 = CARTESIAN_POINT ( 'NONE',  ( -0.2034120734908128059, 0.2952755905511811885, 0.1292274648535926551 ) ) ;
#65839 = CARTESIAN_POINT ( 'NONE',  ( 1.246719160104987623, -0.004921259842519870586, -0.3153832671262229437 ) ) ;
#65840 = CARTESIAN_POINT ( 'NONE',  ( -1.371391076115484831, 0.2952755905511810774, -0.1292274648535930714 ) ) ;
#65841 = CARTESIAN_POINT ( 'NONE',  ( -1.377952755905511140, 0.2952755905511811885, 0.000000000000000000 ) ) ;
#65842 = CARTESIAN_POINT ( 'NONE',  ( 0.8005249343832027131, 0.05413385826771666132, 0.4176697321401328100 ) ) ;
#65843 = CARTESIAN_POINT ( 'NONE',  ( 0.4091458600556403535, 0.2362204724409449896, -0.5229658792650918597 ) ) ;
#65844 = CARTESIAN_POINT ( 'NONE',  ( 0.2867679344610365999, 0.2867679344610365999, -2.019685039370078261 ) ) ;
#65845 = VERTEX_POINT ( 'NONE', #16748 ) ;
#65846 = CARTESIAN_POINT ( 'NONE',  ( 0.1070741851644053527, 0.3996062992125986590, -0.3083989501312335846 ) ) ;
#65847 = ORIENTED_EDGE ( 'NONE', *, *, #81602, .F. ) ;
#65848 = CARTESIAN_POINT ( 'NONE',  ( 0.9973753280839902091, -0.6046776061558807314, 0.2411417322834647770 ) ) ;
#65849 = CARTESIAN_POINT ( 'NONE',  ( 1.141732283464567566, 0.1771653543307087630, 0.000000000000000000 ) ) ;
#65850 = CARTESIAN_POINT ( 'NONE',  ( 0.5839895013123366230, 0.2952755905511811885, 0.1292274648535926551 ) ) ;
#65851 = CARTESIAN_POINT ( 'NONE',  ( -0.4725553370316754043, 1.494684982616656832, 2.558793778315643586 ) ) ;
#65852 = CARTESIAN_POINT ( 'NONE',  ( 0.01968503937007875723, 0.000000000000000000, 0.000000000000000000 ) ) ;
#65853 = CARTESIAN_POINT ( 'NONE',  ( -0.3392501089628017219, -0.1958661417322836718, -1.239501312335958172 ) ) ;
#65854 = CARTESIAN_POINT ( 'NONE',  ( 1.332020997375328974, -0.05778040916215560624, -0.4822834645669293319 ) ) ;
#65855 = DIRECTION ( 'NONE',  ( 0.000000000000000000, 1.000000000000000000, -0.000000000000000000 ) ) ;
#65856 = CARTESIAN_POINT ( 'NONE',  ( -0.4593175853018366950, 0.05413385826771666132, 0.4176697321401328100 ) ) ;
#65857 = CARTESIAN_POINT ( 'NONE',  ( 1.246719160104987623, -0.4281496062992124485, 0.4176697321401328655 ) ) ;
#65858 = EDGE_LOOP ( 'NONE', ( #45490, #21642, #8277, #18835 ) ) ;
#65859 = CARTESIAN_POINT ( 'NONE',  ( -1.377952755905511140, 0.2952755905511811885, 0.000000000000000000 ) ) ;
#65860 = DIRECTION ( 'NONE',  ( 0.000000000000000000, 8.326672684688674053E-16, 1.000000000000000000 ) ) ;
#65861 = DIRECTION ( 'NONE',  ( -5.551115123125779004E-17, -5.551115123125782702E-17, -1.000000000000000000 ) ) ;
#65862 = FACE_OUTER_BOUND ( 'NONE', #76444, .T. ) ;
#65863 = DIRECTION ( 'NONE',  ( -1.000000000000000000, -3.469446951953613696E-16, 0.000000000000000000 ) ) ;
#65864 = CARTESIAN_POINT ( 'NONE',  ( -0.9514435695538050464, -0.08942795157528024563, -0.3641732283464568787 ) ) ;
#65865 = CARTESIAN_POINT ( 'NONE',  ( -1.515748031496062076, -0.5400638737290844871, 0.3530559997133364547 ) ) ;
#65866 = CARTESIAN_POINT ( 'NONE',  ( 0.4855643044619430415, -0.4281496062992127816, -0.4176697321401328100 ) ) ;
#65867 = ORIENTED_EDGE ( 'NONE', *, *, #82467, .T. ) ;
#65869 = FACE_OUTER_BOUND ( 'NONE', #65532, .T. ) ;
#65868 = FACE_OUTER_BOUND ( 'NONE', #68132, .T. ) ;
#65870 = CARTESIAN_POINT ( 'NONE',  ( -0.8595800524934373854, -0.2845877964562161244, -0.3641732283464567121 ) ) ;
#65871 = CARTESIAN_POINT ( 'NONE',  ( 0.7086614173228353852, -0.1870078740157479769, 0.4822834645669291653 ) ) ;
#65872 = CARTESIAN_POINT ( 'NONE',  ( -1.601049868766403650, -0.6046776061558807314, 0.2411417322834647770 ) ) ;
#65873 = CARTESIAN_POINT ( 'NONE',  ( 0.2867679344610365999, -0.2867679344610365999, -1.280820579231284340 ) ) ;
#65874 = CARTESIAN_POINT ( 'NONE',  ( -0.6692913385826764205, -0.5511811023622047445, 6.969142054262312111E-17 ) ) ;
#65875 = CARTESIAN_POINT ( 'NONE',  ( 1.601049868766404982, -0.6046776061558809534, -0.2411417322834644161 ) ) ;
#65876 = CARTESIAN_POINT ( 'NONE',  ( 0.4824498642376759960, 1.223219560026271499E-15, 0.4445507791589056734 ) ) ;
#65877 = CARTESIAN_POINT ( 'NONE',  ( 0.5839895013123367340, -0.6692913385826773087, -0.1292274648535924053 ) ) ;
#65878 = CARTESIAN_POINT ( 'NONE',  ( -0.8989501312335946848, -0.5511811023622046335, 0.09757992244046803654 ) ) ;
#65879 = CARTESIAN_POINT ( 'NONE',  ( -0.3477690288713905509, -0.5511811023622046335, 0.09757992244046803654 ) ) ;
#65880 = CARTESIAN_POINT ( 'NONE',  ( -0.1181102362204717315, 0.2952755905511811885, 0.000000000000000000 ) ) ;
#65881 = CARTESIAN_POINT ( 'NONE',  ( -1.167979002624671470, -0.004921259842519576551, 0.3153832671262227771 ) ) ;
#65882 = CARTESIAN_POINT ( 'NONE',  ( 0.1049643490035304799, -0.3917322834645670104, -0.08204031315716725503 ) ) ;
#65883 = CARTESIAN_POINT ( 'NONE',  ( 0.7808398950131240079, -0.3162353388693405765, 0.4822834645669290543 ) ) ;
#65884 = EDGE_CURVE ( 'NONE', #41808, #6386, #63000, .T. ) ;
#65885 = CARTESIAN_POINT ( 'NONE',  ( 0.4061203303035133549, 3.421639014772782816E-16, 0.3464511005275203726 ) ) ;
#65886 = CARTESIAN_POINT ( 'NONE',  ( 0.2362204724409449064, 0.4091458600556404646, -1.795931758530183719 ) ) ;
#65887 = CARTESIAN_POINT ( 'NONE',  ( -0.8464566929133852113, -0.5400638737290845981, -0.3530559997133363437 ) ) ;
#65888 = CARTESIAN_POINT ( 'NONE',  ( -0.07874015748031421014, -0.1870078740157480601, -0.3641732283464567677 ) ) ;
#65889 = CARTESIAN_POINT ( 'NONE',  ( -1.174540682414697335, -0.05778040916215522460, 0.4822834645669289988 ) ) ;
#65890 = CARTESIAN_POINT ( 'NONE',  ( 0.9645669291338591078, -0.4536011799217368745, -0.2665933059059886201 ) ) ;
#65891 = CARTESIAN_POINT ( 'NONE',  ( -0.7742782152230965886, -0.004921259842519576551, 0.3153832671262227771 ) ) ;
#65892 = CARTESIAN_POINT ( 'NONE',  ( -1.023622047244094002, -0.1870078740157480879, -0.4822834645669291653 ) ) ;
#65893 = CARTESIAN_POINT ( 'NONE',  ( -1.660104986876639543, -0.05778040916215560624, -0.4822834645669293319 ) ) ;
#65894 = CARTESIAN_POINT ( 'NONE',  ( -1.528871391076114250, -0.6692913385826771977, 0.1292274648535927661 ) ) ;
#65895 = CARTESIAN_POINT ( 'NONE',  ( 0.7677165354330716118, 0.07958543189024071263, -0.2665933059059888421 ) ) ;
#65896 = CARTESIAN_POINT ( 'NONE',  ( 0.4921259842519691285, -0.5400638737290845981, -0.3530559997133363437 ) ) ;
#65897 = CARTESIAN_POINT ( 'NONE',  ( -1.443569553805773564, 0.2306618581243847221, -0.2411417322834647770 ) ) ;
#65898 = CARTESIAN_POINT ( 'NONE',  ( 1.384514435695538337, -0.5511811023622046335, 0.09757992244046803654 ) ) ;
#65899 = ORIENTED_EDGE ( 'NONE', *, *, #4970, .F. ) ;
#65900 = CARTESIAN_POINT ( 'NONE',  ( -9.674558042662122972E-17, 0.3949938075777409963, 0.2381889763779528046 ) ) ;
#65901 = CARTESIAN_POINT ( 'NONE',  ( -1.227034120734907141, -0.5511811023622048555, -0.09757992244046775898 ) ) ;
#65902 = CARTESIAN_POINT ( 'NONE',  ( -0.5643044619422565855, -0.4281496062992124485, 0.4176697321401328655 ) ) ;
#65903 = CARTESIAN_POINT ( 'NONE',  ( 0.8989501312335963501, -0.6692913385826773087, -0.1292274648535924053 ) ) ;
#65904 = CARTESIAN_POINT ( 'NONE',  ( -1.332020997375327642, -0.2845877964562161244, -0.3641732283464567121 ) ) ;
#65905 = CARTESIAN_POINT ( 'NONE',  ( 4.893765752498283308E-17, -0.3996062992125985480, -1.730314960629921517 ) ) ;
#65906 = CARTESIAN_POINT ( 'NONE',  ( -1.620734908136482577, -0.6692913385826773087, -0.1292274648535924053 ) ) ;
#65907 = CARTESIAN_POINT ( 'NONE',  ( 0.5643044619422579178, 0.05413385826771666132, 0.4176697321401328100 ) ) ;
#65908 = CARTESIAN_POINT ( 'NONE',  ( 0.6036745406824154392, 0.2306618581243847221, -0.2411417322834647770 ) ) ;
#65909 = CARTESIAN_POINT ( 'NONE',  ( 1.318897637795276356, 0.1660481256975883668, -0.3530559997133364547 ) ) ;
#65910 = CARTESIAN_POINT ( 'NONE',  ( -0.3996062992125985480, -7.340648628747423112E-17, -1.218503937007874072 ) ) ;
#65911 = CARTESIAN_POINT ( 'NONE',  ( -0.3996062992125987146, 0.1070741851644051862, -1.450131233595800317 ) ) ;
#65912 = CARTESIAN_POINT ( 'NONE',  ( -0.2891555358219911054, 0.2891555358219909388, -0.6496062992125984925 ) ) ;
#65913 =( REPRESENTATION_RELATIONSHIP ('NONE','NONE', #79348, #27201 ) REPRESENTATION_RELATIONSHIP_WITH_TRANSFORMATION ( #34701 )SHAPE_REPRESENTATION_RELATIONSHIP( ) );
#65914 = CARTESIAN_POINT ( 'NONE',  ( 0.3162942679073420527, 1.183613643627707157, -1.704860272166652146 ) ) ;
#65915 = CARTESIAN_POINT ( 'NONE',  ( 0.1640419947506569498, -0.08942795157527998196, 0.3641732283464567121 ) ) ;
#65916 = CARTESIAN_POINT ( 'NONE',  ( -0.4330708661417315697, 0.2952755905511811885, 0.000000000000000000 ) ) ;
#65917 = CARTESIAN_POINT ( 'NONE',  ( 1.286089238845145033, 0.2306618581243848609, 0.2411417322834645549 ) ) ;
#65918 = CARTESIAN_POINT ( 'NONE',  ( 0.3949938075777409408, -0.1058382717557499186, -1.763123359580052396 ) ) ;
#65919 = CARTESIAN_POINT ( 'NONE',  ( 0.2690288713910767848, 0.1771653543307087630, 0.09757992244046791164 ) ) ;
#65920 = CARTESIAN_POINT ( 'NONE',  ( -0.7349081364829387342, -0.6046776061558807314, 0.2411417322834647770 ) ) ;
#65921 = CARTESIAN_POINT ( 'NONE',  ( 1.456692913385827515, 0.2952755905511811885, 0.000000000000000000 ) ) ;
#65922 = CARTESIAN_POINT ( 'NONE',  ( 0.5643044619422579178, 0.05413385826771666132, 0.4176697321401328100 ) ) ;
#65923 = CARTESIAN_POINT ( 'NONE',  ( 0.2362204724409449064, 0.4091458600556404646, -2.191601049868766360 ) ) ;
#65924 = CARTESIAN_POINT ( 'NONE',  ( 0.3922539627124315142, -0.006303098004669925071, -2.755905511811024944 ) ) ;
#65925 = ORIENTED_EDGE ( 'NONE', *, *, #31058, .F. ) ;
#65926 = ORIENTED_EDGE ( 'NONE', *, *, #48857, .T. ) ;
#65927 = CARTESIAN_POINT ( 'NONE',  ( -1.574803149606298636, -0.1870078740157479769, 0.4822834645669291653 ) ) ;
#65929 = CARTESIAN_POINT ( 'NONE',  ( -1.181102362204723644, -0.1870078740157479769, 0.4822834645669291653 ) ) ;
#65928 = CARTESIAN_POINT ( 'NONE',  ( -1.108923884514435132, -0.08942795157528024563, -0.3641732283464568787 ) ) ;
#65930 = CARTESIAN_POINT ( 'NONE',  ( 0.3917322834645668994, 0.1049643490035304522, -2.566909818076428706 ) ) ;
#65931 = CARTESIAN_POINT ( 'NONE',  ( 1.614173228346456712, 2.401574803149606474, -0.1372047244094476703 ) ) ;
#65932 = CARTESIAN_POINT ( 'NONE',  ( 1.541994750656168645, 0.2952755905511810774, -0.1292274648535930714 ) ) ;
#65933 = CARTESIAN_POINT ( 'NONE',  ( -1.384514435695537005, 0.2952755905511811885, 0.1292274648535926551 ) ) ;
#65934 = CARTESIAN_POINT ( 'NONE',  ( -0.1049868766404193215, 0.2306618581243847221, -0.2411417322834647770 ) ) ;
#65935 = AXIS2_PLACEMENT_3D ( 'NONE', #9052, #48166, #73444 ) ;
#65936 = CARTESIAN_POINT ( 'NONE',  ( -1.082677165354329896, -0.5400638737290845981, -0.3530559997133363437 ) ) ;
#65937 = CARTESIAN_POINT ( 'NONE',  ( 0.3392501089628018329, -0.1958661417322834497, -2.704705093666980087 ) ) ;
#65938 = CARTESIAN_POINT ( 'NONE',  ( 0.5774278215223103139, -0.6046776061558809534, -0.2411417322834644161 ) ) ;
#65939 = CARTESIAN_POINT ( 'NONE',  ( -0.2867679344610364334, -0.2867679344610367109, -1.940944881889763884 ) ) ;
#65940 = CARTESIAN_POINT ( 'NONE',  ( -1.049868766404198794, -0.5023911411419708095, 0.1820866141732285504 ) ) ;
#65941 = VERTEX_POINT ( 'NONE', #44436 ) ;
#65942 = CARTESIAN_POINT ( 'NONE',  ( -0.1974969037888706647, 0.3420746716998658843, -2.375328083989501238 ) ) ;
#65943 = EDGE_LOOP ( 'NONE', ( #23477, #14604, #697, #79312 ) ) ;
#65944 = DIRECTION ( 'NONE',  ( 0.000000000000000000, 0.000000000000000000, -1.000000000000000000 ) ) ;
#65945 = CARTESIAN_POINT ( 'NONE',  ( -0.9448818897637790704, -0.1870078740157479769, 0.4822834645669291653 ) ) ;
#65946 = CARTESIAN_POINT ( 'NONE',  ( -1.509186351706035767, -0.4281496062992124485, 0.4176697321401328655 ) ) ;
#65947 = CARTESIAN_POINT ( 'NONE',  ( -0.1070741851644056997, 0.3996062992125986035, -0.4790026246719158998 ) ) ;
#65948 = CARTESIAN_POINT ( 'NONE',  ( -1.364829396325458521, 0.2306618581243847221, -0.2411417322834647770 ) ) ;
#65949 = CARTESIAN_POINT ( 'NONE',  ( -1.502624671916009680, -0.05778040916215560624, -0.4822834645669293319 ) ) ;
#65950 = CARTESIAN_POINT ( 'NONE',  ( -1.299212598425196097, 0.2952755905511811885, 0.000000000000000000 ) ) ;
#65951 = CARTESIAN_POINT ( 'NONE',  ( -0.7773926554473638006, -2.191421614605370878E-15, 0.4445507791589071167 ) ) ;
#65952 = CARTESIAN_POINT ( 'NONE',  ( 0.3503937007874015630, -0.5120078740157480990, 0.000000000000000000 ) ) ;
#65953 = CARTESIAN_POINT ( 'NONE',  ( 0.1968503937007881344, -0.5511811023622047445, 6.969142054262312111E-17 ) ) ;
#65954 = CARTESIAN_POINT ( 'NONE',  ( -0.1049643490035307020, 0.3917322834645669549, -0.7211286089238846397 ) ) ;
#65955 = CARTESIAN_POINT ( 'NONE',  ( -0.6167979002624665030, -0.004921259842519576551, 0.3153832671262227771 ) ) ;
#65956 = CARTESIAN_POINT ( 'NONE',  ( -1.240157480314959759, -0.5400638737290845981, -0.3530559997133363437 ) ) ;
#65957 = CARTESIAN_POINT ( 'NONE',  ( 1.135170603674541256, 0.2952755905511811885, 0.1292274648535926551 ) ) ;
#65958 = CARTESIAN_POINT ( 'NONE',  ( -1.122047244094487306, 0.1660481256975883668, -0.3530559997133364547 ) ) ;
#65959 = CARTESIAN_POINT ( 'NONE',  ( -0.2867679344610365999, 0.2867679344610364889, 0.1456692913385827237 ) ) ;
#65960 = VERTEX_POINT ( 'NONE', #68899 ) ;
#65961 = CARTESIAN_POINT ( 'NONE',  ( -0.8858267716535425107, -0.5400638737290844871, 0.3530559997133364547 ) ) ;
#65962 = CARTESIAN_POINT ( 'NONE',  ( 0.9711286089238851948, 0.2306618581243848609, 0.2411417322834645549 ) ) ;
#65963 = CARTESIAN_POINT ( 'NONE',  ( -1.679790026246718693, 0.1283753931104746893, -0.1820866141732285504 ) ) ;
#65964 = CARTESIAN_POINT ( 'NONE',  ( -1.706036745406823485, 0.2306618581243848609, 0.2411417322834645549 ) ) ;
#65965 = CARTESIAN_POINT ( 'NONE',  ( -0.2362204724409451284, 0.4091458600556402425, -1.115485564304461885 ) ) ;
#65966 = CARTESIAN_POINT ( 'NONE',  ( 1.854728618660368422, 1.067671560069314296, 0.06860298820095168948 ) ) ;
#65967 = CARTESIAN_POINT ( 'NONE',  ( 0.3392501089628018329, 0.1958661417322835607, -0.4383202099737532609 ) ) ;
#65968 = CARTESIAN_POINT ( 'NONE',  ( -0.3392501089628019995, 0.1958661417322832277, -2.473097112860892288 ) ) ;
#65969 = CARTESIAN_POINT ( 'NONE',  ( -0.4986876640419939388, 0.2306618581243847221, -0.2411417322834647770 ) ) ;
#65970 = CARTESIAN_POINT ( 'NONE',  ( -1.548556430446193399, -0.5023911411419708095, -0.1820866141732282451 ) ) ;
#65971 = CARTESIAN_POINT ( 'NONE',  ( 0.3460692066303959202, -0.1998031496062991630, -0.02427821522309713681 ) ) ;
#65973 = DIRECTION ( 'NONE',  ( -0.7071067811865524577, 0.000000000000000000, 0.7071067811865425767 ) ) ;
#65972 = CARTESIAN_POINT ( 'NONE',  ( -1.332020997375327642, -0.3162353388693409650, -0.4822834645669289433 ) ) ;
#65974 = CARTESIAN_POINT ( 'NONE',  ( -1.528871391076114250, 0.2952755905511810774, -0.1292274648535930714 ) ) ;
#65975 = CARTESIAN_POINT ( 'NONE',  ( -0.4461942257217840213, 0.2306618581243848609, 0.2411417322834645549 ) ) ;
#65976 = CARTESIAN_POINT ( 'NONE',  ( -0.3949938075777411073, 0.1058382717557497660, -2.471784776902887337 ) ) ;
#65977 = CARTESIAN_POINT ( 'NONE',  ( 0.6233595800524939223, -0.2845877964562159024, 0.3641732283464567677 ) ) ;
#65978 = CARTESIAN_POINT ( 'NONE',  ( 0.1771653543307086798, 0.000000000000000000, 0.000000000000000000 ) ) ;
#65979 = CARTESIAN_POINT ( 'NONE',  ( 0.4330708661417329575, 0.1771653543307087630, 0.000000000000000000 ) ) ;
#65980 = CARTESIAN_POINT ( 'NONE',  ( 1.417322834645670104, -0.1870078740157479769, 0.3641732283464567677 ) ) ;
#65981 = CARTESIAN_POINT ( 'NONE',  ( 0.7611548556430451917, -0.6046776061558807314, 0.2411417322834647770 ) ) ;
#65982 = CARTESIAN_POINT ( 'NONE',  ( 0.3215223097112867578, -0.2845877964562161244, -0.3641732283464567121 ) ) ;
#65983 = CARTESIAN_POINT ( 'NONE',  ( -0.1958661417322836718, 0.3392501089628017219, -2.052493438320210029 ) ) ;
#65984 = CARTESIAN_POINT ( 'NONE',  ( -1.266404199475064773, -0.05778040916215560624, -0.4822834645669293319 ) ) ;
#65985 = CARTESIAN_POINT ( 'NONE',  ( -0.1509186351706028884, -0.08942795157527998196, 0.3641732283464567121 ) ) ;
#65986 = CARTESIAN_POINT ( 'NONE',  ( -1.082677165354329896, -0.4536011799217368745, -0.2665933059059886201 ) ) ;
#65987 = CARTESIAN_POINT ( 'NONE',  ( -0.1265901696524993347, 0.4724409448818895907, -0.3982939632545932085 ) ) ;
#65988 = CARTESIAN_POINT ( 'NONE',  ( -0.4265091863517051496, -0.5511811023622046335, 0.09757992244046803654 ) ) ;
#65989 = CARTESIAN_POINT ( 'NONE',  ( 0.4497368882408442348, 1.386401378945496532, -1.551431943024248472 ) ) ;
#65990 = CARTESIAN_POINT ( 'NONE',  ( 0.09186351706036827158, 0.05413385826771666132, 0.4176697321401328100 ) ) ;
#65991 = DIRECTION ( 'NONE',  ( 0.000000000000000000, -1.000000000000000000, 0.000000000000000000 ) ) ;
#65992 = CARTESIAN_POINT ( 'NONE',  ( 0.4790026246719167324, -0.08942795157527998196, 0.3641732283464567121 ) ) ;
#65993 = CARTESIAN_POINT ( 'NONE',  ( -0.3346456692913377662, -0.4536011799217367080, 0.2665933059059888421 ) ) ;
#65994 = CARTESIAN_POINT ( 'NONE',  ( -0.4068241469816264999, -0.4281496062992124485, 0.4176697321401328655 ) ) ;
#65995 = CARTESIAN_POINT ( 'NONE',  ( -1.692913385826770645, 0.2952755905511811885, 0.000000000000000000 ) ) ;
#65996 = CARTESIAN_POINT ( 'NONE',  ( -1.122047244094487306, 0.07958543189024071263, -0.2665933059059888421 ) ) ;
#65997 = DIRECTION ( 'NONE',  ( -1.000000000000000000, -3.050063254464715288E-16, 0.000000000000000000 ) ) ;
#65998 = CARTESIAN_POINT ( 'NONE',  ( 0.5183727034120741983, -0.6692913385826771977, 0.1292274648535927661 ) ) ;
#65999 = CARTESIAN_POINT ( 'NONE',  ( -0.9251968503937002541, -0.5400638737290845981, -0.3530559997133363437 ) ) ;
#66000 = CARTESIAN_POINT ( 'NONE',  ( 0.2925321140481932369, 0.2925321140481932369, -1.474409448818897683 ) ) ;
#66001 = CARTESIAN_POINT ( 'NONE',  ( -0.2867679344610364334, -0.2867679344610367109, -2.820866141732283339 ) ) ;
#66002 = CARTESIAN_POINT ( 'NONE',  ( -0.3805774278215216522, -0.3690944881889765550, -0.3153832671262227771 ) ) ;
#66003 = CARTESIAN_POINT ( 'NONE',  ( 2.787279214012418738, 1.496062992125984481, 0.000000000000000000 ) ) ;
#66004 = CARTESIAN_POINT ( 'NONE',  ( -1.082677165354329896, -0.4536011799217368745, -0.2665933059059886201 ) ) ;
#66005 = CARTESIAN_POINT ( 'NONE',  ( 1.601049868766404982, -0.6046776061558809534, -0.2411417322834644161 ) ) ;
#66006 =( BOUNDED_CURVE ( )  B_SPLINE_CURVE ( 2, ( #25091, #76866, #82769, #19198, #70545, #38144, #6155, #56262, #30998, #44036, #55839, #81548, #23866 ),
 .UNSPECIFIED., .F., .F. ) 
 B_SPLINE_CURVE_WITH_KNOTS ( ( 3, 2, 2, 2, 2, 2, 3 ),
 ( 0.8125000000000000000, 0.8166666666666666519, 0.8208333333333333037, 0.8249999999999999556, 0.8291666666666667185, 0.8333333333333333703, 0.8375000000000000222 ),
 .UNSPECIFIED. ) 
 CURVE ( )  GEOMETRIC_REPRESENTATION_ITEM ( )  RATIONAL_B_SPLINE_CURVE ( ( 1.000000000000000000, 0.9659258262890683122, 1.000000000000000000, 0.9659258262890683122, 1.000000000000000000, 0.9659258262890683122, 1.000000000000000000, 0.9659258262890683122, 1.000000000000000000, 0.9659258262890683122, 1.000000000000000000, 0.9659258262890683122, 1.000000000000000000 ) ) 
 REPRESENTATION_ITEM ( '' )  );
#66007 = CARTESIAN_POINT ( 'NONE',  ( -0.8202099737532801971, -0.5511811023622046335, 0.09757992244046803654 ) ) ;
#66008 = CARTESIAN_POINT ( 'NONE',  ( -0.7210809602247715278, -2.613618158232546091E-15, -0.3464511005275220379 ) ) ;
#66009 = CARTESIAN_POINT ( 'NONE',  ( 0.8595800524934390507, -0.05778040916215560624, -0.4822834645669293319 ) ) ;
#66010 = CARTESIAN_POINT ( 'NONE',  ( 0.3460692066303959757, -0.1998031496062991907, -0.1049868766404199599 ) ) ;
#66011 = CARTESIAN_POINT ( 'NONE',  ( 0.3917322834645670104, 0.1049643490035304660, -2.326134801346143366 ) ) ;
#66012 = AXIS2_PLACEMENT_3D ( 'NONE', #76973, #62689, #11774 ) ;
#66013 = CARTESIAN_POINT ( 'NONE',  ( 0.4744094488189065095, 1.537401574803149984, -2.554262525012259477 ) ) ;
#66014 = EDGE_CURVE ( 'NONE', #26718, #40163, #44847, .T. ) ;
#66015 = CARTESIAN_POINT ( 'NONE',  ( -1.692913385826770645, 0.2952755905511811885, 0.000000000000000000 ) ) ;
#66016 = CARTESIAN_POINT ( 'NONE',  ( -1.089238845144356427, 0.05413385826771666132, 0.4176697321401328100 ) ) ;
#66017 = CARTESIAN_POINT ( 'NONE',  ( 1.128608923884514947, 0.2306618581243848609, 0.2411417322834645549 ) ) ;
#66018 = CARTESIAN_POINT ( 'NONE',  ( 0.1049643490035303689, 0.3917322834645670104, -2.282808398950130879 ) ) ;
#66019 = CARTESIAN_POINT ( 'NONE',  ( 1.502624671916010790, -0.08942795157527998196, 0.3641732283464567121 ) ) ;
#66020 = EDGE_CURVE ( 'NONE', #43096, #55729, #49749, .T. ) ;
#66021 = CARTESIAN_POINT ( 'NONE',  ( 0.4593175853018380828, 0.05413385826771626580, -0.4176697321401330321 ) ) ;
#66022 = CARTESIAN_POINT ( 'NONE',  ( -0.1902887139107604098, 0.2952755905511810774, -0.1292274648535930714 ) ) ;
#66023 = CARTESIAN_POINT ( 'NONE',  ( 1.502624671916010790, -0.05778040916215522460, 0.4822834645669289988 ) ) ;
#66024 = CARTESIAN_POINT ( 'NONE',  ( 0.8267716535433077274, 0.1771653543307087630, 0.000000000000000000 ) ) ;
#66025 = ORIENTED_EDGE ( 'NONE', *, *, #36840, .F. ) ;
#66026 = CARTESIAN_POINT ( 'NONE',  ( 0.1958661417322836718, -0.3392501089628017219, -0.5610429378290832103 ) ) ;
#66027 = ORIENTED_EDGE ( 'NONE', *, *, #35630, .T. ) ;
#66028 = CARTESIAN_POINT ( 'NONE',  ( -0.2690288713910754526, 0.2952755905511810774, -0.1292274648535930714 ) ) ;
#66029 = CARTESIAN_POINT ( 'NONE',  ( 1.318897637795276356, 0.1660481256975883668, -0.3530559997133364547 ) ) ;
#66030 = CARTESIAN_POINT ( 'NONE',  ( 0.1049868766404206816, 0.2306618581243848609, 0.2411417322834645549 ) ) ;
#66031 = CARTESIAN_POINT ( 'NONE',  ( -0.5183727034120726440, 0.1771653543307087630, 0.09757992244046791164 ) ) ;
#66032 = CARTESIAN_POINT ( 'NONE',  ( 1.286089238845145033, -0.6046776061558809534, -0.2411417322834644161 ) ) ;
#66033 = CARTESIAN_POINT ( 'NONE',  ( -1.102362204724408601, -0.1870078740157480879, -0.4822834645669291653 ) ) ;
#66034 = CARTESIAN_POINT ( 'NONE',  ( 0.03937007874015806264, 0.2952755905511811885, 0.000000000000000000 ) ) ;
#66035 = CARTESIAN_POINT ( 'NONE',  ( 1.515748031496063186, -0.5400638737290845981, -0.3530559997133363437 ) ) ;
#66036 = CARTESIAN_POINT ( 'NONE',  ( 1.003937007874016185, 0.1660481256975883668, -0.3530559997133364547 ) ) ;
#66037 = CARTESIAN_POINT ( 'NONE',  ( 1.102362204724410155, -0.1870078740157480879, -0.4822834645669291653 ) ) ;
#66038 = EDGE_CURVE ( 'NONE', #2797, #23246, #66006, .T. ) ;
#66039 = CARTESIAN_POINT ( 'NONE',  ( 0.3392501089628018329, 0.1958661417322835607, -0.4383202099737532609 ) ) ;
#66040 = CARTESIAN_POINT ( 'NONE',  ( 0.05905511811023709395, -0.4536011799217367080, 0.2665933059059888421 ) ) ;
#66041 = ORIENTED_EDGE ( 'NONE', *, *, #20353, .T. ) ;
#66042 = CARTESIAN_POINT ( 'NONE',  ( 0.3949938075777411073, -0.1058382717557499464, -0.8989501312335956840 ) ) ;
#66043 = ORIENTED_EDGE ( 'NONE', *, *, #83060, .F. ) ;
#66044 = CARTESIAN_POINT ( 'NONE',  ( -0.3215223097112853146, -0.2845877964562159024, 0.3641732283464567677 ) ) ;
#66045 = CARTESIAN_POINT ( 'NONE',  ( 0.04593175853018440641, -0.6692913385826771977, 0.1292274648535927661 ) ) ;
#66046 = DIRECTION ( 'NONE',  ( -0.000000000000000000, -1.000000000000000000, 0.000000000000000000 ) ) ;
#66047 = CARTESIAN_POINT ( 'NONE',  ( -0.4133858267716528645, 0.1660481256975883668, -0.3530559997133364547 ) ) ;
#66048 = CARTESIAN_POINT ( 'NONE',  ( -0.3674540682414692561, -0.6046776061558809534, -0.2411417322834644161 ) ) ;
#66049 = ADVANCED_FACE ( 'NONE', ( #81958 ), #50831, .F. ) ;
#66050 = CARTESIAN_POINT ( 'NONE',  ( -0.7152230971128602510, -0.3162353388693405765, 0.4822834645669290543 ) ) ;
#66051 = CARTESIAN_POINT ( 'NONE',  ( -1.003937007874015297, -0.5400638737290845981, -0.3530559997133363437 ) ) ;
#66052 = CARTESIAN_POINT ( 'NONE',  ( 1.509186351706037543, -0.004921259842519576551, 0.3153832671262227771 ) ) ;
#66053 = FACE_OUTER_BOUND ( 'NONE', #30555, .T. ) ;
#66054 = CARTESIAN_POINT ( 'NONE',  ( -0.4724409448818898682, -8.678599364036362592E-17, -2.716535433070865757 ) ) ;
#66055 = CARTESIAN_POINT ( 'NONE',  ( 0.4002624671916016896, -0.2845877964562161244, -0.3641732283464567121 ) ) ;
#66056 = CARTESIAN_POINT ( 'NONE',  ( 0.4265091863517067594, 0.2952755905511811885, 0.1292274648535926551 ) ) ;
#66057 = CARTESIAN_POINT ( 'NONE',  ( 0.5183727034120741983, -0.6692913385826771977, 0.1292274648535927661 ) ) ;
#66058 = CIRCLE ( 'NONE', #24339, 0.2165354330708661457 ) ;
#66059 = CARTESIAN_POINT ( 'NONE',  ( -0.3996062992125986035, -7.340648628747425578E-17, -1.141732283464566899 ) ) ;
#66060 = CARTESIAN_POINT ( 'NONE',  ( 0.3249695492770460770, 1.223219560026271499E-15, 0.4445507791589056734 ) ) ;
#66061 = CARTESIAN_POINT ( 'NONE',  ( 0.2925321140481932369, 0.2925321140481932369, -0.8444881889763780070 ) ) ;
#66062 = CARTESIAN_POINT ( 'NONE',  ( -0.3996062992125985480, -7.340648628747423112E-17, -0.7460629921259841479 ) ) ;
#66063 = CARTESIAN_POINT ( 'NONE',  ( -0.5446194225721777693, -0.3162353388693409650, -0.4822834645669289433 ) ) ;
#66064 = CARTESIAN_POINT ( 'NONE',  ( 0.4724409448818898682, 2.892866454678787531E-17, -0.1181102362204724532 ) ) ;
#66065 = CARTESIAN_POINT ( 'NONE',  ( 0.3392501089628018329, 0.1958661417322835607, -2.105643044619422533 ) ) ;
#66066 = CARTESIAN_POINT ( 'NONE',  ( -1.364829396325458521, -0.5023911411419708095, 0.1820866141732285504 ) ) ;
#66067 = CARTESIAN_POINT ( 'NONE',  ( 0.9251968503937015864, -0.5400638737290844871, 0.3530559997133364547 ) ) ;
#66068 = CARTESIAN_POINT ( 'NONE',  ( 0.8267716535433078384, -0.6692913385826771977, 8.415575281601705876E-17 ) ) ;
#66069 = CARTESIAN_POINT ( 'NONE',  ( -0.1377952755905504645, -0.4536011799217368745, -0.2665933059059886201 ) ) ;
#66070 = CARTESIAN_POINT ( 'NONE',  ( 0.5314960629921264834, 0.1660481256975883668, -0.3530559997133364547 ) ) ;
#66071 = CARTESIAN_POINT ( 'NONE',  ( -0.1265901696524993347, 0.4724409448818895907, -1.973097112860892510 ) ) ;
#66072 = CARTESIAN_POINT ( 'NONE',  ( -0.1771653543307080136, 0.07958543189024071263, -0.2665933059059888421 ) ) ;
#66073 = CARTESIAN_POINT ( 'NONE',  ( -0.05249343832020938322, -0.6046776061558809534, -0.2411417322834644161 ) ) ;
#66074 = CARTESIAN_POINT ( 'NONE',  ( 0.3949938075777409408, -0.1058382717557499186, -1.605643044619423199 ) ) ;
#66075 = CARTESIAN_POINT ( 'NONE',  ( -1.561679790026246017, 0.05413385826771666132, 0.4176697321401328100 ) ) ;
#66076 = CARTESIAN_POINT ( 'NONE',  ( 0.4855643044619428750, -0.004921259842519576551, 0.3153832671262227771 ) ) ;
#66077 = CARTESIAN_POINT ( 'NONE',  ( 1.509186351706037543, -0.004921259842519576551, 0.3153832671262227771 ) ) ;
#66078 = CARTESIAN_POINT ( 'NONE',  ( -0.7217847769028863381, 0.05413385826771626580, -0.4176697321401330321 ) ) ;
#66079 = CARTESIAN_POINT ( 'NONE',  ( -0.7152230971128602510, -0.2845877964562159024, 0.3641732283464567677 ) ) ;
#66080 = LINE ( 'NONE', #54256, #48033 ) ;
#66081 = CARTESIAN_POINT ( 'NONE',  ( -0.8530183727034112984, -0.4281496062992127816, -0.4176697321401328100 ) ) ;
#66082 = CARTESIAN_POINT ( 'NONE',  ( -0.6889763779527552368, 0.1660481256975885056, 0.3530559997133364547 ) ) ;
#66083 = CARTESIAN_POINT ( 'NONE',  ( -0.1837270341207340729, 0.2306618581243847221, -0.2411417322834647770 ) ) ;
#66084 = CARTESIAN_POINT ( 'NONE',  ( -0.1998031496062991630, -0.3460692066303959202, -2.504593175853018661 ) ) ;
#66085 = CARTESIAN_POINT ( 'NONE',  ( -0.2867679344610364334, -0.2867679344610368219, -2.186332390254906777 ) ) ;
#66086 = CARTESIAN_POINT ( 'NONE',  ( 0.5314960629920849611, 2.682389230697235671, 3.900966923095593675 ) ) ;
#66087 = CARTESIAN_POINT ( 'NONE',  ( 0.8005249343832028242, -0.3690944881889765550, -0.3153832671262227771 ) ) ;
#66088 = EDGE_CURVE ( 'NONE', #21419, #20068, #62169, .T. ) ;
#66089 = CARTESIAN_POINT ( 'NONE',  ( 1.187664041994751285, -0.3162353388693409650, -0.4822834645669289433 ) ) ;
#66090 = CARTESIAN_POINT ( 'NONE',  ( -1.312335958005248715, -0.5023911411419708095, -0.1820866141732282451 ) ) ;
#66091 = CARTESIAN_POINT ( 'NONE',  ( -1.292650918635170010, -0.5511811023622046335, 0.09757992244046803654 ) ) ;
#66092 = CARTESIAN_POINT ( 'NONE',  ( -0.7152230971128602510, -0.05778040916215560624, -0.4822834645669293319 ) ) ;
#66093 = CARTESIAN_POINT ( 'NONE',  ( -0.04593175853018302557, 0.1771653543307087630, 0.09757992244046791164 ) ) ;
#66094 = CARTESIAN_POINT ( 'NONE',  ( -0.4724409448818896462, -0.1265901696524993070, -0.8333333333333332593 ) ) ;
#66095 = CARTESIAN_POINT ( 'NONE',  ( 0.9120734908136489683, -0.5511811023622046335, 0.09757992244046803654 ) ) ;
#66096 = EDGE_CURVE ( 'NONE', #9504, #76416, #75642, .T. ) ;
#66097 = CARTESIAN_POINT ( 'NONE',  ( 0.2427821522309719648, -0.05778040916215522460, 0.4822834645669289988 ) ) ;
#66098 = CARTESIAN_POINT ( 'NONE',  ( -0.2925321140481932369, 0.2925321140481931259, -0.2539370078740156855 ) ) ;
#66099 = CARTESIAN_POINT ( 'NONE',  ( -0.4921259842519677963, -0.5400638737290844871, 0.3530559997133364547 ) ) ;
#66100 = CARTESIAN_POINT ( 'NONE',  ( 0.3392501089628018884, -0.1958661417322834220, -1.449475065616798064 ) ) ;
#66101 = CARTESIAN_POINT ( 'NONE',  ( 1.496062992125984703, -0.1870078740157480601, -0.3641732283464567677 ) ) ;
#66102 = CARTESIAN_POINT ( 'NONE',  ( 0.3543307086614181922, -0.6692913385826771977, 8.415575281601705876E-17 ) ) ;
#66103 = CARTESIAN_POINT ( 'NONE',  ( -0.01968503937007793844, 0.1660481256975883668, -0.3530559997133364547 ) ) ;
#66104 = CARTESIAN_POINT ( 'NONE',  ( 0.05249343832021075018, -0.5023911411419708095, 0.1820866141732285504 ) ) ;
#66105 = DIRECTION ( 'NONE',  ( 0.000000000000000000, -1.000000000000000000, 0.000000000000000000 ) ) ;
#66106 = CARTESIAN_POINT ( 'NONE',  ( -0.1115485564304453947, -0.5511811023622046335, 0.09757992244046803654 ) ) ;
#66107 = CARTESIAN_POINT ( 'NONE',  ( 0.9448818897637802916, -0.1870078740157480879, -0.4822834645669291653 ) ) ;
#66108 = CARTESIAN_POINT ( 'NONE',  ( -0.7742782152230965886, -0.004921259842519576551, 0.3153832671262227771 ) ) ;
#66109 = CARTESIAN_POINT ( 'NONE',  ( 0.3460692066303958092, 0.1998031496062993018, -0.9954068241469815614 ) ) ;
#66110 = CARTESIAN_POINT ( 'NONE',  ( -1.154855643044618851, 0.2306618581243848609, 0.2411417322834645549 ) ) ;
#66111 = CARTESIAN_POINT ( 'NONE',  ( -0.8561328129276786214, -2.191421614605370878E-15, 0.4445507791589071167 ) ) ;
#66112 = VERTEX_POINT ( 'NONE', #63404 ) ;
#66113 = CARTESIAN_POINT ( 'NONE',  ( -1.056430446194224881, -0.6692913385826771977, 0.1292274648535927661 ) ) ;
#66114 = CARTESIAN_POINT ( 'NONE',  ( -1.003937007874015297, -0.4536011799217368745, -0.2665933059059886201 ) ) ;
#66115 = CARTESIAN_POINT ( 'NONE',  ( 0.02624671916010564918, 0.2306618581243848609, 0.2411417322834645549 ) ) ;
#66116 = DIRECTION ( 'NONE',  ( 0.000000000000000000, -0.000000000000000000, 1.000000000000000000 ) ) ;
#66117 = CARTESIAN_POINT ( 'NONE',  ( -0.9514435695538050464, -0.05778040916215560624, -0.4822834645669293319 ) ) ;
#66118 = DIRECTION ( 'NONE',  ( -0.000000000000000000, -1.000000000000000000, -0.000000000000000000 ) ) ;
#66120 = CARTESIAN_POINT ( 'NONE',  ( 1.062992125984252745, -0.6692913385826771977, 8.415575281601705876E-17 ) ) ;
#66119 = CARTESIAN_POINT ( 'NONE',  ( 1.594488188976378673, -0.5400638737290845981, -0.3530559997133363437 ) ) ;
#66121 = CARTESIAN_POINT ( 'NONE',  ( 0.9711286089238851948, -0.6046776061558809534, -0.2411417322834644161 ) ) ;
#66122 = CARTESIAN_POINT ( 'NONE',  ( -0.3025410870193214197, 0.000000000000000000, 0.3464511005275205946 ) ) ;
#66123 = CARTESIAN_POINT ( 'NONE',  ( 1.561679790026247350, -0.4281496062992124485, 0.4176697321401328655 ) ) ;
#66124 = CARTESIAN_POINT ( 'NONE',  ( -1.299212598425196097, -0.6692913385826771977, 8.415575281601705876E-17 ) ) ;
#66125 = CARTESIAN_POINT ( 'NONE',  ( -0.3460692066303958092, -0.1998031496062994683, -0.6824146981627295938 ) ) ;
#66126 = VERTEX_POINT ( 'NONE', #17981 ) ;
#66127 = CARTESIAN_POINT ( 'NONE',  ( -0.6299212598425188991, -0.1870078740157480601, -0.3641732283464567677 ) ) ;
#66128 = CARTESIAN_POINT ( 'NONE',  ( -0.1049643490035307020, 0.3917322834645669549, -2.045931758530183497 ) ) ;
#66129 = ORIENTED_EDGE ( 'NONE', *, *, #52104, .F. ) ;
#66130 = CARTESIAN_POINT ( 'NONE',  ( 0.1443569553805781891, -0.4281496062992124485, 0.4176697321401328655 ) ) ;
#66131 = CARTESIAN_POINT ( 'NONE',  ( 0.1312335958005255154, -0.6046776061558807314, 0.2411417322834647770 ) ) ;
#66132 = CARTESIAN_POINT ( 'NONE',  ( -0.8398950131233585692, 0.2306618581243848609, 0.2411417322834645549 ) ) ;
#66133 = CARTESIAN_POINT ( 'NONE',  ( 1.692913385826772421, 0.2952755905511811885, 0.000000000000000000 ) ) ;
#66134 = CARTESIAN_POINT ( 'NONE',  ( -1.049868766404198794, -0.5023911411419708095, 0.1820866141732285504 ) ) ;
#66135 = CARTESIAN_POINT ( 'NONE',  ( 0.02109673867167633637, 1.063447502424408775, -1.617503877632567422 ) ) ;
#66136 = CARTESIAN_POINT ( 'NONE',  ( 0.6167979002624679463, 0.05413385826771626580, -0.4176697321401330321 ) ) ;
#66137 = CARTESIAN_POINT ( 'NONE',  ( 0.5971128608923890191, -0.5511811023622046335, 0.09757992244046803654 ) ) ;
#66138 = CARTESIAN_POINT ( 'NONE',  ( -0.4593175853018364174, -0.4281496062992127816, -0.4176697321401328100 ) ) ;
#66139 = CARTESIAN_POINT ( 'NONE',  ( 0.1958661417322834497, 0.3392501089628018329, -1.169272022800837973 ) ) ;
#66140 = CARTESIAN_POINT ( 'NONE',  ( -1.194225721784776262, -0.4281496062992124485, 0.4176697321401328655 ) ) ;
#66141 = LINE ( 'NONE', #8479, #64070 ) ;
#66142 =( BOUNDED_CURVE ( )  B_SPLINE_CURVE ( 2, ( #51658, #57564, #19694, #71465, #71048, #7068, #58832, #52078, #78207, #39471, #1190, #20539, #65583 ),
 .UNSPECIFIED., .F., .F. ) 
 B_SPLINE_CURVE_WITH_KNOTS ( ( 3, 2, 2, 2, 2, 2, 3 ),
 ( 0.5824220037257099580, 0.5833333333333333703, 0.5871212121212121549, 0.5909090909090909394, 0.5946969696969697239, 0.5984848484848485084, 0.5993961780924720317 ),
 .UNSPECIFIED. ) 
 CURVE ( )  GEOMETRIC_REPRESENTATION_ITEM ( )  RATIONAL_B_SPLINE_CURVE ( ( 0.9875488213027523443, 0.9918020599134680371, 1.000000000000000000, 0.9659258262890683122, 1.000000000000000000, 0.9659258262890683122, 1.000000000000000000, 0.9659258262890683122, 1.000000000000000000, 0.9659258262890683122, 1.000000000000000000, 0.9918020599134671489, 0.9875488213027514561 ) ) 
 REPRESENTATION_ITEM ( '' )  );
#66143 = CARTESIAN_POINT ( 'NONE',  ( 1.325459317585302665, -0.4281496062992124485, 0.4176697321401328655 ) ) ;
#66144 = CARTESIAN_POINT ( 'NONE',  ( -0.4672625608940637609, 1.453874696264121802, -2.153215735734194336 ) ) ;
#66145 = VERTEX_POINT ( 'NONE', #69319 ) ;
#66146 = CARTESIAN_POINT ( 'NONE',  ( 0.3392501089628018329, 0.1958661417322835607, -2.490176796096799539 ) ) ;
#66147 = CARTESIAN_POINT ( 'NONE',  ( 0.1902887139107617975, -0.6692913385826773087, -0.1292274648535924053 ) ) ;
#66148 = ORIENTED_EDGE ( 'NONE', *, *, #733, .T. ) ;
#66149 = CARTESIAN_POINT ( 'NONE',  ( 0.9251968503937015864, -0.4536011799217367080, 0.2665933059059888421 ) ) ;
#66150 = CARTESIAN_POINT ( 'NONE',  ( -1.312335958005248715, -0.6046776061558809534, -0.2411417322834644161 ) ) ;
#66151 = CARTESIAN_POINT ( 'NONE',  ( 1.181102362204724976, -0.1870078740157480879, -0.4822834645669291653 ) ) ;
#66152 = CARTESIAN_POINT ( 'NONE',  ( 0.6692913385826777528, 0.2952755905511811885, 0.000000000000000000 ) ) ;
#66153 = CARTESIAN_POINT ( 'NONE',  ( 0.3805774278215230400, 0.05413385826771626580, -0.4176697321401330321 ) ) ;
#66154 = CARTESIAN_POINT ( 'NONE',  ( -0.2755905511811015396, -0.6692913385826771977, 8.415575281601705876E-17 ) ) ;
#66155 = CARTESIAN_POINT ( 'NONE',  ( -0.1958661417322834220, -0.3392501089628018884, -1.882545931758530244 ) ) ;
#66156 = CARTESIAN_POINT ( 'NONE',  ( -1.272965879265091305, -0.4281496062992124485, 0.4176697321401328655 ) ) ;
#66157 = CARTESIAN_POINT ( 'NONE',  ( -0.4658792650918627265, -0.3162353388693409650, -0.4822834645669289433 ) ) ;
#66158 = CARTESIAN_POINT ( 'NONE',  ( -0.5511811023622038563, -0.1870078740157479769, 0.3641732283464567677 ) ) ;
#66159 = CARTESIAN_POINT ( 'NONE',  ( 1.692913385826772421, 0.2952755905511811885, 0.000000000000000000 ) ) ;
#66160 = CARTESIAN_POINT ( 'NONE',  ( 1.646981627296588035, -0.3162353388693405765, 0.4822834645669290543 ) ) ;
#66161 = CARTESIAN_POINT ( 'NONE',  ( -0.3805774278215216522, -0.4281496062992127816, -0.4176697321401328100 ) ) ;
#66162 = CARTESIAN_POINT ( 'NONE',  ( 0.4724409448818898682, 0.000000000000000000, -2.755905511811024056 ) ) ;
#66163 = CARTESIAN_POINT ( 'NONE',  ( 0.8398950131233602345, 0.2306618581243847221, -0.2411417322834647770 ) ) ;
#66164 = CARTESIAN_POINT ( 'NONE',  ( 0.3996062992125986590, -0.1070741851644053111, -1.686351706036745446 ) ) ;
#66165 = DIRECTION ( 'NONE',  ( 0.000000000000000000, -1.000000000000000000, -0.000000000000000000 ) ) ;
#66166 = CARTESIAN_POINT ( 'NONE',  ( -0.1640419947506553400, -0.05778040916215560624, -0.4822834645669293319 ) ) ;
#66168 = DIRECTION ( 'NONE',  ( -0.000000000000000000, -1.000000000000000000, -0.000000000000000000 ) ) ;
#66167 = CARTESIAN_POINT ( 'NONE',  ( 1.207349081364829990, 0.1283753931104748280, 0.1820866141732283561 ) ) ;
#66169 = CARTESIAN_POINT ( 'NONE',  ( 0.3458507752293908943, 0.3458507752293908943, -0.5295275590551181688 ) ) ;
#66170 = CARTESIAN_POINT ( 'NONE',  ( 1.036745406824147731, -0.004921259842519576551, 0.3153832671262227771 ) ) ;
#66171 = ADVANCED_FACE ( 'NONE', ( #43618 ), #31568, .F. ) ;
#66172 = CARTESIAN_POINT ( 'NONE',  ( 1.023622047244095112, -0.1870078740157480879, -0.4822834645669291653 ) ) ;
#66173 = CARTESIAN_POINT ( 'NONE',  ( 0.3949938075777409963, 2.418639510665530743E-17, -0.03740157480314962313 ) ) ;
#66174 = PRODUCT_DEFINITION_SHAPE ( 'NONE', 'NONE',  #83316 ) ;
#66175 = CARTESIAN_POINT ( 'NONE',  ( -0.3346456692913377662, -0.5400638737290844871, 0.3530559997133364547 ) ) ;
#66176 = CARTESIAN_POINT ( 'NONE',  ( -1.489501312335957062, -0.05778040916215522460, 0.4822834645669289988 ) ) ;
#66177 = CARTESIAN_POINT ( 'NONE',  ( -1.548556430446193399, 0.2306618581243848609, 0.2411417322834645549 ) ) ;
#66178 = CARTESIAN_POINT ( 'NONE',  ( -0.3018372703412066094, 0.05413385826771666132, 0.4176697321401328100 ) ) ;
#66179 = EDGE_CURVE ( 'NONE', #32176, #32475, #45371, .T. ) ;
#66180 = CARTESIAN_POINT ( 'NONE',  ( 0.2891555358219910499, -0.2891555358219909944, -0.3326771653543307283 ) ) ;
#66181 = CARTESIAN_POINT ( 'NONE',  ( 1.240157480314961314, 0.1660481256975883668, -0.3530559997133364547 ) ) ;
#66182 = CARTESIAN_POINT ( 'NONE',  ( 0.6167979002624678353, -0.4281496062992124485, 0.4176697321401328655 ) ) ;
#66183 = CONICAL_SURFACE ( 'NONE', #25825, 1.220472440944881942, 0.7853981633974621568 ) ;
#66184 = CARTESIAN_POINT ( 'NONE',  ( 0.4855643044619430415, -0.3690944881889765550, -0.3153832671262227771 ) ) ;
#66185 = CARTESIAN_POINT ( 'NONE',  ( 0.2362204724409451007, -0.4091458600556402980, -0.1686351706036745557 ) ) ;
#66186 = CARTESIAN_POINT ( 'NONE',  ( 0.4068241469816281097, -0.004921259842519576551, 0.3153832671262227771 ) ) ;
#66187 = CARTESIAN_POINT ( 'NONE',  ( -1.968503937007874072, 0.000000000000000000, 5.701968306260621233 ) ) ;
#66188 = CARTESIAN_POINT ( 'NONE',  ( 0.3996062992125985480, 2.446882876249141654E-17, -1.454724409448818978 ) ) ;
#66189 = CARTESIAN_POINT ( 'NONE',  ( 0.5905511811023629321, 0.2952755905511811885, 0.000000000000000000 ) ) ;
#66190 = CARTESIAN_POINT ( 'NONE',  ( -0.1049643490035302024, -0.3917322834645671215, -0.5367454068241469534 ) ) ;
#66191 = CARTESIAN_POINT ( 'NONE',  ( -0.4563452811745912219, 0.01305114060239447211, -2.130073781772667374 ) ) ;
#66192 = CARTESIAN_POINT ( 'NONE',  ( -0.7977407017645437026, -5.134928753749862370E-15, -0.4281989832122469752 ) ) ;
#66193 = CARTESIAN_POINT ( 'NONE',  ( -0.01312335958005186876, -0.3690944881889763329, 0.3153832671262228327 ) ) ;
#66194 = CARTESIAN_POINT ( 'NONE',  ( 0.3412073490813655186, -0.6046776061558809534, -0.2411417322834644161 ) ) ;
#66195 = CARTESIAN_POINT ( 'NONE',  ( 1.660104986876641320, -0.08942795157527998196, 0.3641732283464567121 ) ) ;
#66196 = CARTESIAN_POINT ( 'NONE',  ( -1.023622047244094002, -0.1870078740157480601, -0.3641732283464567677 ) ) ;
#66197 = CARTESIAN_POINT ( 'NONE',  ( -0.8595800524934373854, -0.3162353388693409650, -0.4822834645669289433 ) ) ;
#66198 = CARTESIAN_POINT ( 'NONE',  ( -1.594488188976377563, -0.5400638737290844871, 0.3530559997133364547 ) ) ;
#66199 = CARTESIAN_POINT ( 'NONE',  ( 0.4658792650918641698, -0.05778040916215560624, -0.4822834645669293319 ) ) ;
#66200 = CARTESIAN_POINT ( 'NONE',  ( 1.640419947506562393, -0.4281496062992124485, 0.4176697321401328655 ) ) ;
#66201 = FACE_OUTER_BOUND ( 'NONE', #60857, .T. ) ;
#66202 = CARTESIAN_POINT ( 'NONE',  ( 0.4265091863517067039, -0.6692913385826773087, -0.1292274648535924053 ) ) ;
#66203 = CARTESIAN_POINT ( 'NONE',  ( 0.3458507752293908943, -0.3458507752293908943, -2.694881889763780070 ) ) ;
#66204 = CARTESIAN_POINT ( 'NONE',  ( 0.03098196894106152940, 1.062992125984253411, 3.937007874015747699 ) ) ;
#66205 = CARTESIAN_POINT ( 'NONE',  ( 1.430446194225722500, -0.4281496062992127816, -0.4176697321401328100 ) ) ;
#66206 = CARTESIAN_POINT ( 'NONE',  ( -1.266404199475064773, -0.2845877964562159024, 0.3641732283464567677 ) ) ;
#66207 = CARTESIAN_POINT ( 'NONE',  ( 1.253280839895013710, -0.08942795157528024563, -0.3641732283464568787 ) ) ;
#66208 = CARTESIAN_POINT ( 'NONE',  ( -1.515748031496062076, -0.4536011799217367080, 0.2665933059059888421 ) ) ;
#66209 = CARTESIAN_POINT ( 'NONE',  ( -0.7939632545931750718, -0.08942795157528024563, -0.3641732283464568787 ) ) ;
#66210 = CARTESIAN_POINT ( 'NONE',  ( 1.535433070866142335, -0.6692913385826771977, 8.415575281601705876E-17 ) ) ;
#66211 = CARTESIAN_POINT ( 'NONE',  ( 0.4330708661417329575, -0.5511811023622047445, 6.969142054262312111E-17 ) ) ;
#66212 = CARTESIAN_POINT ( 'NONE',  ( -0.07217847769028787330, -0.05778040916215522460, 0.4822834645669289988 ) ) ;
#66213 = CARTESIAN_POINT ( 'NONE',  ( 0.9514435695538062676, -0.05778040916215522460, 0.4822834645669289988 ) ) ;
#66214 = CARTESIAN_POINT ( 'NONE',  ( 0.1837270341207357105, -0.6046776061558809534, -0.2411417322834644161 ) ) ;
#66215 = CARTESIAN_POINT ( 'NONE',  ( 0.2296587926509192634, -0.08942795157528024563, -0.3641732283464568787 ) ) ;
#66216 = CARTESIAN_POINT ( 'NONE',  ( 1.154855643044620184, 0.2306618581243847221, -0.2411417322834647770 ) ) ;
#66217 = CARTESIAN_POINT ( 'NONE',  ( -0.1706036745406816491, 0.009842519685039147898, -0.3409548833797004797 ) ) ;
#66218 = CARTESIAN_POINT ( 'NONE',  ( -0.7808398950131225646, -0.05778040916215522460, 0.4822834645669289988 ) ) ;
#66219 = B_SPLINE_CURVE_WITH_KNOTS ( 'NONE', 3,
 ( #24859, #50938, #18161, #24454 ),
 .UNSPECIFIED., .F., .F.,
 ( 4, 4 ),
 ( 1.999999999897049408E-07, 0.006970199999999935128 ),
 .UNSPECIFIED. ) ;
#66220 = CARTESIAN_POINT ( 'NONE',  ( 0.1998031496062992740, 0.3460692066303959757, -0.7742782152230971437 ) ) ;
#66221 = CARTESIAN_POINT ( 'NONE',  ( 0.04593175853018440641, 0.2066929133858267098, -0.1054918080437494132 ) ) ;
#66222 = CARTESIAN_POINT ( 'NONE',  ( -0.9448818897637790704, -0.1870078740157480879, -0.4822834645669291653 ) ) ;
#66223 = CARTESIAN_POINT ( 'NONE',  ( 0.08530183727034192087, -0.3162353388693409650, -0.4822834645669289433 ) ) ;
#66224 = CARTESIAN_POINT ( 'NONE',  ( 0.3460692066303959202, 0.1998031496062993295, -2.493438320209973469 ) ) ;
#66225 = CARTESIAN_POINT ( 'NONE',  ( 0.1058382717557500713, -0.3949938075777409408, -2.290026246719159886 ) ) ;
#66226 = ORIENTED_EDGE ( 'NONE', *, *, #8016, .F. ) ;
#66227 = CARTESIAN_POINT ( 'NONE',  ( -0.3392501089628017219, -0.1958661417322836718, -0.3595800524934382736 ) ) ;
#66228 = CYLINDRICAL_SURFACE ( 'NONE', #68171, 0.3937007874015748254 ) ;
#66229 = CARTESIAN_POINT ( 'NONE',  ( -1.312335958005248715, -0.5023911411419708095, -0.1820866141732282451 ) ) ;
#66230 = CARTESIAN_POINT ( 'NONE',  ( 0.2867679344610365999, 0.2867679344610365999, -1.074803149606299080 ) ) ;
#66231 = CARTESIAN_POINT ( 'NONE',  ( 1.601049868766404982, 0.1283753931104748280, 0.1820866141732283561 ) ) ;
#66232 = CARTESIAN_POINT ( 'NONE',  ( -0.3917322834645668994, -0.1049643490035306742, 0.1889956937345949883 ) ) ;
#66233 = CARTESIAN_POINT ( 'NONE',  ( 0.3412073490813655186, -0.6046776061558809534, -0.2411417322834644161 ) ) ;
#66234 = CARTESIAN_POINT ( 'NONE',  ( -0.3477690288713905509, -0.5511811023622046335, 0.09757992244046803654 ) ) ;
#66235 = CARTESIAN_POINT ( 'NONE',  ( 0.7874015748031503170, -0.1870078740157479769, 0.4822834645669291653 ) ) ;
#66236 = CARTESIAN_POINT ( 'NONE',  ( 0.4593175853018379162, -0.4281496062992124485, 0.4176697321401328655 ) ) ;
#66237 = CARTESIAN_POINT ( 'NONE',  ( 0.1088160626412674192, 1.075376824458859959, 1.116863795850121521 ) ) ;
#66238 = CARTESIAN_POINT ( 'NONE',  ( 0.1070741851644054915, -0.3996062992125986035, -2.604986876640420057 ) ) ;
#66239 = CARTESIAN_POINT ( 'NONE',  ( 0.1958661417322836718, -0.3392501089628017219, -1.190964197671602998 ) ) ;
#66240 = CARTESIAN_POINT ( 'NONE',  ( 1.240157480314961314, 0.1660481256975883668, -0.3530559997133364547 ) ) ;
#66241 = CARTESIAN_POINT ( 'NONE',  ( -0.1115485564304456306, 0.2952755905511810774, -0.1292274648535930714 ) ) ;
#66242 = CARTESIAN_POINT ( 'NONE',  ( 1.476377952755906220, 0.1660481256975883668, -0.3530559997133364547 ) ) ;
#66243 = CARTESIAN_POINT ( 'NONE',  ( 0.8858267716535438430, 0.1660481256975885056, 0.3530559997133364547 ) ) ;
#66244 = CARTESIAN_POINT ( 'NONE',  ( 0.3917322834645669549, 0.1049643490035304660, -0.5242782152230972548 ) ) ;
#66245 = CARTESIAN_POINT ( 'NONE',  ( 0.1902887139107617975, 0.2952755905511811885, 0.1292274648535926551 ) ) ;
#66246 = CARTESIAN_POINT ( 'NONE',  ( 0.7939632545931766261, -0.3162353388693409650, -0.4822834645669289433 ) ) ;
#66247 = CARTESIAN_POINT ( 'NONE',  ( 0.07874015748031558404, -0.1870078740157479769, 0.4822834645669291653 ) ) ;
#66248 = CARTESIAN_POINT ( 'NONE',  ( 0.7283464566929143125, 0.07958543189024085140, 0.2665933059059887866 ) ) ;
#66249 = CARTESIAN_POINT ( 'NONE',  ( -1.272965879265091305, -0.4281496062992124485, 0.4176697321401328655 ) ) ;
#66250 = CARTESIAN_POINT ( 'NONE',  ( -1.607611548556429737, -0.6692913385826771977, 0.1292274648535927661 ) ) ;
#66251 = CARTESIAN_POINT ( 'NONE',  ( 0.7152230971128614723, -0.3162353388693409650, -0.4822834645669289433 ) ) ;
#66252 = CARTESIAN_POINT ( 'NONE',  ( 0.3078094465266739133, -0.2432155562296511031, -1.929133858267716661 ) ) ;
#66253 = CARTESIAN_POINT ( 'NONE',  ( -0.3917322834645671215, 0.1049643490035301469, -1.914698162729658648 ) ) ;
#66254 = VERTEX_POINT ( 'NONE', #24772 ) ;
#66255 = CARTESIAN_POINT ( 'NONE',  ( -0.1070741851644056997, 0.3996062992125986035, -0.6364829396325458744 ) ) ;
#66256 = ORIENTED_EDGE ( 'NONE', *, *, #70415, .F. ) ;
#66257 = CARTESIAN_POINT ( 'NONE',  ( 0.9580052493438327987, -0.4281496062992127816, -0.4176697321401328100 ) ) ;
#66258 = CARTESIAN_POINT ( 'NONE',  ( 0.3412073490813655186, 0.1283753931104748280, 0.1820866141732283561 ) ) ;
#66259 = CARTESIAN_POINT ( 'NONE',  ( 3.250800428249174256, 2.742781089625998980, -0.5314960629921260393 ) ) ;
#66260 = PLANE ( 'NONE',  #58443 ) ;
#66261 = CARTESIAN_POINT ( 'NONE',  ( 0.1049643490035303689, 0.3917322834645670104, -1.180446194225722056 ) ) ;
#66262 = ADVANCED_FACE ( 'NONE', ( #50441 ), #63499, .F. ) ;
#66263 = CARTESIAN_POINT ( 'NONE',  ( 1.227034120734908917, -0.6692913385826771977, 0.1292274648535927661 ) ) ;
#66264 = CARTESIAN_POINT ( 'NONE',  ( -1.535433070866141225, -0.6692913385826771977, 8.415575281601705876E-17 ) ) ;
#66265 = CIRCLE ( 'NONE', #29955, 0.1771653543307085410 ) ;
#66266 = CARTESIAN_POINT ( 'NONE',  ( -0.3608923884514428360, -0.6692913385826773087, -0.1292274648535924053 ) ) ;
#66267 = CARTESIAN_POINT ( 'NONE',  ( 1.062992125984252745, -0.6692913385826771977, 8.415575281601705876E-17 ) ) ;
#66268 = ORIENTED_EDGE ( 'NONE', *, *, #66096, .T. ) ;
#66269 = CARTESIAN_POINT ( 'NONE',  ( -1.732283464566928277, -0.1870078740157479769, 0.4822834645669291653 ) ) ;
#66270 = CARTESIAN_POINT ( 'NONE',  ( -1.102273020300588602, 1.111722227514729155, -0.2117565784830439668 ) ) ;
#66271 = DIRECTION ( 'NONE',  ( 1.000000000000000000, 0.000000000000000000, 1.047444401652940007E-14 ) ) ;
#66272 = CARTESIAN_POINT ( 'NONE',  ( -1.595398199321657051, 0.7585570207896574768, -0.1559797534342474146 ) ) ;
#66273 = CARTESIAN_POINT ( 'NONE',  ( -0.1070741851644051862, -0.3996062992125986035, -2.038713910761154491 ) ) ;
#66274 = CARTESIAN_POINT ( 'NONE',  ( -1.299212598425196097, 0.1771653543307087630, 0.000000000000000000 ) ) ;
#66275 = CARTESIAN_POINT ( 'NONE',  ( -1.548556430446193399, -0.6046776061558809534, -0.2411417322834644161 ) ) ;
#66276 = CARTESIAN_POINT ( 'NONE',  ( 0.6364829396325465405, -0.3162353388693409650, -0.4822834645669289433 ) ) ;
#66277 = ORIENTED_EDGE ( 'NONE', *, *, #78409, .T. ) ;
#66279 = DIRECTION ( 'NONE',  ( 0.000000000000000000, 0.000000000000000000, 1.000000000000000000 ) ) ;
#66278 = CARTESIAN_POINT ( 'NONE',  ( 1.410761154855643795, -0.05778040916215560624, -0.4822834645669293319 ) ) ;
#66280 = CARTESIAN_POINT ( 'NONE',  ( -0.7414698162729651543, 0.1771653543307087075, -0.09757992244046823083 ) ) ;
#66281 = CARTESIAN_POINT ( 'NONE',  ( 0.8267716535433078384, -0.6692913385826771977, 8.415575281601705876E-17 ) ) ;
#66282 = CARTESIAN_POINT ( 'NONE',  ( 1.594488188976378673, 0.07958543189024085140, 0.2665933059059887866 ) ) ;
#66283 = CARTESIAN_POINT ( 'NONE',  ( -9.594673741351310580E-17, 0.3917322834645669549, -1.339875697341520455 ) ) ;
#66284 = AXIS2_PLACEMENT_3D ( 'NONE', #22317, #28211, #66528 ) ;
#66285 = CARTESIAN_POINT ( 'NONE',  ( -0.9842519685039365918, -0.5511811023622047445, 6.969142054262312111E-17 ) ) ;
#66286 = CARTESIAN_POINT ( 'NONE',  ( -1.502624671916009680, -0.2845877964562159024, 0.3641732283464567677 ) ) ;
#66287 = CARTESIAN_POINT ( 'NONE',  ( -0.3917322834645670104, -7.196005306013484475E-17, -1.068897637795275690 ) ) ;
#66288 = CARTESIAN_POINT ( 'NONE',  ( 0.6102362204724416372, -0.5400638737290844871, 0.3530559997133364547 ) ) ;
#66289 = CARTESIAN_POINT ( 'NONE',  ( -1.069553805774277722, -0.5511811023622048555, -0.09757992244046775898 ) ) ;
#66290 = CARTESIAN_POINT ( 'NONE',  ( -0.2230971128608915943, -0.3690944881889765550, -0.3153832671262227771 ) ) ;
#66291 = CARTESIAN_POINT ( 'NONE',  ( -0.1574803149606292529, -0.1870078740157479769, 0.4822834645669291653 ) ) ;
#66292 = CARTESIAN_POINT ( 'NONE',  ( 1.601049868766404982, -0.6046776061558809534, -0.2411417322834644161 ) ) ;
#66293 = CARTESIAN_POINT ( 'NONE',  ( 0.3917322834645670659, -0.1049643490035303273, -0.2657673472779021884 ) ) ;
#66294 = CARTESIAN_POINT ( 'NONE',  ( 0.9448818897637802916, -0.1870078740157479769, 0.4822834645669291653 ) ) ;
#66295 = DIRECTION ( 'NONE',  ( 0.000000000000000000, -0.000000000000000000, -1.000000000000000000 ) ) ;
#66296 = CARTESIAN_POINT ( 'NONE',  ( 0.3458507752293908943, 0.3458507752293908943, -1.474409448818897683 ) ) ;
#66297 = CARTESIAN_POINT ( 'NONE',  ( -0.7152230971128602510, -0.05778040916215560624, -0.4822834645669293319 ) ) ;
#66298 = CARTESIAN_POINT ( 'NONE',  ( -0.09186351706036689768, -0.004921259842519870586, -0.3153832671262229437 ) ) ;
#66299 = CARTESIAN_POINT ( 'NONE',  ( -1.515748031496062076, -0.5400638737290844871, 0.3530559997133364547 ) ) ;
#66300 = CARTESIAN_POINT ( 'NONE',  ( 0.3805774278215230400, -0.3690944881889763329, 0.3153832671262228327 ) ) ;
#66301 = CARTESIAN_POINT ( 'NONE',  ( -0.5839895013123351797, 0.1771653543307087075, -0.09757992244046823083 ) ) ;
#66302 = CARTESIAN_POINT ( 'NONE',  ( -1.207349081364828880, 0.2306618581243847221, -0.2411417322834647770 ) ) ;
#66303 = CARTESIAN_POINT ( 'NONE',  ( -1.607611548556429737, -0.6692913385826771977, 0.1292274648535927661 ) ) ;
#66304 = CARTESIAN_POINT ( 'NONE',  ( 1.601049868766404982, -0.6046776061558809534, -0.2411417322834644161 ) ) ;
#66305 = CARTESIAN_POINT ( 'NONE',  ( -0.7080320533160967544, 1.900312960331933976, 0.5309055118110236338 ) ) ;
#66306 = CARTESIAN_POINT ( 'NONE',  ( 0.6955380577427828781, -0.3690944881889763329, 0.3153832671262228327 ) ) ;
#66307 = CARTESIAN_POINT ( 'NONE',  ( 0.4002624671916016896, -0.05778040916215522460, 0.4822834645669289988 ) ) ;
#66308 = CARTESIAN_POINT ( 'NONE',  ( -1.463254593175852492, 0.2952755905511811885, 0.1292274648535926551 ) ) ;
#66309 = CARTESIAN_POINT ( 'NONE',  ( 1.469816272965879911, 0.1283753931104746893, -0.1820866141732285504 ) ) ;
#66310 = EDGE_LOOP ( 'NONE', ( #52523, #26140, #20680, #62613 ) ) ;
#66311 = B_SPLINE_CURVE_WITH_KNOTS ( 'NONE', 3,
 ( #31388, #6967, #667, #25068, #6551, #31807, #51559 ),
 .UNSPECIFIED., .F., .F.,
 ( 4, 3, 4 ),
 ( 6.162975822039154730E-33, 0.001246232571205312329, 0.002492492258783241162 ),
 .UNSPECIFIED. ) ;
#66312 = CARTESIAN_POINT ( 'NONE',  ( 0.3996062992125985480, 2.446882876249141654E-17, -2.714566929133858331 ) ) ;
#66313 = CARTESIAN_POINT ( 'NONE',  ( -1.161417322834644716, 0.07958543189024085140, 0.2665933059059887866 ) ) ;
#66314 = CARTESIAN_POINT ( 'NONE',  ( -0.4790026246719152336, -0.05778040916215560624, -0.4822834645669293319 ) ) ;
#66315 = CARTESIAN_POINT ( 'NONE',  ( 0.1509186351706042484, -0.3162353388693405765, 0.4822834645669290543 ) ) ;
#66316 = CARTESIAN_POINT ( 'NONE',  ( -1.469816272965878357, -0.5023911411419708095, -0.1820866141732282451 ) ) ;
#66317 = CARTESIAN_POINT ( 'NONE',  ( 0.2925321140481932369, 0.2925321140481932369, -1.789370078740157410 ) ) ;
#66318 = CARTESIAN_POINT ( 'NONE',  ( -1.351706036745406347, 0.05413385826771626580, -0.4176697321401330321 ) ) ;
#66319 = CARTESIAN_POINT ( 'NONE',  ( 0.5249343832021005074, -0.6046776061558807314, 0.2411417322834647770 ) ) ;
#66320 = CARTESIAN_POINT ( 'NONE',  ( 0.1837270341207357105, -0.6046776061558809534, -0.2411417322834644161 ) ) ;
#66321 = CARTESIAN_POINT ( 'NONE',  ( 1.272965879265092637, 0.05413385826771666132, 0.4176697321401328100 ) ) ;
#66322 = CARTESIAN_POINT ( 'NONE',  ( 0.1998031496062992463, 0.3460692066303959202, -1.008530183727034180 ) ) ;
#66323 = CARTESIAN_POINT ( 'NONE',  ( 0.1070741851644053527, 0.3996062992125986590, -1.568241469816272993 ) ) ;
#66324 = CARTESIAN_POINT ( 'NONE',  ( 0.3420746716998660508, -0.1974969037888703871, -0.7349081364829396223 ) ) ;
#66325 = B_SPLINE_CURVE_WITH_KNOTS ( 'NONE', 3,
 ( #47921, #9227, #10054, #41615 ),
 .UNSPECIFIED., .F., .F.,
 ( 4, 4 ),
 ( 3.593986969192262371E-07, 0.001287825409103183008 ),
 .UNSPECIFIED. ) ;
#66326 = CIRCLE ( 'NONE', #23353, 0.09842519685039372024 ) ;
#66327 = CARTESIAN_POINT ( 'NONE',  ( 0.3917322834645670104, -0.1049643490035303273, -0.1036745406824146343 ) ) ;
#66328 = CARTESIAN_POINT ( 'NONE',  ( -0.01968503937007793844, -0.4536011799217367080, 0.2665933059059888421 ) ) ;
#66329 = CARTESIAN_POINT ( 'NONE',  ( -0.2887139107611542133, 0.2306618581243848609, 0.2411417322834645549 ) ) ;
#66330 = CARTESIAN_POINT ( 'NONE',  ( 0.8070866141732288002, 0.1660481256975885056, 0.3530559997133364547 ) ) ;
#66331 = CARTESIAN_POINT ( 'NONE',  ( 0.3420746716998660508, 0.1974969037888705814, -1.782808398950131101 ) ) ;
#66332 = CARTESIAN_POINT ( 'NONE',  ( -0.2099737532808391705, 0.1283753931104748280, 0.1820866141732283561 ) ) ;
#66333 = CARTESIAN_POINT ( 'NONE',  ( -1.299212598425196097, 0.2952755905511811885, 0.000000000000000000 ) ) ;
#66334 = CARTESIAN_POINT ( 'NONE',  ( -1.594488188976377119, 0.1660481256975883668, -0.3530559997133364547 ) ) ;
#66335 = CARTESIAN_POINT ( 'NONE',  ( 0.1265901696524989462, 0.4724409448818897572, -1.883202099737532276 ) ) ;
#66336 = CARTESIAN_POINT ( 'NONE',  ( 0.2263583204867608833, 0.3204081651523129071, -2.755905511811024056 ) ) ;
#66337 = ORIENTED_EDGE ( 'NONE', *, *, #29846, .F. ) ;
#66338 = VERTEX_POINT ( 'NONE', #41156 ) ;
#66339 = CARTESIAN_POINT ( 'NONE',  ( 1.272965879265092637, 0.05413385826771666132, 0.4176697321401328100 ) ) ;
#66340 = CIRCLE ( 'NONE', #74399, 2.362204724409449064 ) ;
#66341 = CARTESIAN_POINT ( 'NONE',  ( -1.679790026246718693, 0.2306618581243847221, -0.2411417322834647770 ) ) ;
#66343 = CARTESIAN_POINT ( 'NONE',  ( -1.371391076115484609, -0.6692913385826771977, 0.1292274648535927661 ) ) ;
#66342 = CARTESIAN_POINT ( 'NONE',  ( -1.351706036745406347, -0.3690944881889763329, 0.3153832671262228327 ) ) ;
#66344 = CARTESIAN_POINT ( 'NONE',  ( -0.3917322834645670659, 0.1049643490035301607, -2.475046301016061268 ) ) ;
#66345 = CARTESIAN_POINT ( 'NONE',  ( -0.5314960629921122726, 2.559055118110236560, -3.937007874015763687 ) ) ;
#66346 = CARTESIAN_POINT ( 'NONE',  ( 1.043307086614173818, 0.1660481256975885056, 0.3530559997133364547 ) ) ;
#66347 = CARTESIAN_POINT ( 'NONE',  ( 0.1181102362204730916, -0.6692913385826771977, 8.415575281601705876E-17 ) ) ;
#66348 = CARTESIAN_POINT ( 'NONE',  ( -0.2952755905511804668, 0.1660481256975885056, 0.3530559997133364547 ) ) ;
#66349 = CARTESIAN_POINT ( 'NONE',  ( -1.220472440944881054, -0.6692913385826771977, 8.415575281601705876E-17 ) ) ;
#66350 = CARTESIAN_POINT ( 'NONE',  ( 0.3917322834645668994, -0.1049643490035303134, -2.711266773457006174 ) ) ;
#66351 = EDGE_CURVE ( 'NONE', #66780, #9475, #43779, .T. ) ;
#66352 = CARTESIAN_POINT ( 'NONE',  ( 0.5643044619422579178, -0.4281496062992127816, -0.4176697321401328100 ) ) ;
#66353 = CARTESIAN_POINT ( 'NONE',  ( -0.3392501089628019995, 0.1958661417322832277, -1.908136482939632561 ) ) ;
#66354 = CARTESIAN_POINT ( 'NONE',  ( -1.358267716535432434, -0.4536011799217367080, 0.2665933059059888421 ) ) ;
#66355 = VERTEX_POINT ( 'NONE', #59674 ) ;
#66356 = CARTESIAN_POINT ( 'NONE',  ( 4.837279021331060870E-17, -0.3949938075777409963, -2.283464566929133799 ) ) ;
#66357 = VERTEX_POINT ( 'NONE', #53765 ) ;
#66358 = CARTESIAN_POINT ( 'NONE',  ( -2.130073781772662489, 0.01305114060239441834, -0.4563452811746135374 ) ) ;
#66359 = CARTESIAN_POINT ( 'NONE',  ( -1.220472440944881054, 0.2952755905511811885, 0.000000000000000000 ) ) ;
#66360 = CARTESIAN_POINT ( 'NONE',  ( -1.154855643044618851, 0.2306618581243848609, 0.2411417322834645549 ) ) ;
#66361 = CARTESIAN_POINT ( 'NONE',  ( -0.3996062992125987146, 0.1070741851644051862, -0.6627296587926508886 ) ) ;
#66362 = CARTESIAN_POINT ( 'NONE',  ( -1.496062992125983815, -0.1870078740157480879, -0.4822834645669291653 ) ) ;
#66363 = CARTESIAN_POINT ( 'NONE',  ( -1.581364829396324945, -0.3162353388693405765, 0.4822834645669290543 ) ) ;
#66364 = FACE_OUTER_BOUND ( 'NONE', #278, .T. ) ;
#66365 = LINE ( 'NONE', #4042, #43131 ) ;
#66366 = CARTESIAN_POINT ( 'NONE',  ( -0.1049643490035302024, -0.3917322834645671215, -0.1568241469816273603 ) ) ;
#66367 = EDGE_CURVE ( 'NONE', #28871, #10316, #52727, .T. ) ;
#66368 = CARTESIAN_POINT ( 'NONE',  ( -0.07217847769028787330, -0.08942795157527998196, 0.3641732283464567121 ) ) ;
#66369 = CARTESIAN_POINT ( 'NONE',  ( -0.6364829396325453192, -0.2845877964562159024, 0.3641732283464567677 ) ) ;
#66370 = CARTESIAN_POINT ( 'NONE',  ( -1.259842519685038686, -0.1870078740157480879, -0.4822834645669291653 ) ) ;
#66371 = CARTESIAN_POINT ( 'NONE',  ( 1.095800524934383846, -0.3162353388693405765, 0.4822834645669290543 ) ) ;
#66372 = CARTESIAN_POINT ( 'NONE',  ( -1.102362204724408601, -0.1870078740157480879, -0.4822834645669291653 ) ) ;
#66373 = DIRECTION ( 'NONE',  ( -0.000000000000000000, 1.734723475976805615E-16, 1.000000000000000000 ) ) ;
#66374 = VERTEX_POINT ( 'NONE', #66844 ) ;
#66375 = CARTESIAN_POINT ( 'NONE',  ( -1.528871391076114250, -0.6692913385826771977, 0.1292274648535927661 ) ) ;
#66376 = CARTESIAN_POINT ( 'NONE',  ( -1.712598425196849572, 0.07958543189024085140, 0.2665933059059887866 ) ) ;
#66377 = CARTESIAN_POINT ( 'NONE',  ( -1.627296587926508442, -0.6046776061558809534, -0.2411417322834644161 ) ) ;
#66378 = CARTESIAN_POINT ( 'NONE',  ( -0.4091458600556405756, 0.2362204724409446288, -1.286089238845144367 ) ) ;
#66379 = DIRECTION ( 'NONE',  ( 1.000000000000000000, -0.000000000000000000, -0.000000000000000000 ) ) ;
#66380 = CARTESIAN_POINT ( 'NONE',  ( 0.2867679344610365999, -0.2867679344610365444, -0.8779527559055116948 ) ) ;
#66381 = CARTESIAN_POINT ( 'NONE',  ( 0.2867679344610366554, 0.2867679344610366554, -2.427165354330708791 ) ) ;
#66382 = CARTESIAN_POINT ( 'NONE',  ( -0.5183727034120726440, 0.2952755905511811885, 0.1292274648535926551 ) ) ;
#66383 = CARTESIAN_POINT ( 'NONE',  ( -1.509186351706035767, -0.3690944881889763329, 0.3153832671262228327 ) ) ;
#66384 = CARTESIAN_POINT ( 'NONE',  ( -9.787531504996566615E-17, 0.3996062992125985480, 0.08070866141732281618 ) ) ;
#66385 = DIRECTION ( 'NONE',  ( 0.000000000000000000, 0.000000000000000000, -1.000000000000000000 ) ) ;
#66386 = CARTESIAN_POINT ( 'NONE',  ( -1.496062992125983815, -0.1870078740157480879, -0.4822834645669291653 ) ) ;
#66387 = CARTESIAN_POINT ( 'NONE',  ( -0.4921259842519677963, -0.5400638737290844871, 0.3530559997133364547 ) ) ;
#66388 = CARTESIAN_POINT ( 'NONE',  ( 0.3392501089628018329, 0.1958661417322835052, 0.1036938564642537891 ) ) ;
#66389 = CARTESIAN_POINT ( 'NONE',  ( 0.3674540682414705883, 0.1283753931104746893, -0.1820866141732285504 ) ) ;
#66390 = DIRECTION ( 'NONE',  ( 0.000000000000000000, 1.000000000000000000, 0.000000000000000000 ) ) ;
#66391 = CIRCLE ( 'NONE', #9972, 0.2952755905511810774 ) ;
#66392 = CARTESIAN_POINT ( 'NONE',  ( 0.4002624671916016896, -0.08942795157527998196, 0.3641732283464567121 ) ) ;
#66393 = CARTESIAN_POINT ( 'NONE',  ( 0.8595800524934390507, -0.08942795157528024563, -0.3641732283464568787 ) ) ;
#66394 = CARTESIAN_POINT ( 'NONE',  ( 0.8530183727034126306, 0.05413385826771626580, -0.4176697321401330321 ) ) ;
#66395 = CARTESIAN_POINT ( 'NONE',  ( -0.1574803149606292529, -0.1870078740157480601, -0.3641732283464567677 ) ) ;
#66396 = CARTESIAN_POINT ( 'NONE',  ( -0.3917322834645669549, -0.1049643490035306603, -1.770341207349081181 ) ) ;
#66397 = CARTESIAN_POINT ( 'NONE',  ( -1.220472440944881054, -0.6692913385826771977, 8.415575281601705876E-17 ) ) ;
#66398 = CARTESIAN_POINT ( 'NONE',  ( 0.09842519685039434474, -0.4536011799217368745, -0.2665933059059886201 ) ) ;
#66399 = CARTESIAN_POINT ( 'NONE',  ( -1.128608923884513837, 0.1283753931104746893, -0.1820866141732285504 ) ) ;
#66400 = CARTESIAN_POINT ( 'NONE',  ( 0.1265901696524990294, -0.4724409448818896462, -0.4770341207349080848 ) ) ;
#66401 = CARTESIAN_POINT ( 'NONE',  ( -0.7742782152230962556, -0.3690944881889765550, -0.3153832671262227771 ) ) ;
#66402 = CARTESIAN_POINT ( 'NONE',  ( 0.4177787735906991484, 1.312623414240987163, -1.404325600637324367 ) ) ;
#66403 = CARTESIAN_POINT ( 'NONE',  ( -0.1640419947506553400, -0.05778040916215560624, -0.4822834645669293319 ) ) ;
#66404 = CARTESIAN_POINT ( 'NONE',  ( 1.633858267716535639, -0.4536011799217367080, 0.2665933059059888421 ) ) ;
#66405 = CIRCLE ( 'NONE', #70405, 0.1279527559055117503 ) ;
#66406 = CARTESIAN_POINT ( 'NONE',  ( 0.6758530183727039509, 0.1771653543307087075, -0.09757992244046823083 ) ) ;
#66407 = CARTESIAN_POINT ( 'NONE',  ( -0.2624671916010490880, 0.1283753931104746893, -0.1820866141732285504 ) ) ;
#66408 = CARTESIAN_POINT ( 'NONE',  ( -0.3149606299212590610, -0.1870078740157480879, -0.4822834645669291653 ) ) ;
#66409 = DIRECTION ( 'NONE',  ( 0.000000000000000000, 0.000000000000000000, -1.000000000000000000 ) ) ;
#66410 = CARTESIAN_POINT ( 'NONE',  ( -1.213910761154854745, -0.5511811023622046335, 0.09757992244046803654 ) ) ;
#66411 = LINE ( 'NONE', #34419, #21986 ) ;
#66412 = CARTESIAN_POINT ( 'NONE',  ( 0.7742782152230979209, 0.05413385826771626580, -0.4176697321401330321 ) ) ;
#66413 = ORIENTED_EDGE ( 'NONE', *, *, #74544, .F. ) ;
#66414 = CARTESIAN_POINT ( 'NONE',  ( -0.3996062992125986590, 0.1070741851644051723, -1.526902887139107490 ) ) ;
#66415 = DIRECTION ( 'NONE',  ( -1.000000000000000000, -3.412570772413390973E-16, 0.000000000000000000 ) ) ;
#66416 = CARTESIAN_POINT ( 'NONE',  ( -0.2559055118110230564, 0.07958543189024071263, -0.2665933059059888421 ) ) ;
#66417 = CARTESIAN_POINT ( 'NONE',  ( -1.581364829396324945, -0.05778040916215560624, -0.4822834645669293319 ) ) ;
#66418 = CARTESIAN_POINT ( 'NONE',  ( 1.568241469816273659, -0.05778040916215560624, -0.4822834645669293319 ) ) ;
#66419 = CARTESIAN_POINT ( 'NONE',  ( 1.391076115485564868, 0.2306618581243847221, -0.2411417322834647770 ) ) ;
#66420 = CARTESIAN_POINT ( 'NONE',  ( -0.5380577427821514602, -0.3690944881889765550, -0.3153832671262227771 ) ) ;
#66421 = CARTESIAN_POINT ( 'NONE',  ( -1.090866038711135744, -2.570477104772672414E-15, 0.3791475997938242304 ) ) ;
#66422 = CARTESIAN_POINT ( 'NONE',  ( 0.7677165354330716118, -0.5400638737290844871, 0.3530559997133364547 ) ) ;
#66423 = CARTESIAN_POINT ( 'NONE',  ( 0.3996062992125986035, 2.446882876249141962E-17, -0.2755905511811023723 ) ) ;
#66424 = CARTESIAN_POINT ( 'NONE',  ( -0.3392501089628017219, -0.1958661417322836995, -2.726397268537744445 ) ) ;
#66425 = EDGE_CURVE ( 'NONE', #30161, #7970, #26656, .T. ) ;
#66426 = FACE_BOUND ( 'NONE', #79170, .T. ) ;
#66427 = CARTESIAN_POINT ( 'NONE',  ( 1.476377952755906220, 0.07958543189024071263, -0.2665933059059888421 ) ) ;
#66428 = CARTESIAN_POINT ( 'NONE',  ( -1.338582677165353729, -0.1870078740157480879, -0.4822834645669291653 ) ) ;
#66429 = CARTESIAN_POINT ( 'NONE',  ( 1.286089238845145033, 0.2306618581243848609, 0.2411417322834645549 ) ) ;
#66430 = CARTESIAN_POINT ( 'NONE',  ( 0.1049643490035304938, -0.3917322834645669549, -2.217191601049868677 ) ) ;
#66431 = CARTESIAN_POINT ( 'NONE',  ( 1.102362204724410155, -0.1870078740157480601, -0.3641732283464567677 ) ) ;
#66432 = CARTESIAN_POINT ( 'NONE',  ( 0.1181102362204730916, 0.2952755905511811885, 0.000000000000000000 ) ) ;
#66433 = CARTESIAN_POINT ( 'NONE',  ( -0.4855643044619415427, 0.05413385826771626580, -0.4176697321401330321 ) ) ;
#66434 = CARTESIAN_POINT ( 'NONE',  ( 1.620734908136483465, -0.6692913385826771977, 0.1292274648535927661 ) ) ;
#66435 = CARTESIAN_POINT ( 'NONE',  ( 0.3996062992125985480, 0.1070741851644054637, -2.014435695538057125 ) ) ;
#66436 = CARTESIAN_POINT ( 'NONE',  ( 0.1902887139107617975, 0.1771653543307087630, 0.09757992244046791164 ) ) ;
#66437 = ORIENTED_EDGE ( 'NONE', *, *, #17226, .F. ) ;
#66438 = CARTESIAN_POINT ( 'NONE',  ( -0.3917322834645671770, 0.1049643490035302024, -0.5019878197188469837 ) ) ;
#66439 = VERTEX_POINT ( 'NONE', #1618 ) ;
#66440 = CARTESIAN_POINT ( 'NONE',  ( -0.2821522309711278487, 0.2952755905511811885, 0.1292274648535926551 ) ) ;
#66441 = CARTESIAN_POINT ( 'NONE',  ( 1.377952755905512472, -0.6692913385826771977, 8.415575281601705876E-17 ) ) ;
#66442 = CARTESIAN_POINT ( 'NONE',  ( 0.05905511811023709395, -0.5400638737290844871, 0.3530559997133364547 ) ) ;
#66443 = CARTESIAN_POINT ( 'NONE',  ( -0.2230971128608915943, -0.004921259842519576551, 0.3153832671262227771 ) ) ;
#66444 = AXIS2_PLACEMENT_3D ( 'NONE', #81504, #55386, #62959 ) ;
#66445 = CARTESIAN_POINT ( 'NONE',  ( 1.194225721784777594, 0.05413385826771666132, 0.4176697321401328100 ) ) ;
#66446 = CARTESIAN_POINT ( 'NONE',  ( -0.8661417322834640276, -0.1870078740157479769, 0.4822834645669291653 ) ) ;
#66447 = CARTESIAN_POINT ( 'NONE',  ( -0.1574803149606292529, -0.1870078740157479769, 0.4822834645669291653 ) ) ;
#66448 = CARTESIAN_POINT ( 'NONE',  ( -0.7808398950131225646, -0.05778040916215522460, 0.4822834645669289988 ) ) ;
#66449 = CARTESIAN_POINT ( 'NONE',  ( 1.174540682414699111, -0.05778040916215560624, -0.4822834645669293319 ) ) ;
#66450 = CARTESIAN_POINT ( 'NONE',  ( 1.089238845144357537, -0.4281496062992124485, 0.4176697321401328655 ) ) ;
#66451 = CARTESIAN_POINT ( 'NONE',  ( 1.187664041994751285, -0.05778040916215522460, 0.4822834645669289988 ) ) ;
#66452 = CARTESIAN_POINT ( 'NONE',  ( -0.3917322834645670104, -7.196005306013484475E-17, -0.8188976377952754682 ) ) ;
#66453 = CARTESIAN_POINT ( 'NONE',  ( 0.1312335958005257930, 0.1283753931104746893, -0.1820866141732285504 ) ) ;
#66454 = EDGE_LOOP ( 'NONE', ( #66732, #45720, #1476, #48535 ) ) ;
#66455 = CARTESIAN_POINT ( 'NONE',  ( -0.3949938075777411628, 0.1058382717557497937, -0.9776902887139109488 ) ) ;
#66456 = ORIENTED_EDGE ( 'NONE', *, *, #60880, .F. ) ;
#66457 = CARTESIAN_POINT ( 'NONE',  ( -0.9448818897637790704, -0.1870078740157479769, 0.3641732283464567677 ) ) ;
#66458 = CARTESIAN_POINT ( 'NONE',  ( -0.1574803149606292529, -0.1870078740157480879, -0.4822834645669291653 ) ) ;
#66459 = CARTESIAN_POINT ( 'NONE',  ( -1.485206097856770269, 1.138394384027662243, 0.2566527756886388123 ) ) ;
#66460 = CARTESIAN_POINT ( 'NONE',  ( -0.4199475065616791736, 0.2306618581243847221, -0.2411417322834647770 ) ) ;
#66461 = CARTESIAN_POINT ( 'NONE',  ( -0.5249343832020990641, -0.6046776061558809534, -0.2411417322834644161 ) ) ;
#66462 = CARTESIAN_POINT ( 'NONE',  ( -0.8858267716535425107, -0.5400638737290844871, 0.3530559997133364547 ) ) ;
#66463 = CARTESIAN_POINT ( 'NONE',  ( -1.358267716535432434, 0.1660481256975883668, -0.3530559997133364547 ) ) ;
#66464 = CIRCLE ( 'NONE', #46312, 3.582677165354332338 ) ;
#66465 = CARTESIAN_POINT ( 'NONE',  ( 1.528871391076116026, 0.1771653543307087630, 0.09757992244046791164 ) ) ;
#66466 = DIRECTION ( 'NONE',  ( -0.7071067811865495711, 0.000000000000000000, 0.7071067811865454633 ) ) ;
#66467 = CARTESIAN_POINT ( 'NONE',  ( 0.2490413359174502850, 0.1587297840844698882, 5.622433025490734870 ) ) ;
#66468 = CARTESIAN_POINT ( 'NONE',  ( 0.2952755905511816326, -0.4536011799217367080, 0.2665933059059888421 ) ) ;
#66469 = CARTESIAN_POINT ( 'NONE',  ( -0.04593175853018302557, 0.2952755905511811885, 0.1292274648535926551 ) ) ;
#66470 = CARTESIAN_POINT ( 'NONE',  ( 0.3805774278215230400, -0.4281496062992124485, 0.4176697321401328655 ) ) ;
#66471 = ORIENTED_EDGE ( 'NONE', *, *, #68170, .T. ) ;
#66472 = CARTESIAN_POINT ( 'NONE',  ( -0.1070741851644056997, 0.3996062992125986035, -1.896325459317584894 ) ) ;
#66473 = FACE_OUTER_BOUND ( 'NONE', #34031, .T. ) ;
#66474 = CARTESIAN_POINT ( 'NONE',  ( 0.1998031496062992463, 0.3460692066303959202, -1.166010498687663821 ) ) ;
#66475 = CARTESIAN_POINT ( 'NONE',  ( 0.1070741851644053388, 0.3996062992125986035, -0.3851706036745406458 ) ) ;
#66476 = CARTESIAN_POINT ( 'NONE',  ( -0.6036745406824141069, 0.2306618581243848609, 0.2411417322834645549 ) ) ;
#66477 = CARTESIAN_POINT ( 'NONE',  ( -0.4724409448818899238, 0.1265901696524986686, -0.03280839895013123314 ) ) ;
#66478 = CARTESIAN_POINT ( 'NONE',  ( 0.1958661417322834775, 0.3392501089628018884, -2.118766404199475151 ) ) ;
#66479 = CARTESIAN_POINT ( 'NONE',  ( -1.601049868766403650, 0.1283753931104746893, -0.1820866141732285504 ) ) ;
#66480 = CARTESIAN_POINT ( 'NONE',  ( 1.043307086614173818, -0.5400638737290845981, -0.3530559997133363437 ) ) ;
#66481 = CARTESIAN_POINT ( 'NONE',  ( 0.8464566929133866546, -0.5400638737290844871, 0.3530559997133364547 ) ) ;
#66482 = CARTESIAN_POINT ( 'NONE',  ( -0.2755905511811015396, -0.5511811023622047445, 6.969142054262312111E-17 ) ) ;
#66483 = CARTESIAN_POINT ( 'NONE',  ( 0.2427821522309716595, -0.3162353388693409650, -0.4822834645669289433 ) ) ;
#66484 = CARTESIAN_POINT ( 'NONE',  ( 0.4091458600556404646, -0.2362204724409448231, -1.914041994750656395 ) ) ;
#66485 = CARTESIAN_POINT ( 'NONE',  ( -0.04593175853018302557, 0.1771653543307087630, 0.09757992244046791164 ) ) ;
#66486 = CARTESIAN_POINT ( 'NONE',  ( -0.3280839895013117347, -0.4281496062992124485, 0.4176697321401328655 ) ) ;
#66487 = CARTESIAN_POINT ( 'NONE',  ( -0.1058382717557503072, 0.3949938075777408852, -1.973097112860892510 ) ) ;
#66488 = CARTESIAN_POINT ( 'NONE',  ( -1.607611548556429737, -0.6692913385826771977, 0.1292274648535927661 ) ) ;
#66489 = CARTESIAN_POINT ( 'NONE',  ( 0.2624671916010504757, -0.5023911411419708095, -0.1820866141732282451 ) ) ;
#66490 = CARTESIAN_POINT ( 'NONE',  ( -0.7330015572057683171, 1.982446682556143758, -0.5178628694646268960 ) ) ;
#66492 = ADVANCED_FACE ( 'NONE', ( #72325 ), #52935, .F. ) ;
#66491 = CARTESIAN_POINT ( 'NONE',  ( -1.017060367454067249, -0.3162353388693409650, -0.4822834645669289433 ) ) ;
#66493 = CARTESIAN_POINT ( 'NONE',  ( -0.5511811023622038563, -0.1870078740157479769, 0.3641732283464567677 ) ) ;
#66494 = DIRECTION ( 'NONE',  ( 0.000000000000000000, 1.000000000000000000, -0.000000000000000000 ) ) ;
#66495 = CARTESIAN_POINT ( 'NONE',  ( -0.6758530183727028406, -0.6692913385826773087, -0.1292274648535924053 ) ) ;
#66496 = CARTESIAN_POINT ( 'NONE',  ( -0.4593175853018364174, -0.4281496062992127816, -0.4176697321401328100 ) ) ;
#66497 = CARTESIAN_POINT ( 'NONE',  ( 0.07874015748031558404, -0.1870078740157479769, 0.4822834645669291653 ) ) ;
#66498 = CARTESIAN_POINT ( 'NONE',  ( -0.1998031496062991630, -0.3460692066303959202, -2.662073490813648746 ) ) ;
#66499 = CARTESIAN_POINT ( 'NONE',  ( 4.797336870675655290E-17, -0.3917322834645669549, -2.206017429624985038 ) ) ;
#66500 = CARTESIAN_POINT ( 'NONE',  ( -0.5314960629921127166, 2.755905511811024056, -3.831929248781930308 ) ) ;
#66501 = CARTESIAN_POINT ( 'NONE',  ( 0.3018372703412079971, -0.004921259842519870586, -0.3153832671262229437 ) ) ;
#66502 = CARTESIAN_POINT ( 'NONE',  ( 1.076115485564305141, -0.6046776061558807314, 0.2411417322834647770 ) ) ;
#66503 = CARTESIAN_POINT ( 'NONE',  ( -1.253280839895012377, -0.08942795157527998196, 0.3641732283464567121 ) ) ;
#66504 =( BOUNDED_CURVE ( )  B_SPLINE_CURVE ( 2, ( #66122, #8458, #42088, #21496, #15613, #66958, #29463, #34128, #9702, #2562, #15194, #28220, #16029 ),
 .UNSPECIFIED., .F., .F. ) 
 B_SPLINE_CURVE_WITH_KNOTS ( ( 3, 2, 2, 2, 2, 2, 3 ),
 ( 0.4126696296615054438, 0.4128787878787879562, 0.4166666666666667407, 0.4204545454545455252, 0.4242424242424243097, 0.4280303030303030942, 0.4282394612475854956 ),
 .UNSPECIFIED. ) 
 CURVE ( )  GEOMETRIC_REPRESENTATION_ITEM ( )  RATIONAL_B_SPLINE_CURVE ( ( 0.9964447847208419695, 0.9981185001348091834, 1.000000000000000000, 0.9659258262890683122, 1.000000000000000000, 0.9659258262890683122, 1.000000000000000000, 0.9659258262890683122, 1.000000000000000000, 0.9659258262890683122, 1.000000000000000000, 0.9981185001348101826, 0.9964447847208438569 ) ) 
 REPRESENTATION_ITEM ( '' )  );
#66505 = CARTESIAN_POINT ( 'NONE',  ( 1.049868766404200349, 0.2306618581243848609, 0.2411417322834645549 ) ) ;
#66506 = CARTESIAN_POINT ( 'NONE',  ( -1.220472440944881054, 0.1771653543307087630, 0.000000000000000000 ) ) ;
#66507 = CARTESIAN_POINT ( 'NONE',  ( -0.3477690288713905509, -0.6692913385826771977, 0.1292274648535927661 ) ) ;
#66508 = CARTESIAN_POINT ( 'NONE',  ( 0.2362204724409456558, -0.1870078740157479769, 0.3641732283464567677 ) ) ;
#66509 = CARTESIAN_POINT ( 'NONE',  ( 1.607547226907515947, 0.2919332483279780122, 0.05801724265248875412 ) ) ;
#66510 = CARTESIAN_POINT ( 'NONE',  ( 0.6692913385826777528, 0.1771653543307087630, 0.000000000000000000 ) ) ;
#66511 = AXIS2_PLACEMENT_3D ( 'NONE', #63762, #20405, #38919 ) ;
#66512 = CARTESIAN_POINT ( 'NONE',  ( 0.1509186351706045259, -0.05778040916215560624, -0.4822834645669293319 ) ) ;
#66513 = EDGE_CURVE ( 'NONE', #77522, #48621, #20712, .T. ) ;
#66514 = CARTESIAN_POINT ( 'NONE',  ( 0.2925321140481932369, -0.2925321140481931814, -0.3326771653543306728 ) ) ;
#66515 = CARTESIAN_POINT ( 'NONE',  ( -0.6364829396325453192, -0.3162353388693405765, 0.4822834645669290543 ) ) ;
#66516 = CARTESIAN_POINT ( 'NONE',  ( -0.1958661417322836718, 0.3392501089628017219, -1.672572178477690352 ) ) ;
#66517 = CARTESIAN_POINT ( 'NONE',  ( 1.233595800524935227, -0.5023911411419708095, 0.1820866141732285504 ) ) ;
#66518 = CARTESIAN_POINT ( 'NONE',  ( 0.6430446194225729606, -0.4281496062992127816, -0.4176697321401328100 ) ) ;
#66519 = CARTESIAN_POINT ( 'NONE',  ( -0.3871391076115476282, -0.05778040916215522460, 0.4822834645669289988 ) ) ;
#66520 = CARTESIAN_POINT ( 'NONE',  ( -0.3543307086614165824, 0.1771653543307087630, 0.000000000000000000 ) ) ;
#66521 = DIRECTION ( 'NONE',  ( -0.7071067811865489050, -2.189697074797801291E-16, 0.7071067811865460184 ) ) ;
#66522 = CARTESIAN_POINT ( 'NONE',  ( 0.1115485564304470323, 0.1771653543307087630, 0.09757992244046791164 ) ) ;
#66523 = CARTESIAN_POINT ( 'NONE',  ( 0.5314960629921267055, -0.5400638737290844871, 0.3530559997133364547 ) ) ;
#66524 = CARTESIAN_POINT ( 'NONE',  ( -0.5643044619422565855, -0.004921259842519870586, -0.3153832671262229437 ) ) ;
#66526 = CARTESIAN_POINT ( 'NONE',  ( 0.1998031496062992463, 0.3460692066303959202, -1.166010498687663821 ) ) ;
#66525 = VECTOR ( 'NONE', #23803, 39.37007874015748143 ) ;
#66527 = CARTESIAN_POINT ( 'NONE',  ( -1.194225721784776262, -0.4281496062992124485, 0.4176697321401328655 ) ) ;
#66528 = DIRECTION ( 'NONE',  ( 0.000000000000000000, 1.387778780781445676E-15, -1.000000000000000000 ) ) ;
#66529 = ORIENTED_EDGE ( 'NONE', *, *, #22849, .F. ) ;
#66530 = CARTESIAN_POINT ( 'NONE',  ( -1.253280839895012377, -0.08942795157527998196, 0.3641732283464567121 ) ) ;
#66531 = CARTESIAN_POINT ( 'NONE',  ( -0.2362204724409442680, -0.1870078740157480879, -0.4822834645669291653 ) ) ;
#66532 = CARTESIAN_POINT ( 'NONE',  ( -1.502624671916009680, -0.05778040916215560624, -0.4822834645669293319 ) ) ;
#66533 = CARTESIAN_POINT ( 'NONE',  ( -0.9776902887139098386, 0.2952755905511810774, -0.1292274648535930714 ) ) ;
#66534 = DIRECTION ( 'NONE',  ( 0.000000000000000000, 1.000000000000000000, 0.000000000000000000 ) ) ;
#66535 = CARTESIAN_POINT ( 'NONE',  ( 1.174540682414699111, -0.3162353388693405765, 0.4822834645669290543 ) ) ;
#66536 = CARTESIAN_POINT ( 'NONE',  ( 1.049868766404200349, 0.2306618581243848609, 0.2411417322834645549 ) ) ;
#66537 = DIRECTION ( 'NONE',  ( 1.000000000000000000, 0.000000000000000000, -0.000000000000000000 ) ) ;
#66538 = CARTESIAN_POINT ( 'NONE',  ( 1.456692913385827515, 0.2952755905511811885, 0.000000000000000000 ) ) ;
#66539 = CARTESIAN_POINT ( 'NONE',  ( 0.2952755905511810774, 3.179810529374183920E-17, 5.879133660591329580 ) ) ;
#66540 = CARTESIAN_POINT ( 'NONE',  ( -1.305774278215222184, -0.6692913385826773087, -0.1292274648535924053 ) ) ;
#66541 = CARTESIAN_POINT ( 'NONE',  ( -0.2925321140481930704, -0.2925321140481933480, -0.5314960629921260393 ) ) ;
#66542 = EDGE_LOOP ( 'NONE', ( #61170, #26571, #32286, #14970 ) ) ;
#66543 = CARTESIAN_POINT ( 'NONE',  ( -0.5446194225721777693, -0.08942795157527998196, 0.3641732283464567121 ) ) ;
#66544 = CARTESIAN_POINT ( 'NONE',  ( -0.3917322834645670104, -7.196005306013484475E-17, -2.393700787401574992 ) ) ;
#66545 = EDGE_LOOP ( 'NONE', ( #25866, #50857, #6703, #70554 ) ) ;
#66546 = CARTESIAN_POINT ( 'NONE',  ( 0.8005249343832027131, 0.05413385826771666132, 0.4176697321401328100 ) ) ;
#66547 = CARTESIAN_POINT ( 'NONE',  ( -0.09186351706036689768, 0.05413385826771626580, -0.4176697321401330321 ) ) ;
#66548 = CARTESIAN_POINT ( 'NONE',  ( -0.8792650918635160906, -0.4281496062992124485, 0.4176697321401328655 ) ) ;
#66549 = CARTESIAN_POINT ( 'NONE',  ( 1.515748031496063408, 0.1660481256975885056, 0.3530559997133364547 ) ) ;
#66550 = CARTESIAN_POINT ( 'NONE',  ( -0.7349081364829387342, -0.5023911411419708095, 0.1820866141732285504 ) ) ;
#66551 = DIRECTION ( 'NONE',  ( 0.000000000000000000, -1.000000000000000000, 0.000000000000000000 ) ) ;
#66552 = CARTESIAN_POINT ( 'NONE',  ( 0.4527559055118117182, 0.1660481256975883668, -0.3530559997133364547 ) ) ;
#66553 = CARTESIAN_POINT ( 'NONE',  ( 0.5249343832021003964, 0.1283753931104746893, -0.1820866141732285504 ) ) ;
#66554 = CARTESIAN_POINT ( 'NONE',  ( -1.030183727034119867, -0.3162353388693405765, 0.4822834645669290543 ) ) ;
#66555 = CARTESIAN_POINT ( 'NONE',  ( 0.3917322834645668994, 0.1049643490035304522, -1.464547613352018773 ) ) ;
#66556 = CARTESIAN_POINT ( 'NONE',  ( -1.240157480314959759, -0.5400638737290845981, -0.3530559997133363437 ) ) ;
#66557 = FACE_OUTER_BOUND ( 'NONE', #45888, .T. ) ;
#66558 = CARTESIAN_POINT ( 'NONE',  ( 0.9973753280839902091, -0.6046776061558807314, 0.2411417322834647770 ) ) ;
#66559 = CARTESIAN_POINT ( 'NONE',  ( 1.187664041994751285, -0.08942795157527998196, 0.3641732283464567121 ) ) ;
#66560 = VERTEX_POINT ( 'NONE', #46629 ) ;
#66561 = CARTESIAN_POINT ( 'NONE',  ( -0.3392501089628017219, -0.1958661417322836995, -2.883877583498374531 ) ) ;
#66562 = CARTESIAN_POINT ( 'NONE',  ( -0.4724409448818890911, -0.1870078740157480879, -0.4822834645669291653 ) ) ;
#66563 = ORIENTED_EDGE ( 'NONE', *, *, #32628, .F. ) ;
#66564 = CARTESIAN_POINT ( 'NONE',  ( 0.4724409448818904789, -0.1870078740157479769, 0.3641732283464567677 ) ) ;
#66565 = CARTESIAN_POINT ( 'NONE',  ( -1.318897637795274802, -0.5400638737290845981, -0.3530559997133363437 ) ) ;
#66566 = CARTESIAN_POINT ( 'NONE',  ( 0.8398950131233602345, 0.2306618581243847221, -0.2411417322834647770 ) ) ;
#66567 = CARTESIAN_POINT ( 'NONE',  ( 0.8595800524934390507, -0.05778040916215560624, -0.4822834645669293319 ) ) ;
#66568 = CARTESIAN_POINT ( 'NONE',  ( -0.2165354330708654795, -0.5400638737290845981, -0.3530559997133363437 ) ) ;
#66569 = CARTESIAN_POINT ( 'NONE',  ( -0.4921259842519677963, 0.1660481256975883668, -0.3530559997133364547 ) ) ;
#66570 = CARTESIAN_POINT ( 'NONE',  ( 0.1958661417322836440, -0.3392501089628017219, -2.223753280839895208 ) ) ;
#66571 = CARTESIAN_POINT ( 'NONE',  ( -1.548556430446193399, 0.2306618581243848609, 0.2411417322834645549 ) ) ;
#66572 = CARTESIAN_POINT ( 'NONE',  ( -0.8070866141732276899, 0.1660481256975883668, -0.3530559997133364547 ) ) ;
#66573 = CARTESIAN_POINT ( 'NONE',  ( -0.3740157480314953431, 0.07958543189024085140, 0.2665933059059887866 ) ) ;
#66574 = CARTESIAN_POINT ( 'NONE',  ( 1.384514435695538559, 0.2952755905511810774, -0.1292274648535930714 ) ) ;
#66575 = CARTESIAN_POINT ( 'NONE',  ( 1.581364829396326277, -0.3162353388693409650, -0.4822834645669289433 ) ) ;
#66576 = CARTESIAN_POINT ( 'NONE',  ( -0.5774278215223089816, 0.2306618581243847221, -0.2411417322834647770 ) ) ;
#66577 = CARTESIAN_POINT ( 'NONE',  ( -0.1998031496062994405, 0.3460692066303957537, 0.06758530183727033680 ) ) ;
#66578 = CARTESIAN_POINT ( 'NONE',  ( 0.8595800524934390507, -0.05778040916215560624, -0.4822834645669293319 ) ) ;
#66579 = CARTESIAN_POINT ( 'NONE',  ( -0.2925321140481932924, 0.2925321140481931814, -1.751968503937007648 ) ) ;
#66580 = DIRECTION ( 'NONE',  ( -0.000000000000000000, 1.000000000000000000, -0.000000000000000000 ) ) ;
#66581 = CARTESIAN_POINT ( 'NONE',  ( -0.07874015748031421014, -0.1870078740157479769, 0.4822834645669291653 ) ) ;
#66582 = CARTESIAN_POINT ( 'NONE',  ( -1.325459317585300889, -0.004921259842519576551, 0.3153832671262227771 ) ) ;
#66584 = CARTESIAN_POINT ( 'NONE',  ( -0.4563452811745912219, 0.01305114060239447385, 2.130073781772667374 ) ) ;
#66583 = CARTESIAN_POINT ( 'NONE',  ( 1.200787401574803681, 0.07958543189024085140, 0.2665933059059887866 ) ) ;
#66585 = CARTESIAN_POINT ( 'NONE',  ( 0.4724409448818896462, 0.1265901696524990294, -0.8313648293963252778 ) ) ;
#66586 = CARTESIAN_POINT ( 'NONE',  ( 1.207349081364829990, 0.1283753931104748280, 0.1820866141732283561 ) ) ;
#66587 = CARTESIAN_POINT ( 'NONE',  ( 1.397637795275591177, -0.5400638737290844871, 0.3530559997133364547 ) ) ;
#66588 = AXIS2_PLACEMENT_3D ( 'NONE', #8683, #34353, #53689 ) ;
#66589 = CARTESIAN_POINT ( 'NONE',  ( -0.2891555358219909388, -0.2891555358219912164, -0.2933070866141732624 ) ) ;
#66590 = CARTESIAN_POINT ( 'NONE',  ( -0.1968503937007867743, -0.6692913385826771977, 8.415575281601705876E-17 ) ) ;
#66591 = DIRECTION ( 'NONE',  ( 1.408710688920637755E-15, -1.000000000000000000, 4.918487082195260922E-30 ) ) ;
#66592 = CARTESIAN_POINT ( 'NONE',  ( 1.213910761154856299, -0.5511811023622048555, -0.09757992244046775898 ) ) ;
#66593 = CARTESIAN_POINT ( 'NONE',  ( -0.1377952755905504645, 0.1660481256975885056, 0.3530559997133364547 ) ) ;
#66594 = CARTESIAN_POINT ( 'NONE',  ( -0.3420746716998660508, -0.1974969037888706924, -0.4442257217847768724 ) ) ;
#66595 = EDGE_CURVE ( 'NONE', #57500, #75161, #78226, .T. ) ;
#66596 = CARTESIAN_POINT ( 'NONE',  ( 1.325459317585302665, -0.4281496062992124485, 0.4176697321401328655 ) ) ;
#66597 = CARTESIAN_POINT ( 'NONE',  ( 0.4855643044619428750, 0.05413385826771666132, 0.4176697321401328100 ) ) ;
#66598 = CARTESIAN_POINT ( 'NONE',  ( 0.4527559055118117182, 0.07958543189024071263, -0.2665933059059888421 ) ) ;
#66599 = CARTESIAN_POINT ( 'NONE',  ( -0.01569160312983191446, 1.062992125984252967, -1.122047244094488194 ) ) ;
#66600 = CARTESIAN_POINT ( 'NONE',  ( 0.3280839895013130669, -0.3690944881889765550, -0.3153832671262227771 ) ) ;
#66601 = CARTESIAN_POINT ( 'NONE',  ( -1.594488188976377119, 0.1660481256975883668, -0.3530559997133364547 ) ) ;
#66602 = CARTESIAN_POINT ( 'NONE',  ( -0.3460692066303960313, 0.1998031496062989965, -1.520341207349081403 ) ) ;
#66603 = CARTESIAN_POINT ( 'NONE',  ( 0.7545931758530189937, 0.2952755905511810774, -0.1292274648535930714 ) ) ;
#66604 = CARTESIAN_POINT ( 'NONE',  ( -0.3917322834645669549, -0.1049643490035306603, -0.9829396325459317518 ) ) ;
#66605 = CARTESIAN_POINT ( 'NONE',  ( 0.8761506516392508770, -4.927456884911482678E-16, 0.4445507791589062840 ) ) ;
#66606 = CARTESIAN_POINT ( 'NONE',  ( 0.000000000000000000, 2.559055118110236560, 0.000000000000000000 ) ) ;
#66607 = CARTESIAN_POINT ( 'NONE',  ( -0.1181102362204717315, 0.1771653543307087630, 0.000000000000000000 ) ) ;
#66608 = CARTESIAN_POINT ( 'NONE',  ( -0.09186351706036663400, -0.4281496062992124485, 0.4176697321401328655 ) ) ;
#66609 = CARTESIAN_POINT ( 'NONE',  ( 1.430446194225722500, -0.3690944881889765550, -0.3153832671262227771 ) ) ;
#66610 = CARTESIAN_POINT ( 'NONE',  ( -1.469816272965878357, -0.5023911411419708095, -0.1820866141732282451 ) ) ;
#66611 = CARTESIAN_POINT ( 'NONE',  ( -1.240157480314959759, 0.1660481256975885056, 0.3530559997133364547 ) ) ;
#66612 = CARTESIAN_POINT ( 'NONE',  ( 0.5380577427821529035, -0.4281496062992124485, 0.4176697321401328655 ) ) ;
#66613 = CARTESIAN_POINT ( 'NONE',  ( 1.469816272965879911, -0.6046776061558807314, 0.2411417322834647770 ) ) ;
#66614 = CARTESIAN_POINT ( 'NONE',  ( 2.795275590551181910, 1.568468489416428469, 0.000000000000000000 ) ) ;
#66615 = CARTESIAN_POINT ( 'NONE',  ( 0.4527559055118117182, -0.5400638737290844871, 0.3530559997133364547 ) ) ;
#66616 = CARTESIAN_POINT ( 'NONE',  ( -0.1070741851644056997, 0.3996062992125984925, 0.2316272965879264956 ) ) ;
#66617 = CARTESIAN_POINT ( 'NONE',  ( 1.555118110236221041, 0.1660481256975883668, -0.3530559997133364547 ) ) ;
#66618 = CARTESIAN_POINT ( 'NONE',  ( 1.082677165354331228, 0.1660481256975883668, -0.3530559997133364547 ) ) ;
#66619 = CARTESIAN_POINT ( 'NONE',  ( -1.463254593175852492, -0.5511811023622048555, -0.09757992244046775898 ) ) ;
#66620 = CARTESIAN_POINT ( 'NONE',  ( 1.227034120734908917, 0.1771653543307087075, -0.09757992244046823083 ) ) ;
#66621 = CARTESIAN_POINT ( 'NONE',  ( -1.541994750656167090, -0.5511811023622048555, -0.09757992244046775898 ) ) ;
#66622 = CARTESIAN_POINT ( 'NONE',  ( -0.8727034120734901146, -0.2845877964562159024, 0.3641732283464567677 ) ) ;
#66623 = CARTESIAN_POINT ( 'NONE',  ( 1.502624671916010790, -0.3162353388693409650, -0.4822834645669289433 ) ) ;
#66624 = CARTESIAN_POINT ( 'NONE',  ( 0.5708661417322841158, -0.4536011799217368745, -0.2665933059059886201 ) ) ;
#66625 = CARTESIAN_POINT ( 'NONE',  ( 0.2624671916010504757, 0.2306618581243848609, 0.2411417322834645549 ) ) ;
#66626 = CARTESIAN_POINT ( 'NONE',  ( 1.246719160104987623, -0.4281496062992124485, 0.4176697321401328655 ) ) ;
#66627 = CARTESIAN_POINT ( 'NONE',  ( -0.5577427821522301654, -0.3162353388693405765, 0.4822834645669290543 ) ) ;
#66628 = CARTESIAN_POINT ( 'NONE',  ( 0.2559055118110243332, -0.4536011799217368745, -0.2665933059059886201 ) ) ;
#66629 = CARTESIAN_POINT ( 'NONE',  ( 1.167979002624672580, 0.05413385826771626580, -0.4176697321401330321 ) ) ;
#66630 =( BOUNDED_CURVE ( )  B_SPLINE_CURVE ( 2, ( #23822, #81915, #49491, #42343, #75183, #17529, #28897, #44697, #16290, #68856, #11205, #4877, #25356 ),
 .UNSPECIFIED., .F., .F. ) 
 B_SPLINE_CURVE_WITH_KNOTS ( ( 3, 2, 2, 2, 2, 2, 3 ),
 ( 0.3375000000000000222, 0.3416666666666666741, 0.3458333333333333259, 0.3499999999999999778, 0.3541666666666666852, 0.3583333333333333370, 0.3624999999999999889 ),
 .UNSPECIFIED. ) 
 CURVE ( )  GEOMETRIC_REPRESENTATION_ITEM ( )  RATIONAL_B_SPLINE_CURVE ( ( 1.000000000000000000, 0.9659258262890683122, 1.000000000000000000, 0.9659258262890683122, 1.000000000000000000, 0.9659258262890683122, 1.000000000000000000, 0.9659258262890683122, 1.000000000000000000, 0.9659258262890683122, 1.000000000000000000, 0.9659258262890683122, 1.000000000000000000 ) ) 
 REPRESENTATION_ITEM ( '' )  );
#66631 = CARTESIAN_POINT ( 'NONE',  ( -1.633858267716534529, 0.1660481256975885056, 0.3530559997133364547 ) ) ;
#66632 = CARTESIAN_POINT ( 'NONE',  ( -0.8530183727034112984, -0.4281496062992127816, -0.4176697321401328100 ) ) ;
#66634 = CARTESIAN_POINT ( 'NONE',  ( -0.2925321140481930704, -0.2925321140481933480, -0.6889763779527556808 ) ) ;
#66633 = CARTESIAN_POINT ( 'NONE',  ( -1.456692913385826182, -0.5511811023622047445, 6.969142054262312111E-17 ) ) ;
#66635 = CARTESIAN_POINT ( 'NONE',  ( -0.2160876265729054779, 1.080600139074564536, 0.2277452782751286098 ) ) ;
#66637 = AXIS2_PLACEMENT_3D ( 'NONE', #27849, #15653, #9327 ) ;
#66636 = CARTESIAN_POINT ( 'NONE',  ( -0.9317585301837263412, -0.4281496062992127816, -0.4176697321401328100 ) ) ;
#66638 = CARTESIAN_POINT ( 'NONE',  ( -0.05905511811023545637, -0.5400638737290845981, -0.3530559997133363437 ) ) ;
#66639 = ADVANCED_FACE ( 'NONE', ( #15498 ), #28111, .T. ) ;
#66640 = CARTESIAN_POINT ( 'NONE',  ( -0.2925321140481930704, -0.2925321140481933480, -2.893700787401574992 ) ) ;
#66641 = CARTESIAN_POINT ( 'NONE',  ( 0.1974969037888706369, -0.3420746716998659953, -2.296587926509186417 ) ) ;
#66642 = ORIENTED_EDGE ( 'NONE', *, *, #27425, .T. ) ;
#66643 = CARTESIAN_POINT ( 'NONE',  ( 0.8333333333333340365, -0.5511811023622046335, 0.09757992244046803654 ) ) ;
#66644 = CARTESIAN_POINT ( 'NONE',  ( 0.1049643490035304938, -0.3917322834645669549, -1.022309711286088829 ) ) ;
#66645 = CARTESIAN_POINT ( 'NONE',  ( 1.141732283464567566, 0.2952755905511811885, 0.000000000000000000 ) ) ;
#66646 = CARTESIAN_POINT ( 'NONE',  ( -1.646051170424378096, -0.1870078740157480046, 1.254653134982923898E-17 ) ) ;
#66647 = ADVANCED_FACE ( 'NONE', ( #71906 ), #58909, .F. ) ;
#66648 = CARTESIAN_POINT ( 'NONE',  ( -1.200787401574802349, 0.07958543189024071263, -0.2665933059059888421 ) ) ;
#66649 = CARTESIAN_POINT ( 'NONE',  ( 1.410761154855643795, -0.05778040916215560624, -0.4822834645669293319 ) ) ;
#66650 = CARTESIAN_POINT ( 'NONE',  ( -1.423884514435694859, -0.3162353388693405765, 0.4822834645669290543 ) ) ;
#66651 = CARTESIAN_POINT ( 'NONE',  ( 0.1958661417322836162, -0.3392501089628018329, -0.4868573246381086017 ) ) ;
#66652 = CARTESIAN_POINT ( 'NONE',  ( -0.1377952755905504645, -0.5400638737290845981, -0.3530559997133363437 ) ) ;
#66653 = CARTESIAN_POINT ( 'NONE',  ( -0.4527559055118102749, 0.07958543189024085140, 0.2665933059059887866 ) ) ;
#66654 = CARTESIAN_POINT ( 'NONE',  ( 0.7414698162729663755, -0.6692913385826773087, -0.1292274648535924053 ) ) ;
#66655 = CARTESIAN_POINT ( 'NONE',  ( 0.3149606299212603933, -0.1870078740157479769, 0.4822834645669291653 ) ) ;
#66656 = CARTESIAN_POINT ( 'NONE',  ( 0.000000000000000000, 1.062992125984252745, 1.122047244094488194 ) ) ;
#66657 = CARTESIAN_POINT ( 'NONE',  ( 0.2925321140481932369, -0.2925321140481932369, -2.933070866141732402 ) ) ;
#66658 = CARTESIAN_POINT ( 'NONE',  ( -0.3917322834645670104, -0.1049643490035307020, -1.459993069062679005 ) ) ;
#66659 = CARTESIAN_POINT ( 'NONE',  ( 0.7677165354330716118, 0.1660481256975883668, -0.3530559997133364547 ) ) ;
#66660 = CARTESIAN_POINT ( 'NONE',  ( 0.01312335958005323398, 0.05413385826771666132, 0.4176697321401328100 ) ) ;
#66661 = CARTESIAN_POINT ( 'NONE',  ( -1.049868766404198794, -0.6046776061558807314, 0.2411417322834647770 ) ) ;
#66662 = CARTESIAN_POINT ( 'NONE',  ( 1.410761154855643795, -0.3162353388693405765, 0.4822834645669290543 ) ) ;
#66663 = CARTESIAN_POINT ( 'NONE',  ( 1.010498687664042716, -0.4281496062992124485, 0.4176697321401328655 ) ) ;
#66664 = CARTESIAN_POINT ( 'NONE',  ( 0.2867679344610365999, 0.2867679344610365999, -0.6948818897637795144 ) ) ;
#66665 = CARTESIAN_POINT ( 'NONE',  ( -0.1706036745406816491, -0.4281496062992124485, 0.4176697321401328655 ) ) ;
#66666 = CARTESIAN_POINT ( 'NONE',  ( 0.4658792650918641698, -0.05778040916215560624, -0.4822834645669293319 ) ) ;
#66667 = CARTESIAN_POINT ( 'NONE',  ( -0.1049868766404193215, -0.6046776061558807314, 0.2411417322834647770 ) ) ;
#66668 = CARTESIAN_POINT ( 'NONE',  ( 0.6561679790026253567, -0.5023911411419708095, -0.1820866141732282451 ) ) ;
#66669 = CARTESIAN_POINT ( 'NONE',  ( -1.548556430446193399, 0.2306618581243848609, 0.2411417322834645549 ) ) ;
#66670 = CARTESIAN_POINT ( 'NONE',  ( -1.587926509186350810, -0.4281496062992124485, 0.4176697321401328655 ) ) ;
#66671 = CARTESIAN_POINT ( 'NONE',  ( 0.5511811023622054106, -0.1870078740157480879, -0.4822834645669291653 ) ) ;
#66672 = CARTESIAN_POINT ( 'NONE',  ( -0.1882840440700958018, -0.3436793299040552530, -1.929133858267716439 ) ) ;
#66673 = EDGE_CURVE ( 'NONE', #44273, #81026, #16602, .T. ) ;
#66674 = CARTESIAN_POINT ( 'NONE',  ( -0.1958661417322834220, -0.3392501089628018884, -2.262467191601049699 ) ) ;
#66675 = VERTEX_POINT ( 'NONE', #7515 ) ;
#66676 = CARTESIAN_POINT ( 'NONE',  ( -9.787531504996567848E-17, 0.3996062992125986035, -0.4724409448818898127 ) ) ;
#66677 = ORIENTED_EDGE ( 'NONE', *, *, #68728, .T. ) ;
#66678 = CARTESIAN_POINT ( 'NONE',  ( 1.213910761154856299, 0.2952755905511811885, 0.1292274648535926551 ) ) ;
#66679 = CARTESIAN_POINT ( 'NONE',  ( 0.3543307086614179147, 0.1771653543307087630, 0.000000000000000000 ) ) ;
#66680 = VECTOR ( 'NONE', #59657, 39.37007874015748143 ) ;
#66681 = AXIS2_PLACEMENT_3D ( 'NONE', #56120, #25368, #30864 ) ;
#66682 = CARTESIAN_POINT ( 'NONE',  ( 0.000000000000000000, 2.755905511811024056, 0.000000000000000000 ) ) ;
#66683 = FACE_OUTER_BOUND ( 'NONE', #60220, .T. ) ;
#66684 = CARTESIAN_POINT ( 'NONE',  ( -0.2867679344610365999, 0.2867679344610364889, -1.364173228346456268 ) ) ;
#66685 = EDGE_CURVE ( 'NONE', #45904, #58800, #80523, .T. ) ;
#66686 = CARTESIAN_POINT ( 'NONE',  ( 0.1070741851644054776, -0.3996062992125984925, -1.894356955380577023 ) ) ;
#66687 = CARTESIAN_POINT ( 'NONE',  ( -1.627296587926508442, 0.2306618581243848609, 0.2411417322834645549 ) ) ;
#66688 = CARTESIAN_POINT ( 'NONE',  ( -0.4133858267716528645, 0.1660481256975883668, -0.3530559997133364547 ) ) ;
#66689 = CARTESIAN_POINT ( 'NONE',  ( 1.227034120734908917, -0.6692913385826771977, 0.1292274648535927661 ) ) ;
#66690 = VERTEX_POINT ( 'NONE', #7833 ) ;
#66691 = CARTESIAN_POINT ( 'NONE',  ( 1.614173228346457378, 0.2952755905511811885, 0.000000000000000000 ) ) ;
#66692 = CARTESIAN_POINT ( 'NONE',  ( 1.594488188976378673, -0.4536011799217368745, -0.2665933059059886201 ) ) ;
#66693 = PRODUCT_CONTEXT ( 'NONE', #12679, 'mechanical' ) ;
#66694 = LINE ( 'NONE', #28790, #33094 ) ;
#66695 = DIRECTION ( 'NONE',  ( 0.000000000000000000, 1.000000000000000000, 0.000000000000000000 ) ) ;
#66696 = CARTESIAN_POINT ( 'NONE',  ( -1.266404199475064773, -0.08942795157528024563, -0.3641732283464568787 ) ) ;
#66697 = ADVANCED_FACE ( 'NONE', ( #27174 ), #78548, .F. ) ;
#66698 = CARTESIAN_POINT ( 'NONE',  ( 1.586052503253845503, 0.7480314960629931287, 0.1653254495020587966 ) ) ;
#66699 = CARTESIAN_POINT ( 'NONE',  ( 0.01312335958005323398, -0.4281496062992127816, -0.4176697321401328100 ) ) ;
#66700 = AXIS2_PLACEMENT_3D ( 'NONE', #38076, #37664, #13670 ) ;
#66702 = DIRECTION ( 'NONE',  ( -0.000000000000000000, -1.000000000000000000, -0.000000000000000000 ) ) ;
#66701 = CARTESIAN_POINT ( 'NONE',  ( 1.430446194225722500, -0.4281496062992127816, -0.4176697321401328100 ) ) ;
#66703 = CARTESIAN_POINT ( 'NONE',  ( -0.8989501312335946848, 0.1771653543307087075, -0.09757992244046823083 ) ) ;
#66704 = CARTESIAN_POINT ( 'NONE',  ( 0.6496062992125991586, -0.5400638737290845981, -0.3530559997133363437 ) ) ;
#66705 = CARTESIAN_POINT ( 'NONE',  ( 1.227034120734908917, -0.5511811023622046335, 0.09757992244046803654 ) ) ;
#66706 = CARTESIAN_POINT ( 'NONE',  ( -0.3917322834645670659, 0.1049643490035301607, -1.372684096291651556 ) ) ;
#66707 = CARTESIAN_POINT ( 'NONE',  ( -0.7086614173228339419, -0.1870078740157480601, -0.3641732283464567677 ) ) ;
#66708 = CARTESIAN_POINT ( 'NONE',  ( 1.207349081364829990, 0.2306618581243848609, 0.2411417322834645549 ) ) ;
#66709 = CARTESIAN_POINT ( 'NONE',  ( -2.362204724409448620, 0.03937007874015751446, -2.474278114140802984E-14 ) ) ;
#66710 = CARTESIAN_POINT ( 'NONE',  ( 0.3740157480314966754, 0.1660481256975883668, -0.3530559997133364547 ) ) ;
#66711 = CARTESIAN_POINT ( 'NONE',  ( -0.7349081364829387342, -0.5023911411419708095, 0.1820866141732285504 ) ) ;
#66712 = CARTESIAN_POINT ( 'NONE',  ( -0.4527559055118102749, 0.07958543189024085140, 0.2665933059059887866 ) ) ;
#66713 = CARTESIAN_POINT ( 'NONE',  ( -0.2624671916010490880, 0.2306618581243847221, -0.2411417322834647770 ) ) ;
#66714 = CARTESIAN_POINT ( 'NONE',  ( -1.482939632545930975, -0.004921259842519576551, 0.3153832671262227771 ) ) ;
#66715 = CARTESIAN_POINT ( 'NONE',  ( 4.797336870675656522E-17, -0.3917322834645670659, -0.07547863336714100146 ) ) ;
#66716 = CARTESIAN_POINT ( 'NONE',  ( 0.6758530183727039509, 0.2952755905511810774, -0.1292274648535930714 ) ) ;
#66717 = CARTESIAN_POINT ( 'NONE',  ( -0.1938976377952756625, 0.1938976377952755792, -0.3740157480314971750 ) ) ;
#66718 = CARTESIAN_POINT ( 'NONE',  ( -0.3458507752293909498, 0.3458507752293907833, -1.671259842519685179 ) ) ;
#66719 = CARTESIAN_POINT ( 'NONE',  ( -0.9055118110236215490, 0.2952755905511811885, 0.000000000000000000 ) ) ;
#66720 = CARTESIAN_POINT ( 'NONE',  ( -0.03937007874015669567, -0.5511811023622047445, 6.969142054262312111E-17 ) ) ;
#66721 = CARTESIAN_POINT ( 'NONE',  ( -1.450131233595799651, 0.2952755905511810774, -0.1292274648535930714 ) ) ;
#66722 = CARTESIAN_POINT ( 'NONE',  ( 0.4855643044619430415, -0.3690944881889765550, -0.3153832671262227771 ) ) ;
#66723 = CARTESIAN_POINT ( 'NONE',  ( -0.5380577427821514602, -0.3690944881889765550, -0.3153832671262227771 ) ) ;
#66724 = CARTESIAN_POINT ( 'NONE',  ( -0.9383202099737524282, -0.05778040916215522460, 0.4822834645669289988 ) ) ;
#66725 = CARTESIAN_POINT ( 'NONE',  ( -1.515748031496062076, 0.1660481256975883668, -0.3530559997133364547 ) ) ;
#66726 = CARTESIAN_POINT ( 'NONE',  ( 1.207349081364829990, 0.2306618581243848609, 0.2411417322834645549 ) ) ;
#66727 = DIRECTION ( 'NONE',  ( -0.000000000000000000, 1.000000000000000000, -0.000000000000000000 ) ) ;
#66728 = CARTESIAN_POINT ( 'NONE',  ( 0.8530183727034128527, -0.3690944881889763329, 0.3153832671262228327 ) ) ;
#66729 = CARTESIAN_POINT ( 'NONE',  ( 0.5774278215223104249, 0.2306618581243848609, 0.2411417322834645549 ) ) ;
#66730 = LINE ( 'NONE', #31189, #12490 ) ;
#66731 = CARTESIAN_POINT ( 'NONE',  ( 1.338582677165355062, -0.1870078740157480601, -0.3641732283464567677 ) ) ;
#66732 = ORIENTED_EDGE ( 'NONE', *, *, #70646, .T. ) ;
#66733 = CARTESIAN_POINT ( 'NONE',  ( -0.1058382717557497660, -0.3949938075777411073, 0.1660104986876640432 ) ) ;
#66734 = CARTESIAN_POINT ( 'NONE',  ( -1.207349081364828436, -0.5023911411419708095, 0.1820866141732285504 ) ) ;
#66735 = CARTESIAN_POINT ( 'NONE',  ( -0.3018372703412066094, -0.4281496062992127816, -0.4176697321401328100 ) ) ;
#66736 = CARTESIAN_POINT ( 'NONE',  ( 0.3674540682414705883, 0.2306618581243847221, -0.2411417322834647770 ) ) ;
#66737 = VECTOR ( 'NONE', #20414, 39.37007874015748854 ) ;
#66738 = CARTESIAN_POINT ( 'NONE',  ( -1.397637795275589623, 0.07958543189024085140, 0.2665933059059887866 ) ) ;
#66739 = CARTESIAN_POINT ( 'NONE',  ( -0.1070741851644056997, 0.3996062992125984925, -2.130577427821522818 ) ) ;
#66740 = CARTESIAN_POINT ( 'NONE',  ( -1.443569553805773564, -0.6046776061558807314, 0.2411417322834647770 ) ) ;
#66741 = VECTOR ( 'NONE', #22201, 39.37007874015748143 ) ;
#66742 = VECTOR ( 'NONE', #70552, 39.37007874015748143 ) ;
#66743 = CARTESIAN_POINT ( 'NONE',  ( 0.6036745406824154392, 0.2306618581243847221, -0.2411417322834647770 ) ) ;
#66744 = CARTESIAN_POINT ( 'NONE',  ( 0.01968503937007957949, -0.5400638737290845981, -0.3530559997133363437 ) ) ;
#66745 = CARTESIAN_POINT ( 'NONE',  ( 1.122047244094488860, 0.1660481256975885056, 0.3530559997133364547 ) ) ;
#66747 = EDGE_CURVE ( 'NONE', #78156, #77294, #72633, .T. ) ;
#66746 = PLANE ( 'NONE',  #29162 ) ;
#66748 = CARTESIAN_POINT ( 'NONE',  ( -0.1070741851644051862, -0.3996062992125987146, -1.174540682414698001 ) ) ;
#66749 = CARTESIAN_POINT ( 'NONE',  ( -0.3420746716998659953, -0.1974969037888706647, -1.154855643044619518 ) ) ;
#66750 = CARTESIAN_POINT ( 'NONE',  ( 0.1998031496062994405, -0.3460692066303958092, -2.296587926509186417 ) ) ;
#66751 = CARTESIAN_POINT ( 'NONE',  ( -0.1972978822260921805, -0.2198823481317033202, 0.1376690760605703556 ) ) ;
#66752 = CARTESIAN_POINT ( 'NONE',  ( -0.3392501089628019995, 0.1958661417322832277, -0.3333333333333333148 ) ) ;
#66753 = CARTESIAN_POINT ( 'NONE',  ( -0.06561679790026180015, -0.3690944881889765550, -0.3153832671262227771 ) ) ;
#66754 = CARTESIAN_POINT ( 'NONE',  ( -0.4921259842519677963, -0.5400638737290844871, 0.3530559997133364547 ) ) ;
#66755 = CARTESIAN_POINT ( 'NONE',  ( 0.8923884514435701520, -0.6046776061558809534, -0.2411417322834644161 ) ) ;
#66756 = CARTESIAN_POINT ( 'NONE',  ( -0.3949938075777409963, -7.255918531996591613E-17, -1.690944881889764329 ) ) ;
#66757 = CARTESIAN_POINT ( 'NONE',  ( -0.1706036745406816491, -0.004921259842519870586, -0.3153832671262229437 ) ) ;
#66758 = CARTESIAN_POINT ( 'NONE',  ( -0.9514435695538050464, -0.05778040916215560624, -0.4822834645669293319 ) ) ;
#66759 = CARTESIAN_POINT ( 'NONE',  ( 1.489501312335958172, -0.05778040916215560624, -0.4822834645669293319 ) ) ;
#66760 = CARTESIAN_POINT ( 'NONE',  ( 0.1265901696524990294, -0.4724409448818896462, -2.132545931758530244 ) ) ;
#66761 = CARTESIAN_POINT ( 'NONE',  ( 0.000000000000000000, 0.03937007874015751446, -2.362204724409448620 ) ) ;
#66762 = VECTOR ( 'NONE', #7892, 39.37007874015748143 ) ;
#66763 = ORIENTED_EDGE ( 'NONE', *, *, #82446, .F. ) ;
#66764 = ORIENTED_EDGE ( 'NONE', *, *, #64982, .T. ) ;
#66765 = CARTESIAN_POINT ( 'NONE',  ( 0.9842519685039375910, 0.2952755905511811885, 0.000000000000000000 ) ) ;
#66766 = CARTESIAN_POINT ( 'NONE',  ( 1.496062992125984703, -0.1870078740157480601, -0.3641732283464567677 ) ) ;
#66768 = CARTESIAN_POINT ( 'NONE',  ( -1.128608923884513837, 0.2306618581243847221, -0.2411417322834647770 ) ) ;
#66767 = CARTESIAN_POINT ( 'NONE',  ( -1.062992125984250968, -0.5511811023622047445, 6.969142054262312111E-17 ) ) ;
#66769 = CARTESIAN_POINT ( 'NONE',  ( 0.1049643490035303689, 0.3917322834645668994, -2.278195907315273327 ) ) ;
#66770 = CARTESIAN_POINT ( 'NONE',  ( -1.010849322905837955, 0.004960608223778821026, 0.3437734562760189072 ) ) ;
#66771 = CARTESIAN_POINT ( 'NONE',  ( 1.292650918635171564, -0.6692913385826773087, -0.1292274648535924053 ) ) ;
#66772 = CARTESIAN_POINT ( 'NONE',  ( -1.581364829396324945, -0.3162353388693405765, 0.4822834645669290543 ) ) ;
#66773 = CARTESIAN_POINT ( 'NONE',  ( 0.09186351706036799403, -0.4281496062992127816, -0.4176697321401328100 ) ) ;
#66774 = CARTESIAN_POINT ( 'NONE',  ( 0.05249343832021075018, 0.2306618581243847221, -0.2411417322834647770 ) ) ;
#66775 = CARTESIAN_POINT ( 'NONE',  ( -1.108923884514435132, -0.05778040916215560624, -0.4822834645669293319 ) ) ;
#66776 = CARTESIAN_POINT ( 'NONE',  ( 0.1958661417322836440, -0.3392501089628017219, 0.1384514435695537171 ) ) ;
#66777 = CARTESIAN_POINT ( 'NONE',  ( 0.3871391076115492380, -0.05778040916215560624, -0.4822834645669293319 ) ) ;
#66778 = CARTESIAN_POINT ( 'NONE',  ( 0.2867679344610365999, 0.2867679344610365999, -1.704724409448818978 ) ) ;
#66779 = CARTESIAN_POINT ( 'NONE',  ( -1.108923884514435132, -0.08942795157528024563, -0.3641732283464568787 ) ) ;
#66780 = VERTEX_POINT ( 'NONE', #41473 ) ;
#66781 = CARTESIAN_POINT ( 'NONE',  ( -0.3949938075777409963, -7.255918531996591613E-17, -2.401574803149606474 ) ) ;
#66782 = ORIENTED_EDGE ( 'NONE', *, *, #11244, .T. ) ;
#66783 = CARTESIAN_POINT ( 'NONE',  ( 1.595398199321655275, 1.288687073698532526, 0.1559797534342495240 ) ) ;
#66784 = CARTESIAN_POINT ( 'NONE',  ( -1.417322834645668772, -0.1870078740157479769, 0.4822834645669291653 ) ) ;
#66785 = CARTESIAN_POINT ( 'NONE',  ( -1.522309711286088607, -0.6046776061558807314, 0.2411417322834647770 ) ) ;
#66786 = CARTESIAN_POINT ( 'NONE',  ( -0.3460692066303960868, 0.1998031496062990242, -0.6561679790026246906 ) ) ;
#66787 = CARTESIAN_POINT ( 'NONE',  ( -1.430446194225721390, -0.4281496062992124485, 0.4176697321401328655 ) ) ;
#66788 = CARTESIAN_POINT ( 'NONE',  ( -1.522309711286088607, 0.2306618581243847221, -0.2411417322834647770 ) ) ;
#66789 = DIRECTION ( 'NONE',  ( -0.5773502691896310601, -0.5773502691896310601, -0.5773502691896149619 ) ) ;
#66790 = DIRECTION ( 'NONE',  ( 0.000000000000000000, 1.000000000000000000, 0.000000000000000000 ) ) ;
#66791 = CARTESIAN_POINT ( 'NONE',  ( -0.3917322834645669549, -0.1049643490035306603, 0.1843832020997374643 ) ) ;
#66792 = CARTESIAN_POINT ( 'NONE',  ( -0.3018372703412066094, -0.3690944881889765550, -0.3153832671262227771 ) ) ;
#66793 = CARTESIAN_POINT ( 'NONE',  ( -0.6430446194225716283, -0.3690944881889763329, 0.3153832671262228327 ) ) ;
#66794 = CARTESIAN_POINT ( 'NONE',  ( -1.338582677165353729, -0.1870078740157479769, 0.4822834645669291653 ) ) ;
#66795 = CARTESIAN_POINT ( 'NONE',  ( 0.9842519685039375910, 0.2952755905511811885, 0.000000000000000000 ) ) ;
#66796 = CARTESIAN_POINT ( 'NONE',  ( -1.056430446194224881, -0.6692913385826771977, 0.1292274648535927661 ) ) ;
#66797 = CARTESIAN_POINT ( 'NONE',  ( -0.3917322834645669549, -0.1049643490035306603, -0.03805774278215218187 ) ) ;
#66798 = ORIENTED_EDGE ( 'NONE', *, *, #75407, .F. ) ;
#66799 = CARTESIAN_POINT ( 'NONE',  ( -1.338582677165353729, -0.1870078740157479769, 0.4822834645669291653 ) ) ;
#66800 = FACE_OUTER_BOUND ( 'NONE', #18723, .T. ) ;
#66801 = CARTESIAN_POINT ( 'NONE',  ( -1.686351706036744558, 0.2952755905511810774, -0.1292274648535930714 ) ) ;
#66802 = CARTESIAN_POINT ( 'NONE',  ( -0.4724409448818899238, 0.1265901696524986686, -1.450131233595800317 ) ) ;
#66803 = CARTESIAN_POINT ( 'NONE',  ( 1.857147851633400792, 1.070284760220071352, -0.08454815954499718400 ) ) ;
#66804 = CARTESIAN_POINT ( 'NONE',  ( -0.3392501089628017219, -0.1958661417322836718, -0.6745406824146981117 ) ) ;
#66805 = VECTOR ( 'NONE', #16186, 39.37007874015748143 ) ;
#66806 = CARTESIAN_POINT ( 'NONE',  ( 4.797336870675656522E-17, -0.3917322834645670104, -2.525590551181102317 ) ) ;
#66807 = CARTESIAN_POINT ( 'NONE',  ( -0.3543307086614165824, 0.2952755905511811885, 0.000000000000000000 ) ) ;
#66808 = CARTESIAN_POINT ( 'NONE',  ( 1.272965879265092637, -0.4281496062992127816, -0.4176697321401328100 ) ) ;
#66809 = AXIS2_PLACEMENT_3D ( 'NONE', #41209, #22675, #3736 ) ;
#66810 = CARTESIAN_POINT ( 'NONE',  ( -0.1070741851644051862, -0.3996062992125986590, 0.008530183727034094596 ) ) ;
#66812 = FACE_OUTER_BOUND ( 'NONE', #30285, .T. ) ;
#66811 = CARTESIAN_POINT ( 'NONE',  ( -1.220472440944882386, 0.000000000000000000, -0.4445507791589061175 ) ) ;
#66813 = CARTESIAN_POINT ( 'NONE',  ( -1.233595800524933894, 0.2306618581243848609, 0.2411417322834645549 ) ) ;
#66814 = CARTESIAN_POINT ( 'NONE',  ( -0.9383202099737524282, -0.05778040916215522460, 0.4822834645669289988 ) ) ;
#66815 = CARTESIAN_POINT ( 'NONE',  ( 0.1958661417322836162, -0.3392501089628018329, 0.1430639352044112689 ) ) ;
#66816 = CARTESIAN_POINT ( 'NONE',  ( 0.3608923884514443348, 0.1771653543307087075, -0.09757992244046823083 ) ) ;
#66817 = CARTESIAN_POINT ( 'NONE',  ( -0.3392501089628017219, -0.1958661417322836718, -0.6095800524934383846 ) ) ;
#66818 = CARTESIAN_POINT ( 'NONE',  ( 0.5118110236220480003, -0.5511811023622047445, 6.969142054262312111E-17 ) ) ;
#66819 = CARTESIAN_POINT ( 'NONE',  ( 0.9251968503937015864, -0.4536011799217367080, 0.2665933059059888421 ) ) ;
#66820 = CARTESIAN_POINT ( 'NONE',  ( 0.9711286089238851948, 0.2306618581243848609, 0.2411417322834645549 ) ) ;
#66821 = CARTESIAN_POINT ( 'NONE',  ( -0.1443569553805765515, -0.3690944881889765550, -0.3153832671262227771 ) ) ;
#66822 = CARTESIAN_POINT ( 'NONE',  ( 0.1958661417322836440, -0.3392501089628017219, -1.973753280839895208 ) ) ;
#66823 = CARTESIAN_POINT ( 'NONE',  ( -1.167979002624671470, 0.05413385826771666132, 0.4176697321401328100 ) ) ;
#66824 = CARTESIAN_POINT ( 'NONE',  ( -0.1574803149606292529, -0.1870078740157479769, 0.3641732283464567677 ) ) ;
#66825 = CARTESIAN_POINT ( 'NONE',  ( -1.292650918635170010, 0.1771653543307087075, -0.09757992244046823083 ) ) ;
#66826 = CARTESIAN_POINT ( 'NONE',  ( 0.4091458600556403535, 0.2362204724409449896, -0.5229658792650918597 ) ) ;
#66827 = CARTESIAN_POINT ( 'NONE',  ( -0.8792650918635160906, -0.3690944881889763329, 0.3153832671262228327 ) ) ;
#66828 = CARTESIAN_POINT ( 'NONE',  ( -0.1837270341207340729, 0.2306618581243847221, -0.2411417322834647770 ) ) ;
#66829 = CYLINDRICAL_SURFACE ( 'NONE', #29051, 0.4744094488188972947 ) ;
#66830 = CARTESIAN_POINT ( 'NONE',  ( 0.3280839895013130669, -0.004921259842519576551, 0.3153832671262227771 ) ) ;
#66831 = CARTESIAN_POINT ( 'NONE',  ( -0.3477690288713905509, -0.5511811023622046335, 0.09757992244046803654 ) ) ;
#66832 = CARTESIAN_POINT ( 'NONE',  ( -0.8661417322834640276, -0.1870078740157479769, 0.4822834645669291653 ) ) ;
#66833 = DIRECTION ( 'NONE',  ( -0.000000000000000000, -1.000000000000000000, -0.000000000000000000 ) ) ;
#66834 = DIRECTION ( 'NONE',  ( -1.000000000000000000, -0.000000000000000000, -0.000000000000000000 ) ) ;
#66835 = CARTESIAN_POINT ( 'NONE',  ( 0.6167979002624679463, 0.05413385826771626580, -0.4176697321401330321 ) ) ;
#66836 = CARTESIAN_POINT ( 'NONE',  ( -0.3460692066303957537, -0.1998031496062994405, -1.389107611548556553 ) ) ;
#66837 = CARTESIAN_POINT ( 'NONE',  ( 1.443569553805774897, 0.2306618581243848609, 0.2411417322834645549 ) ) ;
#66838 = CARTESIAN_POINT ( 'NONE',  ( -0.4002624671916004129, -0.08942795157528024563, -0.3641732283464568787 ) ) ;
#66839 = CARTESIAN_POINT ( 'NONE',  ( -0.1640419947506555343, -0.3162353388693405765, 0.4822834645669290543 ) ) ;
#66840 = CARTESIAN_POINT ( 'NONE',  ( -1.351706036745406347, -0.4281496062992124485, 0.4176697321401328655 ) ) ;
#66841 = CARTESIAN_POINT ( 'NONE',  ( 1.692913385826772421, 0.2952755905511811885, 0.000000000000000000 ) ) ;
#66842 = CARTESIAN_POINT ( 'NONE',  ( 1.207349081364829990, 0.2306618581243848609, 0.2411417322834645549 ) ) ;
#66843 = CARTESIAN_POINT ( 'NONE',  ( -0.4986876640419942164, -0.5023911411419708095, 0.1820866141732285504 ) ) ;
#66845 = EDGE_CURVE ( 'NONE', #50773, #39166, #65516, .T. ) ;
#66844 = CARTESIAN_POINT ( 'NONE',  ( 3.924389226575468737, 2.165354330708661568, -0.3149606299212595606 ) ) ;
#66846 = CARTESIAN_POINT ( 'NONE',  ( -0.1998031496062994683, 0.3460692066303958092, -0.01312335958005250193 ) ) ;
#66847 = CARTESIAN_POINT ( 'NONE',  ( -0.1974969037888706647, 0.3420746716998658843, -0.01312335958005255224 ) ) ;
#66848 = CARTESIAN_POINT ( 'NONE',  ( 0.4359958488159816348, 1.724409448818897905, -2.630268417803909298 ) ) ;
#66849 = CARTESIAN_POINT ( 'NONE',  ( 1.338582677165355062, -0.1870078740157480601, -0.3641732283464567677 ) ) ;
#66850 = CARTESIAN_POINT ( 'NONE',  ( -1.574803149606298636, -0.1870078740157479769, 0.4822834645669291653 ) ) ;
#66851 = AXIS2_PLACEMENT_3D ( 'NONE', #15722, #16130, #48094 ) ;
#66852 = CARTESIAN_POINT ( 'NONE',  ( 1.003937007874016185, 0.1660481256975883668, -0.3530559997133364547 ) ) ;
#66853 = CARTESIAN_POINT ( 'NONE',  ( -9.594673741351313045E-17, 0.3917322834645670104, -2.289370078740157410 ) ) ;
#66854 = CARTESIAN_POINT ( 'NONE',  ( 1.194225721784777594, -0.004921259842519576551, 0.3153832671262227771 ) ) ;
#66855 = CARTESIAN_POINT ( 'NONE',  ( -0.03937007874015669567, 0.2952755905511811885, 0.000000000000000000 ) ) ;
#66856 = CARTESIAN_POINT ( 'NONE',  ( -0.3674540682414689785, 0.2306618581243848609, 0.2411417322834645549 ) ) ;
#66857 = DIRECTION ( 'NONE',  ( 0.000000000000000000, 0.000000000000000000, 1.000000000000000000 ) ) ;
#66858 = CONICAL_SURFACE ( 'NONE', #58781, 2.165354330708661568, 0.7853981633974500554 ) ;
#66859 = CARTESIAN_POINT ( 'NONE',  ( 0.4091458600556404646, -0.2362204724409448231, -0.5774278215223097588 ) ) ;
#66860 = AXIS2_PLACEMENT_3D ( 'NONE', #60091, #3264, #29343 ) ;
#66861 = CARTESIAN_POINT ( 'NONE',  ( 3.861135848600278475, 2.745602313593968447, 0.5314960629921260393 ) ) ;
#66862 = CARTESIAN_POINT ( 'NONE',  ( 0.2821522309711292364, -0.5511811023622046335, 0.09757992244046803654 ) ) ;
#66863 = EDGE_LOOP ( 'NONE', ( #27744, #27609, #55029, #31338 ) ) ;
#66864 = CARTESIAN_POINT ( 'NONE',  ( -0.3392501089628019995, 0.1958661417322831999, -0.3379458249681908666 ) ) ;
#66865 = ORIENTED_EDGE ( 'NONE', *, *, #14300, .T. ) ;
#66866 = CARTESIAN_POINT ( 'NONE',  ( -0.2296587926509179312, -0.3162353388693409650, -0.4822834645669289433 ) ) ;
#66867 = CARTESIAN_POINT ( 'NONE',  ( 1.410761154855643795, -0.3162353388693405765, 0.4822834645669290543 ) ) ;
#66868 = CARTESIAN_POINT ( 'NONE',  ( 0.2165354330708668673, -0.5400638737290844871, 0.3530559997133364547 ) ) ;
#66869 = CARTESIAN_POINT ( 'NONE',  ( -0.4330708661417315697, -0.5511811023622047445, 6.969142054262312111E-17 ) ) ;
#66870 = CARTESIAN_POINT ( 'NONE',  ( 0.7480314960629927956, 0.2952755905511811885, 0.000000000000000000 ) ) ;
#66871 = CARTESIAN_POINT ( 'NONE',  ( -1.010498687664041384, 0.05413385826771666132, 0.4176697321401328100 ) ) ;
#66872 = CARTESIAN_POINT ( 'NONE',  ( -0.2952755905511804668, 0.1660481256975885056, 0.3530559997133364547 ) ) ;
#66873 = CARTESIAN_POINT ( 'NONE',  ( -0.8792650918635160906, 0.05413385826771626580, -0.4176697321401330321 ) ) ;
#66874 = CARTESIAN_POINT ( 'NONE',  ( 1.292650918635171564, 0.2952755905511811885, 0.1292274648535926551 ) ) ;
#66875 = CARTESIAN_POINT ( 'NONE',  ( 0.7677165354330716118, -0.5400638737290844871, 0.3530559997133364547 ) ) ;
#66876 = CARTESIAN_POINT ( 'NONE',  ( 0.7349081364829403995, 0.2306618581243848609, 0.2411417322834645549 ) ) ;
#66877 = CARTESIAN_POINT ( 'NONE',  ( 0.3917322834645670104, 2.398668435337828261E-17, -0.4251968503937007537 ) ) ;
#66878 = CARTESIAN_POINT ( 'NONE',  ( -0.1246719160104980823, -0.5511811023622048555, -0.09757992244046775898 ) ) ;
#66879 = ORIENTED_EDGE ( 'NONE', *, *, #74381, .T. ) ;
#66880 = CARTESIAN_POINT ( 'NONE',  ( 0.2891555358219910499, 0.2891555358219910499, -1.240157480314960869 ) ) ;
#66881 = EDGE_LOOP ( 'NONE', ( #76351, #53289 ) ) ;
#66882 = CARTESIAN_POINT ( 'NONE',  ( -0.8464566929133852113, -0.4536011799217368745, -0.2665933059059886201 ) ) ;
#66883 = CARTESIAN_POINT ( 'NONE',  ( 0.1049868766404206816, 0.2306618581243848609, 0.2411417322834645549 ) ) ;
#66884 = CARTESIAN_POINT ( 'NONE',  ( -1.559171609364246924, 1.128537896298103416, 0.2406134192599649890 ) ) ;
#66885 = CARTESIAN_POINT ( 'NONE',  ( -0.4002624671916004129, -0.05778040916215560624, -0.4822834645669293319 ) ) ;
#66886 = CARTESIAN_POINT ( 'NONE',  ( -0.4658792650918627265, -0.05778040916215522460, 0.4822834645669289988 ) ) ;
#66887 = CARTESIAN_POINT ( 'NONE',  ( -1.286089238845143479, 0.2306618581243847221, -0.2411417322834647770 ) ) ;
#66888 = CARTESIAN_POINT ( 'NONE',  ( -1.351706036745406347, 0.05413385826771626580, -0.4176697321401330321 ) ) ;
#66889 = CARTESIAN_POINT ( 'NONE',  ( 0.7808398950131241190, -0.08942795157528024563, -0.3641732283464568787 ) ) ;
#66890 = CARTESIAN_POINT ( 'NONE',  ( 0.4422863986689484772, 1.709743469447152719, 1.031222268885702231 ) ) ;
#66891 = CARTESIAN_POINT ( 'NONE',  ( 5.785732909357575061E-17, -0.4724409448818898682, -0.6279527559055118058 ) ) ;
#66892 = CARTESIAN_POINT ( 'NONE',  ( 0.3871391076115492380, -0.08942795157528024563, -0.3641732283464568787 ) ) ;
#66893 = CARTESIAN_POINT ( 'NONE',  ( -0.05249343832020911260, 0.2306618581243848609, 0.2411417322834645549 ) ) ;
#66894 = CARTESIAN_POINT ( 'NONE',  ( 0.4396325459317593221, 0.2952755905511810774, -0.1292274648535930714 ) ) ;
#66895 = VERTEX_POINT ( 'NONE', #56458 ) ;
#66896 = CARTESIAN_POINT ( 'NONE',  ( 0.2925321140481932369, -0.2925321140481932369, -1.673228346456692828 ) ) ;
#66897 = DIRECTION ( 'NONE',  ( -3.491481338843133355E-15, -0.000000000000000000, 1.000000000000000000 ) ) ;
#66898 = ORIENTED_EDGE ( 'NONE', *, *, #1215, .F. ) ;
#66899 = CARTESIAN_POINT ( 'NONE',  ( 0.2925321140481932369, -0.2925321140481931814, -0.9625984251968502381 ) ) ;
#66900 = CARTESIAN_POINT ( 'NONE',  ( 0.1070741851644054776, -0.3996062992125984925, -0.6345144356955381149 ) ) ;
#66901 = CARTESIAN_POINT ( 'NONE',  ( -0.3937007874015740483, -0.1870078740157480879, -0.4822834645669291653 ) ) ;
#66902 = CARTESIAN_POINT ( 'NONE',  ( -0.4091458600556405756, 0.2362204724409446288, 0.1312335958005249326 ) ) ;
#66903 = CARTESIAN_POINT ( 'NONE',  ( -0.2867679344610365999, 0.2867679344610364889, -2.624015748031495399 ) ) ;
#66904 = CARTESIAN_POINT ( 'NONE',  ( 1.679790026246720025, 0.2306618581243848609, 0.2411417322834645549 ) ) ;
#66905 = CARTESIAN_POINT ( 'NONE',  ( 0.8267716535433077274, 0.2952755905511811885, 0.000000000000000000 ) ) ;
#66906 = CARTESIAN_POINT ( 'NONE',  ( 0.7611548556430454138, 0.2306618581243847221, -0.2411417322834647770 ) ) ;
#66907 = CARTESIAN_POINT ( 'NONE',  ( -0.1312335958005241554, -0.5023911411419708095, -0.1820866141732282451 ) ) ;
#66908 = CARTESIAN_POINT ( 'NONE',  ( -0.1377952755905504645, 0.1660481256975885056, 0.3530559997133364547 ) ) ;
#66909 = CARTESIAN_POINT ( 'NONE',  ( 0.2362204724409451007, -0.4091458600556402980, -2.058398950131233640 ) ) ;
#66910 = CARTESIAN_POINT ( 'NONE',  ( -0.1181102362204717315, -0.5511811023622047445, 6.969142054262312111E-17 ) ) ;
#66911 = CARTESIAN_POINT ( 'NONE',  ( -0.5905511811023615998, 0.2952755905511811885, 0.000000000000000000 ) ) ;
#66912 = CARTESIAN_POINT ( 'NONE',  ( 0.3420746716998660508, -0.1974969037888704149, -1.756561679790026309 ) ) ;
#66913 = CARTESIAN_POINT ( 'NONE',  ( -1.712598425196849572, 0.1660481256975885056, 0.3530559997133364547 ) ) ;
#66914 = CARTESIAN_POINT ( 'NONE',  ( -0.02624671916010428221, -0.5023911411419708095, 0.1820866141732285504 ) ) ;
#66915 = CARTESIAN_POINT ( 'NONE',  ( 1.476377952755906442, -0.4536011799217367080, 0.2665933059059888421 ) ) ;
#66916 = CARTESIAN_POINT ( 'NONE',  ( -1.128608923884513837, -0.6046776061558807314, 0.2411417322834647770 ) ) ;
#66917 = CARTESIAN_POINT ( 'NONE',  ( -0.7808398950131222316, -0.2845877964562161244, -0.3641732283464567121 ) ) ;
#66918 = CARTESIAN_POINT ( 'NONE',  ( -1.036041590146031366, -2.613618158232546091E-15, -0.3464511005275220379 ) ) ;
#66919 = CARTESIAN_POINT ( 'NONE',  ( -1.259842519685038686, -0.1870078740157479769, 0.4822834645669291653 ) ) ;
#66920 = CARTESIAN_POINT ( 'NONE',  ( 0.07217847769028949700, -0.3162353388693405765, 0.4822834645669290543 ) ) ;
#66921 = CARTESIAN_POINT ( 'NONE',  ( -0.3996062992125984925, -0.1070741851644056858, -2.642388451443570041 ) ) ;
#66923 = CARTESIAN_POINT ( 'NONE',  ( 0.1049643490035303689, 0.3917322834645668994, -2.435676222275903857 ) ) ;
#66922 = CIRCLE ( 'NONE', #57498, 0.09842519685039351207 ) ;
#66924 = CARTESIAN_POINT ( 'NONE',  ( -1.968503937007874072, 2.049113738730800541E-17, 5.859448621221250875 ) ) ;
#66925 = CARTESIAN_POINT ( 'NONE',  ( 0.4921259842519691285, -0.4536011799217368745, -0.2665933059059886201 ) ) ;
#66926 = CARTESIAN_POINT ( 'NONE',  ( 0.8398950131233602345, 0.2306618581243847221, -0.2411417322834647770 ) ) ;
#66927 = CARTESIAN_POINT ( 'NONE',  ( -1.292650918635170010, -0.5511811023622046335, 0.09757992244046803654 ) ) ;
#66928 = CARTESIAN_POINT ( 'NONE',  ( 1.272965879265092637, -0.4281496062992127816, -0.4176697321401328100 ) ) ;
#66929 = CARTESIAN_POINT ( 'NONE',  ( -1.463254593175852492, -0.5511811023622048555, -0.09757992244046775898 ) ) ;
#66930 = CARTESIAN_POINT ( 'NONE',  ( -0.5643044619422565855, 0.05413385826771626580, -0.4176697321401330321 ) ) ;
#66931 = CARTESIAN_POINT ( 'NONE',  ( 0.2034120734908144990, -0.5511811023622046335, 0.09757992244046803654 ) ) ;
#66932 = CARTESIAN_POINT ( 'NONE',  ( 1.363814626685862175, 0.1354692512615924549, -0.3875633260700433458 ) ) ;
#66933 = CARTESIAN_POINT ( 'NONE',  ( 0.6561679790026253567, 0.1283753931104748280, 0.1820866141732283561 ) ) ;
#66934 = CARTESIAN_POINT ( 'NONE',  ( -0.05905511811023545637, 0.1660481256975885056, 0.3530559997133364547 ) ) ;
#66935 = CARTESIAN_POINT ( 'NONE',  ( 0.3460692066303959202, -0.1998031496062991630, -0.3392388451443569819 ) ) ;
#66936 = EDGE_CURVE ( 'NONE', #30111, #48126, #11867, .T. ) ;
#66937 = CARTESIAN_POINT ( 'NONE',  ( -0.5643044619422565855, 0.05413385826771626580, -0.4176697321401330321 ) ) ;
#66938 = CARTESIAN_POINT ( 'NONE',  ( -0.3392501089628017219, -0.1958661417322836718, -1.869422572178477848 ) ) ;
#66939 = CARTESIAN_POINT ( 'NONE',  ( 0.9120734908136489683, -0.5511811023622046335, 0.09757992244046803654 ) ) ;
#66940 = CARTESIAN_POINT ( 'NONE',  ( -0.006561679790025524116, -0.05778040916215560624, -0.4822834645669293319 ) ) ;
#66941 = CARTESIAN_POINT ( 'NONE',  ( -0.3018372703412066094, -0.4281496062992127816, -0.4176697321401328100 ) ) ;
#66942 = CARTESIAN_POINT ( 'NONE',  ( -0.4986876640419939388, 0.1283753931104746893, -0.1820866141732285504 ) ) ;
#66943 = CARTESIAN_POINT ( 'NONE',  ( 0.9576546141020361169, 0.004960608223778963273, 0.3437734562760189072 ) ) ;
#66944 = CARTESIAN_POINT ( 'NONE',  ( -0.6430446194225712953, -0.004921259842519870586, -0.3153832671262229437 ) ) ;
#66945 = CARTESIAN_POINT ( 'NONE',  ( 0.4986876640419954376, -0.6046776061558809534, -0.2411417322834644161 ) ) ;
#66946 = CARTESIAN_POINT ( 'NONE',  ( -0.8923884514435688198, 0.1283753931104746893, -0.1820866141732285504 ) ) ;
#66947 = CARTESIAN_POINT ( 'NONE',  ( 0.3460692066303958092, 0.1998031496062993018, -0.8379265091863516979 ) ) ;
#66948 = CARTESIAN_POINT ( 'NONE',  ( -1.167979002624671470, 0.05413385826771666132, 0.4176697321401328100 ) ) ;
#66949 = CARTESIAN_POINT ( 'NONE',  ( -0.8558026128237093966, -1.094630224652485432E-15, 0.4281993546915541238 ) ) ;
#66950 = ORIENTED_EDGE ( 'NONE', *, *, #41759, .F. ) ;
#66951 = CARTESIAN_POINT ( 'NONE',  ( -1.181102362204723644, -0.1870078740157480601, -0.3641732283464567677 ) ) ;
#66952 = CARTESIAN_POINT ( 'NONE',  ( -0.2690288713910754526, 0.2952755905511810774, -0.1292274648535930714 ) ) ;
#66953 = CARTESIAN_POINT ( 'NONE',  ( -1.712598425196849572, 0.1660481256975885056, 0.3530559997133364547 ) ) ;
#66954 = CARTESIAN_POINT ( 'NONE',  ( -0.9842519685039360366, 0.2952755905511811885, 0.000000000000000000 ) ) ;
#66955 = DIRECTION ( 'NONE',  ( 0.000000000000000000, 0.000000000000000000, 1.000000000000000000 ) ) ;
#66956 = CARTESIAN_POINT ( 'NONE',  ( 1.515748031496063408, 0.1660481256975885056, 0.3530559997133364547 ) ) ;
#66957 = CARTESIAN_POINT ( 'NONE',  ( 0.7349081364829403995, 0.2306618581243848609, 0.2411417322834645549 ) ) ;
#66958 = CARTESIAN_POINT ( 'NONE',  ( -0.2821522309711278487, 0.2066929133858267931, 0.1054918080437490802 ) ) ;
#66959 = CARTESIAN_POINT ( 'NONE',  ( 0.2371319115525429566, -0.1759675087575592323, 5.678257627497695914 ) ) ;
#66960 = CARTESIAN_POINT ( 'NONE',  ( -1.561679790026246017, 0.05413385826771666132, 0.4176697321401328100 ) ) ;
#66961 = CARTESIAN_POINT ( 'NONE',  ( -0.3996062992125986035, -0.1070741851644056997, -0.6758530183727035068 ) ) ;
#66962 = ORIENTED_EDGE ( 'NONE', *, *, #61781, .T. ) ;
#66963 = CARTESIAN_POINT ( 'NONE',  ( -0.5249343832020990641, 0.1283753931104748280, 0.1820866141732283561 ) ) ;
#66964 = CARTESIAN_POINT ( 'NONE',  ( 0.3392501089628018884, -0.1958661417322834220, -2.144356955380577467 ) ) ;
#66965 = VERTEX_POINT ( 'NONE', #18586 ) ;
#66966 = CARTESIAN_POINT ( 'NONE',  ( 0.6692913385826777528, 0.2952755905511811885, 0.000000000000000000 ) ) ;
#66967 = CARTESIAN_POINT ( 'NONE',  ( 0.2165354330708668673, 0.1660481256975883668, -0.3530559997133364547 ) ) ;
#66968 = CARTESIAN_POINT ( 'NONE',  ( -0.5314960629921250401, 0.1660481256975885056, 0.3530559997133364547 ) ) ;
#66969 = CARTESIAN_POINT ( 'NONE',  ( 1.292650918635171564, -0.6692913385826773087, -0.1292274648535924053 ) ) ;
#66970 = CARTESIAN_POINT ( 'NONE',  ( -1.450131233595799651, 0.1771653543307087075, -0.09757992244046823083 ) ) ;
#66971 = CARTESIAN_POINT ( 'NONE',  ( 0.02826831778055379635, 1.063821329225880019, -1.462794063659299093 ) ) ;
#66972 = CARTESIAN_POINT ( 'NONE',  ( 0.3149606299212606708, -0.1870078740157480879, -0.4822834645669291653 ) ) ;
#66973 = CARTESIAN_POINT ( 'NONE',  ( -0.7414698162729651543, -0.6692913385826771977, 0.1292274648535927661 ) ) ;
#66974 = CARTESIAN_POINT ( 'NONE',  ( -0.3917322834645669549, -7.196005306013483243E-17, -1.379245776081677866 ) ) ;
#66975 = CARTESIAN_POINT ( 'NONE',  ( -1.450131233595799651, 0.2952755905511810774, -0.1292274648535930714 ) ) ;
#66976 = CARTESIAN_POINT ( 'NONE',  ( 1.306827173596997183, 0.000000000000000000, 0.4445507791589062285 ) ) ;
#66977 = CARTESIAN_POINT ( 'NONE',  ( 0.9711286089238851948, -0.6046776061558809534, -0.2411417322834644161 ) ) ;
#66978 = CARTESIAN_POINT ( 'NONE',  ( 1.430446194225722500, -0.3690944881889765550, -0.3153832671262227771 ) ) ;
#66979 = ORIENTED_EDGE ( 'NONE', *, *, #73302, .T. ) ;
#66980 = CARTESIAN_POINT ( 'NONE',  ( 0.3949938075777411073, -0.1058382717557499464, 0.04593175853018367782 ) ) ;
#66981 = CARTESIAN_POINT ( 'NONE',  ( -0.3280839895013117347, 0.05413385826771626580, -0.4176697321401330321 ) ) ;
#66982 = VERTEX_POINT ( 'NONE', #30378 ) ;
#66983 = VECTOR ( 'NONE', #24865, 39.37007874015748143 ) ;
#66984 = CARTESIAN_POINT ( 'NONE',  ( 0.2559055118110243332, -0.4536011799217368745, -0.2665933059059886201 ) ) ;
#66985 = CARTESIAN_POINT ( 'NONE',  ( -1.194225721784776262, 0.05413385826771626580, -0.4176697321401330321 ) ) ;
#66986 = CARTESIAN_POINT ( 'NONE',  ( 0.9645669291338588858, 0.1660481256975885056, 0.3530559997133364547 ) ) ;
#66987 = CARTESIAN_POINT ( 'NONE',  ( 0.7742782152230978099, -0.4281496062992124485, 0.4176697321401328655 ) ) ;
#66988 = CARTESIAN_POINT ( 'NONE',  ( -0.05249343832020938322, -0.6046776061558809534, -0.2411417322834644161 ) ) ;
#66989 = CARTESIAN_POINT ( 'NONE',  ( -0.8989501312335946848, -0.6692913385826771977, 0.1292274648535927661 ) ) ;
#66990 = CARTESIAN_POINT ( 'NONE',  ( -0.3392501089628019995, 0.1958661417322832277, -2.315616797900262647 ) ) ;
#66991 = CARTESIAN_POINT ( 'NONE',  ( -1.443569553805773564, -0.6046776061558807314, 0.2411417322834647770 ) ) ;
#66992 = CARTESIAN_POINT ( 'NONE',  ( -0.5577427821522301654, -0.3162353388693405765, 0.4822834645669290543 ) ) ;
#66993 = CARTESIAN_POINT ( 'NONE',  ( -0.4658792650918627265, -0.2845877964562161244, -0.3641732283464567121 ) ) ;
#66994 = CARTESIAN_POINT ( 'NONE',  ( 1.437007874015748810, -0.5400638737290845981, -0.3530559997133363437 ) ) ;
#66995 = CARTESIAN_POINT ( 'NONE',  ( 1.522309711286089939, 0.2306618581243848609, 0.2411417322834645549 ) ) ;
#66996 = CARTESIAN_POINT ( 'NONE',  ( -1.082677165354329896, 0.1660481256975885056, 0.3530559997133364547 ) ) ;
#66997 = CARTESIAN_POINT ( 'NONE',  ( -9.787531504996566615E-17, 0.3996062992125985480, -0.07677165354330710290 ) ) ;
#66998 = CARTESIAN_POINT ( 'NONE',  ( 0.7545931758530188826, -0.6692913385826771977, 0.1292274648535927661 ) ) ;
#66999 = CARTESIAN_POINT ( 'NONE',  ( -0.1070741851644056997, 0.3996062992125986035, -1.896325459317584894 ) ) ;
#67000 = CARTESIAN_POINT ( 'NONE',  ( 0.4606732211678797317, 2.793565526369266028, -0.5309055118110236338 ) ) ;
#67001 = CARTESIAN_POINT ( 'NONE',  ( -0.3083989501312330295, -0.3162353388693409650, -0.4822834645669289433 ) ) ;
#67002 = CARTESIAN_POINT ( 'NONE',  ( -1.135170603674539924, 0.1771653543307087075, -0.09757992244046823083 ) ) ;
#67003 = CARTESIAN_POINT ( 'NONE',  ( 1.003937007874016407, -0.4536011799217367080, 0.2665933059059888421 ) ) ;
#67004 = CARTESIAN_POINT ( 'NONE',  ( 0.4724409448818897572, -0.1265901696524988906, -0.6607611548556431291 ) ) ;
#67005 = CARTESIAN_POINT ( 'NONE',  ( 1.240157480314961314, 0.07958543189024071263, -0.2665933059059888421 ) ) ;
#67006 = CARTESIAN_POINT ( 'NONE',  ( 0.7414698162729663755, -0.6692913385826773087, -0.1292274648535924053 ) ) ;
#67007 = CARTESIAN_POINT ( 'NONE',  ( -0.1058382717557503072, 0.3949938075777408852, -0.5557742782152231831 ) ) ;
#67008 = CARTESIAN_POINT ( 'NONE',  ( -0.2755905511811018171, 0.2952755905511811885, 0.000000000000000000 ) ) ;
#67009 = CARTESIAN_POINT ( 'NONE',  ( -0.1938976377952756625, -0.1938976377952756625, 0.1574803149606299191 ) ) ;
#67010 = CARTESIAN_POINT ( 'NONE',  ( 1.522309711286089939, -0.5023911411419708095, -0.1820866141732282451 ) ) ;
#67011 = CARTESIAN_POINT ( 'NONE',  ( -0.6167979002624665030, 0.05413385826771666132, 0.4176697321401328100 ) ) ;
#67012 = CARTESIAN_POINT ( 'NONE',  ( -0.1974969037888706924, 0.3420746716998658843, -0.4048556430446195176 ) ) ;
#67013 = CARTESIAN_POINT ( 'NONE',  ( 1.384514435695538559, 0.2952755905511810774, -0.1292274648535930714 ) ) ;
#67014 = CARTESIAN_POINT ( 'NONE',  ( 0.05249343832021075018, 0.2306618581243847221, -0.2411417322834647770 ) ) ;
#67015 = CARTESIAN_POINT ( 'NONE',  ( 0.5052493438320218022, -0.5511811023622048555, -0.09757992244046775898 ) ) ;
#67016 = CARTESIAN_POINT ( 'NONE',  ( -0.4744094488188934089, 1.521776870516600821, -1.016821367227985551 ) ) ;
#67017 = CARTESIAN_POINT ( 'NONE',  ( 0.3083989501312343062, -0.08942795157528024563, -0.3641732283464568787 ) ) ;
#67018 = CARTESIAN_POINT ( 'NONE',  ( -1.640419947506561060, 0.05413385826771666132, 0.4176697321401328100 ) ) ;
#67019 = CARTESIAN_POINT ( 'NONE',  ( -0.1998031496062994405, 0.3460692066303957537, -1.349737532808399143 ) ) ;
#67020 = CARTESIAN_POINT ( 'NONE',  ( 0.7086614173228353852, -0.1870078740157479769, 0.4822834645669291653 ) ) ;
#67021 = CARTESIAN_POINT ( 'NONE',  ( -0.1049643490035307020, 0.3917322834645669549, -1.101049868766403872 ) ) ;
#67022 = CARTESIAN_POINT ( 'NONE',  ( 1.620734908136483465, -0.5511811023622046335, 0.09757992244046803654 ) ) ;
#67023 = CARTESIAN_POINT ( 'NONE',  ( -0.2502216998114409341, 0.3021538998228462392, 1.649893717844496181E-17 ) ) ;
#67024 = CARTESIAN_POINT ( 'NONE',  ( -0.1640419947506555343, -0.2845877964562159024, 0.3641732283464567677 ) ) ;
#67025 = CARTESIAN_POINT ( 'NONE',  ( 0.03280839895013198948, -0.6692913385826773087, -0.1292274648535924053 ) ) ;
#67026 = APPLICATION_CONTEXT ( 'automotive_design' ) ;
#67027 = CARTESIAN_POINT ( 'NONE',  ( 1.404199475065617708, -0.004921259842519870586, -0.3153832671262229437 ) ) ;
#67028 = CARTESIAN_POINT ( 'NONE',  ( -1.351706036745406347, -0.004921259842519870586, -0.3153832671262229437 ) ) ;
#67029 = CARTESIAN_POINT ( 'NONE',  ( -1.292650918635170010, -0.6692913385826771977, 0.1292274648535927661 ) ) ;
#67030 = CARTESIAN_POINT ( 'NONE',  ( 0.6233595800524942554, -0.05778040916215560624, -0.4822834645669293319 ) ) ;
#67031 = CARTESIAN_POINT ( 'NONE',  ( 1.108923884514436686, -0.3162353388693409650, -0.4822834645669289433 ) ) ;
#67032 = DIRECTION ( 'NONE',  ( -0.2810846377148183417, 0.6785983445458432239, 0.6785983445458515506 ) ) ;
#67033 = CARTESIAN_POINT ( 'NONE',  ( 0.7677165354330716118, -0.5400638737290844871, 0.3530559997133364547 ) ) ;
#67034 = CARTESIAN_POINT ( 'NONE',  ( 1.430446194225722500, -0.4281496062992127816, -0.4176697321401328100 ) ) ;
#67035 = CARTESIAN_POINT ( 'NONE',  ( 1.036745406824147731, 0.05413385826771666132, 0.4176697321401328100 ) ) ;
#67036 = CARTESIAN_POINT ( 'NONE',  ( -1.706036745406823485, 0.1283753931104748280, 0.1820866141732283561 ) ) ;
#67037 = CARTESIAN_POINT ( 'NONE',  ( 0.6692913385826778638, -0.5511811023622047445, 6.969142054262312111E-17 ) ) ;
#67038 = CARTESIAN_POINT ( 'NONE',  ( 1.594488188976378673, -0.5400638737290845981, -0.3530559997133363437 ) ) ;
#67039 = CARTESIAN_POINT ( 'NONE',  ( -0.9514435695538050464, -0.08942795157528024563, -0.3641732283464568787 ) ) ;
#67040 = CARTESIAN_POINT ( 'NONE',  ( 0.4068241469816279987, -0.3690944881889765550, -0.3153832671262227771 ) ) ;
#67041 = CARTESIAN_POINT ( 'NONE',  ( 0.08530183727034192087, -0.05778040916215522460, 0.4822834645669289988 ) ) ;
#67042 = CARTESIAN_POINT ( 'NONE',  ( 0.7020997375328090762, -0.05778040916215560624, -0.4822834645669293319 ) ) ;
#67043 = CARTESIAN_POINT ( 'NONE',  ( -0.1968503937007867743, 0.2952755905511811885, 0.000000000000000000 ) ) ;
#67044 = CARTESIAN_POINT ( 'NONE',  ( 0.02624671916010564918, 0.1283753931104748280, 0.1820866141732283561 ) ) ;
#67045 = CARTESIAN_POINT ( 'NONE',  ( 1.102362204724410155, -0.1870078740157479769, 0.4822834645669291653 ) ) ;
#67046 = CARTESIAN_POINT ( 'NONE',  ( -1.559171609364246924, 1.128537896298103416, 0.2406134192599649890 ) ) ;
#67047 = CARTESIAN_POINT ( 'NONE',  ( -1.089238845144356427, 0.05413385826771666132, 0.4176697321401328100 ) ) ;
#67049 = CARTESIAN_POINT ( 'NONE',  ( -0.1998031496062991907, -0.3460692066303959757, -0.6955380577427822120 ) ) ;
#67048 = CARTESIAN_POINT ( 'NONE',  ( 0.3503937007874015075, -0.3044824468161027586, -0.01968503937007903132 ) ) ;
#67050 = DIRECTION ( 'NONE',  ( 0.000000000000000000, 0.000000000000000000, -1.000000000000000000 ) ) ;
#67051 = CARTESIAN_POINT ( 'NONE',  ( -0.7349081364829387342, -0.6046776061558807314, 0.2411417322834647770 ) ) ;
#67052 = CARTESIAN_POINT ( 'NONE',  ( -0.6102362204724400829, 0.1660481256975885056, 0.3530559997133364547 ) ) ;
#67053 = CARTESIAN_POINT ( 'NONE',  ( 0.4091458600556404646, -0.2362204724409448231, 0.05249343832020997302 ) ) ;
#67054 = CARTESIAN_POINT ( 'NONE',  ( 0.3420746716998660508, -0.1974969037888703871, -2.467191601049868677 ) ) ;
#67055 = ORIENTED_EDGE ( 'NONE', *, *, #28103, .T. ) ;
#67056 = CARTESIAN_POINT ( 'NONE',  ( 0.6889763779527566800, -0.4536011799217367080, 0.2665933059059888421 ) ) ;
#67057 = CARTESIAN_POINT ( 'NONE',  ( -0.3917322834645671215, 0.1049643490035301469, -1.127296587926509108 ) ) ;
#67058 = CARTESIAN_POINT ( 'NONE',  ( 1.095800524934383846, -0.3162353388693405765, 0.4822834645669290543 ) ) ;
#67059 = CARTESIAN_POINT ( 'NONE',  ( -0.2481535038101752855, 4.694981358611540289E-15, -0.3627989612356130045 ) ) ;
#67060 = CARTESIAN_POINT ( 'NONE',  ( -1.437007874015747477, -0.4536011799217367080, 0.2665933059059888421 ) ) ;
#67061 = CARTESIAN_POINT ( 'NONE',  ( 1.660104986876641320, -0.05778040916215522460, 0.4822834645669289988 ) ) ;
#67062 = EDGE_CURVE ( 'NONE', #25317, #51716, #48191, .T. ) ;
#67063 = CARTESIAN_POINT ( 'NONE',  ( -1.397637795275589623, 0.1660481256975885056, 0.3530559997133364547 ) ) ;
#67064 = CARTESIAN_POINT ( 'NONE',  ( 0.3917322834645669549, 2.398668435337827645E-17, -0.3556237288375834749 ) ) ;
#67065 = CARTESIAN_POINT ( 'NONE',  ( 0.1837270341207357105, -0.6046776061558809534, -0.2411417322834644161 ) ) ;
#67066 = CARTESIAN_POINT ( 'NONE',  ( -0.2887139107611542133, 0.1283753931104748280, 0.1820866141732283561 ) ) ;
#67067 = CARTESIAN_POINT ( 'NONE',  ( 0.9514435695538062676, -0.05778040916215522460, 0.4822834645669289988 ) ) ;
#67069 = EDGE_CURVE ( 'NONE', #80835, #53475, #12648, .T. ) ;
#67068 = CARTESIAN_POINT ( 'NONE',  ( 0.01312335958005323398, 0.05413385826771666132, 0.4176697321401328100 ) ) ;
#67070 = CARTESIAN_POINT ( 'NONE',  ( 0.4986876640419954376, 0.2306618581243848609, 0.2411417322834645549 ) ) ;
#67071 = CARTESIAN_POINT ( 'NONE',  ( 0.2362204724409449064, 0.4091458600556404646, -1.089238845144356871 ) ) ;
#67072 = CARTESIAN_POINT ( 'NONE',  ( -0.1049643490035302301, -0.3917322834645671770, -1.643720103183414105 ) ) ;
#67073 = CARTESIAN_POINT ( 'NONE',  ( 0.7349081364829403995, 0.2306618581243848609, 0.2411417322834645549 ) ) ;
#67074 = CARTESIAN_POINT ( 'NONE',  ( 0.1115485564304467270, -0.6692913385826773087, -0.1292274648535924053 ) ) ;
#67075 = CARTESIAN_POINT ( 'NONE',  ( -1.010498687664041384, 0.05413385826771666132, 0.4176697321401328100 ) ) ;
#67076 = CARTESIAN_POINT ( 'NONE',  ( 1.076115485564305141, -0.6046776061558807314, 0.2411417322834647770 ) ) ;
#67077 = CARTESIAN_POINT ( 'NONE',  ( 1.062992125984252745, 0.2952755905511811885, 0.000000000000000000 ) ) ;
#67078 = CARTESIAN_POINT ( 'NONE',  ( -0.2867679344610364334, -0.2867679344610367109, -1.088582677165354173 ) ) ;
#67079 = CARTESIAN_POINT ( 'NONE',  ( -0.1968503937007867743, -0.6692913385826771977, 8.415575281601705876E-17 ) ) ;
#67080 = CARTESIAN_POINT ( 'NONE',  ( 0.4527559055118117182, 0.1660481256975883668, -0.3530559997133364547 ) ) ;
#67081 = CARTESIAN_POINT ( 'NONE',  ( 0.1049868766404206816, 0.2306618581243848609, 0.2411417322834645549 ) ) ;
#67082 = CARTESIAN_POINT ( 'NONE',  ( 0.9055118110236227702, 0.1771653543307087630, 0.000000000000000000 ) ) ;
#67083 = CARTESIAN_POINT ( 'NONE',  ( -1.187664041994750175, -0.05778040916215560624, -0.4822834645669293319 ) ) ;
#67084 = CARTESIAN_POINT ( 'NONE',  ( -0.4744094488188880798, 1.537401574803149984, -2.554262525012305218 ) ) ;
#67085 = CARTESIAN_POINT ( 'NONE',  ( 0.4068241469816279987, -0.4281496062992127816, -0.4176697321401328100 ) ) ;
#67086 = DIRECTION ( 'NONE',  ( 1.000000000000000000, 1.387778780781445676E-15, 0.000000000000000000 ) ) ;
#67087 = B_SPLINE_CURVE_WITH_KNOTS ( 'NONE', 3,
 ( #77636, #20801, #1039, #40571 ),
 .UNSPECIFIED., .F., .F.,
 ( 4, 4 ),
 ( 0.000000000000000000, 0.001421551995671103573 ),
 .UNSPECIFIED. ) ;
#67088 = CARTESIAN_POINT ( 'NONE',  ( 0.1049643490035304938, -0.3917322834645669549, -2.282152230971128404 ) ) ;
#67089 = ORIENTED_EDGE ( 'NONE', *, *, #51971, .F. ) ;
#67090 = ADVANCED_FACE ( 'NONE', ( #37520 ), #34753, .F. ) ;
#67091 = ORIENTED_EDGE ( 'NONE', *, *, #37822, .T. ) ;
#67092 = CARTESIAN_POINT ( 'NONE',  ( 1.089238845144357759, 0.05413385826771626580, -0.4176697321401330321 ) ) ;
#67093 = CARTESIAN_POINT ( 'NONE',  ( 0.5183727034120741983, 0.1771653543307087075, -0.09757992244046823083 ) ) ;
#67095 = CARTESIAN_POINT ( 'NONE',  ( 0.5643044619422579178, 0.05413385826771666132, 0.4176697321401328100 ) ) ;
#67094 = CARTESIAN_POINT ( 'NONE',  ( 0.4744094488188900782, 1.537401574803149984, 2.170146923806596906 ) ) ;
#67096 = ADVANCED_FACE ( 'NONE', ( #60413 ), #66746, .F. ) ;
#67097 = CARTESIAN_POINT ( 'NONE',  ( -0.4712114270530097793, 1.601157653251831903, 3.908712503217392609 ) ) ;
#67098 = CARTESIAN_POINT ( 'NONE',  ( 0.3392501089628018884, -0.1958661417322834220, -1.134514435695538115 ) ) ;
#67099 = CARTESIAN_POINT ( 'NONE',  ( -0.3996062992125986590, 0.1070741851644051723, -2.314304461942256808 ) ) ;
#67100 = CARTESIAN_POINT ( 'NONE',  ( -0.7677165354330699465, -0.5400638737290845981, -0.3530559997133363437 ) ) ;
#67101 = CARTESIAN_POINT ( 'NONE',  ( -0.7349081364829390672, 0.2306618581243847221, -0.2411417322834647770 ) ) ;
#67102 = CARTESIAN_POINT ( 'NONE',  ( 0.6955380577427828781, 0.05413385826771626580, -0.4176697321401330321 ) ) ;
#67103 = ORIENTED_EDGE ( 'NONE', *, *, #18560, .T. ) ;
#67104 = CARTESIAN_POINT ( 'NONE',  ( 1.397637795275591177, -0.5400638737290844871, 0.3530559997133364547 ) ) ;
#67105 = CARTESIAN_POINT ( 'NONE',  ( 1.207349081364829990, 0.1539470093639523085, 0.1968503937007873850 ) ) ;
#67106 = CARTESIAN_POINT ( 'NONE',  ( 1.535433070866142558, 0.1771653543307087630, 0.000000000000000000 ) ) ;
#67107 = CARTESIAN_POINT ( 'NONE',  ( -0.1998031496062994405, 0.3460692066303957537, -2.137139107611548905 ) ) ;
#67108 = CARTESIAN_POINT ( 'NONE',  ( -1.450131233595799651, 0.1771653543307087075, -0.09757992244046823083 ) ) ;
#67109 = LINE ( 'NONE', #9032, #16785 ) ;
#67110 = CARTESIAN_POINT ( 'NONE',  ( 0.2165354330708668673, -0.5400638737290844871, 0.3530559997133364547 ) ) ;
#67112 = CARTESIAN_POINT ( 'NONE',  ( -3.908417273630399258, 1.569223574151384470, -0.4736117085908965185 ) ) ;
#67111 = CARTESIAN_POINT ( 'NONE',  ( 1.397637795275591177, 0.1660481256975883668, -0.3530559997133364547 ) ) ;
#67113 = CARTESIAN_POINT ( 'NONE',  ( -1.017060367454067249, -0.2845877964562161244, -0.3641732283464567121 ) ) ;
#67114 = CARTESIAN_POINT ( 'NONE',  ( 0.7611548556430454138, 0.2306618581243847221, -0.2411417322834647770 ) ) ;
#67115 = CARTESIAN_POINT ( 'NONE',  ( 1.266404199475066328, -0.08942795157527998196, 0.3641732283464567121 ) ) ;
#67116 = CARTESIAN_POINT ( 'NONE',  ( 0.3917322834645668994, 0.1049643490035304522, -1.149586983430759490 ) ) ;
#67117 = CARTESIAN_POINT ( 'NONE',  ( -0.9251968503937002541, 0.07958543189024085140, 0.2665933059059887866 ) ) ;
#67118 = CARTESIAN_POINT ( 'NONE',  ( 1.476377952755906442, -0.5400638737290844871, 0.3530559997133364547 ) ) ;
#67119 = CARTESIAN_POINT ( 'NONE',  ( 2.558921551581142317, 1.580736828574225150, -0.4725026149319433433 ) ) ;
#67121 = EDGE_CURVE ( 'NONE', #81558, #5170, #40186, .T. ) ;
#67120 = CARTESIAN_POINT ( 'NONE',  ( -0.2755905511811018171, 0.2952755905511811885, 0.000000000000000000 ) ) ;
#67122 = CARTESIAN_POINT ( 'NONE',  ( -1.548556430446193399, -0.5023911411419708095, -0.1820866141732282451 ) ) ;
#67123 = CARTESIAN_POINT ( 'NONE',  ( -0.2034120734908131112, -0.5511811023622048555, -0.09757992244046775898 ) ) ;
#67124 = CARTESIAN_POINT ( 'NONE',  ( -0.1837270341207343505, -0.6046776061558807314, 0.2411417322834647770 ) ) ;
#67125 = CARTESIAN_POINT ( 'NONE',  ( -1.430446194225720724, -0.004921259842519870586, -0.3153832671262229437 ) ) ;
#67126 = CARTESIAN_POINT ( 'NONE',  ( -0.1049643490035307158, 0.3917322834645670104, -0.6332214155193720551 ) ) ;
#67127 = CARTESIAN_POINT ( 'NONE',  ( 0.2887139107611556010, -0.6046776061558807314, 0.2411417322834647770 ) ) ;
#67128 = CARTESIAN_POINT ( 'NONE',  ( 0.4037097067573611753, 1.223219560026271499E-15, 0.4445507791589056734 ) ) ;
#67129 = CARTESIAN_POINT ( 'NONE',  ( 0.4724409448818898682, 2.892866454678787531E-17, -1.769685039370078927 ) ) ;
#67130 = CARTESIAN_POINT ( 'NONE',  ( -1.167979002624671470, -0.4281496062992127816, -0.4176697321401328100 ) ) ;
#67131 = AXIS2_PLACEMENT_3D ( 'NONE', #39220, #77963, #33345 ) ;
#67132 = CARTESIAN_POINT ( 'NONE',  ( -0.03280839895013062252, -0.5511811023622046335, 0.09757992244046803654 ) ) ;
#67133 = CARTESIAN_POINT ( 'NONE',  ( -1.496062992125983815, -0.1870078740157479769, 0.4822834645669291653 ) ) ;
#67134 = CARTESIAN_POINT ( 'NONE',  ( 0.01968503937007957949, -0.5400638737290845981, -0.3530559997133363437 ) ) ;
#67135 = CARTESIAN_POINT ( 'NONE',  ( 0.5971128608923891301, 0.1771653543307087075, -0.09757992244046823083 ) ) ;
#67136 = CARTESIAN_POINT ( 'NONE',  ( -0.6692913385826764205, -0.5511811023622047445, 6.969142054262312111E-17 ) ) ;
#67137 = CARTESIAN_POINT ( 'NONE',  ( -0.9317585301837263412, 0.05413385826771666132, 0.4176697321401328100 ) ) ;
#67138 = CARTESIAN_POINT ( 'NONE',  ( -1.666666666666665853, 0.05413385826771626580, -0.4176697321401330321 ) ) ;
#67139 = CARTESIAN_POINT ( 'NONE',  ( 1.469816272965879911, -0.6046776061558807314, 0.2411417322834647770 ) ) ;
#67140 = LINE ( 'NONE', #22922, #24607 ) ;
#67141 = CARTESIAN_POINT ( 'NONE',  ( 1.056430446194226658, 0.1771653543307087630, 0.09757992244046791164 ) ) ;
#67142 = CARTESIAN_POINT ( 'NONE',  ( 0.7283464566929143125, 0.1660481256975885056, 0.3530559997133364547 ) ) ;
#67143 = CARTESIAN_POINT ( 'NONE',  ( -1.614173228346457378, 0.7166040191147894367, 0.1372047244094476981 ) ) ;
#67144 = CARTESIAN_POINT ( 'NONE',  ( 1.561679790026247350, -0.3690944881889763329, 0.3153832671262228327 ) ) ;
#67145 = VERTEX_POINT ( 'NONE', #47774 ) ;
#67146 = CARTESIAN_POINT ( 'NONE',  ( -0.8136482939632537770, 0.2306618581243847221, -0.2411417322834647770 ) ) ;
#67147 = ADVANCED_FACE ( 'NONE', ( #49733 ), #34797, .F. ) ;
#67148 = CARTESIAN_POINT ( 'NONE',  ( -0.1070741851644051862, -0.3996062992125986590, -2.826115485564304475 ) ) ;
#67149 = CARTESIAN_POINT ( 'NONE',  ( -1.391076115485563314, -0.5023911411419708095, -0.1820866141732282451 ) ) ;
#67150 = CARTESIAN_POINT ( 'NONE',  ( -0.7283464566929126471, -0.5400638737290844871, 0.3530559997133364547 ) ) ;
#67151 = CARTESIAN_POINT ( 'NONE',  ( 0.1443569553805781891, -0.4281496062992124485, 0.4176697321401328655 ) ) ;
#67152 = CARTESIAN_POINT ( 'NONE',  ( -1.351706036745406347, -0.004921259842519870586, -0.3153832671262229437 ) ) ;
#67153 = CARTESIAN_POINT ( 'NONE',  ( -0.2925321140481930149, -0.2925321140481933480, -2.183070866141731958 ) ) ;
#67154 = CARTESIAN_POINT ( 'NONE',  ( -1.338582677165353729, -0.1870078740157480879, -0.4822834645669291653 ) ) ;
#67155 = CARTESIAN_POINT ( 'NONE',  ( 0.4855643044619430415, -0.4281496062992127816, -0.4176697321401328100 ) ) ;
#67156 = CARTESIAN_POINT ( 'NONE',  ( 0.09842519685039434474, 0.1660481256975885056, 0.3530559997133364547 ) ) ;
#67157 = CARTESIAN_POINT ( 'NONE',  ( 0.9514435695538062676, -0.05778040916215522460, 0.4822834645669289988 ) ) ;
#67158 = DIRECTION ( 'NONE',  ( 3.386413887818973075E-16, -0.7071067811865519026, 0.7071067811865432429 ) ) ;
#67159 = CARTESIAN_POINT ( 'NONE',  ( 0.1070741851644053527, 0.3996062992125986590, -1.725721784776903078 ) ) ;
#67160 = CARTESIAN_POINT ( 'NONE',  ( 0.3949938075777409408, 0.1058382717557500574, -1.227034120734908473 ) ) ;
#67161 = CARTESIAN_POINT ( 'NONE',  ( -0.3460692066303960868, 0.1998031496062990242, -2.388451443569553856 ) ) ;
#67162 = CARTESIAN_POINT ( 'NONE',  ( -1.604771003085130099, 1.002618919725274838, -0.1466069496707743947 ) ) ;
#67163 = CARTESIAN_POINT ( 'NONE',  ( -0.1958661417322836718, 0.3392501089628017219, -0.1627296587926508609 ) ) ;
#67164 = CARTESIAN_POINT ( 'NONE',  ( 0.006561679790026889343, -0.08942795157527998196, 0.3641732283464567121 ) ) ;
#67165 = CARTESIAN_POINT ( 'NONE',  ( -0.3280839895013117347, -0.4281496062992124485, 0.4176697321401328655 ) ) ;
#67166 = CARTESIAN_POINT ( 'NONE',  ( 0.7808398950131240079, -0.3162353388693405765, 0.4822834645669290543 ) ) ;
#67167 = CARTESIAN_POINT ( 'NONE',  ( 0.1058382717557500852, -0.3949938075777408852, -2.051837270341207109 ) ) ;
#67168 = CARTESIAN_POINT ( 'NONE',  ( -0.1443569553805765515, -0.3690944881889765550, -0.3153832671262227771 ) ) ;
#67169 = EDGE_CURVE ( 'NONE', #53039, #62716, #22440, .T. ) ;
#67170 = CARTESIAN_POINT ( 'NONE',  ( -1.122047244094487306, 0.1660481256975883668, -0.3530559997133364547 ) ) ;
#67171 = CARTESIAN_POINT ( 'NONE',  ( 1.233595800524935227, -0.6046776061558807314, 0.2411417322834647770 ) ) ;
#67172 = CARTESIAN_POINT ( 'NONE',  ( 0.1265901696524990294, -0.4724409448818896462, -2.290026246719159442 ) ) ;
#67173 = CARTESIAN_POINT ( 'NONE',  ( 0.1070741851644053527, 0.3996062992125986590, -1.883202099737532276 ) ) ;
#67174 = CARTESIAN_POINT ( 'NONE',  ( 1.113948071074811752, 0.02791078216816225699, 0.4328096321851905293 ) ) ;
#67175 = EDGE_LOOP ( 'NONE', ( #6503, #51696, #45622, #14690 ) ) ;
#67176 = ORIENTED_EDGE ( 'NONE', *, *, #41242, .T. ) ;
#67177 = CARTESIAN_POINT ( 'NONE',  ( 1.174540682414699111, -0.05778040916215560624, -0.4822834645669293319 ) ) ;
#67178 = CARTESIAN_POINT ( 'NONE',  ( 1.574803149606299746, -0.1870078740157479769, 0.3641732283464567677 ) ) ;
#67180 = CARTESIAN_POINT ( 'NONE',  ( -0.9645669291338575535, 0.1660481256975883668, -0.3530559997133364547 ) ) ;
#67179 = CARTESIAN_POINT ( 'NONE',  ( -0.9973753280839886548, 0.1283753931104748280, 0.1820866141732283561 ) ) ;
#67181 = CARTESIAN_POINT ( 'NONE',  ( 4.797336870675656522E-17, -0.3917322834645670104, 0.1515748031496061965 ) ) ;
#67182 = CARTESIAN_POINT ( 'NONE',  ( 1.135170603674541256, -0.6692913385826773087, -0.1292274648535924053 ) ) ;
#67183 = CARTESIAN_POINT ( 'NONE',  ( 0.000000000000000000, 0.04921259842519689481, -0.08523872084492506440 ) ) ;
#67184 = CARTESIAN_POINT ( 'NONE',  ( 0.06561679790026316017, 0.05413385826771626580, -0.4176697321401330321 ) ) ;
#67185 = CARTESIAN_POINT ( 'NONE',  ( -0.4002624671916004129, -0.05778040916215560624, -0.4822834645669293319 ) ) ;
#67186 = CARTESIAN_POINT ( 'NONE',  ( -1.548556430446193399, -0.6046776061558809534, -0.2411417322834644161 ) ) ;
#67187 = CARTESIAN_POINT ( 'NONE',  ( 0.3392501089628018884, -0.1958661417322834220, -0.3471128608923885195 ) ) ;
#67188 = CARTESIAN_POINT ( 'NONE',  ( 0.3805774278215230400, 0.05413385826771626580, -0.4176697321401330321 ) ) ;
#67189 = CARTESIAN_POINT ( 'NONE',  ( -0.1049643490035307020, 0.3917322834645669549, -2.360892388451444113 ) ) ;
#67190 = CARTESIAN_POINT ( 'NONE',  ( -1.417322834645668772, -0.1870078740157480601, -0.3641732283464567677 ) ) ;
#67191 = ORIENTED_EDGE ( 'NONE', *, *, #33761, .F. ) ;
#67192 = CARTESIAN_POINT ( 'NONE',  ( 0.1058382717557499880, 0.3949938075777411073, -2.355643044619422533 ) ) ;
#67193 = ORIENTED_EDGE ( 'NONE', *, *, #52442, .F. ) ;
#67194 = CARTESIAN_POINT ( 'NONE',  ( -1.518978356207579372, 1.376229525351539973, 0.4462089517855873932 ) ) ;
#67195 = CARTESIAN_POINT ( 'NONE',  ( -1.423884514435694859, -0.3162353388693405765, 0.4822834645669290543 ) ) ;
#67196 = CARTESIAN_POINT ( 'NONE',  ( 0.2925321140481932369, -0.2925321140481932369, -1.043307086614173151 ) ) ;
#67197 = CARTESIAN_POINT ( 'NONE',  ( -1.417322834645668772, -0.1870078740157479769, 0.4822834645669291653 ) ) ;
#67198 = CARTESIAN_POINT ( 'NONE',  ( -0.2017716535433071445, 0.2017716535433070613, -0.3937007874015748254 ) ) ;
#67199 = CARTESIAN_POINT ( 'NONE',  ( 0.4744094488188940750, 1.537401574803149984, 1.016821367227985329 ) ) ;
#67200 = CARTESIAN_POINT ( 'NONE',  ( -0.3608923884514428360, 0.2952755905511811885, 0.1292274648535926551 ) ) ;
#67201 = CARTESIAN_POINT ( 'NONE',  ( -0.3917322834645670104, -7.196005306013484475E-17, -0.1240157480314961758 ) ) ;
#67202 = CARTESIAN_POINT ( 'NONE',  ( -0.4002624671916004129, -0.2845877964562159024, 0.3641732283464567677 ) ) ;
#67203 = CARTESIAN_POINT ( 'NONE',  ( -0.9645669291338575535, -0.4536011799217367080, 0.2665933059059888421 ) ) ;
#67204 = CARTESIAN_POINT ( 'NONE',  ( -1.213910761154854745, -0.6692913385826771977, 0.1292274648535927661 ) ) ;
#67205 = CARTESIAN_POINT ( 'NONE',  ( 0.6955380577427828781, 0.05413385826771626580, -0.4176697321401330321 ) ) ;
#67206 = CARTESIAN_POINT ( 'NONE',  ( -0.8530183727034112984, 0.05413385826771666132, 0.4176697321401328100 ) ) ;
#67207 = CARTESIAN_POINT ( 'NONE',  ( -0.1049643490035302024, -0.3917322834645671215, -0.06430446194225715451 ) ) ;
#67208 = ORIENTED_EDGE ( 'NONE', *, *, #74915, .T. ) ;
#67209 = CARTESIAN_POINT ( 'NONE',  ( -1.200787401574802349, -0.5400638737290844871, 0.3530559997133364547 ) ) ;
#67210 = CARTESIAN_POINT ( 'NONE',  ( -0.2087913723976025926, 0.2087913723976025371, 0.1248231986745539646 ) ) ;
#67211 =( NAMED_UNIT ( * ) PLANE_ANGLE_UNIT ( ) SI_UNIT ( $, .RADIAN. ) );
#67212 = CARTESIAN_POINT ( 'NONE',  ( 0.4724409448818896462, 0.1265901696524990294, -1.856955380577427928 ) ) ;
#67213 = CARTESIAN_POINT ( 'NONE',  ( -0.7426113562972000981, 2.362204724409448620, -0.5309055118110235227 ) ) ;
#67214 = CARTESIAN_POINT ( 'NONE',  ( -9.594673741351313045E-17, 0.3917322834645670104, -0.6220472440944880832 ) ) ;
#67215 = CARTESIAN_POINT ( 'NONE',  ( 0.3917322834645669549, 0.1049643490035304660, -2.256561679790026531 ) ) ;
#67216 = CARTESIAN_POINT ( 'NONE',  ( -0.7480314960629914633, -0.6692913385826771977, 8.415575281601705876E-17 ) ) ;
#67217 = CARTESIAN_POINT ( 'NONE',  ( 1.338582677165355062, -0.1870078740157479769, 0.4822834645669291653 ) ) ;
#67218 = CARTESIAN_POINT ( 'NONE',  ( 0.2925321140481932369, 0.2925321140481932369, -0.5295275590551181688 ) ) ;
#67220 = DIRECTION ( 'NONE',  ( 0.000000000000000000, 1.000000000000000000, 0.000000000000000000 ) ) ;
#67219 = CARTESIAN_POINT ( 'NONE',  ( 0.7210809602247731931, 4.888820689338890882E-16, 0.3464511005275202615 ) ) ;
#67221 = ADVANCED_FACE ( 'NONE', ( #53043 ), #34541, .T. ) ;
#67222 = CARTESIAN_POINT ( 'NONE',  ( -1.358267716535432434, 0.1660481256975883668, -0.3530559997133364547 ) ) ;
#67223 = CARTESIAN_POINT ( 'NONE',  ( -0.9448818897637790704, -0.1870078740157479769, 0.4822834645669291653 ) ) ;
#67225 = B_SPLINE_CURVE_WITH_KNOTS ( 'NONE', 3,
 ( #55674, #50189, #61173, #75886, #16582, #42227, #80973 ),
 .UNSPECIFIED., .F., .F.,
 ( 4, 3, 4 ),
 ( 5.204170427930420513E-18, 0.001246230184515574775, 0.002492489877932649832 ),
 .UNSPECIFIED. ) ;
#67224 = CARTESIAN_POINT ( 'NONE',  ( 0.1958661417322836162, -0.3392501089628018329, -0.1718966947168485970 ) ) ;
#67226 = CARTESIAN_POINT ( 'NONE',  ( 0.3149606299212603933, -0.1870078740157479769, 0.3641732283464567677 ) ) ;
#67227 = CARTESIAN_POINT ( 'NONE',  ( -0.1049643490035301885, -0.3917322834645671215, -0.4717847769028871707 ) ) ;
#67228 = EDGE_CURVE ( 'NONE', #23851, #72980, #71831, .T. ) ;
#67229 = CARTESIAN_POINT ( 'NONE',  ( 0.2559055118110243332, 0.07958543189024085140, 0.2665933059059887866 ) ) ;
#67230 = CARTESIAN_POINT ( 'NONE',  ( 1.135170603674541256, 0.1771653543307087630, 0.09757992244046791164 ) ) ;
#67231 = CARTESIAN_POINT ( 'NONE',  ( 0.8923884514435701520, -0.6046776061558809534, -0.2411417322834644161 ) ) ;
#67232 = CARTESIAN_POINT ( 'NONE',  ( -0.2230971128608915943, -0.004921259842519576551, 0.3153832671262227771 ) ) ;
#67233 = CARTESIAN_POINT ( 'NONE',  ( 0.1049643490035304938, -0.3917322834645669549, -2.282152230971128404 ) ) ;
#67234 = CARTESIAN_POINT ( 'NONE',  ( -1.607611548556429737, 0.2952755905511810774, -0.1292274648535930714 ) ) ;
#67235 = CARTESIAN_POINT ( 'NONE',  ( -1.240157480314959759, -0.4536011799217368745, -0.2665933059059886201 ) ) ;
#67236 = CARTESIAN_POINT ( 'NONE',  ( 0.2362204724409451007, -0.4091458600556402980, -0.1686351706036745557 ) ) ;
#67237 = CARTESIAN_POINT ( 'NONE',  ( -0.9186351706036736120, -0.5023911411419708095, -0.1820866141732282451 ) ) ;
#67238 = CARTESIAN_POINT ( 'NONE',  ( -0.07874015748031421014, -0.1870078740157479769, 0.4822834645669291653 ) ) ;
#67239 = CARTESIAN_POINT ( 'NONE',  ( -2.583694225513480713, 2.755905511811024056, 0.5314960629921260393 ) ) ;
#67240 = CARTESIAN_POINT ( 'NONE',  ( 0.7020997375328090762, -0.08942795157528024563, -0.3641732283464568787 ) ) ;
#67241 = CARTESIAN_POINT ( 'NONE',  ( -0.06561679790026180015, -0.3690944881889765550, -0.3153832671262227771 ) ) ;
#67242 = CARTESIAN_POINT ( 'NONE',  ( -0.9186351706036736120, -0.6046776061558809534, -0.2411417322834644161 ) ) ;
#67243 = LINE ( 'NONE', #28097, #57322 ) ;
#67244 = CARTESIAN_POINT ( 'NONE',  ( 0.000000000000000000, 0.000000000000000000, 0.000000000000000000 ) ) ;
#67245 = CARTESIAN_POINT ( 'NONE',  ( 0.2427821522309719648, -0.05778040916215522460, 0.4822834645669289988 ) ) ;
#67246 = B_SPLINE_CURVE_WITH_KNOTS ( 'NONE', 3,
 ( #56994, #50683, #5662, #82691 ),
 .UNSPECIFIED., .F., .F.,
 ( 4, 4 ),
 ( 0.1635406000437870655, 0.1649189557199158829 ),
 .UNSPECIFIED. ) ;
#67247 = CARTESIAN_POINT ( 'NONE',  ( -0.1998031496062994405, 0.3460692066303957537, -1.664698162729658426 ) ) ;
#67248 = CARTESIAN_POINT ( 'NONE',  ( 1.463254593175853824, 0.2952755905511810774, -0.1292274648535930714 ) ) ;
#67249 = CARTESIAN_POINT ( 'NONE',  ( -0.4068241469816267775, -0.004921259842519870586, -0.3153832671262229437 ) ) ;
#67250 = CARTESIAN_POINT ( 'NONE',  ( -0.2296587926509179312, -0.3162353388693409650, -0.4822834645669289433 ) ) ;
#67251 = CARTESIAN_POINT ( 'NONE',  ( -1.541994750656167090, -0.6692913385826773087, -0.1292274648535924053 ) ) ;
#67252 = CARTESIAN_POINT ( 'NONE',  ( 1.496062992125985147, -0.1870078740157479769, 0.4822834645669291653 ) ) ;
#67253 = CARTESIAN_POINT ( 'NONE',  ( 1.456692913385827515, -0.6692913385826771977, 8.415575281601705876E-17 ) ) ;
#67254 = CARTESIAN_POINT ( 'NONE',  ( -0.7677165354330699465, 0.07958543189024085140, 0.2665933059059887866 ) ) ;
#67255 = CARTESIAN_POINT ( 'NONE',  ( -0.1998031496062991630, -0.3460692066303959202, -0.1423884514435695692 ) ) ;
#67256 = CARTESIAN_POINT ( 'NONE',  ( 0.3460692066303959202, 0.1998031496062993295, -0.4461942257217847430 ) ) ;
#67257 = CARTESIAN_POINT ( 'NONE',  ( -0.1958661417322833942, -0.3392501089628018884, -2.739520628117797063 ) ) ;
#67258 = AXIS2_PLACEMENT_3D ( 'NONE', #27950, #61177, #53609 ) ;
#67259 = CARTESIAN_POINT ( 'NONE',  ( 1.541994750656168645, 0.1771653543307087075, -0.09757992244046823083 ) ) ;
#67260 = CARTESIAN_POINT ( 'NONE',  ( 1.154855643044620184, 0.1283753931104746893, -0.1820866141732285504 ) ) ;
#67261 = CARTESIAN_POINT ( 'NONE',  ( 0.4461942257217855756, 0.1539470093639521697, -0.1968503937007875793 ) ) ;
#67262 = CARTESIAN_POINT ( 'NONE',  ( 0.7742782152230978099, -0.4281496062992124485, 0.4176697321401328655 ) ) ;
#67263 = CARTESIAN_POINT ( 'NONE',  ( -0.2891555358219911054, 0.2891555358219909388, -0.7263779527559056648 ) ) ;
#67264 = CARTESIAN_POINT ( 'NONE',  ( 1.082677165354331228, 0.07958543189024071263, -0.2665933059059888421 ) ) ;
#67265 = CARTESIAN_POINT ( 'NONE',  ( -0.09842519685039295696, -0.5400638737290844871, 0.3530559997133364547 ) ) ;
#67266 = CARTESIAN_POINT ( 'NONE',  ( -0.2362204724409440182, -0.1870078740157479769, 0.4822834645669291653 ) ) ;
#67267 = CARTESIAN_POINT ( 'NONE',  ( 1.692913385826772421, 0.2952755905511811885, 0.000000000000000000 ) ) ;
#67268 = CARTESIAN_POINT ( 'NONE',  ( 0.4091458600556404646, -0.2362204724409448231, -0.8923884514435694859 ) ) ;
#67269 = CARTESIAN_POINT ( 'NONE',  ( -0.1998031496062991907, -0.3460692066303959757, -2.112860892388451539 ) ) ;
#67270 = CARTESIAN_POINT ( 'NONE',  ( 0.3805774278215230400, -0.004921259842519870586, -0.3153832671262229437 ) ) ;
#67271 = ORIENTED_EDGE ( 'NONE', *, *, #46853, .F. ) ;
#67272 = CARTESIAN_POINT ( 'NONE',  ( 0.1049643490035303967, 0.3917322834645670659, -0.4626177409786895178 ) ) ;
#67273 = ORIENTED_EDGE ( 'NONE', *, *, #19808, .T. ) ;
#67274 = CARTESIAN_POINT ( 'NONE',  ( -0.4265091863517051496, 0.2952755905511810774, -0.1292274648535930714 ) ) ;
#67275 = CARTESIAN_POINT ( 'NONE',  ( 0.7874015748031503170, -0.1870078740157479769, 0.4822834645669291653 ) ) ;
#67276 = CARTESIAN_POINT ( 'NONE',  ( 0.07874015748031558404, -0.1870078740157479769, 0.4822834645669291653 ) ) ;
#67277 = CARTESIAN_POINT ( 'NONE',  ( -0.2624671916010490880, -0.5023911411419708095, 0.1820866141732285504 ) ) ;
#67278 = CARTESIAN_POINT ( 'NONE',  ( 0.7152230971128616943, -0.05778040916215522460, 0.4822834645669289988 ) ) ;
#67279 = CARTESIAN_POINT ( 'NONE',  ( -0.9645669291338575535, 0.1660481256975883668, -0.3530559997133364547 ) ) ;
#67280 = CARTESIAN_POINT ( 'NONE',  ( -0.4724409448818890911, -0.1870078740157479769, 0.4822834645669291653 ) ) ;
#67281 = CARTESIAN_POINT ( 'NONE',  ( 0.9908136482939640111, 0.2952755905511810774, -0.1292274648535930714 ) ) ;
#67282 = CARTESIAN_POINT ( 'NONE',  ( 0.9842519685039375910, 0.2952755905511811885, 0.000000000000000000 ) ) ;
#67283 = CARTESIAN_POINT ( 'NONE',  ( 0.9251968503937015864, 0.1660481256975883668, -0.3530559997133364547 ) ) ;
#67284 = CARTESIAN_POINT ( 'NONE',  ( 0.1049643490035303689, 0.3917322834645670104, -0.4580052493438320216 ) ) ;
#67285 = CARTESIAN_POINT ( 'NONE',  ( -0.02624671916010428221, 0.1283753931104746893, -0.1820866141732285504 ) ) ;
#67286 = EDGE_LOOP ( 'NONE', ( #79742, #62101, #48226 ) ) ;
#67287 = CARTESIAN_POINT ( 'NONE',  ( 4.837279021331060870E-17, -0.3949938075777409963, -1.023622047244094446 ) ) ;
#67288 = ORIENTED_EDGE ( 'NONE', *, *, #61360, .T. ) ;
#67289 = CARTESIAN_POINT ( 'NONE',  ( -0.9514435695538050464, -0.2845877964562159024, 0.3641732283464567677 ) ) ;
#67290 = CARTESIAN_POINT ( 'NONE',  ( -0.4593175853018364174, -0.4281496062992127816, -0.4176697321401328100 ) ) ;
#67291 = CARTESIAN_POINT ( 'NONE',  ( 0.000000000000000000, 2.755905511811024056, 0.000000000000000000 ) ) ;
#67292 = CARTESIAN_POINT ( 'NONE',  ( -0.4724409448818890911, -0.1870078740157479769, 0.4822834645669291653 ) ) ;
#67293 = CARTESIAN_POINT ( 'NONE',  ( -0.5643044619422565855, 0.05413385826771626580, -0.4176697321401330321 ) ) ;
#67294 = CARTESIAN_POINT ( 'NONE',  ( -1.371391076115484609, -0.6692913385826771977, 0.1292274648535927661 ) ) ;
#67295 = CARTESIAN_POINT ( 'NONE',  ( -1.601049868766403650, -0.6046776061558807314, 0.2411417322834647770 ) ) ;
#67296 = CARTESIAN_POINT ( 'NONE',  ( 0.9120734908136490793, 0.1771653543307087075, -0.09757992244046823083 ) ) ;
#67297 = CARTESIAN_POINT ( 'NONE',  ( -0.4091458600556402980, -0.2362204724409451284, -0.9973753280839895430 ) ) ;
#67298 = CARTESIAN_POINT ( 'NONE',  ( -1.614173228346456712, 2.362204724409448620, 0.1372047244094477536 ) ) ;
#67299 = CARTESIAN_POINT ( 'NONE',  ( 0.4593175853018379162, -0.3690944881889763329, 0.3153832671262228327 ) ) ;
#67300 = CARTESIAN_POINT ( 'NONE',  ( 0.2559055118110243332, 0.1660481256975885056, 0.3530559997133364547 ) ) ;
#67301 = CARTESIAN_POINT ( 'NONE',  ( 0.2427821522309719648, -0.05778040916215522460, 0.4822834645669289988 ) ) ;
#67302 = ORIENTED_EDGE ( 'NONE', *, *, #78140, .F. ) ;
#67303 = CARTESIAN_POINT ( 'NONE',  ( -0.2925321140481930704, -0.2925321140481933480, -1.633858267716534973 ) ) ;
#67304 = DIRECTION ( 'NONE',  ( 0.000000000000000000, 0.000000000000000000, -1.000000000000000000 ) ) ;
#67305 = ORIENTED_EDGE ( 'NONE', *, *, #29099, .T. ) ;
#67306 = CARTESIAN_POINT ( 'NONE',  ( -0.1998031496062991630, -0.3460692066303959202, -1.244750656167979086 ) ) ;
#67307 = CARTESIAN_POINT ( 'NONE',  ( 0.2925321140481932369, -0.2925321140481931814, -0.6476377952755905110 ) ) ;
#67308 = CARTESIAN_POINT ( 'NONE',  ( -0.6561679790026240244, -0.5023911411419708095, 0.1820866141732285504 ) ) ;
#67309 = CARTESIAN_POINT ( 'NONE',  ( -1.056430446194224881, 0.2952755905511810774, -0.1292274648535930714 ) ) ;
#67310 = CARTESIAN_POINT ( 'NONE',  ( -0.4724409448818898682, -8.678599364036362592E-17, 0.1181102362204724532 ) ) ;
#67311 = CARTESIAN_POINT ( 'NONE',  ( -0.1958661417322834220, -0.3392501089628018884, -2.669947506561679784 ) ) ;
#67312 = CARTESIAN_POINT ( 'NONE',  ( 1.555118110236221041, 0.1660481256975883668, -0.3530559997133364547 ) ) ;
#67313 = CARTESIAN_POINT ( 'NONE',  ( 1.049868766404200127, -0.6046776061558809534, -0.2411417322834644161 ) ) ;
#67314 = CARTESIAN_POINT ( 'NONE',  ( 0.3215223097112867578, -0.3162353388693409650, -0.4822834645669289433 ) ) ;
#67315 = CARTESIAN_POINT ( 'NONE',  ( -0.5314960629921250401, 0.07958543189024085140, 0.2665933059059887866 ) ) ;
#67316 = CARTESIAN_POINT ( 'NONE',  ( 0.2230971128608929543, 0.05413385826771626580, -0.4176697321401330321 ) ) ;
#67317 = CARTESIAN_POINT ( 'NONE',  ( -0.2362204724409447953, -0.4091458600556404646, -1.874671916010498762 ) ) ;
#67318 = CARTESIAN_POINT ( 'NONE',  ( -0.1443569553805765515, -0.3690944881889765550, -0.3153832671262227771 ) ) ;
#67319 = CARTESIAN_POINT ( 'NONE',  ( -0.6627296587926503335, -0.6692913385826771977, 0.1292274648535927661 ) ) ;
#67320 = EDGE_CURVE ( 'NONE', #43965, #76998, #33381, .T. ) ;
#67321 = CARTESIAN_POINT ( 'NONE',  ( 0.1058382717557499880, 0.3949938075777409408, -1.645013123359580831 ) ) ;
#67322 = CARTESIAN_POINT ( 'NONE',  ( -1.568241469816272105, -0.05778040916215522460, 0.4822834645669289988 ) ) ;
#67323 = CARTESIAN_POINT ( 'NONE',  ( 0.1181102362204730916, -0.5511811023622047445, 6.969142054262312111E-17 ) ) ;
#67324 = CARTESIAN_POINT ( 'NONE',  ( 1.607611548556431069, -0.5511811023622048555, -0.09757992244046775898 ) ) ;
#67325 = CARTESIAN_POINT ( 'NONE',  ( -1.030183727034119867, -0.05778040916215560624, -0.4822834645669293319 ) ) ;
#67326 = AXIS2_PLACEMENT_3D ( 'NONE', #51206, #11708, #12937 ) ;
#67327 = CARTESIAN_POINT ( 'NONE',  ( -0.7349081364829387342, -0.5023911411419708095, 0.1820866141732285504 ) ) ;
#67328 = CARTESIAN_POINT ( 'NONE',  ( -1.035118193396259434, 5.987370802660155681E-15, -0.3791483426435156567 ) ) ;
#67329 = CARTESIAN_POINT ( 'NONE',  ( -1.194225721784776262, 0.05413385826771626580, -0.4176697321401330321 ) ) ;
#67330 = CARTESIAN_POINT ( 'NONE',  ( 0.1312335958005257930, 0.2306618581243847221, -0.2411417322834647770 ) ) ;
#67331 = CARTESIAN_POINT ( 'NONE',  ( -0.3996062992125986590, 0.1070741851644051723, -2.471784776902887337 ) ) ;
#67332 = CARTESIAN_POINT ( 'NONE',  ( 0.1902887139107617975, -0.6692913385826773087, -0.1292274648535924053 ) ) ;
#67333 = CARTESIAN_POINT ( 'NONE',  ( 0.2867679344610365999, -0.2867679344610365999, -2.383182783955693829 ) ) ;
#67334 = CARTESIAN_POINT ( 'NONE',  ( -2.077216372526510479, 1.325969025732672391, -0.4256800600601859941 ) ) ;
#67335 = CARTESIAN_POINT ( 'NONE',  ( 0.2099737532808405305, -0.5023911411419708095, 0.1820866141732285504 ) ) ;
#67336 = CARTESIAN_POINT ( 'NONE',  ( 1.017060367454068581, -0.05778040916215560624, -0.4822834645669293319 ) ) ;
#67337 = CARTESIAN_POINT ( 'NONE',  ( -1.233595800524933894, 0.1283753931104748280, 0.1820866141732283561 ) ) ;
#67338 = CARTESIAN_POINT ( 'NONE',  ( 1.043307086614173818, 0.1660481256975885056, 0.3530559997133364547 ) ) ;
#67339 = CARTESIAN_POINT ( 'NONE',  ( -1.692913385826770645, 0.1771653543307087630, 0.000000000000000000 ) ) ;
#67340 = CARTESIAN_POINT ( 'NONE',  ( -0.5905511811023615998, 0.2952755905511811885, 0.000000000000000000 ) ) ;
#67341 = CARTESIAN_POINT ( 'NONE',  ( 0.3477690288713918276, -0.5511811023622048555, -0.09757992244046775898 ) ) ;
#67342 = CARTESIAN_POINT ( 'NONE',  ( 1.606165476768023126, 0.2953034477953545567, -0.04641075316546838109 ) ) ;
#67343 = CARTESIAN_POINT ( 'NONE',  ( 0.4593175853018379162, -0.3690944881889763329, 0.3153832671262228327 ) ) ;
#67344 = CARTESIAN_POINT ( 'NONE',  ( -0.1706036745406816491, 0.05413385826771626580, -0.4176697321401330321 ) ) ;
#67345 = CARTESIAN_POINT ( 'NONE',  ( -0.3460692066303960313, 0.1998031496062989965, -0.4179790026246719137 ) ) ;
#67346 = CARTESIAN_POINT ( 'NONE',  ( -0.9448818897637790704, -0.1870078740157479769, 0.4822834645669291653 ) ) ;
#67347 = CARTESIAN_POINT ( 'NONE',  ( 0.3917322834645670104, 2.398668435337828261E-17, -1.777559055118110409 ) ) ;
#67348 = CARTESIAN_POINT ( 'NONE',  ( 1.154855643044620184, 0.1283753931104746893, -0.1820866141732285504 ) ) ;
#67349 = CARTESIAN_POINT ( 'NONE',  ( 0.2099737532808405305, -0.6046776061558807314, 0.2411417322834647770 ) ) ;
#67350 = CARTESIAN_POINT ( 'NONE',  ( -0.3608923884514428360, 0.2952755905511811885, 0.1292274648535926551 ) ) ;
#67351 = CARTESIAN_POINT ( 'NONE',  ( -0.1902887139107604098, 0.1771653543307087075, -0.09757992244046823083 ) ) ;
#67352 = CARTESIAN_POINT ( 'NONE',  ( 0.9908136482939640111, 0.2066929133858267098, -0.1054918080437494132 ) ) ;
#67353 = CARTESIAN_POINT ( 'NONE',  ( -0.5905511811023613777, -0.5511811023622047445, 6.969142054262312111E-17 ) ) ;
#67354 = CARTESIAN_POINT ( 'NONE',  ( 0.4068241469816281097, 0.05413385826771666132, 0.4176697321401328100 ) ) ;
#67355 = CARTESIAN_POINT ( 'NONE',  ( -1.305774278215222184, -0.5511811023622048555, -0.09757992244046775898 ) ) ;
#67356 = CARTESIAN_POINT ( 'NONE',  ( -0.2925321140481930149, -0.2925321140481933480, -0.9232283464566929387 ) ) ;
#67357 = CARTESIAN_POINT ( 'NONE',  ( -0.9973753280839886548, 0.2306618581243848609, 0.2411417322834645549 ) ) ;
#67358 = CARTESIAN_POINT ( 'NONE',  ( 0.8542087009142342868, -6.211426067506147994E-17, -0.3627989612356148363 ) ) ;
#67359 = ORIENTED_EDGE ( 'NONE', *, *, #58958, .F. ) ;
#67360 = CARTESIAN_POINT ( 'NONE',  ( -1.712598425196849572, 0.07958543189024085140, 0.2665933059059887866 ) ) ;
#67361 = CARTESIAN_POINT ( 'NONE',  ( -0.5643044619422565855, 0.05413385826771626580, -0.4176697321401330321 ) ) ;
#67363 = CARTESIAN_POINT ( 'NONE',  ( 0.3801136020054692310, 1.252211066003288131, -1.385051565532328111 ) ) ;
#67362 = B_SPLINE_CURVE_WITH_KNOTS ( 'NONE', 3,
 ( #13969, #26583, #46343, #40051 ),
 .UNSPECIFIED., .F., .F.,
 ( 4, 4 ),
 ( 3.210432057725814518E-07, 0.001287787053612126330 ),
 .UNSPECIFIED. ) ;
#67364 = CARTESIAN_POINT ( 'NONE',  ( -1.253280839895012377, -0.3162353388693409650, -0.4822834645669289433 ) ) ;
#67365 = CARTESIAN_POINT ( 'NONE',  ( 0.3021538998228436301, 0.2502216998114438762, -1.220472440944881942 ) ) ;
#67366 = CARTESIAN_POINT ( 'NONE',  ( 1.574803149606299746, -0.1870078740157480879, -0.4822834645669291653 ) ) ;
#67367 = CARTESIAN_POINT ( 'NONE',  ( 1.010498687664042716, -0.4281496062992124485, 0.4176697321401328655 ) ) ;
#67368 = CARTESIAN_POINT ( 'NONE',  ( 0.4724409448818898682, 2.892866454678787531E-17, -0.4330708661417322913 ) ) ;
#67369 = CARTESIAN_POINT ( 'NONE',  ( 1.306827173596997183, 0.000000000000000000, 0.4445507791589062285 ) ) ;
#67370 = CARTESIAN_POINT ( 'NONE',  ( 1.410761154855643795, -0.2845877964562159024, 0.3641732283464567677 ) ) ;
#67371 = CARTESIAN_POINT ( 'NONE',  ( 0.1070741851644054915, -0.3996062992125986035, -0.4002624671916010235 ) ) ;
#67372 = ORIENTED_EDGE ( 'NONE', *, *, #49490, .T. ) ;
#67373 = CARTESIAN_POINT ( 'NONE',  ( -0.3018372703412066094, -0.3690944881889765550, -0.3153832671262227771 ) ) ;
#67374 = CARTESIAN_POINT ( 'NONE',  ( 0.2867679344610365999, 0.2867679344610365999, -2.019685039370078261 ) ) ;
#67375 = ORIENTED_EDGE ( 'NONE', *, *, #78984, .F. ) ;
#67376 = CARTESIAN_POINT ( 'NONE',  ( 0.7152230971128614723, -0.3162353388693409650, -0.4822834645669289433 ) ) ;
#67377 = CARTESIAN_POINT ( 'NONE',  ( -0.2493438320209966919, 0.05413385826771626580, -0.4176697321401330321 ) ) ;
#67378 = CARTESIAN_POINT ( 'NONE',  ( -0.9448818897637790704, -0.1870078740157480879, -0.4822834645669291653 ) ) ;
#67379 = CARTESIAN_POINT ( 'NONE',  ( 1.633858267716535639, -0.5400638737290844871, 0.3530559997133364547 ) ) ;
#67380 = CARTESIAN_POINT ( 'NONE',  ( -1.115485564304461219, -0.004921259842519870586, -0.3153832671262229437 ) ) ;
#67381 = CARTESIAN_POINT ( 'NONE',  ( 0.3937007874015754361, -0.1870078740157479769, 0.4822834645669291653 ) ) ;
#67382 = VECTOR ( 'NONE', #53768, 39.37007874015748143 ) ;
#67383 = CARTESIAN_POINT ( 'NONE',  ( -0.7217847769028863381, -0.4281496062992124485, 0.4176697321401328655 ) ) ;
#67384 = CARTESIAN_POINT ( 'NONE',  ( -0.3917322834645669549, -7.196005306013483243E-17, -1.536726091042307951 ) ) ;
#67385 = CARTESIAN_POINT ( 'NONE',  ( -1.305774278215222184, 0.2952755905511811885, 0.1292274648535926551 ) ) ;
#67386 = DIRECTION ( 'NONE',  ( 1.445602896647338917E-16, 1.000000000000000000, 0.000000000000000000 ) ) ;
#67387 = CARTESIAN_POINT ( 'NONE',  ( 1.095800524934383846, -0.05778040916215560624, -0.4822834645669293319 ) ) ;
#67388 = CARTESIAN_POINT ( 'NONE',  ( 1.069553805774278832, 0.1771653543307087075, -0.09757992244046823083 ) ) ;
#67389 = VERTEX_POINT ( 'NONE', #38139 ) ;
#67390 = CARTESIAN_POINT ( 'NONE',  ( -0.1958661417322833942, -0.3392501089628018884, -2.897000943078426705 ) ) ;
#67391 = CARTESIAN_POINT ( 'NONE',  ( -0.5314960629921250401, 0.1660481256975885056, 0.3530559997133364547 ) ) ;
#67392 = ORIENTED_EDGE ( 'NONE', *, *, #5222, .F. ) ;
#67393 = CARTESIAN_POINT ( 'NONE',  ( 0.4265091863517067039, -0.5511811023622048555, -0.09757992244046775898 ) ) ;
#67394 = CARTESIAN_POINT ( 'NONE',  ( -1.213910761154854745, 0.2952755905511810774, -0.1292274648535930714 ) ) ;
#67395 = CARTESIAN_POINT ( 'NONE',  ( 0.9251968503937015864, -0.5400638737290844871, 0.3530559997133364547 ) ) ;
#67396 = CARTESIAN_POINT ( 'NONE',  ( 0.9383202099737536495, -0.3162353388693405765, 0.4822834645669290543 ) ) ;
#67397 = CARTESIAN_POINT ( 'NONE',  ( -0.3346456692913377662, -0.5400638737290844871, 0.3530559997133364547 ) ) ;
#67398 = CARTESIAN_POINT ( 'NONE',  ( 0.3917322834645670104, 0.1049643490035304660, -1.066292281661104457 ) ) ;
#67399 = CARTESIAN_POINT ( 'NONE',  ( -0.7545931758530176614, -0.6692913385826773087, -0.1292274648535924053 ) ) ;
#67400 = CARTESIAN_POINT ( 'NONE',  ( 0.3392501089628018884, -0.1958661417322834220, -2.394356955380577467 ) ) ;
#67401 = CARTESIAN_POINT ( 'NONE',  ( -1.515748031496062076, 0.1660481256975883668, -0.3530559997133364547 ) ) ;
#67402 = CARTESIAN_POINT ( 'NONE',  ( -0.6430446194225712953, 0.05413385826771626580, -0.4176697321401330321 ) ) ;
#67403 = CARTESIAN_POINT ( 'NONE',  ( 1.194225721784777594, 0.05413385826771666132, 0.4176697321401328100 ) ) ;
#67404 = CIRCLE ( 'NONE', #45853, 0.2165354330708661457 ) ;
#67405 = CARTESIAN_POINT ( 'NONE',  ( 1.410761154855643795, -0.05778040916215560624, -0.4822834645669293319 ) ) ;
#67406 = CARTESIAN_POINT ( 'NONE',  ( -0.7480314960629914633, 0.2952755905511811885, 0.000000000000000000 ) ) ;
#67407 = CARTESIAN_POINT ( 'NONE',  ( 0.7349081364829402885, -0.6046776061558809534, -0.2411417322834644161 ) ) ;
#67408 = CARTESIAN_POINT ( 'NONE',  ( 0.1998031496062992740, 0.3460692066303959757, -1.719160104986876769 ) ) ;
#67409 = EDGE_CURVE ( 'NONE', #82725, #10316, #37210, .T. ) ;
#67410 = CARTESIAN_POINT ( 'NONE',  ( -0.7086614173228339419, -0.1870078740157479769, 0.4822834645669291653 ) ) ;
#67411 = CARTESIAN_POINT ( 'NONE',  ( -1.181102362204723644, -0.1870078740157479769, 0.3641732283464567677 ) ) ;
#67412 = CARTESIAN_POINT ( 'NONE',  ( 0.6233595800524942554, -0.08942795157528024563, -0.3641732283464568787 ) ) ;
#67413 = CARTESIAN_POINT ( 'NONE',  ( 0.4091458600556404646, -0.2362204724409448231, -0.4967191601049869010 ) ) ;
#67414 = CARTESIAN_POINT ( 'NONE',  ( 1.056430446194226658, 0.1771653543307087630, 0.09757992244046791164 ) ) ;
#67415 = CARTESIAN_POINT ( 'NONE',  ( 0.9383202099737536495, -0.3162353388693405765, 0.4822834645669290543 ) ) ;
#67416 = EDGE_CURVE ( 'NONE', #77721, #19150, #53771, .T. ) ;
#67417 = CARTESIAN_POINT ( 'NONE',  ( 0.3949938075777409408, -0.1058382717557499186, -0.5032808398950131545 ) ) ;
#67418 = CARTESIAN_POINT ( 'NONE',  ( -0.3608923884514428360, -0.6692913385826773087, -0.1292274648535924053 ) ) ;
#67419 = CARTESIAN_POINT ( 'NONE',  ( 2.570293859026651972, 2.742779986175213569, 0.5314960629921260393 ) ) ;
#67420 = CARTESIAN_POINT ( 'NONE',  ( 1.338582677165355062, -0.1870078740157480601, -0.3641732283464567677 ) ) ;
#67421 = CARTESIAN_POINT ( 'NONE',  ( -0.4330708661417315697, 0.2952755905511811885, 0.000000000000000000 ) ) ;
#67422 = CARTESIAN_POINT ( 'NONE',  ( -0.3949938075777408852, -0.1058382717557502933, -0.5951443569553805935 ) ) ;
#67423 = CARTESIAN_POINT ( 'NONE',  ( 1.417322834645670104, -0.1870078740157480879, -0.4822834645669291653 ) ) ;
#67424 = CARTESIAN_POINT ( 'NONE',  ( -0.07874015748031421014, -0.1870078740157480879, -0.4822834645669291653 ) ) ;
#67425 = CARTESIAN_POINT ( 'NONE',  ( 0.6299212598425204535, -0.1870078740157480601, -0.3641732283464567677 ) ) ;
#67426 = CARTESIAN_POINT ( 'NONE',  ( -0.3769492730837889494, 1.247705490064275446, -1.056993455451901376 ) ) ;
#67427 = CARTESIAN_POINT ( 'NONE',  ( 0.09186351706036827158, -0.004921259842519576551, 0.3153832671262227771 ) ) ;
#67428 = DIRECTION ( 'NONE',  ( -0.000000000000000000, -1.000000000000000000, -0.000000000000000000 ) ) ;
#67429 = CARTESIAN_POINT ( 'NONE',  ( 0.3460692066303959202, -0.1998031496062991630, -1.441601049868766582 ) ) ;
#67430 = CARTESIAN_POINT ( 'NONE',  ( 0.5511811023622055217, -0.1870078740157479769, 0.4822834645669291653 ) ) ;
#67431 = CARTESIAN_POINT ( 'NONE',  ( 0.3392501089628018884, -0.1958661417322834220, -0.8845144356955378928 ) ) ;
#67432 = CARTESIAN_POINT ( 'NONE',  ( -0.4744094488189005143, 1.537401574803149984, 1.016821367227982220 ) ) ;
#67433 = CARTESIAN_POINT ( 'NONE',  ( -0.3796925558546807578, -0.09865214182457832104, -3.091116300196737326E-17 ) ) ;
#67434 = CARTESIAN_POINT ( 'NONE',  ( 0.2034120734908142214, 0.1771653543307087075, -0.09757992244046823083 ) ) ;
#67435 = CARTESIAN_POINT ( 'NONE',  ( 0.1509186351706045259, -0.05778040916215560624, -0.4822834645669293319 ) ) ;
#67436 = CARTESIAN_POINT ( 'NONE',  ( 1.279527559055118724, -0.4536011799217368745, -0.2665933059059886201 ) ) ;
#67437 = CARTESIAN_POINT ( 'NONE',  ( -1.154855643044618851, -0.5023911411419708095, -0.1820866141732282451 ) ) ;
#67438 = CARTESIAN_POINT ( 'NONE',  ( -1.496062992125983815, -0.1870078740157480879, -0.4822834645669291653 ) ) ;
#67439 = CIRCLE ( 'NONE', #13659, 0.3149606299212598381 ) ;
#67440 = CARTESIAN_POINT ( 'NONE',  ( 0.5708661417322842269, 0.1660481256975885056, 0.3530559997133364547 ) ) ;
#67441 = CARTESIAN_POINT ( 'NONE',  ( 1.338582677165355062, -0.1870078740157479769, 0.4822834645669291653 ) ) ;
#67442 = PLANE ( 'NONE',  #23600 ) ;
#67443 = CARTESIAN_POINT ( 'NONE',  ( 0.2165354330708668673, 0.1660481256975883668, -0.3530559997133364547 ) ) ;
#67444 = CARTESIAN_POINT ( 'NONE',  ( 1.207349081364829990, 0.2306618581243848609, 0.2411417322834645549 ) ) ;
#67445 = CARTESIAN_POINT ( 'NONE',  ( 1.076115485564305141, 0.2306618581243847221, -0.2411417322834647770 ) ) ;
#67446 = CARTESIAN_POINT ( 'NONE',  ( 0.000000000000000000, 0.000000000000000000, -2.755905511811024056 ) ) ;
#67447 = CARTESIAN_POINT ( 'NONE',  ( 0.9711286089238851948, -0.5023911411419708095, -0.1820866141732282451 ) ) ;
#67448 = CARTESIAN_POINT ( 'NONE',  ( 1.692913385826772421, 0.2952755905511811885, 0.000000000000000000 ) ) ;
#67449 = CARTESIAN_POINT ( 'NONE',  ( -0.8333333333333323711, 0.1771653543307087630, 0.09757992244046791164 ) ) ;
#67450 = CARTESIAN_POINT ( 'NONE',  ( 0.3674540682414705883, 0.1283753931104746893, -0.1820866141732285504 ) ) ;
#67451 = CARTESIAN_POINT ( 'NONE',  ( 0.01968503937007957949, -0.5400638737290845981, -0.3530559997133363437 ) ) ;
#67452 = CARTESIAN_POINT ( 'NONE',  ( 0.8136482939632553313, 0.2306618581243848609, 0.2411417322834645549 ) ) ;
#67453 = CARTESIAN_POINT ( 'NONE',  ( -0.2952755905511803003, -0.5400638737290845981, -0.3530559997133363437 ) ) ;
#67454 = CARTESIAN_POINT ( 'NONE',  ( 0.2362204724409456558, -0.1870078740157480601, -0.3641732283464567677 ) ) ;
#67455 = CARTESIAN_POINT ( 'NONE',  ( 0.8005249343832027131, 0.05413385826771666132, 0.4176697321401328100 ) ) ;
#67456 = FACE_OUTER_BOUND ( 'NONE', #3413, .T. ) ;
#67457 = CARTESIAN_POINT ( 'NONE',  ( -1.049868766404198794, 0.2306618581243847221, -0.2411417322834647770 ) ) ;
#67459 = CARTESIAN_POINT ( 'NONE',  ( 0.3460692066303959757, -0.1998031496062991907, -1.049868766404199460 ) ) ;
#67458 = CARTESIAN_POINT ( 'NONE',  ( -1.076115485564303809, 0.2306618581243848609, 0.2411417322834645549 ) ) ;
#67460 = CARTESIAN_POINT ( 'NONE',  ( 1.012922870834582101, 2.412178165100495768E-16, -0.4118484887281966822 ) ) ;
#67461 = CARTESIAN_POINT ( 'NONE',  ( -0.7020997375328074108, -0.05778040916215522460, 0.4822834645669289988 ) ) ;
#67462 = CARTESIAN_POINT ( 'NONE',  ( -0.6627296587926503335, -0.6692913385826771977, 0.1292274648535927661 ) ) ;
#67463 = CARTESIAN_POINT ( 'NONE',  ( -0.4091458600556402980, -0.2362204724409451284, -0.05249343832020997302 ) ) ;
#67464 = CARTESIAN_POINT ( 'NONE',  ( -9.674558042662121740E-17, 0.3949938075777409963, -2.519685039370078705 ) ) ;
#67465 = VERTEX_POINT ( 'NONE', #25500 ) ;
#67466 = CARTESIAN_POINT ( 'NONE',  ( 0.8792650918635177559, -0.004921259842519576551, 0.3153832671262227771 ) ) ;
#67467 = CARTESIAN_POINT ( 'NONE',  ( -0.1049643490035302024, -0.3917322834645671215, -1.009186351706036433 ) ) ;
#67468 = CARTESIAN_POINT ( 'NONE',  ( 0.9908136482939640111, 0.2952755905511810774, -0.1292274648535930714 ) ) ;
#67469 = EDGE_CURVE ( 'NONE', #72870, #55060, #34725, .T. ) ;
#67470 = CARTESIAN_POINT ( 'NONE',  ( 2.795275590551181910, 1.535433070866142335, 0.000000000000000000 ) ) ;
#67471 = CARTESIAN_POINT ( 'NONE',  ( -1.318897637795274802, -0.4536011799217368745, -0.2665933059059886201 ) ) ;
#67472 = CARTESIAN_POINT ( 'NONE',  ( 2.795275590551181910, 1.771653543307087242, 0.000000000000000000 ) ) ;
#67473 = CARTESIAN_POINT ( 'NONE',  ( -1.515748031496062076, 0.1660481256975883668, -0.3530559997133364547 ) ) ;
#67474 = CARTESIAN_POINT ( 'NONE',  ( 0.2690288713910767848, 0.2952755905511811885, 0.1292274648535926551 ) ) ;
#67475 = CARTESIAN_POINT ( 'NONE',  ( -0.3917322834645670659, 0.1049643490035301607, -0.2703218915672423450 ) ) ;
#67476 = CARTESIAN_POINT ( 'NONE',  ( 0.08530183727034192087, -0.05778040916215522460, 0.4822834645669289988 ) ) ;
#67477 = CARTESIAN_POINT ( 'NONE',  ( -0.9317585301837263412, -0.004921259842519576551, 0.3153832671262227771 ) ) ;
#67478 = CARTESIAN_POINT ( 'NONE',  ( 0.8858267716535438430, -0.5400638737290845981, -0.3530559997133363437 ) ) ;
#67479 = CARTESIAN_POINT ( 'NONE',  ( -0.2099737532808391705, -0.6046776061558809534, -0.2411417322834644161 ) ) ;
#67480 = CARTESIAN_POINT ( 'NONE',  ( 0.4921259842519691841, 0.1660481256975885056, 0.3530559997133364547 ) ) ;
#67481 = DIRECTION ( 'NONE',  ( -1.000000000000000000, -3.412570772413390973E-16, 0.000000000000000000 ) ) ;
#67482 = CARTESIAN_POINT ( 'NONE',  ( -0.3917322834645671770, 0.1049643490035302024, -1.604350024443256695 ) ) ;
#67483 = CARTESIAN_POINT ( 'NONE',  ( 0.8727034120734913358, -0.05778040916215522460, 0.4822834645669289988 ) ) ;
#67484 = CARTESIAN_POINT ( 'NONE',  ( 0.07874015748031558404, -0.1870078740157480879, -0.4822834645669291653 ) ) ;
#67485 = CARTESIAN_POINT ( 'NONE',  ( -1.076115485564303809, -0.6046776061558809534, -0.2411417322834644161 ) ) ;
#67486 = CARTESIAN_POINT ( 'NONE',  ( 1.292650918635171564, 0.2952755905511811885, 0.1292274648535926551 ) ) ;
#67487 = CARTESIAN_POINT ( 'NONE',  ( 0.5971128608923891301, 0.2952755905511810774, -0.1292274648535930714 ) ) ;
#67488 = CARTESIAN_POINT ( 'NONE',  ( -0.2867679344610364334, -0.2867679344610367109, -0.9311023622047245318 ) ) ;
#67489 = CARTESIAN_POINT ( 'NONE',  ( -0.4593175853018366950, 0.05413385826771666132, 0.4176697321401328100 ) ) ;
#67490 = CARTESIAN_POINT ( 'NONE',  ( 0.6364829396325465405, -0.3162353388693409650, -0.4822834645669289433 ) ) ;
#67491 = CARTESIAN_POINT ( 'NONE',  ( 0.08530183727034192087, -0.05778040916215522460, 0.4822834645669289988 ) ) ;
#67492 = CARTESIAN_POINT ( 'NONE',  ( 0.6955380577427828781, -0.3690944881889763329, 0.3153832671262228327 ) ) ;
#67493 = CARTESIAN_POINT ( 'NONE',  ( -1.437007874015747477, -0.5400638737290844871, 0.3530559997133364547 ) ) ;
#67494 = DIRECTION ( 'NONE',  ( 0.000000000000000000, -1.000000000000000000, 0.000000000000000000 ) ) ;
#67495 = CARTESIAN_POINT ( 'NONE',  ( 0.2034120734908142214, 0.2952755905511810774, -0.1292274648535930714 ) ) ;
#67496 = AXIS2_PLACEMENT_3D ( 'NONE', #9792, #10631, #80516 ) ;
#67497 = CARTESIAN_POINT ( 'NONE',  ( -0.4724409448818898682, -8.678599364036362592E-17, -0.9035433070866141225 ) ) ;
#67498 = CARTESIAN_POINT ( 'NONE',  ( -0.3917322834645670104, -7.196005306013484475E-17, -2.393700787401574992 ) ) ;
#67499 = ORIENTED_EDGE ( 'NONE', *, *, #23397, .T. ) ;
#67500 = ORIENTED_EDGE ( 'NONE', *, *, #72060, .T. ) ;
#67501 = CARTESIAN_POINT ( 'NONE',  ( 1.181102362204725198, -0.1870078740157479769, 0.4822834645669291653 ) ) ;
#67502 = CARTESIAN_POINT ( 'NONE',  ( 0.6561679790026253567, 0.1283753931104748280, 0.1820866141732283561 ) ) ;
#67504 = CARTESIAN_POINT ( 'NONE',  ( 0.4744094488189113945, 1.537401574803149984, -3.937007874015760578 ) ) ;
#67503 = CARTESIAN_POINT ( 'NONE',  ( 0.6299212598424784870, 2.165354330708661568, 3.937007874015796105 ) ) ;
#67505 = CARTESIAN_POINT ( 'NONE',  ( -0.1958661417322834220, -0.3392501089628018884, -0.6227034120734910028 ) ) ;
#67506 = CARTESIAN_POINT ( 'NONE',  ( -0.4359958488159683676, 1.724409448818897905, -1.033875059083678272 ) ) ;
#67507 = CARTESIAN_POINT ( 'NONE',  ( -0.1958661417322834220, -0.3392501089628018884, -1.410104986876640654 ) ) ;
#67508 = CARTESIAN_POINT ( 'NONE',  ( -0.3460692066303960313, 0.1998031496062989965, -2.465223097112860806 ) ) ;
#67509 = CARTESIAN_POINT ( 'NONE',  ( 1.049868766404200127, -0.6046776061558809534, -0.2411417322834644161 ) ) ;
#67510 = CARTESIAN_POINT ( 'NONE',  ( -1.003937007874014853, 0.1660481256975885056, 0.3530559997133364547 ) ) ;
#67511 = CARTESIAN_POINT ( 'NONE',  ( -0.8595800524934373854, -0.3162353388693409650, -0.4822834645669289433 ) ) ;
#67512 = CARTESIAN_POINT ( 'NONE',  ( 0.5446194225721792126, -0.05778040916215560624, -0.4822834645669293319 ) ) ;
#67513 = ORIENTED_EDGE ( 'NONE', *, *, #34562, .T. ) ;
#67514 = CARTESIAN_POINT ( 'NONE',  ( 1.292650918635171564, 0.2952755905511811885, 0.1292274648535926551 ) ) ;
#67515 = CARTESIAN_POINT ( 'NONE',  ( 1.200787401574803681, 0.1012011053420777407, 0.2882089793578256898 ) ) ;
#67516 = APPLICATION_PROTOCOL_DEFINITION ( 'draft international standard', 'automotive_design', 1998, #65425 ) ;
#67517 = CARTESIAN_POINT ( 'NONE',  ( 1.548556430446194954, 0.1283753931104746893, -0.1820866141732285504 ) ) ;
#67518 = LINE ( 'NONE', #35943, #54637 ) ;
#67519 = CARTESIAN_POINT ( 'NONE',  ( -1.246719160104985846, -0.3690944881889765550, -0.3153832671262227771 ) ) ;
#67520 = DIRECTION ( 'NONE',  ( -0.7071067811865489050, -0.000000000000000000, 0.7071067811865460184 ) ) ;
#67521 = CARTESIAN_POINT ( 'NONE',  ( 0.07217847769028949700, -0.3162353388693405765, 0.4822834645669290543 ) ) ;
#67523 = CARTESIAN_POINT ( 'NONE',  ( -1.220472440944881054, 2.401574803149606474, 0.5309055118110237448 ) ) ;
#67522 = DIRECTION ( 'NONE',  ( 1.000000000000000000, -0.000000000000000000, -0.000000000000000000 ) ) ;
#67524 = CARTESIAN_POINT ( 'NONE',  ( -1.220472440944881054, 0.1771653543307087630, 0.000000000000000000 ) ) ;
#67525 = CARTESIAN_POINT ( 'NONE',  ( 0.2034120734908144990, -0.6692913385826771977, 0.1292274648535927661 ) ) ;
#67526 = CARTESIAN_POINT ( 'NONE',  ( 1.292650918635171564, 0.1771653543307087630, 0.09757992244046791164 ) ) ;
#67527 = CARTESIAN_POINT ( 'NONE',  ( 0.2867679344610365999, -0.2867679344610365999, -1.438300894191914425 ) ) ;
#67528 = CARTESIAN_POINT ( 'NONE',  ( -1.272965879265091305, -0.3690944881889763329, 0.3153832671262228327 ) ) ;
#67529 = CARTESIAN_POINT ( 'NONE',  ( 1.351706036745407680, 0.05413385826771666132, 0.4176697321401328100 ) ) ;
#67530 = CARTESIAN_POINT ( 'NONE',  ( 0.1641164824122239851, 1.933755502706929530, 0.2669431538071869725 ) ) ;
#67531 = CARTESIAN_POINT ( 'NONE',  ( -0.3543307086614165824, -0.6692913385826771977, 8.415575281601705876E-17 ) ) ;
#67532 = CARTESIAN_POINT ( 'NONE',  ( -1.489501312335957062, -0.08942795157527998196, 0.3641732283464567121 ) ) ;
#67533 = CARTESIAN_POINT ( 'NONE',  ( -0.2362204724409442680, -0.1870078740157480601, -0.3641732283464567677 ) ) ;
#67534 = ADVANCED_FACE ( 'NONE', ( #64650 ), #27177, .F. ) ;
#67535 = CARTESIAN_POINT ( 'NONE',  ( -0.8661417322834640276, -0.1870078740157480879, -0.4822834645669291653 ) ) ;
#67536 = CARTESIAN_POINT ( 'NONE',  ( -1.561679790026246017, -0.3690944881889765550, -0.3153832671262227771 ) ) ;
#67537 = CARTESIAN_POINT ( 'NONE',  ( -0.3392501089628019995, 0.1958661417322831999, -0.6529064548894508713 ) ) ;
#67538 = CARTESIAN_POINT ( 'NONE',  ( 0.1968503937007881344, 0.2952755905511811885, 0.000000000000000000 ) ) ;
#67539 =( BOUNDED_CURVE ( )  B_SPLINE_CURVE ( 2, ( #33059, #7818, #58729, #52398, #59147, #1504, #20855, #46507, #29651, #61646, #16629, #54905, #30062 ),
 .UNSPECIFIED., .F., .F. ) 
 B_SPLINE_CURVE_WITH_KNOTS ( ( 3, 2, 2, 2, 2, 2, 3 ),
 ( 0.7374999999999999334, 0.7416666666666665853, 0.7458333333333333481, 0.7500000000000000000, 0.7541666666666666519, 0.7583333333333334147, 0.7625000000000000666 ),
 .UNSPECIFIED. ) 
 CURVE ( )  GEOMETRIC_REPRESENTATION_ITEM ( )  RATIONAL_B_SPLINE_CURVE ( ( 1.000000000000000888, 0.9659258262890674240, 1.000000000000000000, 0.9659258262890683122, 1.000000000000000000, 0.9659258262890683122, 1.000000000000000000, 0.9659258262890683122, 1.000000000000000000, 0.9659258262890683122, 1.000000000000000000, 0.9659258262890674240, 1.000000000000000888 ) ) 
 REPRESENTATION_ITEM ( '' )  );
#67540 = EDGE_CURVE ( 'NONE', #58460, #52853, #8250, .T. ) ;
#67541 = CARTESIAN_POINT ( 'NONE',  ( 0.4724409448818898682, 2.892866454678787531E-17, -0.2755905511811023723 ) ) ;
#67542 = CARTESIAN_POINT ( 'NONE',  ( 5.785732909357575061E-17, -0.4724409448818898682, -2.045275590551181022 ) ) ;
#67543 = CARTESIAN_POINT ( 'NONE',  ( -1.030183727034119867, -0.05778040916215560624, -0.4822834645669293319 ) ) ;
#67544 = CARTESIAN_POINT ( 'NONE',  ( -0.6102362204724400829, 0.07958543189024085140, 0.2665933059059887866 ) ) ;
#67545 = CARTESIAN_POINT ( 'NONE',  ( -0.4852136692201448609, 0.004960608223778509643, -0.3437734562760191848 ) ) ;
#67546 = CARTESIAN_POINT ( 'NONE',  ( -0.1377952755905504645, -0.5400638737290845981, -0.3530559997133363437 ) ) ;
#67547 = CARTESIAN_POINT ( 'NONE',  ( 0.2559055118110243332, 0.07958543189024085140, 0.2665933059059887866 ) ) ;
#67548 = CARTESIAN_POINT ( 'NONE',  ( -1.240157480314959759, 0.07958543189024085140, 0.2665933059059887866 ) ) ;
#67549 = CARTESIAN_POINT ( 'NONE',  ( -1.443569553805773564, -0.6046776061558807314, 0.2411417322834647770 ) ) ;
#67550 = CARTESIAN_POINT ( 'NONE',  ( -1.463254593175852492, -0.6692913385826773087, -0.1292274648535924053 ) ) ;
#67551 = CARTESIAN_POINT ( 'NONE',  ( 1.541994750656168645, 0.2952755905511810774, -0.1292274648535930714 ) ) ;
#67552 = DIRECTION ( 'NONE',  ( 1.000000000000000000, 0.000000000000000000, -0.000000000000000000 ) ) ;
#67553 = CARTESIAN_POINT ( 'NONE',  ( 0.5971128608923891301, 0.1771653543307087075, -0.09757992244046823083 ) ) ;
#67554 = CARTESIAN_POINT ( 'NONE',  ( 0.7939632545931766261, -0.3162353388693409650, -0.4822834645669289433 ) ) ;
#67555 = CARTESIAN_POINT ( 'NONE',  ( -1.586052503253848611, 0.7480314960629931287, 0.1653254495020559378 ) ) ;
#67556 = CARTESIAN_POINT ( 'NONE',  ( 1.437007874015748810, 0.07958543189024085140, 0.2665933059059887866 ) ) ;
#67557 = AXIS2_PLACEMENT_3D ( 'NONE', #3894, #55216, #80103 ) ;
#67558 = ORIENTED_EDGE ( 'NONE', *, *, #51210, .T. ) ;
#67559 = EDGE_CURVE ( 'NONE', #38353, #45259, #52417, .T. ) ;
#67560 = CARTESIAN_POINT ( 'NONE',  ( -1.062992125984250968, -0.6692913385826771977, 8.415575281601705876E-17 ) ) ;
#67561 = EDGE_CURVE ( 'NONE', #77098, #51714, #43920, .T. ) ;
#67562 = CARTESIAN_POINT ( 'NONE',  ( -0.8530183727034112984, 0.05413385826771666132, 0.4176697321401328100 ) ) ;
#67563 = CARTESIAN_POINT ( 'NONE',  ( 0.4593175853018379162, -0.4281496062992124485, 0.4176697321401328655 ) ) ;
#67564 = CARTESIAN_POINT ( 'NONE',  ( -1.391076115485563758, 0.1283753931104748280, 0.1820866141732283561 ) ) ;
#67565 = CARTESIAN_POINT ( 'NONE',  ( 0.1998031496062994128, -0.3460692066303957537, -2.215879265091863726 ) ) ;
#67566 = CARTESIAN_POINT ( 'NONE',  ( 1.338582677165355062, -0.1870078740157480601, -0.3641732283464567677 ) ) ;
#67567 = CARTESIAN_POINT ( 'NONE',  ( 0.4593175853018380828, 0.05413385826771626580, -0.4176697321401330321 ) ) ;
#67568 = CARTESIAN_POINT ( 'NONE',  ( 0.6889763779527563470, 0.1660481256975883668, -0.3530559997133364547 ) ) ;
#67569 = CARTESIAN_POINT ( 'NONE',  ( -1.614173228346456712, 1.267785121476993737, -0.1372047244094478091 ) ) ;
#67570 = CARTESIAN_POINT ( 'NONE',  ( -0.3460692066303960868, 0.1998031496062990242, -1.601049868766404094 ) ) ;
#67571 = CARTESIAN_POINT ( 'NONE',  ( 0.1058382717557499880, 0.3949938075777411073, -1.095800524934383180 ) ) ;
#67572 = CARTESIAN_POINT ( 'NONE',  ( 0.1998031496062992740, 0.3460692066303959757, -2.664041994750656173 ) ) ;
#67573 = DIRECTION ( 'NONE',  ( 0.000000000000000000, 0.000000000000000000, -1.000000000000000000 ) ) ;
#67574 = CARTESIAN_POINT ( 'NONE',  ( -0.3917322834645671215, 0.1049643490035301469, -0.02493438320209968861 ) ) ;
#67575 = CARTESIAN_POINT ( 'NONE',  ( 0.03937007874015806264, 0.1771653543307087630, 0.000000000000000000 ) ) ;
#67576 = CARTESIAN_POINT ( 'NONE',  ( -0.2559055118110230564, 0.1660481256975883668, -0.3530559997133364547 ) ) ;
#67577 = CARTESIAN_POINT ( 'NONE',  ( 0.8333333333333340365, 0.2952755905511810774, -0.1292274648535930714 ) ) ;
#67578 = CARTESIAN_POINT ( 'NONE',  ( 0.2891555358219910499, -0.2891555358219909944, -2.064960629921260171 ) ) ;
#67579 = CARTESIAN_POINT ( 'NONE',  ( -0.1115485564304453947, -0.5511811023622046335, 0.09757992244046803654 ) ) ;
#67580 = CARTESIAN_POINT ( 'NONE',  ( -1.266404199475064773, -0.05778040916215560624, -0.4822834645669293319 ) ) ;
#67581 = CARTESIAN_POINT ( 'NONE',  ( 1.043307086614173818, -0.5400638737290845981, -0.3530559997133363437 ) ) ;
#67582 = CARTESIAN_POINT ( 'NONE',  ( -0.3458507752293906723, -0.3458507752293910609, -2.578740157480315265 ) ) ;
#67583 = CARTESIAN_POINT ( 'NONE',  ( 0.3996062992125986035, 0.1070741851644054776, -1.699475065616798064 ) ) ;
#67584 = CARTESIAN_POINT ( 'NONE',  ( 0.2362204724409449064, 0.4091458600556404646, -2.740813648293963567 ) ) ;
#67585 = VECTOR ( 'NONE', #3225, 39.37007874015748143 ) ;
#67586 = EDGE_LOOP ( 'NONE', ( #24668, #54134, #74832, #41911 ) ) ;
#67587 = EDGE_LOOP ( 'NONE', ( #3940, #23752, #71857, #21219 ) ) ;
#67588 = CARTESIAN_POINT ( 'NONE',  ( 0.8398950131233602345, 0.2306618581243847221, -0.2411417322834647770 ) ) ;
#67589 = CARTESIAN_POINT ( 'NONE',  ( 1.561679790026247350, -0.3690944881889763329, 0.3153832671262228327 ) ) ;
#67591 = CARTESIAN_POINT ( 'NONE',  ( -1.463254593175852492, 0.2952755905511811885, 0.1292274648535926551 ) ) ;
#67590 = CARTESIAN_POINT ( 'NONE',  ( -1.463254593175852492, 0.1771653543307087630, 0.09757992244046791164 ) ) ;
#67592 = CARTESIAN_POINT ( 'NONE',  ( -0.3917322834645671215, 0.1049643490035301469, 0.1975065616797899160 ) ) ;
#67593 = DIRECTION ( 'NONE',  ( -1.000000000000000000, 0.000000000000000000, 0.000000000000000000 ) ) ;
#67594 = CARTESIAN_POINT ( 'NONE',  ( 1.141732283464567788, -0.6692913385826771977, 8.415575281601705876E-17 ) ) ;
#67595 = CARTESIAN_POINT ( 'NONE',  ( -1.725721784776902190, -0.05778040916215522460, 0.4822834645669289988 ) ) ;
#67596 = CARTESIAN_POINT ( 'NONE',  ( -0.04593175853018302557, -0.6692913385826773087, -0.1292274648535924053 ) ) ;
#67597 = CARTESIAN_POINT ( 'NONE',  ( -0.7480314960629914633, 0.2952755905511811885, 0.000000000000000000 ) ) ;
#67598 = CARTESIAN_POINT ( 'NONE',  ( 1.528871391076116026, -0.6692913385826773087, -0.1292274648535924053 ) ) ;
#67599 = CARTESIAN_POINT ( 'NONE',  ( 0.3917322834645670104, -0.1049643490035303411, -0.1961942257217848817 ) ) ;
#67600 = CARTESIAN_POINT ( 'NONE',  ( 0.1509186351706042484, -0.3162353388693405765, 0.4822834645669290543 ) ) ;
#67601 = CARTESIAN_POINT ( 'NONE',  ( 0.3917322834645670104, 2.398668435337828261E-17, -2.157480314960630086 ) ) ;
#67602 = CARTESIAN_POINT ( 'NONE',  ( -1.062992125984250968, -0.5511811023622047445, 6.969142054262312111E-17 ) ) ;
#67603 = ORIENTED_EDGE ( 'NONE', *, *, #40920, .T. ) ;
#67604 = CARTESIAN_POINT ( 'NONE',  ( -0.1974969037888703871, -0.3420746716998661063, -2.112860892388451539 ) ) ;
#67605 = EDGE_LOOP ( 'NONE', ( #77653, #72667, #11183, #74950 ) ) ;
#67606 = CARTESIAN_POINT ( 'NONE',  ( -1.313877454013331780, 1.062992125984252079, 0.6999040823587869831 ) ) ;
#67607 = CARTESIAN_POINT ( 'NONE',  ( -1.620734908136482577, -0.6692913385826773087, -0.1292274648535924053 ) ) ;
#67608 = CARTESIAN_POINT ( 'NONE',  ( 0.2925321140481932369, 0.2925321140481932369, -1.082677165354330562 ) ) ;
#67609 = CARTESIAN_POINT ( 'NONE',  ( 1.640419947506562393, -0.3690944881889763329, 0.3153832671262228327 ) ) ;
#67610 = CARTESIAN_POINT ( 'NONE',  ( -0.3458507752293906723, -0.3458507752293910609, -0.7657480314960628531 ) ) ;
#67611 = CARTESIAN_POINT ( 'NONE',  ( 0.4396325459317593221, 0.2952755905511810219, -0.1292274648535930437 ) ) ;
#67612 = CARTESIAN_POINT ( 'NONE',  ( 0.004548682155579284771, -0.3974711515625322655, -2.755905511811026276 ) ) ;
#67613 = CARTESIAN_POINT ( 'NONE',  ( 0.3917322834645670104, 2.398668435337828261E-17, -0.2027559055118111353 ) ) ;
#67614 = VECTOR ( 'NONE', #25037, 39.37007874015748143 ) ;
#67615 = CARTESIAN_POINT ( 'NONE',  ( -0.4527559055118102749, -0.4536011799217368745, -0.2665933059059886201 ) ) ;
#67616 = CARTESIAN_POINT ( 'NONE',  ( -0.7742782152230965886, -0.004921259842519576551, 0.3153832671262227771 ) ) ;
#67617 = CARTESIAN_POINT ( 'NONE',  ( -1.200787401574802349, -0.5400638737290844871, 0.3530559997133364547 ) ) ;
#67618 = CARTESIAN_POINT ( 'NONE',  ( 0.5380577427821529035, 0.05413385826771626580, -0.4176697321401330321 ) ) ;
#67619 = CARTESIAN_POINT ( 'NONE',  ( -1.469816272965878357, 0.2306618581243848609, 0.2411417322834645549 ) ) ;
#67620 = CARTESIAN_POINT ( 'NONE',  ( 0.1049643490035304938, -0.3917322834645669549, -0.07742782152230967552 ) ) ;
#67621 = VERTEX_POINT ( 'NONE', #27599 ) ;
#67622 = CARTESIAN_POINT ( 'NONE',  ( -1.587926509186350810, 0.05413385826771626580, -0.4176697321401330321 ) ) ;
#67623 = DIRECTION ( 'NONE',  ( 0.000000000000000000, 0.000000000000000000, 1.000000000000000000 ) ) ;
#67624 =( NAMED_UNIT ( * ) SI_UNIT ( $, .STERADIAN. ) SOLID_ANGLE_UNIT ( ) );
#67625 = CARTESIAN_POINT ( 'NONE',  ( 0.4091458600556404646, -0.2362204724409448231, -1.522309711286089273 ) ) ;
#67626 = EDGE_CURVE ( 'NONE', #74015, #77721, #64821, .T. ) ;
#67627 = CARTESIAN_POINT ( 'NONE',  ( 2.170146923806634653, 1.537401574803149984, -0.4744094488188970171 ) ) ;
#67628 = CARTESIAN_POINT ( 'NONE',  ( 0.1049643490035304938, -0.3917322834645669549, -0.8648293963254591876 ) ) ;
#67629 =( BOUNDED_CURVE ( )  B_SPLINE_CURVE ( 3, ( #19904, #71667, #72502, #2213 ),
 .UNSPECIFIED., .F., .F. ) 
 B_SPLINE_CURVE_WITH_KNOTS ( ( 4, 4 ),
 ( 1.631439550826413676, 1.635357296112374570 ),
 .UNSPECIFIED. ) 
 CURVE ( )  GEOMETRIC_REPRESENTATION_ITEM ( )  RATIONAL_B_SPLINE_CURVE ( ( 1.000000000000000000, 0.9999987209397318555, 0.9999987209397318555, 1.000000000000000000 ) ) 
 REPRESENTATION_ITEM ( '' )  );
#67630 = CARTESIAN_POINT ( 'NONE',  ( 0.1467283321115955275, 0.3676198365746946584, -2.752234641088710632 ) ) ;
#67631 = CARTESIAN_POINT ( 'NONE',  ( -0.7217847769028863381, -0.4281496062992124485, 0.4176697321401328655 ) ) ;
#67632 = CARTESIAN_POINT ( 'NONE',  ( 1.502624671916010790, -0.05778040916215522460, 0.4822834645669289988 ) ) ;
#67634 = CARTESIAN_POINT ( 'NONE',  ( 3.937007874015748143, 2.559055118110236560, 0.5314960629921260393 ) ) ;
#67633 = DIRECTION ( 'NONE',  ( 0.000000000000000000, 0.000000000000000000, 1.000000000000000000 ) ) ;
#67635 = CARTESIAN_POINT ( 'NONE',  ( -1.351706036745406347, 0.05413385826771626580, -0.4176697321401330321 ) ) ;
#67636 = CARTESIAN_POINT ( 'NONE',  ( -1.010498687664041384, -0.4281496062992127816, -0.4176697321401328100 ) ) ;
#67637 = CARTESIAN_POINT ( 'NONE',  ( -0.1958661417322834497, -0.3392501089628018884, 0.1693106543645162554 ) ) ;
#67638 = CARTESIAN_POINT ( 'NONE',  ( 0.04593175853018440641, 0.1771653543307087075, -0.09757992244046823083 ) ) ;
#67639 = CARTESIAN_POINT ( 'NONE',  ( -0.2867679344610364334, -0.2867679344610367109, -0.4586614173228347746 ) ) ;
#67640 = CARTESIAN_POINT ( 'NONE',  ( -0.03937007874015669567, 0.1771653543307087630, 0.000000000000000000 ) ) ;
#67641 = CARTESIAN_POINT ( 'NONE',  ( 0.8530183727034126306, -0.004921259842519870586, -0.3153832671262229437 ) ) ;
#67642 = CARTESIAN_POINT ( 'NONE',  ( 0.4199475065616803948, -0.6046776061558809534, -0.2411417322834644161 ) ) ;
#67643 = CARTESIAN_POINT ( 'NONE',  ( -0.1181102362204717315, -0.5511811023622047445, 6.969142054262312111E-17 ) ) ;
#67644 = CARTESIAN_POINT ( 'NONE',  ( -0.1958661417322834220, -0.3392501089628018884, -2.419947506561679784 ) ) ;
#67645 = CARTESIAN_POINT ( 'NONE',  ( 1.371391076115485719, -0.6692913385826773087, -0.1292274648535924053 ) ) ;
#67646 = CARTESIAN_POINT ( 'NONE',  ( -1.430446194225720724, -0.004921259842519870586, -0.3153832671262229437 ) ) ;
#67647 = CARTESIAN_POINT ( 'NONE',  ( 0.1265901696524990294, -0.4724409448818896462, -0.3195538057742782212 ) ) ;
#67648 = CARTESIAN_POINT ( 'NONE',  ( 0.1771653543307093182, 0.1660481256975885056, 0.3530559997133364547 ) ) ;
#67649 = CARTESIAN_POINT ( 'NONE',  ( -0.4986876640419939388, 0.2306618581243847221, -0.2411417322834647770 ) ) ;
#67650 = CARTESIAN_POINT ( 'NONE',  ( 0.000000000000000000, 0.000000000000000000, 0.000000000000000000 ) ) ;
#67651 = CARTESIAN_POINT ( 'NONE',  ( 0.5052493438320215802, 0.1771653543307087630, 0.09757992244046791164 ) ) ;
#67652 = CARTESIAN_POINT ( 'NONE',  ( -0.4068241469816267775, 0.05413385826771626580, -0.4176697321401330321 ) ) ;
#67653 = CARTESIAN_POINT ( 'NONE',  ( -0.5380577427821514602, 0.05413385826771666132, 0.4176697321401328100 ) ) ;
#67654 = DIRECTION ( 'NONE',  ( -0.000000000000000000, 1.000000000000000000, 1.224646799147353207E-16 ) ) ;
#67655 = DIRECTION ( 'NONE',  ( 0.000000000000000000, 0.000000000000000000, 1.000000000000000000 ) ) ;
#67656 = AXIS2_PLACEMENT_3D ( 'NONE', #4394, #17461, #68788 ) ;
#67657 = CARTESIAN_POINT ( 'NONE',  ( 0.03937007874015833325, -0.6692913385826771977, 8.415575281601705876E-17 ) ) ;
#67658 = CARTESIAN_POINT ( 'NONE',  ( 0.3996062992125984925, 0.1070741851644054637, -1.461286089238844843 ) ) ;
#67659 = CARTESIAN_POINT ( 'NONE',  ( -1.614173228346457378, 1.330640075373402897, -0.1372047244094477536 ) ) ;
#67660 = CARTESIAN_POINT ( 'NONE',  ( -0.06561679790026180015, -0.3690944881889765550, -0.3153832671262227771 ) ) ;
#67661 = CARTESIAN_POINT ( 'NONE',  ( -0.5971128608923877978, 0.2952755905511811885, 0.1292274648535926551 ) ) ;
#67662 = CARTESIAN_POINT ( 'NONE',  ( 1.686351706036745890, 0.2952755905511811885, 0.1292274648535926551 ) ) ;
#67663 = CARTESIAN_POINT ( 'NONE',  ( 1.312335958005250269, -0.6046776061558807314, 0.2411417322834647770 ) ) ;
#67664 = DIRECTION ( 'NONE',  ( -1.000000000000000000, -0.000000000000000000, -0.000000000000000000 ) ) ;
#67665 = CARTESIAN_POINT ( 'NONE',  ( -0.4855643044619415427, -0.3690944881889763329, 0.3153832671262228327 ) ) ;
#67666 = CARTESIAN_POINT ( 'NONE',  ( 0.3460692066303959202, -0.1998031496062991630, -0.3392388451443569819 ) ) ;
#67667 = CARTESIAN_POINT ( 'NONE',  ( -0.2925321140481930704, -0.2925321140481933480, -0.6889763779527556808 ) ) ;
#67668 = AXIS2_PLACEMENT_3D ( 'NONE', #70748, #63597, #13508 ) ;
#67669 = CARTESIAN_POINT ( 'NONE',  ( -0.2867679344610365444, -0.2867679344610367664, -2.890439263288400618 ) ) ;
#67670 = CARTESIAN_POINT ( 'NONE',  ( 1.548556430446194954, 0.1283753931104746893, -0.1820866141732285504 ) ) ;
#67671 = CARTESIAN_POINT ( 'NONE',  ( 0.9908136482939640111, 0.1771653543307087075, -0.09757992244046823083 ) ) ;
#67672 = CARTESIAN_POINT ( 'NONE',  ( 0.9120734908136489683, -0.6692913385826771977, 0.1292274648535927661 ) ) ;
#67673 = CARTESIAN_POINT ( 'NONE',  ( 0.4199475065616804503, 0.1539470093639523085, 0.1968503937007873850 ) ) ;
#67674 = CARTESIAN_POINT ( 'NONE',  ( 0.9973753280839902091, 0.2306618581243847221, -0.2411417322834647770 ) ) ;
#67675 = CARTESIAN_POINT ( 'NONE',  ( -0.1058382717557497660, -0.3949938075777411073, -0.7788713910761156933 ) ) ;
#67676 = CARTESIAN_POINT ( 'NONE',  ( 1.017060367454068803, -0.2845877964562159024, 0.3641732283464567677 ) ) ;
#67677 = CARTESIAN_POINT ( 'NONE',  ( -0.06561679790026180015, 0.05413385826771666132, 0.4176697321401328100 ) ) ;
#67678 = CARTESIAN_POINT ( 'NONE',  ( -0.6299212598425188991, -0.1870078740157480879, -0.4822834645669291653 ) ) ;
#67679 = CARTESIAN_POINT ( 'NONE',  ( -0.4600214019799515053, 0.000000000000000000, 0.3464511005275205946 ) ) ;
#67680 = CARTESIAN_POINT ( 'NONE',  ( 0.4724409448818896462, 0.1265901696524990294, -1.227034120734908029 ) ) ;
#67681 = CARTESIAN_POINT ( 'NONE',  ( 0.2925321140481932369, 0.2925321140481932369, -2.342519685039369914 ) ) ;
#67682 = CARTESIAN_POINT ( 'NONE',  ( 0.3740157480314966754, 0.07958543189024071263, -0.2665933059059888421 ) ) ;
#67683 = EDGE_CURVE ( 'NONE', #10557, #68129, #34291, .T. ) ;
#67684 = ORIENTED_EDGE ( 'NONE', *, *, #79905, .T. ) ;
#67685 = CARTESIAN_POINT ( 'NONE',  ( -0.3917322834645671770, 0.1049643490035302024, -0.3445075047582172312 ) ) ;
#67686 = ORIENTED_EDGE ( 'NONE', *, *, #19758, .T. ) ;
#67687 = CARTESIAN_POINT ( 'NONE',  ( -0.3018372703412066094, 0.05413385826771666132, 0.4176697321401328100 ) ) ;
#67688 = CARTESIAN_POINT ( 'NONE',  ( -0.3477690288713902178, 0.2952755905511810774, -0.1292274648535930714 ) ) ;
#67689 = CARTESIAN_POINT ( 'NONE',  ( -0.4265091863517051496, -0.6692913385826771977, 0.1292274648535927661 ) ) ;
#67690 = CARTESIAN_POINT ( 'NONE',  ( 0.9055118110236227702, 0.2952755905511811885, 0.000000000000000000 ) ) ;
#67691 = EDGE_CURVE ( 'NONE', #28560, #17617, #12896, .T. ) ;
#67692 = CARTESIAN_POINT ( 'NONE',  ( -0.9251968503937002541, -0.5400638737290845981, -0.3530559997133363437 ) ) ;
#67693 = CARTESIAN_POINT ( 'NONE',  ( -0.3215223097112853146, -0.3162353388693405765, 0.4822834645669290543 ) ) ;
#67694 = CARTESIAN_POINT ( 'NONE',  ( 1.332020997375328974, -0.05778040916215560624, -0.4822834645669293319 ) ) ;
#67695 = CARTESIAN_POINT ( 'NONE',  ( 0.8267716535433077274, 0.2952755905511811885, 0.000000000000000000 ) ) ;
#67696 = CARTESIAN_POINT ( 'NONE',  ( 0.7611548556430454138, 0.2306618581243847221, -0.2411417322834647770 ) ) ;
#67697 = CARTESIAN_POINT ( 'NONE',  ( 0.3392501089628018884, -0.1958661417322834220, -1.041994750656167756 ) ) ;
#67698 = CARTESIAN_POINT ( 'NONE',  ( 0.02624671916010564918, -0.5023911411419708095, -0.1820866141732282451 ) ) ;
#67699 = ORIENTED_EDGE ( 'NONE', *, *, #35564, .T. ) ;
#67700 = CARTESIAN_POINT ( 'NONE',  ( -0.1058382717557497937, -0.3949938075777411628, -0.8595800524934383846 ) ) ;
#67701 = ORIENTED_EDGE ( 'NONE', *, *, #39397, .T. ) ;
#67702 = CARTESIAN_POINT ( 'NONE',  ( -0.7414698162729651543, 0.1771653543307087075, -0.09757992244046823083 ) ) ;
#67703 = CARTESIAN_POINT ( 'NONE',  ( -0.3740157480314953431, 0.1660481256975885056, 0.3530559997133364547 ) ) ;
#67704 = DIRECTION ( 'NONE',  ( -0.000000000000000000, -1.000000000000000000, -0.000000000000000000 ) ) ;
#67705 = CARTESIAN_POINT ( 'NONE',  ( -0.5577427821522301654, -0.05778040916215560624, -0.4822834645669293319 ) ) ;
#67706 = CARTESIAN_POINT ( 'NONE',  ( -0.2755905511811018171, 0.2952755905511811885, 0.000000000000000000 ) ) ;
#67707 = CARTESIAN_POINT ( 'NONE',  ( -1.299212598425196097, 0.2952755905511811885, 0.000000000000000000 ) ) ;
#67708 = CARTESIAN_POINT ( 'NONE',  ( -1.377952755905511140, 0.2952755905511811885, 0.000000000000000000 ) ) ;
#67709 = CARTESIAN_POINT ( 'NONE',  ( 0.8858267716535438430, 0.07958543189024085140, 0.2665933059059887866 ) ) ;
#67710 = CARTESIAN_POINT ( 'NONE',  ( -0.4724409448818904234, 0.1265901696524979470, -0.4245406824146981117 ) ) ;
#67711 = CARTESIAN_POINT ( 'NONE',  ( -0.2362204724409447953, -0.4091458600556404646, -0.6148293963254594097 ) ) ;
#67712 = CARTESIAN_POINT ( 'NONE',  ( 0.5905511811023629321, -0.5511811023622047445, 6.969142054262312111E-17 ) ) ;
#67713 = AXIS2_PLACEMENT_3D ( 'NONE', #56745, #63078, #23529 ) ;
#67714 = CARTESIAN_POINT ( 'NONE',  ( -0.1312335958005241554, -0.6046776061558809534, -0.2411417322834644161 ) ) ;
#67715 = CARTESIAN_POINT ( 'NONE',  ( -0.1837270341207340729, 0.2306618581243847221, -0.2411417322834647770 ) ) ;
#67716 = ORIENTED_EDGE ( 'NONE', *, *, #16485, .F. ) ;
#67717 = CARTESIAN_POINT ( 'NONE',  ( -0.1998031496062991907, -0.3460692066303959757, -1.640419947506561726 ) ) ;
#67718 = CARTESIAN_POINT ( 'NONE',  ( -0.6036745406824141069, 0.2306618581243848609, 0.2411417322834645549 ) ) ;
#67719 = EDGE_LOOP ( 'NONE', ( #37350, #24220, #48805, #45081 ) ) ;
#67720 = CARTESIAN_POINT ( 'NONE',  ( -0.3996062992125985480, -7.340648628747423112E-17, -1.061023622047243986 ) ) ;
#67721 = DIRECTION ( 'NONE',  ( 0.000000000000000000, -1.387778780781445676E-15, -1.000000000000000000 ) ) ;
#67722 = CARTESIAN_POINT ( 'NONE',  ( -0.8923884514435688198, 0.1283753931104746893, -0.1820866141732285504 ) ) ;
#67723 = CARTESIAN_POINT ( 'NONE',  ( -1.154855643044618851, -0.6046776061558809534, -0.2411417322834644161 ) ) ;
#67724 = CARTESIAN_POINT ( 'NONE',  ( -0.1265901696524993347, 0.4724409448818895907, -0.6364829396325458744 ) ) ;
#67725 = EDGE_CURVE ( 'NONE', #82476, #5673, #79901, .T. ) ;
#67726 = CARTESIAN_POINT ( 'NONE',  ( 0.3392501089628018884, -0.1958661417322834220, -2.709317585301837195 ) ) ;
#67727 = CARTESIAN_POINT ( 'NONE',  ( -1.496062992125983815, -0.1870078740157479769, 0.3641732283464567677 ) ) ;
#67728 = CARTESIAN_POINT ( 'NONE',  ( 0.2427821522309716595, -0.3162353388693409650, -0.4822834645669289433 ) ) ;
#67729 = CARTESIAN_POINT ( 'NONE',  ( 0.6233595800524942554, -0.05778040916215560624, -0.4822834645669293319 ) ) ;
#67730 = CARTESIAN_POINT ( 'NONE',  ( -0.4855643044619415427, -0.004921259842519870586, -0.3153832671262229437 ) ) ;
#67731 = CARTESIAN_POINT ( 'NONE',  ( -0.05905511811023545637, -0.5400638737290845981, -0.3530559997133363437 ) ) ;
#67732 = CARTESIAN_POINT ( 'NONE',  ( 0.3458507752293908943, -0.3458507752293908943, -2.379921259842520342 ) ) ;
#67733 = CARTESIAN_POINT ( 'NONE',  ( -0.4921259842519677963, 0.07958543189024071263, -0.2665933059059888421 ) ) ;
#67734 = CARTESIAN_POINT ( 'NONE',  ( -0.5314960629921254842, -0.5400638737290845981, -0.3530559997133363437 ) ) ;
#67735 = EDGE_CURVE ( 'NONE', #77301, #68995, #6570, .T. ) ;
#67736 = AXIS2_PLACEMENT_3D ( 'NONE', #82994, #77096, #76677 ) ;
#67737 = CARTESIAN_POINT ( 'NONE',  ( 0.3949938075777408852, 0.1058382717557500435, -1.933727034120735100 ) ) ;
#67738 = CARTESIAN_POINT ( 'NONE',  ( -1.719160104986876103, 0.05413385826771666132, 0.4176697321401328100 ) ) ;
#67739 = CARTESIAN_POINT ( 'NONE',  ( -0.05905511811023545637, -0.4536011799217368745, -0.2665933059059886201 ) ) ;
#67740 = CARTESIAN_POINT ( 'NONE',  ( 1.003937007874016407, -0.4536011799217367080, 0.2665933059059888421 ) ) ;
#67741 = CARTESIAN_POINT ( 'NONE',  ( -1.318897637795274802, -0.5400638737290845981, -0.3530559997133363437 ) ) ;
#67742 = CARTESIAN_POINT ( 'NONE',  ( -0.8202099737532799750, 0.1771653543307087075, -0.09757992244046823083 ) ) ;
#67743 = CARTESIAN_POINT ( 'NONE',  ( 1.614173228346456712, 1.496062992125984037, -0.1372047244094476703 ) ) ;
#67744 = CARTESIAN_POINT ( 'NONE',  ( -1.003937007874015297, -0.5400638737290845981, -0.3530559997133363437 ) ) ;
#67745 = CARTESIAN_POINT ( 'NONE',  ( -0.2690288713910754526, -0.6692913385826771977, 0.1292274648535927661 ) ) ;
#67746 = CARTESIAN_POINT ( 'NONE',  ( 0.2559055118110243332, 0.1660481256975885056, 0.3530559997133364547 ) ) ;
#67747 = CARTESIAN_POINT ( 'NONE',  ( 0.3392501089628018329, 0.1958661417322835052, -2.573471497866454794 ) ) ;
#67748 = CARTESIAN_POINT ( 'NONE',  ( -2.159196716652983739, 1.469708627452553706, -0.4698506773045486029 ) ) ;
#67749 = CARTESIAN_POINT ( 'NONE',  ( 0.3149606299212606708, -0.1870078740157480601, -0.3641732283464567677 ) ) ;
#67750 = CARTESIAN_POINT ( 'NONE',  ( 1.030183727034121421, -0.3162353388693409650, -0.4822834645669289433 ) ) ;
#67751 = CARTESIAN_POINT ( 'NONE',  ( -1.076115485564303809, 0.1283753931104748280, 0.1820866141732283561 ) ) ;
#67752 = CARTESIAN_POINT ( 'NONE',  ( 1.148293963254593875, -0.6692913385826771977, 0.1292274648535927661 ) ) ;
#67753 = CARTESIAN_POINT ( 'NONE',  ( -1.620734908136482577, -0.5511811023622048555, -0.09757992244046775898 ) ) ;
#67754 = CARTESIAN_POINT ( 'NONE',  ( 1.594488188976378673, 0.07958543189024085140, 0.2665933059059887866 ) ) ;
#67755 = CARTESIAN_POINT ( 'NONE',  ( -0.7742782152230965886, 0.05413385826771666132, 0.4176697321401328100 ) ) ;
#67756 = CARTESIAN_POINT ( 'NONE',  ( 0.03280839895013198948, -0.5511811023622048555, -0.09757992244046775898 ) ) ;
#67757 = PLANE ( 'NONE',  #68964 ) ;
#67758 = CARTESIAN_POINT ( 'NONE',  ( 0.5971128608923890191, -0.5511811023622046335, 0.09757992244046803654 ) ) ;
#67759 = CARTESIAN_POINT ( 'NONE',  ( 0.01312335958005323398, -0.4281496062992127816, -0.4176697321401328100 ) ) ;
#67760 = CARTESIAN_POINT ( 'NONE',  ( -0.2925321140481930149, -0.2925321140481933480, -0.2933070866141732069 ) ) ;
#67761 = CARTESIAN_POINT ( 'NONE',  ( -1.286089238845143479, -0.6046776061558807314, 0.2411417322834647770 ) ) ;
#67762 = CARTESIAN_POINT ( 'NONE',  ( -0.1049643490035307020, 0.3917322834645669549, -1.823490813648294129 ) ) ;
#67763 = CARTESIAN_POINT ( 'NONE',  ( 1.010498687664042716, -0.004921259842519870586, -0.3153832671262229437 ) ) ;
#67764 = CARTESIAN_POINT ( 'NONE',  ( -0.07217847769028787330, -0.05778040916215522460, 0.4822834645669289988 ) ) ;
#67765 = CARTESIAN_POINT ( 'NONE',  ( -0.4068241469816264999, -0.4281496062992124485, 0.4176697321401328655 ) ) ;
#67766 = CARTESIAN_POINT ( 'NONE',  ( -0.4133858267716528645, -0.4536011799217367080, 0.2665933059059888421 ) ) ;
#67767 = FACE_OUTER_BOUND ( 'NONE', #19596, .T. ) ;
#67768 = CARTESIAN_POINT ( 'NONE',  ( -0.3018372703412066094, -0.3690944881889765550, -0.3153832671262227771 ) ) ;
#67769 = CARTESIAN_POINT ( 'NONE',  ( 0.4461942257217856311, 0.2306618581243847221, -0.2411417322834647770 ) ) ;
#67770 = CARTESIAN_POINT ( 'NONE',  ( -0.9973753280839886548, -0.5023911411419708095, -0.1820866141732282451 ) ) ;
#67771 = CARTESIAN_POINT ( 'NONE',  ( 0.2925321140481932369, -0.2925321140481931814, -1.120078740157480324 ) ) ;
#67772 = CARTESIAN_POINT ( 'NONE',  ( -1.240157480314959759, -0.5400638737290845981, -0.3530559997133363437 ) ) ;
#67773 = CARTESIAN_POINT ( 'NONE',  ( 0.4724409448818898682, 2.892866454678787531E-17, -2.165354330708661568 ) ) ;
#67774 = ORIENTED_EDGE ( 'NONE', *, *, #21915, .F. ) ;
#67775 = CARTESIAN_POINT ( 'NONE',  ( -1.719160104986876103, -0.004921259842519576551, 0.3153832671262227771 ) ) ;
#67776 = CARTESIAN_POINT ( 'NONE',  ( -0.3346456692913377662, -0.5400638737290844871, 0.3530559997133364547 ) ) ;
#67777 = CARTESIAN_POINT ( 'NONE',  ( 0.4744094488188886904, 1.537401574803149984, 2.554262525012303886 ) ) ;
#67778 = CARTESIAN_POINT ( 'NONE',  ( -1.122047244094487306, 0.1660481256975883668, -0.3530559997133364547 ) ) ;
#67779 = CARTESIAN_POINT ( 'NONE',  ( -0.3392501089628017219, -0.1958661417322836718, -1.396981627296587813 ) ) ;
#67780 = CARTESIAN_POINT ( 'NONE',  ( 0.3401783215957711048, 0.1988659768032686181, -1.220472440944881720 ) ) ;
#67781 = CARTESIAN_POINT ( 'NONE',  ( 1.482939632545932307, -0.4281496062992124485, 0.4176697321401328655 ) ) ;
#67782 = CARTESIAN_POINT ( 'NONE',  ( 0.2952755905511819101, 0.1660481256975883668, -0.3530559997133364547 ) ) ;
#67783 = DIRECTION ( 'NONE',  ( -0.000000000000000000, -1.000000000000000000, -0.000000000000000000 ) ) ;
#67784 = CARTESIAN_POINT ( 'NONE',  ( -0.3996062992125985480, -7.340648628747423112E-17, -2.320866141732283783 ) ) ;
#67785 = CARTESIAN_POINT ( 'NONE',  ( 1.594488188976378673, 0.07958543189024085140, 0.2665933059059887866 ) ) ;
#67786 = EDGE_CURVE ( 'NONE', #38903, #28439, #266, .T. ) ;
#67787 = CARTESIAN_POINT ( 'NONE',  ( 0.3460692066303959202, 0.1998031496062993295, -0.6036745406824146620 ) ) ;
#67788 = EDGE_LOOP ( 'NONE', ( #617, #35687, #3992, #64448 ) ) ;
#67789 = CARTESIAN_POINT ( 'NONE',  ( -0.9776902887139098386, 0.1771653543307087075, -0.09757992244046823083 ) ) ;
#67791 = CARTESIAN_POINT ( 'NONE',  ( 0.3917322834645670104, -0.1049643490035303411, -2.150918635170603554 ) ) ;
#67790 = AXIS2_PLACEMENT_3D ( 'NONE', #82161, #30793, #56867 ) ;
#67792 = ORIENTED_EDGE ( 'NONE', *, *, #81099, .F. ) ;
#67793 = CARTESIAN_POINT ( 'NONE',  ( 0.9908136482939640111, 0.2952755905511810774, -0.1292274648535930714 ) ) ;
#67794 = CARTESIAN_POINT ( 'NONE',  ( -0.1902887139107604098, -0.6692913385826771977, 0.1292274648535927661 ) ) ;
#67795 = CARTESIAN_POINT ( 'NONE',  ( -1.240157480314959759, -0.5400638737290845981, -0.3530559997133363437 ) ) ;
#67796 = CARTESIAN_POINT ( 'NONE',  ( 1.154855643044620184, -0.6046776061558807314, 0.2411417322834647770 ) ) ;
#67797 = CARTESIAN_POINT ( 'NONE',  ( -1.312335958005248715, 0.1283753931104748280, 0.1820866141732283561 ) ) ;
#67798 = CARTESIAN_POINT ( 'NONE',  ( 0.08874907683610111508, -2.191421614605370878E-15, 0.4445507791589071167 ) ) ;
#67799 = CARTESIAN_POINT ( 'NONE',  ( 0.3083989501312343062, -0.05778040916215560624, -0.4822834645669293319 ) ) ;
#67800 = CARTESIAN_POINT ( 'NONE',  ( -0.7283464566929126471, -0.5400638737290844871, 0.3530559997133364547 ) ) ;
#67801 = CARTESIAN_POINT ( 'NONE',  ( -0.3917322834645668994, -0.1049643490035306742, -1.385807455871704175 ) ) ;
#67802 = CARTESIAN_POINT ( 'NONE',  ( -1.351706036745406347, -0.4281496062992124485, 0.4176697321401328655 ) ) ;
#67803 = DIRECTION ( 'NONE',  ( -0.000000000000000000, -1.000000000000000000, -0.000000000000000000 ) ) ;
#67804 = CARTESIAN_POINT ( 'NONE',  ( 1.030183727034121421, -0.05778040916215522460, 0.4822834645669289988 ) ) ;
#67805 = CARTESIAN_POINT ( 'NONE',  ( -0.3392501089628017219, -0.1958661417322836718, 0.1128608923884514836 ) ) ;
#67806 = CARTESIAN_POINT ( 'NONE',  ( 1.404199475065617708, -0.004921259842519870586, -0.3153832671262229437 ) ) ;
#67807 = ORIENTED_EDGE ( 'NONE', *, *, #36043, .F. ) ;
#67808 = CARTESIAN_POINT ( 'NONE',  ( -0.3949938075777409963, -7.255918531996591613E-17, 0.1181102362204723977 ) ) ;
#67809 = CARTESIAN_POINT ( 'NONE',  ( -0.4330708661417315697, -0.6692913385826771977, 8.415575281601705876E-17 ) ) ;
#67810 = VERTEX_POINT ( 'NONE', #9493 ) ;
#67811 = CARTESIAN_POINT ( 'NONE',  ( 0.3280839895013130669, -0.004921259842519576551, 0.3153832671262227771 ) ) ;
#67812 = CARTESIAN_POINT ( 'NONE',  ( -1.568241469816272105, -0.05778040916215522460, 0.4822834645669289988 ) ) ;
#67813 = CARTESIAN_POINT ( 'NONE',  ( 0.7742782152230978099, -0.4281496062992124485, 0.4176697321401328655 ) ) ;
#67814 = CARTESIAN_POINT ( 'NONE',  ( 0.8005249343832027131, 0.05413385826771666132, 0.4176697321401328100 ) ) ;
#67815 = CARTESIAN_POINT ( 'NONE',  ( -0.01968503937007793844, -0.5400638737290844871, 0.3530559997133364547 ) ) ;
#67816 = CARTESIAN_POINT ( 'NONE',  ( 0.1958661417322836718, -0.3392501089628017219, -1.348444512632232861 ) ) ;
#67817 = CARTESIAN_POINT ( 'NONE',  ( -0.8398950131233585692, 0.2306618581243848609, 0.2411417322834645549 ) ) ;
#67818 = CARTESIAN_POINT ( 'NONE',  ( 0.1958661417322834775, 0.3392501089628018884, -2.433727034120734878 ) ) ;
#67819 = CARTESIAN_POINT ( 'NONE',  ( -1.692913385826770645, 0.2952755905511811885, 0.000000000000000000 ) ) ;
#67820 = CARTESIAN_POINT ( 'NONE',  ( -0.9186351706036736120, -0.6046776061558809534, -0.2411417322834644161 ) ) ;
#67821 = CARTESIAN_POINT ( 'NONE',  ( 1.456692913385827515, -0.6692913385826771977, 8.415575281601705876E-17 ) ) ;
#67822 = CARTESIAN_POINT ( 'NONE',  ( 1.633858267716535639, -0.5400638737290844871, 0.3530559997133364547 ) ) ;
#67823 = CARTESIAN_POINT ( 'NONE',  ( -0.9776902887139098386, -0.6692913385826771977, 0.1292274648535927661 ) ) ;
#67824 = CARTESIAN_POINT ( 'NONE',  ( 0.1070741851644054776, -0.3996062992125984925, 0.1528871391076115360 ) ) ;
#67825 = CARTESIAN_POINT ( 'NONE',  ( 0.1509186351706042484, -0.3162353388693405765, 0.4822834645669290543 ) ) ;
#67826 = CARTESIAN_POINT ( 'NONE',  ( -0.3460692066303960868, 0.1998031496062990242, -2.388451443569553856 ) ) ;
#67827 = CARTESIAN_POINT ( 'NONE',  ( -0.3937007874015740483, -0.1870078740157479769, 0.4822834645669291653 ) ) ;
#67828 = CARTESIAN_POINT ( 'NONE',  ( -1.437007874015747477, 0.07958543189024071263, -0.2665933059059888421 ) ) ;
#67829 = CARTESIAN_POINT ( 'NONE',  ( 0.5971128608923891301, 0.1771653543307087075, -0.09757992244046823083 ) ) ;
#67830 = CARTESIAN_POINT ( 'NONE',  ( 1.456692913385827515, 0.2952755905511811885, 0.000000000000000000 ) ) ;
#67831 = CARTESIAN_POINT ( 'NONE',  ( 0.4724409448818897572, -0.1265901696524988906, -1.290682414698162583 ) ) ;
#67832 = CARTESIAN_POINT ( 'NONE',  ( 0.6036745406824154392, 0.1283753931104746893, -0.1820866141732285504 ) ) ;
#67833 = CARTESIAN_POINT ( 'NONE',  ( 0.8661417322834652488, -0.1870078740157480879, -0.4822834645669291653 ) ) ;
#67834 = CARTESIAN_POINT ( 'NONE',  ( -0.3420746716998660508, -0.1974969037888706924, -0.7591863517060368771 ) ) ;
#67835 = CARTESIAN_POINT ( 'NONE',  ( -0.5708661417322828946, 0.1660481256975883668, -0.3530559997133364547 ) ) ;
#67836 = CARTESIAN_POINT ( 'NONE',  ( 0.5314960629921373636, 2.755905511811024056, -3.264097702071371288 ) ) ;
#67837 = CARTESIAN_POINT ( 'NONE',  ( 1.456692913385827515, 0.1771653543307087630, 0.000000000000000000 ) ) ;
#67838 = CARTESIAN_POINT ( 'NONE',  ( -0.5183727034120726440, -0.6692913385826773087, -0.1292274648535924053 ) ) ;
#67839 = CARTESIAN_POINT ( 'NONE',  ( -9.674558042662122972E-17, 0.3949938075777409963, -0.5492125984251968740 ) ) ;
#67840 = CARTESIAN_POINT ( 'NONE',  ( 1.227034120734908917, 0.2952755905511810774, -0.1292274648535930714 ) ) ;
#67841 = CARTESIAN_POINT ( 'NONE',  ( 0.1181102362204730916, -0.6692913385826771977, 8.415575281601705876E-17 ) ) ;
#67842 = CARTESIAN_POINT ( 'NONE',  ( 0.3477690288713918276, -0.5511811023622048555, -0.09757992244046775898 ) ) ;
#67843 = CARTESIAN_POINT ( 'NONE',  ( 0.8537221893815273299, 2.409604939980833412E-17, -0.3464511005275205946 ) ) ;
#67844 = CARTESIAN_POINT ( 'NONE',  ( 0.01312335958005323398, -0.3690944881889765550, -0.3153832671262227771 ) ) ;
#67845 = CARTESIAN_POINT ( 'NONE',  ( 0.7677165354330716118, -0.4536011799217367080, 0.2665933059059888421 ) ) ;
#67846 = CARTESIAN_POINT ( 'NONE',  ( -1.587926509186350810, 0.05413385826771626580, -0.4176697321401330321 ) ) ;
#67847 = CARTESIAN_POINT ( 'NONE',  ( 0.2925321140481932369, -0.2925321140481931814, -1.435039370078740495 ) ) ;
#67848 = CARTESIAN_POINT ( 'NONE',  ( 0.7611548556430454138, 0.2306618581243847221, -0.2411417322834647770 ) ) ;
#67849 = CARTESIAN_POINT ( 'NONE',  ( -0.2867679344610365999, 0.2867679344610364889, -1.114173228346456712 ) ) ;
#67850 = CARTESIAN_POINT ( 'NONE',  ( 1.456692913385827515, -0.5511811023622047445, 6.969142054262312111E-17 ) ) ;
#67851 = CARTESIAN_POINT ( 'NONE',  ( -0.09156050430092219083, -0.3808816823641230087, -1.492482962822815952E-17 ) ) ;
#67852 = CARTESIAN_POINT ( 'NONE',  ( 0.2165354330708668673, 0.07958543189024071263, -0.2665933059059888421 ) ) ;
#67853 = AXIS2_PLACEMENT_3D ( 'NONE', #36349, #28375, #22066 ) ;
#67854 = CARTESIAN_POINT ( 'NONE',  ( 0.1771653543307093182, -0.5400638737290845981, -0.3530559997133363437 ) ) ;
#67855 = CARTESIAN_POINT ( 'NONE',  ( 1.305774278215223960, -0.5511811023622046335, 0.09757992244046803654 ) ) ;
#67856 = CARTESIAN_POINT ( 'NONE',  ( -1.318897637795274802, -0.4536011799217368745, -0.2665933059059886201 ) ) ;
#67857 = CARTESIAN_POINT ( 'NONE',  ( -1.286089238845143479, -0.6046776061558807314, 0.2411417322834647770 ) ) ;
#67858 = CARTESIAN_POINT ( 'NONE',  ( 0.1640419947506569498, -0.3162353388693409650, -0.4822834645669289433 ) ) ;
#67859 = CARTESIAN_POINT ( 'NONE',  ( 1.017060367454068803, -0.3162353388693405765, 0.4822834645669290543 ) ) ;
#67860 =( BOUNDED_CURVE ( )  B_SPLINE_CURVE ( 2, ( #76144, #37420, #13412, #44945, #18883, #57167, #70642, #82866, #39067, #12998, #50855, #5834, #64750 ),
 .UNSPECIFIED., .F., .F. ) 
 B_SPLINE_CURVE_WITH_KNOTS ( ( 3, 2, 2, 2, 2, 2, 3 ),
 ( 0.2624999999999999556, 0.2666666666666666075, 0.2708333333333333148, 0.2750000000000000222, 0.2791666666666666741, 0.2833333333333333814, 0.2875000000000000333 ),
 .UNSPECIFIED. ) 
 CURVE ( )  GEOMETRIC_REPRESENTATION_ITEM ( )  RATIONAL_B_SPLINE_CURVE ( ( 1.000000000000000444, 0.9659258262890678681, 1.000000000000000000, 0.9659258262890683122, 1.000000000000000000, 0.9659258262890683122, 1.000000000000000000, 0.9659258262890683122, 1.000000000000000000, 0.9659258262890683122, 1.000000000000000000, 0.9659258262890678681, 1.000000000000000444 ) ) 
 REPRESENTATION_ITEM ( '' )  );
#67861 = CARTESIAN_POINT ( 'NONE',  ( 0.3458507752293908943, 0.3458507752293908943, -0.2145669291338582751 ) ) ;
#67862 = CARTESIAN_POINT ( 'NONE',  ( 0.1706036745406830368, 0.05413385826771666132, 0.4176697321401328100 ) ) ;
#67863 = CARTESIAN_POINT ( 'NONE',  ( 1.108923884514436686, -0.3162353388693409650, -0.4822834645669289433 ) ) ;
#67864 = CARTESIAN_POINT ( 'NONE',  ( 1.056430446194226658, 0.2952755905511811885, 0.1292274648535926551 ) ) ;
#67865 = DIRECTION ( 'NONE',  ( 0.000000000000000000, -1.000000000000000000, 0.000000000000000000 ) ) ;
#67866 = CARTESIAN_POINT ( 'NONE',  ( 0.6102362204724416372, 0.07958543189024071263, -0.2665933059059888421 ) ) ;
#67867 = CARTESIAN_POINT ( 'NONE',  ( 1.555118110236221041, 0.1660481256975883668, -0.3530559997133364547 ) ) ;
#67868 = CARTESIAN_POINT ( 'NONE',  ( 0.2493438320209980519, -0.3690944881889765550, -0.3153832671262227771 ) ) ;
#67869 = CARTESIAN_POINT ( 'NONE',  ( 0.2427821522309719648, -0.05778040916215522460, 0.4822834645669289988 ) ) ;
#67870 = CARTESIAN_POINT ( 'NONE',  ( 0.7217847769028878924, -0.4281496062992127816, -0.4176697321401328100 ) ) ;
#67871 = CARTESIAN_POINT ( 'NONE',  ( -0.3412073490813641308, 0.2306618581243847221, -0.2411417322834647770 ) ) ;
#67872 = CARTESIAN_POINT ( 'NONE',  ( -0.07874015748031421014, -0.1870078740157480601, -0.3641732283464567677 ) ) ;
#67873 = CARTESIAN_POINT ( 'NONE',  ( 0.9317585301837276734, -0.4281496062992124485, 0.4176697321401328655 ) ) ;
#67874 = CARTESIAN_POINT ( 'NONE',  ( 0.8661417322834653598, -0.1870078740157479769, 0.3641732283464567677 ) ) ;
#67875 = EDGE_CURVE ( 'NONE', #60134, #72980, #7998, .T. ) ;
#67876 = CARTESIAN_POINT ( 'NONE',  ( -1.724509498540856889, 1.220656357563485228, 0.3534487381068502909 ) ) ;
#67878 = CARTESIAN_POINT ( 'NONE',  ( 0.1998031496062994405, -0.3460692066303958092, -1.194225721784776928 ) ) ;
#67877 = CARTESIAN_POINT ( 'NONE',  ( -1.036745406824146176, 0.05413385826771626580, -0.4176697321401330321 ) ) ;
#67879 = CARTESIAN_POINT ( 'NONE',  ( 0.000000000000000000, 2.716535433070866645, 0.000000000000000000 ) ) ;
#67880 = CARTESIAN_POINT ( 'NONE',  ( -1.358267716535432434, -0.5400638737290844871, 0.3530559997133364547 ) ) ;
#67881 = CARTESIAN_POINT ( 'NONE',  ( -0.4133858267716528645, 0.1660481256975883668, -0.3530559997133364547 ) ) ;
#67882 = CARTESIAN_POINT ( 'NONE',  ( -0.4724409448818899238, 0.1265901696524986686, -0.03280839895013123314 ) ) ;
#67883 = CARTESIAN_POINT ( 'NONE',  ( -0.3949938075777411628, 0.1058382717557497937, -2.552493438320210473 ) ) ;
#67884 = ORIENTED_EDGE ( 'NONE', *, *, #27570, .T. ) ;
#67885 = CARTESIAN_POINT ( 'NONE',  ( 0.1443569553805781891, -0.004921259842519870586, -0.3153832671262229437 ) ) ;
#67886 = CARTESIAN_POINT ( 'NONE',  ( 0.1049643490035303689, 0.3917322834645670104, -1.087926509186351476 ) ) ;
#67887 = CARTESIAN_POINT ( 'NONE',  ( 0.9580052493438326877, 0.05413385826771666132, 0.4176697321401328100 ) ) ;
#67888 = CARTESIAN_POINT ( 'NONE',  ( -1.157146581871515012E-16, 0.4724409448818898682, -2.362204724409448620 ) ) ;
#67889 =( GEOMETRIC_REPRESENTATION_CONTEXT ( 3 ) GLOBAL_UNCERTAINTY_ASSIGNED_CONTEXT ( ( #64722 ) ) GLOBAL_UNIT_ASSIGNED_CONTEXT ( ( #2298, #45638, #7784 ) ) REPRESENTATION_CONTEXT ( 'NONE', 'WORKASPACE' ) );
#67890 = CARTESIAN_POINT ( 'NONE',  ( 0.4724409448818898682, 2.892866454678787531E-17, -0.8248031496062991907 ) ) ;
#67891 = CARTESIAN_POINT ( 'NONE',  ( -1.174540682414697335, -0.2845877964562161244, -0.3641732283464567121 ) ) ;
#67892 = CARTESIAN_POINT ( 'NONE',  ( 1.679790026246720025, 0.2306618581243848609, 0.2411417322834645549 ) ) ;
#67893 = CARTESIAN_POINT ( 'NONE',  ( 1.522309711286089939, -0.5023911411419708095, -0.1820866141732282451 ) ) ;
#67894 = CARTESIAN_POINT ( 'NONE',  ( 0.5839895013123367340, 0.2952755905511811885, 0.1292274648535926551 ) ) ;
#67895 = CARTESIAN_POINT ( 'NONE',  ( -0.2867679344610366554, 0.2867679344610365444, -0.2571985319871897824 ) ) ;
#67896 = CARTESIAN_POINT ( 'NONE',  ( 0.03937007874015833325, -0.6692913385826771977, 8.415575281601705876E-17 ) ) ;
#67897 = CARTESIAN_POINT ( 'NONE',  ( -1.062992125984250968, 0.1771653543307087630, 0.000000000000000000 ) ) ;
#67898 = CARTESIAN_POINT ( 'NONE',  ( 0.4593175853018379162, -0.4281496062992124485, 0.4176697321401328655 ) ) ;
#67899 = CARTESIAN_POINT ( 'NONE',  ( -0.07874015748031421014, -0.1870078740157480879, -0.4822834645669291653 ) ) ;
#67900 = CARTESIAN_POINT ( 'NONE',  ( 0.5314960629921265944, 0.1660481256975883391, -0.3530559997133364547 ) ) ;
#67901 = CARTESIAN_POINT ( 'NONE',  ( -0.1998031496062991907, -0.3460692066303959757, -2.900262467191600635 ) ) ;
#67902 = CARTESIAN_POINT ( 'NONE',  ( -9.594673741351313045E-17, 0.3917322834645670659, -1.571541625493125149 ) ) ;
#67903 = CARTESIAN_POINT ( 'NONE',  ( 0.7020997375328090762, -0.3162353388693405765, 0.4822834645669290543 ) ) ;
#67904 = CARTESIAN_POINT ( 'NONE',  ( -0.3083989501312330295, -0.05778040916215522460, 0.4822834645669289988 ) ) ;
#67905 = CARTESIAN_POINT ( 'NONE',  ( -1.036745406824146176, -0.4281496062992124485, 0.4176697321401328655 ) ) ;
#67907 = CARTESIAN_POINT ( 'NONE',  ( 1.174540682414699111, -0.05778040916215560624, -0.4822834645669293319 ) ) ;
#67906 = CIRCLE ( 'NONE', #22181, 0.2165354330708659791 ) ;
#67908 = CARTESIAN_POINT ( 'NONE',  ( 0.6430446194225729606, -0.4281496062992127816, -0.4176697321401328100 ) ) ;
#67909 = CARTESIAN_POINT ( 'NONE',  ( 0.1958661417322836440, -0.3392501089628017219, -0.8064304461942258806 ) ) ;
#67910 = CARTESIAN_POINT ( 'NONE',  ( -0.5446194225721777693, -0.3162353388693409650, -0.4822834645669289433 ) ) ;
#67911 = CARTESIAN_POINT ( 'NONE',  ( 0.4002624671916016896, -0.05778040916215522460, 0.4822834645669289988 ) ) ;
#67912 = CARTESIAN_POINT ( 'NONE',  ( -0.3543307086614165824, 0.2952755905511811885, 0.000000000000000000 ) ) ;
#67913 = CARTESIAN_POINT ( 'NONE',  ( 0.8267716535433078384, -0.5511811023622047445, 6.969142054262312111E-17 ) ) ;
#67914 = CARTESIAN_POINT ( 'NONE',  ( 1.666666666666667185, -0.004921259842519576551, 0.3153832671262227771 ) ) ;
#67915 = CARTESIAN_POINT ( 'NONE',  ( -1.732283464566928277, -0.1870078740157479769, 0.4822834645669291653 ) ) ;
#67916 = CARTESIAN_POINT ( 'NONE',  ( 0.3608923884514443348, 0.2952755905511810774, -0.1292274648535930714 ) ) ;
#67917 = CARTESIAN_POINT ( 'NONE',  ( 0.3392501089628018884, -0.1958661417322834220, -2.144356955380577467 ) ) ;
#67918 = ORIENTED_EDGE ( 'NONE', *, *, #7540, .F. ) ;
#67919 = ORIENTED_EDGE ( 'NONE', *, *, #8676, .F. ) ;
#67920 = CARTESIAN_POINT ( 'NONE',  ( 0.5249343832021005074, -0.6046776061558807314, 0.2411417322834647770 ) ) ;
#67921 = CARTESIAN_POINT ( 'NONE',  ( 0.6496062992125991586, 0.07958543189024085140, 0.2665933059059887866 ) ) ;
#67923 = CARTESIAN_POINT ( 'NONE',  ( 0.000000000000000000, 0.000000000000000000, 6.062992125984251857 ) ) ;
#67922 = DIRECTION ( 'NONE',  ( 0.000000000000000000, 0.000000000000000000, -1.000000000000000000 ) ) ;
#67924 = CARTESIAN_POINT ( 'NONE',  ( -0.1049643490035307020, 0.3917322834645669549, -0.8786089238845143923 ) ) ;
#67925 = CARTESIAN_POINT ( 'NONE',  ( -0.03443470937339728616, 0.000000000000000000, -1.537015892239756099 ) ) ;
#67926 = CARTESIAN_POINT ( 'NONE',  ( 0.3996062992125984925, 0.1070741851644054637, -2.248687664041994605 ) ) ;
#67927 = CARTESIAN_POINT ( 'NONE',  ( 0.9842519685039375910, 0.2952755905511811885, 0.000000000000000000 ) ) ;
#67928 = CARTESIAN_POINT ( 'NONE',  ( -0.9251968503937002541, -0.5400638737290845981, -0.3530559997133363437 ) ) ;
#67929 = CARTESIAN_POINT ( 'NONE',  ( -0.7020997375328076329, -0.3162353388693409650, -0.4822834645669289433 ) ) ;
#67930 = CARTESIAN_POINT ( 'NONE',  ( 0.5052493438320215802, 0.2952755905511811885, 0.1292274648535926551 ) ) ;
#67931 = CARTESIAN_POINT ( 'NONE',  ( 1.568241469816273437, -0.3162353388693405765, 0.4822834645669290543 ) ) ;
#67932 = CARTESIAN_POINT ( 'NONE',  ( -1.168682819302786058, -2.294479370626195693E-15, 0.3464511005275217603 ) ) ;
#67933 = SHAPE_DEFINITION_REPRESENTATION ( #15100, #82043 ) ;
#67934 = CARTESIAN_POINT ( 'NONE',  ( 1.332020997375329197, -0.2845877964562159024, 0.3641732283464567677 ) ) ;
#67935 = PLANE ( 'NONE',  #74793 ) ;
#67936 = CARTESIAN_POINT ( 'NONE',  ( -1.181102362204723644, -0.1870078740157479769, 0.3641732283464567677 ) ) ;
#67937 = CARTESIAN_POINT ( 'NONE',  ( -0.2867679344610365999, 0.2867679344610364889, -0.01181102362204719709 ) ) ;
#67938 = CARTESIAN_POINT ( 'NONE',  ( 0.09842519685039434474, 0.1660481256975885056, 0.3530559997133364547 ) ) ;
#67940 = CARTESIAN_POINT ( 'NONE',  ( 0.000000000000000000, 2.185078740157480937, 0.4527559055118110520 ) ) ;
#67939 = CARTESIAN_POINT ( 'NONE',  ( 1.253280839895013710, -0.05778040916215560624, -0.4822834645669293319 ) ) ;
#67941 = CARTESIAN_POINT ( 'NONE',  ( -1.279527559055116948, -0.4536011799217367080, 0.2665933059059888421 ) ) ;
#67942 = CARTESIAN_POINT ( 'NONE',  ( 0.4265091863517067594, 0.2952755905511811885, 0.1292274648535926551 ) ) ;
#67943 = CARTESIAN_POINT ( 'NONE',  ( 1.338582677165355062, -0.1870078740157480601, -0.3641732283464567677 ) ) ;
#67944 = CARTESIAN_POINT ( 'NONE',  ( -9.594673741351310580E-17, 0.3917322834645669549, -1.654836327262780182 ) ) ;
#67945 = CARTESIAN_POINT ( 'NONE',  ( -1.036745406824146176, -0.004921259842519870586, -0.3153832671262229437 ) ) ;
#67946 = CARTESIAN_POINT ( 'NONE',  ( 1.496062992125985147, -0.1870078740157479769, 0.4822834645669291653 ) ) ;
#67947 = CARTESIAN_POINT ( 'NONE',  ( 2.554262525012263474, 1.546132656481029155, -0.4744094488188972392 ) ) ;
#67948 = CARTESIAN_POINT ( 'NONE',  ( -0.3805774278215216522, -0.4281496062992127816, -0.4176697321401328100 ) ) ;
#67949 = CARTESIAN_POINT ( 'NONE',  ( -1.469816272965878357, 0.1283753931104748280, 0.1820866141732283561 ) ) ;
#67950 = CARTESIAN_POINT ( 'NONE',  ( -0.7808398950131225646, -0.05778040916215522460, 0.4822834645669289988 ) ) ;
#67951 = CARTESIAN_POINT ( 'NONE',  ( -1.509186351706035767, -0.3690944881889763329, 0.3153832671262228327 ) ) ;
#67952 = CARTESIAN_POINT ( 'NONE',  ( 4.797336870675656522E-17, -0.3917322834645670659, -0.3904392632884007841 ) ) ;
#67953 = CARTESIAN_POINT ( 'NONE',  ( 0.4986876640419954376, 0.2306618581243848609, 0.2411417322834645549 ) ) ;
#67954 = LINE ( 'NONE', #34411, #18475 ) ;
#67955 = CARTESIAN_POINT ( 'NONE',  ( 1.384514435695538337, -0.6692913385826771977, 0.1292274648535927661 ) ) ;
#67956 = CARTESIAN_POINT ( 'NONE',  ( -0.4091458600556405756, 0.2362204724409446288, -2.150262467191601079 ) ) ;
#67957 = AXIS2_PLACEMENT_3D ( 'NONE', #82541, #50120, #70310 ) ;
#67958 = CARTESIAN_POINT ( 'NONE',  ( -1.332020997375327642, -0.3162353388693409650, -0.4822834645669289433 ) ) ;
#67959 = CARTESIAN_POINT ( 'NONE',  ( -1.108923884514435132, -0.08942795157528024563, -0.3641732283464568787 ) ) ;
#67960 = CARTESIAN_POINT ( 'NONE',  ( -0.5314960629921254842, -0.4536011799217368745, -0.2665933059059886201 ) ) ;
#67961 = CARTESIAN_POINT ( 'NONE',  ( -0.5384083780239481420, 0.004960608223778821026, 0.3437734562760189072 ) ) ;
#67962 = CARTESIAN_POINT ( 'NONE',  ( 0.2362204724409456558, -0.1870078740157479769, 0.4822834645669291653 ) ) ;
#67963 = CARTESIAN_POINT ( 'NONE',  ( 0.4002624671916016896, -0.08942795157527998196, 0.3641732283464567121 ) ) ;
#67964 = CARTESIAN_POINT ( 'NONE',  ( -0.9842519685039365918, -0.5511811023622047445, 6.969142054262312111E-17 ) ) ;
#67965 = CARTESIAN_POINT ( 'NONE',  ( -1.437007874015747477, -0.5400638737290844871, 0.3530559997133364547 ) ) ;
#67966 = CARTESIAN_POINT ( 'NONE',  ( 1.541994750656168645, -0.5511811023622046335, 0.09757992244046803654 ) ) ;
#67967 = CARTESIAN_POINT ( 'NONE',  ( 1.377952755905512472, 0.2952755905511811885, 0.000000000000000000 ) ) ;
#67968 = CARTESIAN_POINT ( 'NONE',  ( 0.2100141437675508982, 1.111707297776196812, 1.895198704147436741 ) ) ;
#67969 = CARTESIAN_POINT ( 'NONE',  ( 0.3018372703412079971, -0.004921259842519870586, -0.3153832671262229437 ) ) ;
#67970 = CARTESIAN_POINT ( 'NONE',  ( 0.9842519685039378130, -0.6692913385826771977, 8.415575281601705876E-17 ) ) ;
#67971 = CARTESIAN_POINT ( 'NONE',  ( -1.604771003085130543, 0.7270283685441724097, 0.1466069496707740338 ) ) ;
#67972 = CARTESIAN_POINT ( 'NONE',  ( 1.017060367454068581, -0.08942795157528024563, -0.3641732283464568787 ) ) ;
#67973 = ORIENTED_EDGE ( 'NONE', *, *, #5358, .T. ) ;
#67974 = CARTESIAN_POINT ( 'NONE',  ( -1.286089238845143479, 0.2306618581243847221, -0.2411417322834647770 ) ) ;
#67975 = EDGE_CURVE ( 'NONE', #80562, #43140, #1470, .T. ) ;
#67976 = CARTESIAN_POINT ( 'NONE',  ( -0.7874015748031489847, -0.1870078740157480879, -0.4822834645669291653 ) ) ;
#67977 = CARTESIAN_POINT ( 'NONE',  ( 0.04593175853018440641, 0.2952755905511810774, -0.1292274648535930714 ) ) ;
#67978 = CARTESIAN_POINT ( 'NONE',  ( -2.112655059233905508, 1.697151583350147153, -0.4469586986359067593 ) ) ;
#67979 = CARTESIAN_POINT ( 'NONE',  ( -0.2925321140481932369, 0.2925321140481931259, -2.301181102362204633 ) ) ;
#67980 = CARTESIAN_POINT ( 'NONE',  ( 1.049868766404200127, -0.6046776061558809534, -0.2411417322834644161 ) ) ;
#67981 = CARTESIAN_POINT ( 'NONE',  ( -1.725721784776902190, -0.05778040916215522460, 0.4822834645669289988 ) ) ;
#67982 = CARTESIAN_POINT ( 'NONE',  ( -0.01968503937007793844, 0.1660481256975883668, -0.3530559997133364547 ) ) ;
#67983 = CARTESIAN_POINT ( 'NONE',  ( 0.7480314960629927956, -0.6692913385826771977, 8.415575281601705876E-17 ) ) ;
#67984 = CARTESIAN_POINT ( 'NONE',  ( -0.3996062992125986035, -7.340648628747425578E-17, -1.929133858267716439 ) ) ;
#67985 = CARTESIAN_POINT ( 'NONE',  ( -0.3420746716998661618, 0.1974969037888702206, -1.286089238845144367 ) ) ;
#67986 = CARTESIAN_POINT ( 'NONE',  ( 0.1998031496062992740, 0.3460692066303959757, -2.349081364829396446 ) ) ;
#67987 = CARTESIAN_POINT ( 'NONE',  ( -0.3458507752293909498, 0.3458507752293908388, -0.6496062992125984925 ) ) ;
#67988 = CARTESIAN_POINT ( 'NONE',  ( -0.1049643490035301885, -0.3917322834645671215, -0.2217847769028870319 ) ) ;
#67989 = CARTESIAN_POINT ( 'NONE',  ( -0.2559055118110230564, 0.07958543189024071263, -0.2665933059059888421 ) ) ;
#67990 = CARTESIAN_POINT ( 'NONE',  ( -0.7939632545931754048, -0.3162353388693405765, 0.4822834645669290543 ) ) ;
#67991 = CARTESIAN_POINT ( 'NONE',  ( 0.6758530183727039509, 0.2952755905511810774, -0.1292274648535930714 ) ) ;
#67992 = CARTESIAN_POINT ( 'NONE',  ( 0.3949938075777409408, -0.1058382717557499186, -2.235564304461942431 ) ) ;
#67993 = CARTESIAN_POINT ( 'NONE',  ( -0.3412073490813641308, 0.1283753931104746893, -0.1820866141732285504 ) ) ;
#67994 = CARTESIAN_POINT ( 'NONE',  ( 1.614173228346457378, 0.2952755905511811885, 0.000000000000000000 ) ) ;
#67995 = CARTESIAN_POINT ( 'NONE',  ( 1.076115485564305141, -0.6046776061558807314, 0.2411417322834647770 ) ) ;
#67996 = CARTESIAN_POINT ( 'NONE',  ( -0.4091458600556402980, -0.2362204724409451284, -2.257217847769029007 ) ) ;
#67997 = CARTESIAN_POINT ( 'NONE',  ( 0.1998031496062992740, 0.3460692066303959757, -1.719160104986876769 ) ) ;
#67998 = FACE_OUTER_BOUND ( 'NONE', #63650, .T. ) ;
#67999 = CIRCLE ( 'NONE', #18366, 3.307086614173228689 ) ;
#68000 = ORIENTED_EDGE ( 'NONE', *, *, #17343, .T. ) ;
#68001 = CARTESIAN_POINT ( 'NONE',  ( 1.148293963254593653, 0.2952755905511810774, -0.1292274648535930714 ) ) ;
#68002 = CARTESIAN_POINT ( 'NONE',  ( 1.141732283464567566, 0.1771653543307087630, 0.000000000000000000 ) ) ;
#68004 = CARTESIAN_POINT ( 'NONE',  ( -1.417322834645668772, -0.1870078740157480879, -0.4822834645669291653 ) ) ;
#68003 = CARTESIAN_POINT ( 'NONE',  ( -1.430446194225720724, -0.004921259842519870586, -0.3153832671262229437 ) ) ;
#68005 = CARTESIAN_POINT ( 'NONE',  ( 0.3392501089628018329, 0.1958661417322835607, 0.09908136482939623735 ) ) ;
#68006 = CARTESIAN_POINT ( 'NONE',  ( -0.9776902887139098386, 0.2066929133858267098, -0.1054918080437494132 ) ) ;
#68007 = CARTESIAN_POINT ( 'NONE',  ( 1.108923884514436686, -0.3162353388693409650, -0.4822834645669289433 ) ) ;
#68008 = CARTESIAN_POINT ( 'NONE',  ( -1.587926509186350810, -0.4281496062992124485, 0.4176697321401328655 ) ) ;
#68009 = CARTESIAN_POINT ( 'NONE',  ( -0.5052493438320203589, -0.6692913385826771977, 0.1292274648535927661 ) ) ;
#68010 = CARTESIAN_POINT ( 'NONE',  ( -0.4265091863517051496, 0.2952755905511810774, -0.1292274648535930714 ) ) ;
#68011 = EDGE_CURVE ( 'NONE', #30111, #72870, #32607, .T. ) ;
#68012 = CARTESIAN_POINT ( 'NONE',  ( 1.535433070866142335, -0.6692913385826771977, 8.415575281601705876E-17 ) ) ;
#68013 = CARTESIAN_POINT ( 'NONE',  ( 0.1049643490035303689, 0.3917322834645670104, -0.07808398950131241467 ) ) ;
#68014 = CARTESIAN_POINT ( 'NONE',  ( 0.1968503937007881344, 0.2952755905511811885, 0.000000000000000000 ) ) ;
#68015 = CARTESIAN_POINT ( 'NONE',  ( 0.2867679344610365999, -0.2867679344610365444, -2.452755905511811108 ) ) ;
#68016 = CARTESIAN_POINT ( 'NONE',  ( -1.574803149606298192, -0.1870078740157480601, -0.3641732283464567677 ) ) ;
#68017 = ORIENTED_EDGE ( 'NONE', *, *, #7858, .T. ) ;
#68018 = CARTESIAN_POINT ( 'NONE',  ( 0.3420746716998660508, -0.1974969037888703871, -2.782152230971128848 ) ) ;
#68019 = ORIENTED_EDGE ( 'NONE', *, *, #80061, .T. ) ;
#68020 = CARTESIAN_POINT ( 'NONE',  ( -0.05905511811023543556, 0.1012011053420777407, 0.2882089793578256898 ) ) ;
#68021 = AXIS2_PLACEMENT_3D ( 'NONE', #71738, #59101, #14513 ) ;
#68022 = CARTESIAN_POINT ( 'NONE',  ( -1.404199475065615932, 0.05413385826771666132, 0.4176697321401328100 ) ) ;
#68023 = CARTESIAN_POINT ( 'NONE',  ( -0.2925321140481930704, -0.2925321140481933480, -0.8464566929133857665 ) ) ;
#68024 = CARTESIAN_POINT ( 'NONE',  ( -0.4744094488188832504, 1.537401574803149984, -3.937007874015763687 ) ) ;
#68025 = FACE_OUTER_BOUND ( 'NONE', #64663, .T. ) ;
#68026 = CARTESIAN_POINT ( 'NONE',  ( 4.893765752498283924E-17, -0.3996062992125986035, -2.755905511811023612 ) ) ;
#68027 = CARTESIAN_POINT ( 'NONE',  ( -0.1049643490035302024, -0.3917322834645671215, -0.6292650918635172008 ) ) ;
#68028 = CARTESIAN_POINT ( 'NONE',  ( -0.1246719160104980823, -0.5511811023622048555, -0.09757992244046775898 ) ) ;
#68029 = CARTESIAN_POINT ( 'NONE',  ( -1.128608923884513837, -0.5023911411419708095, 0.1820866141732285504 ) ) ;
#68030 = CARTESIAN_POINT ( 'NONE',  ( -1.509186351706035767, -0.4281496062992124485, 0.4176697321401328655 ) ) ;
#68031 = CARTESIAN_POINT ( 'NONE',  ( 0.3346456692913390985, 0.1660481256975885056, 0.3530559997133364547 ) ) ;
#68032 = CARTESIAN_POINT ( 'NONE',  ( -1.489501312335957062, -0.05778040916215522460, 0.4822834645669289988 ) ) ;
#68033 = CARTESIAN_POINT ( 'NONE',  ( -0.3392501089628017219, -0.1958661417322836718, -0.2020997375328083545 ) ) ;
#68034 = ORIENTED_EDGE ( 'NONE', *, *, #52780, .T. ) ;
#68035 = CARTESIAN_POINT ( 'NONE',  ( -1.450131233595799651, 0.2952755905511810774, -0.1292274648535930714 ) ) ;
#68036 = DIRECTION ( 'NONE',  ( 0.000000000000000000, 1.000000000000000000, 0.000000000000000000 ) ) ;
#68037 = SHAPE_REPRESENTATION_RELATIONSHIP ( 'NONE' , 'NONE' ,  #27201, #53490 ) ;
#68038 = CARTESIAN_POINT ( 'NONE',  ( 0.4724409448818898682, 2.892866454678787531E-17, -1.692913385826771533 ) ) ;
#68039 = CARTESIAN_POINT ( 'NONE',  ( 0.1321325610835860920, 0.2642592750917004407, 0.1571896754257856577 ) ) ;
#68040 = ADVANCED_FACE ( 'NONE', ( #52741 ), #66228, .F. ) ;
#68041 = CARTESIAN_POINT ( 'NONE',  ( 3.833048050305355326E-17, 1.954428616053095924, 0.3129921259842520787 ) ) ;
#68042 = CARTESIAN_POINT ( 'NONE',  ( -0.6692913385826764205, 0.2952755905511811885, 0.000000000000000000 ) ) ;
#68043 = CARTESIAN_POINT ( 'NONE',  ( 1.522309711286089939, 0.2306618581243848609, 0.2411417322834645549 ) ) ;
#68045 = DIRECTION ( 'NONE',  ( 0.000000000000000000, 0.000000000000000000, -1.000000000000000000 ) ) ;
#68044 = CARTESIAN_POINT ( 'NONE',  ( -1.568241469816272105, -0.05778040916215522460, 0.4822834645669289988 ) ) ;
#68046 = CARTESIAN_POINT ( 'NONE',  ( -1.660104986876639543, -0.05778040916215560624, -0.4822834645669293319 ) ) ;
#68047 = CARTESIAN_POINT ( 'NONE',  ( -0.7086614173228339419, -0.1870078740157480879, -0.4822834645669291653 ) ) ;
#68048 = CARTESIAN_POINT ( 'NONE',  ( -9.594673741351310580E-17, 0.3917322834645669549, -0.08003317765648111648 ) ) ;
#68049 = CARTESIAN_POINT ( 'NONE',  ( 0.2296587926509192634, -0.08942795157528024563, -0.3641732283464568787 ) ) ;
#68050 = CARTESIAN_POINT ( 'NONE',  ( 0.3392501089628018329, 0.1958661417322835607, -0.5308398950131234528 ) ) ;
#68051 = CARTESIAN_POINT ( 'NONE',  ( -0.01312335958005186876, -0.004921259842519870586, -0.3153832671262229437 ) ) ;
#68052 = CARTESIAN_POINT ( 'NONE',  ( 0.7677165354330716118, -0.4536011799217367080, 0.2665933059059888421 ) ) ;
#68053 = CARTESIAN_POINT ( 'NONE',  ( 0.4790026246719167324, -0.05778040916215522460, 0.4822834645669289988 ) ) ;
#68054 = CARTESIAN_POINT ( 'NONE',  ( -0.2427821522309703550, -0.2845877964562159024, 0.3641732283464567677 ) ) ;
#68055 = CARTESIAN_POINT ( 'NONE',  ( 0.1049643490035303689, 0.3917322834645670104, -2.505249343832020248 ) ) ;
#68056 = CARTESIAN_POINT ( 'NONE',  ( 1.594488188976378673, 0.1660481256975885056, 0.3530559997133364547 ) ) ;
#68057 = AXIS2_PLACEMENT_3D ( 'NONE', #40185, #22069, #26720 ) ;
#68058 = CARTESIAN_POINT ( 'NONE',  ( -1.003937007874014853, 0.1660481256975885056, 0.3530559997133364547 ) ) ;
#68059 = VECTOR ( 'NONE', #80309, 39.37007874015748143 ) ;
#68060 = CARTESIAN_POINT ( 'NONE',  ( -1.157146581871515012E-16, 0.4724409448818898682, -0.8641732283464567121 ) ) ;
#68061 = VECTOR ( 'NONE', #77822, 39.37007874015748143 ) ;
#68062 = CARTESIAN_POINT ( 'NONE',  ( 0.2296587926509192634, -0.05778040916215560624, -0.4822834645669293319 ) ) ;
#68063 = CARTESIAN_POINT ( 'NONE',  ( -0.5774278215223089816, -0.6046776061558807314, 0.2411417322834647770 ) ) ;
#68064 = FACE_OUTER_BOUND ( 'NONE', #54856, .T. ) ;
#68065 = CARTESIAN_POINT ( 'NONE',  ( 0.02624671916010564918, 0.1283753931104748280, 0.1820866141732283561 ) ) ;
#68066 = CARTESIAN_POINT ( 'NONE',  ( -0.2493438320209966919, 0.05413385826771626580, -0.4176697321401330321 ) ) ;
#68067 = CARTESIAN_POINT ( 'NONE',  ( -0.5708661417322825615, -0.5400638737290844871, 0.3530559997133364547 ) ) ;
#68068 = FACE_OUTER_BOUND ( 'NONE', #61287, .T. ) ;
#68069 = CARTESIAN_POINT ( 'NONE',  ( 1.574803149606299746, -0.1870078740157480601, -0.3641732283464567677 ) ) ;
#68070 = CARTESIAN_POINT ( 'NONE',  ( 0.2690288713910767848, 0.2952755905511811885, 0.1292274648535926551 ) ) ;
#68071 = CARTESIAN_POINT ( 'NONE',  ( -0.2925321140481930149, -0.2925321140481933480, -2.183070866141731958 ) ) ;
#68072 = CARTESIAN_POINT ( 'NONE',  ( 1.522309711286089939, -0.6046776061558809534, -0.2411417322834644161 ) ) ;
#68073 = CARTESIAN_POINT ( 'NONE',  ( -0.8005249343832013809, -0.3690944881889763329, 0.3153832671262228327 ) ) ;
#68074 = VECTOR ( 'NONE', #17623, 39.37007874015748143 ) ;
#68075 = CARTESIAN_POINT ( 'NONE',  ( -0.6955380577427815458, -0.4281496062992127816, -0.4176697321401328100 ) ) ;
#68076 = CARTESIAN_POINT ( 'NONE',  ( 1.345144356955381593, -0.05778040916215522460, 0.4822834645669289988 ) ) ;
#68077 = CARTESIAN_POINT ( 'NONE',  ( 1.233595800524935227, 0.2306618581243847221, -0.2411417322834647770 ) ) ;
#68078 = DIRECTION ( 'NONE',  ( -1.000000000000000000, -0.000000000000000000, -0.000000000000000000 ) ) ;
#68079 = CARTESIAN_POINT ( 'NONE',  ( -1.010498687664041384, -0.3690944881889765550, -0.3153832671262227771 ) ) ;
#68080 = CARTESIAN_POINT ( 'NONE',  ( -0.3996062992125985480, -7.340648628747423112E-17, -0.1161417322834645965 ) ) ;
#68081 = CARTESIAN_POINT ( 'NONE',  ( -0.3996062992125987146, 0.1070741851644051862, -0.3477690288713909950 ) ) ;
#68082 = CARTESIAN_POINT ( 'NONE',  ( -0.1049643490035302301, -0.3917322834645671770, -2.903562622868453680 ) ) ;
#68083 = CARTESIAN_POINT ( 'NONE',  ( -0.7480314960629922405, 2.001539355558159983, 0.000000000000000000 ) ) ;
#68084 = CARTESIAN_POINT ( 'NONE',  ( 1.062992125984252745, -0.5511811023622047445, 6.969142054262312111E-17 ) ) ;
#68085 = CARTESIAN_POINT ( 'NONE',  ( 0.8727034120734912248, -0.3162353388693409650, -0.4822834645669289433 ) ) ;
#68086 = CARTESIAN_POINT ( 'NONE',  ( -1.640419947506561060, -0.4281496062992127816, -0.4176697321401328100 ) ) ;
#68087 = CARTESIAN_POINT ( 'NONE',  ( 0.8661417322834652488, -0.1870078740157480879, -0.4822834645669291653 ) ) ;
#68088 = CARTESIAN_POINT ( 'NONE',  ( 0.3420746716998660508, -0.1974969037888704149, -0.8116797900262466836 ) ) ;
#68089 = CARTESIAN_POINT ( 'NONE',  ( 1.220472440944882608, 0.1771653543307087630, 0.000000000000000000 ) ) ;
#68090 = CARTESIAN_POINT ( 'NONE',  ( 0.2296587926509192634, -0.3162353388693405765, 0.4822834645669290543 ) ) ;
#68091 = CARTESIAN_POINT ( 'NONE',  ( -0.9514435695538050464, -0.05778040916215560624, -0.4822834645669293319 ) ) ;
#68092 = CARTESIAN_POINT ( 'NONE',  ( 1.292650918635171564, -0.6692913385826773087, -0.1292274648535924053 ) ) ;
#68093 = CARTESIAN_POINT ( 'NONE',  ( -0.4724409448818898682, -8.678599364036362592E-17, -1.141732283464566899 ) ) ;
#68094 = CARTESIAN_POINT ( 'NONE',  ( 0.3996062992125986035, -0.1070741851644053111, -2.473753280839894764 ) ) ;
#68095 = CARTESIAN_POINT ( 'NONE',  ( 0.4593175853018379162, -0.3690944881889763329, 0.3153832671262228327 ) ) ;
#68096 = ORIENTED_EDGE ( 'NONE', *, *, #37207, .T. ) ;
#68097 = CARTESIAN_POINT ( 'NONE',  ( 0.1958661417322834775, 0.3392501089628018884, -0.9284970060705530770 ) ) ;
#68098 = VERTEX_POINT ( 'NONE', #33817 ) ;
#68099 = CARTESIAN_POINT ( 'NONE',  ( -0.6758530183727028406, -0.6692913385826773087, -0.1292274648535924053 ) ) ;
#68100 = CARTESIAN_POINT ( 'NONE',  ( -0.2034120734908128059, 0.2952755905511811885, 0.1292274648535926551 ) ) ;
#68101 = CARTESIAN_POINT ( 'NONE',  ( -0.5052493438320203589, 0.2952755905511810774, -0.1292274648535930714 ) ) ;
#68102 = CARTESIAN_POINT ( 'NONE',  ( 0.9251968503937015864, 0.1660481256975883668, -0.3530559997133364547 ) ) ;
#68103 = CARTESIAN_POINT ( 'NONE',  ( -1.292650918635170010, 0.2952755905511810774, -0.1292274648535930714 ) ) ;
#68104 = CARTESIAN_POINT ( 'NONE',  ( -0.3674540682414692561, -0.6046776061558809534, -0.2411417322834644161 ) ) ;
#68105 = CARTESIAN_POINT ( 'NONE',  ( 1.338582677165355062, -0.1870078740157480879, -0.4822834645669291653 ) ) ;
#68106 = CARTESIAN_POINT ( 'NONE',  ( 0.4724409448818904789, -0.1870078740157479769, 0.4822834645669291653 ) ) ;
#68107 = CARTESIAN_POINT ( 'NONE',  ( 0.6167979002624679463, 0.05413385826771626580, -0.4176697321401330321 ) ) ;
#68108 = CARTESIAN_POINT ( 'NONE',  ( -0.3917322834645671215, 0.1049643490035301469, -1.127296587926509108 ) ) ;
#68109 = CARTESIAN_POINT ( 'NONE',  ( -0.6036745406824141069, -0.5023911411419708095, -0.1820866141732282451 ) ) ;
#68110 = ORIENTED_EDGE ( 'NONE', *, *, #54370, .T. ) ;
#68111 = CARTESIAN_POINT ( 'NONE',  ( -0.1058382717557497937, -0.3949938075777411628, -1.332020997375328086 ) ) ;
#68112 = CIRCLE ( 'NONE', #17057, 0.5118110236220472231 ) ;
#68113 = ORIENTED_EDGE ( 'NONE', *, *, #68170, .F. ) ;
#68114 = CARTESIAN_POINT ( 'NONE',  ( -0.9120734908136475250, 0.1771653543307087630, 0.09757992244046791164 ) ) ;
#68115 = AXIS2_PLACEMENT_3D ( 'NONE', #55409, #81115, #76841 ) ;
#68116 = AXIS2_PLACEMENT_3D ( 'NONE', #13634, #9291, #34962 ) ;
#68117 = CARTESIAN_POINT ( 'NONE',  ( -0.2755905511811015396, -0.6692913385826771977, 8.415575281601705876E-17 ) ) ;
#68118 = CARTESIAN_POINT ( 'NONE',  ( -0.3996062992125986035, -0.1070741851644056997, 0.1115485564304461580 ) ) ;
#68119 = CARTESIAN_POINT ( 'NONE',  ( -0.6036745406824141069, 0.2306618581243848609, 0.2411417322834645549 ) ) ;
#68120 = CARTESIAN_POINT ( 'NONE',  ( -1.043307086614172707, 0.1660481256975883668, -0.3530559997133364547 ) ) ;
#68121 = CARTESIAN_POINT ( 'NONE',  ( -1.377952755905511140, -0.6692913385826771977, 8.415575281601705876E-17 ) ) ;
#68122 = CARTESIAN_POINT ( 'NONE',  ( -1.450131233595799651, -0.6692913385826771977, 0.1292274648535927661 ) ) ;
#68123 = CARTESIAN_POINT ( 'NONE',  ( 0.7414698162729663755, 0.1771653543307087630, 0.09757992244046791164 ) ) ;
#68124 = LINE ( 'NONE', #29393, #72659 ) ;
#68125 = CARTESIAN_POINT ( 'NONE',  ( 0.1406185367545949583, 0.2755905511811023723, -1.409564117849439802 ) ) ;
#68126 = CARTESIAN_POINT ( 'NONE',  ( 0.2427821522309716595, -0.2845877964562161244, -0.3641732283464567121 ) ) ;
#68127 = CARTESIAN_POINT ( 'NONE',  ( 0.01968503937007957949, -0.5400638737290845981, -0.3530559997133363437 ) ) ;
#68128 = CARTESIAN_POINT ( 'NONE',  ( -0.2493438320209966919, -0.4281496062992124485, 0.4176697321401328655 ) ) ;
#68129 = VERTEX_POINT ( 'NONE', #80117 ) ;
#68130 = CARTESIAN_POINT ( 'NONE',  ( 0.1070741851644054915, -0.3996062992125986035, -1.660104986876640210 ) ) ;
#68131 = CARTESIAN_POINT ( 'NONE',  ( 0.3503937007874015630, 0.3733313776025731778, -1.512162153811850596 ) ) ;
#68132 = EDGE_LOOP ( 'NONE', ( #43990, #35699, #40021, #72589 ) ) ;
#68133 = CARTESIAN_POINT ( 'NONE',  ( -0.3996062992125985480, -7.340648628747423112E-17, -1.218503937007874072 ) ) ;
#68134 = CARTESIAN_POINT ( 'NONE',  ( 1.548556430446194954, -0.6046776061558807314, 0.2411417322834647770 ) ) ;
#68135 = CARTESIAN_POINT ( 'NONE',  ( -0.6036745406824141069, 0.1283753931104748280, 0.1820866141732283561 ) ) ;
#68136 = CARTESIAN_POINT ( 'NONE',  ( -1.102362204724408601, -0.1870078740157479769, 0.4822834645669291653 ) ) ;
#68137 = CARTESIAN_POINT ( 'NONE',  ( -0.2362204724409451284, 0.4091458600556402425, -0.4855643044619422644 ) ) ;
#68138 = DIRECTION ( 'NONE',  ( -1.000000000000000000, -0.000000000000000000, -0.000000000000000000 ) ) ;
#68139 = CARTESIAN_POINT ( 'NONE',  ( 0.3917322834645670104, -0.1049643490035303411, -2.558398950131233196 ) ) ;
#68140 = CARTESIAN_POINT ( 'NONE',  ( 1.692913385826772421, 0.2952755905511811885, 0.000000000000000000 ) ) ;
#68141 = CARTESIAN_POINT ( 'NONE',  ( 0.3674540682414705883, 0.2306618581243847221, -0.2411417322834647770 ) ) ;
#68142 = CARTESIAN_POINT ( 'NONE',  ( 0.6102362204724416372, 0.1660481256975883668, -0.3530559997133364547 ) ) ;
#68143 = CARTESIAN_POINT ( 'NONE',  ( -0.6233595800524928121, -0.2845877964562161244, -0.3641732283464567121 ) ) ;
#68144 = CARTESIAN_POINT ( 'NONE',  ( -0.09186351706036689768, 0.05413385826771626580, -0.4176697321401330321 ) ) ;
#68145 = CARTESIAN_POINT ( 'NONE',  ( -0.4724409448818898682, -8.678599364036362592E-17, -2.320866141732283783 ) ) ;
#68146 = EDGE_CURVE ( 'NONE', #36842, #77755, #74822, .T. ) ;
#68147 = CARTESIAN_POINT ( 'NONE',  ( -0.6430446194225716283, -0.4281496062992124485, 0.4176697321401328655 ) ) ;
#68148 = CARTESIAN_POINT ( 'NONE',  ( 0.1974969037888704704, 0.3420746716998660508, -1.953412073490814027 ) ) ;
#68149 = CARTESIAN_POINT ( 'NONE',  ( 1.187664041994751285, -0.2845877964562161244, -0.3641732283464567121 ) ) ;
#68150 = CARTESIAN_POINT ( 'NONE',  ( 0.06561679790026316017, -0.004921259842519870586, -0.3153832671262229437 ) ) ;
#68151 = CARTESIAN_POINT ( 'NONE',  ( 1.292650918635171564, -0.5511811023622048555, -0.09757992244046775898 ) ) ;
#68152 = CARTESIAN_POINT ( 'NONE',  ( -1.279527559055116948, -0.5400638737290844871, 0.3530559997133364547 ) ) ;
#68153 = CARTESIAN_POINT ( 'NONE',  ( -1.082677165354329896, -0.4536011799217368745, -0.2665933059059886201 ) ) ;
#68154 = DIRECTION ( 'NONE',  ( -1.000000000000000000, 0.000000000000000000, 1.692413147294446216E-16 ) ) ;
#68155 = CARTESIAN_POINT ( 'NONE',  ( -0.9908136482939626788, -0.6692913385826773087, -0.1292274648535924053 ) ) ;
#68156 = CARTESIAN_POINT ( 'NONE',  ( -0.2755905511811015396, -0.6692913385826771977, 8.415575281601705876E-17 ) ) ;
#68157 = CARTESIAN_POINT ( 'NONE',  ( 0.4527559055118117182, 0.1660481256975883668, -0.3530559997133364547 ) ) ;
#68158 = CARTESIAN_POINT ( 'NONE',  ( -0.1958661417322836440, 0.3392501089628016664, -2.612841576606612204 ) ) ;
#68159 = CARTESIAN_POINT ( 'NONE',  ( 1.091663011964304930, -3.876714527516387216E-16, -0.4118477457932991359 ) ) ;
#68160 = CARTESIAN_POINT ( 'NONE',  ( 0.1377952755905518800, 0.07958543189024071263, -0.2665933059059888421 ) ) ;
#68161 = CARTESIAN_POINT ( 'NONE',  ( -1.515748031496062076, 0.07958543189024071263, -0.2665933059059888421 ) ) ;
#68162 = EDGE_CURVE ( 'NONE', #22548, #36796, #3080, .T. ) ;
#68163 = CARTESIAN_POINT ( 'NONE',  ( 0.7939632545931766261, -0.3162353388693409650, -0.4822834645669289433 ) ) ;
#68164 = CARTESIAN_POINT ( 'NONE',  ( 0.000000000000000000, 0.000000000000000000, 0.000000000000000000 ) ) ;
#68165 = CARTESIAN_POINT ( 'NONE',  ( 1.312335958005249825, 0.1283753931104746893, -0.1820866141732285504 ) ) ;
#68166 = CARTESIAN_POINT ( 'NONE',  ( -0.7874015748031489847, -0.1870078740157479769, 0.4822834645669291653 ) ) ;
#68167 = CARTESIAN_POINT ( 'NONE',  ( -0.07874015748031421014, -0.1870078740157479769, 0.3641732283464567677 ) ) ;
#68168 = CARTESIAN_POINT ( 'NONE',  ( 0.000000000000000000, 1.724409448818897461, 0.000000000000000000 ) ) ;
#68169 = CARTESIAN_POINT ( 'NONE',  ( 0.7939632545931766261, -0.08942795157527998196, 0.3641732283464567121 ) ) ;
#68170 = EDGE_CURVE ( 'NONE', #78980, #69205, #15302, .T. ) ;
#68171 = AXIS2_PLACEMENT_3D ( 'NONE', #66646, #80531, #72540 ) ;
#68172 = CARTESIAN_POINT ( 'NONE',  ( -0.2230971128608915943, 0.05413385826771666132, 0.4176697321401328100 ) ) ;
#68173 = CARTESIAN_POINT ( 'NONE',  ( 0.3996062992125985480, 2.446882876249141654E-17, -0.8248031496062991907 ) ) ;
#68174 = VECTOR ( 'NONE', #68154, 39.37007874015748143 ) ;
#68175 = CARTESIAN_POINT ( 'NONE',  ( 0.2867679344610365999, -0.2867679344610365444, -1.757874015748031260 ) ) ;
#68176 = CARTESIAN_POINT ( 'NONE',  ( 0.8398950131233602345, 0.1283753931104746893, -0.1820866141732285504 ) ) ;
#68178 = MECHANICAL_DESIGN_GEOMETRIC_PRESENTATION_REPRESENTATION (  '', ( #2325 ), #33200 ) ;
#68177 = CARTESIAN_POINT ( 'NONE',  ( 0.02624671916010564918, -0.6046776061558809534, -0.2411417322834644161 ) ) ;
#68179 = VECTOR ( 'NONE', #16649, 39.37007874015748143 ) ;
#68180 = CARTESIAN_POINT ( 'NONE',  ( -0.4855643044619415427, 0.05413385826771626580, -0.4176697321401330321 ) ) ;
#68181 = CARTESIAN_POINT ( 'NONE',  ( -0.5971128608923877978, -0.5511811023622048555, -0.09757992244046775898 ) ) ;
#68182 = CARTESIAN_POINT ( 'NONE',  ( 0.9580052493438326877, 0.009842519685039463617, 0.3409548833797002576 ) ) ;
#68183 = CARTESIAN_POINT ( 'NONE',  ( -0.5774278215223089816, -0.5023911411419708095, 0.1820866141732285504 ) ) ;
#68184 = CARTESIAN_POINT ( 'NONE',  ( 0.5249343832021005074, -0.6046776061558807314, 0.2411417322834647770 ) ) ;
#68185 = CARTESIAN_POINT ( 'NONE',  ( -1.003937007874015297, -0.4536011799217368745, -0.2665933059059886201 ) ) ;
#68186 = CARTESIAN_POINT ( 'NONE',  ( 0.1070741851644053388, 0.3996062992125986035, -1.487532808398950301 ) ) ;
#68187 = CARTESIAN_POINT ( 'NONE',  ( -1.397637795275589623, -0.5400638737290845981, -0.3530559997133363437 ) ) ;
#68188 = DIRECTION ( 'NONE',  ( 0.000000000000000000, -1.734723475976808327E-16, -1.000000000000000000 ) ) ;
#68189 = ORIENTED_EDGE ( 'NONE', *, *, #67875, .F. ) ;
#68190 = CARTESIAN_POINT ( 'NONE',  ( -1.423884514435694859, -0.2845877964562159024, 0.3641732283464567677 ) ) ;
#68191 = CARTESIAN_POINT ( 'NONE',  ( -0.4790026246719154557, -0.3162353388693405765, 0.4822834645669290543 ) ) ;
#68192 = EDGE_CURVE ( 'NONE', #70928, #66145, #44104, .T. ) ;
#68193 = CARTESIAN_POINT ( 'NONE',  ( -1.069553805774277722, -0.6692913385826773087, -0.1292274648535924053 ) ) ;
#68194 = CARTESIAN_POINT ( 'NONE',  ( -0.2867679344610364334, -0.2867679344610367109, -1.403543307086614123 ) ) ;
#68195 = DIRECTION ( 'NONE',  ( 0.000000000000000000, 0.000000000000000000, 1.000000000000000000 ) ) ;
#68196 = CARTESIAN_POINT ( 'NONE',  ( 1.384514435695538559, 0.2952755905511810774, -0.1292274648535930714 ) ) ;
#68197 = CARTESIAN_POINT ( 'NONE',  ( 0.4527559055118117182, 0.1660481256975883668, -0.3530559997133364547 ) ) ;
#68198 = CARTESIAN_POINT ( 'NONE',  ( 0.000000000000000000, 0.000000000000000000, 0.000000000000000000 ) ) ;
#68199 = CARTESIAN_POINT ( 'NONE',  ( 0.3996062992125985480, -0.1070741851644052972, -2.550524934383202158 ) ) ;
#68200 = CARTESIAN_POINT ( 'NONE',  ( 1.502624671916010790, -0.2845877964562161244, -0.3641732283464567121 ) ) ;
#68201 = CARTESIAN_POINT ( 'NONE',  ( 0.1070741851644054915, -0.3996062992125986035, -0.7152230971128609172 ) ) ;
#68203 = EDGE_CURVE ( 'NONE', #24205, #35380, #21191, .T. ) ;
#68202 = ORIENTED_EDGE ( 'NONE', *, *, #63295, .T. ) ;
#68204 = CARTESIAN_POINT ( 'NONE',  ( -0.7480314960629914633, -0.5511811023622047445, 6.969142054262312111E-17 ) ) ;
#68205 = CARTESIAN_POINT ( 'NONE',  ( 0.3392501089628018884, -0.1958661417322834220, -2.774278215223096922 ) ) ;
#68206 = ORIENTED_EDGE ( 'NONE', *, *, #4912, .F. ) ;
#68207 = CARTESIAN_POINT ( 'NONE',  ( 1.017060367454068581, -0.05778040916215560624, -0.4822834645669293319 ) ) ;
#68208 = CARTESIAN_POINT ( 'NONE',  ( -0.4068241469816267775, 0.05413385826771626580, -0.4176697321401330321 ) ) ;
#68209 = CARTESIAN_POINT ( 'NONE',  ( -1.056430446194224881, -0.6692913385826771977, 0.1292274648535927661 ) ) ;
#68210 = CARTESIAN_POINT ( 'NONE',  ( 1.003937007874016407, -0.5400638737290844871, 0.3530559997133364547 ) ) ;
#68211 = CARTESIAN_POINT ( 'NONE',  ( -1.194225721784776262, -0.3690944881889763329, 0.3153832671262228327 ) ) ;
#68212 = CARTESIAN_POINT ( 'NONE',  ( 0.000000000000000000, 0.000000000000000000, 6.062992125984251857 ) ) ;
#68213 = CARTESIAN_POINT ( 'NONE',  ( 0.1509186351706045259, -0.05778040916215560624, -0.4822834645669293319 ) ) ;
#68214 = CARTESIAN_POINT ( 'NONE',  ( -0.9514435695538050464, -0.05778040916215560624, -0.4822834645669293319 ) ) ;
#68215 = B_SPLINE_CURVE_WITH_KNOTS ( 'NONE', 3,
 ( #67094, #32279, #33542, #1565, #26385, #39856, #47710, #71009, #73408, #78169, #52880, #27219 ),
 .UNSPECIFIED., .F., .F.,
 ( 4, 2, 2, 2, 2, 4 ),
 ( 0.05454303362711801495, 0.05585633982237168255, 0.05651299291999852675, 0.05716964601762537096, 0.05848295221287905937, 0.05979625840813274779 ),
 .UNSPECIFIED. ) ;
#68216 = CARTESIAN_POINT ( 'NONE',  ( 0.1049643490035304522, -0.3917322834645668994, -1.740138164533121756 ) ) ;
#68217 = CARTESIAN_POINT ( 'NONE',  ( 1.535433070866142335, -0.6692913385826771977, 8.415575281601705876E-17 ) ) ;
#68218 = CARTESIAN_POINT ( 'NONE',  ( 0.000000000000000000, 2.755905511811024056, 0.000000000000000000 ) ) ;
#68219 = EDGE_CURVE ( 'NONE', #51179, #51564, #73794, .T. ) ;
#68220 = CARTESIAN_POINT ( 'NONE',  ( 0.8858267716535438430, 0.1660481256975885056, 0.3530559997133364547 ) ) ;
#68221 = CARTESIAN_POINT ( 'NONE',  ( 0.3917322834645670104, 2.398668435337828261E-17, -2.879921259842519454 ) ) ;
#68222 = CARTESIAN_POINT ( 'NONE',  ( 0.9908136482939640111, -0.5511811023622046335, 0.09757992244046803654 ) ) ;
#68223 = ORIENTED_EDGE ( 'NONE', *, *, #70912, .T. ) ;
#68224 = CARTESIAN_POINT ( 'NONE',  ( 4.797336870675656522E-17, -0.3917322834645670659, -2.752643987697849237 ) ) ;
#68225 = CARTESIAN_POINT ( 'NONE',  ( -0.3149606299212590610, -0.1870078740157480879, -0.4822834645669291653 ) ) ;
#68226 = ORIENTED_EDGE ( 'NONE', *, *, #64961, .T. ) ;
#68227 = CARTESIAN_POINT ( 'NONE',  ( 0.4855643044619428750, -0.004921259842519576551, 0.3153832671262227771 ) ) ;
#68228 = CARTESIAN_POINT ( 'NONE',  ( -1.706036745406823485, 0.2306618581243848609, 0.2411417322834645549 ) ) ;
#68229 = CARTESIAN_POINT ( 'NONE',  ( 0.5971128608923890191, -0.6692913385826771977, 0.1292274648535927661 ) ) ;
#68230 = CARTESIAN_POINT ( 'NONE',  ( 0.3215223097112867578, -0.05778040916215522460, 0.4822834645669289988 ) ) ;
#68231 = CARTESIAN_POINT ( 'NONE',  ( -0.06561679790026180015, -0.4281496062992127816, -0.4176697321401328100 ) ) ;
#68232 = CARTESIAN_POINT ( 'NONE',  ( 0.1049643490035303967, 0.3917322834645670659, -1.250019315781839113 ) ) ;
#68233 = CARTESIAN_POINT ( 'NONE',  ( -0.9580052493438311334, 0.05413385826771626580, -0.4176697321401330321 ) ) ;
#68234 = CARTESIAN_POINT ( 'NONE',  ( -0.1049643490035302024, -0.3917322834645671215, -2.046587926509185973 ) ) ;
#68235 = CARTESIAN_POINT ( 'NONE',  ( 1.581364829396326277, -0.08942795157527998196, 0.3641732283464567121 ) ) ;
#68236 = CARTESIAN_POINT ( 'NONE',  ( -1.141732283464566011, 0.2952755905511811885, 0.000000000000000000 ) ) ;
#68237 = CARTESIAN_POINT ( 'NONE',  ( 1.371391076115485941, 0.2952755905511811885, 0.1292274648535926551 ) ) ;
#68238 = CARTESIAN_POINT ( 'NONE',  ( 1.358267716535433323, 0.1660481256975885056, 0.3530559997133364547 ) ) ;
#68239 = CARTESIAN_POINT ( 'NONE',  ( 0.1070741851644053527, 0.3996062992125986590, -0.6233595800524933672 ) ) ;
#68240 = CARTESIAN_POINT ( 'NONE',  ( -0.8070866141732276899, -0.5400638737290844871, 0.3530559997133364547 ) ) ;
#68241 = DIRECTION ( 'NONE',  ( 0.000000000000000000, 0.000000000000000000, -1.000000000000000000 ) ) ;
#68242 = CARTESIAN_POINT ( 'NONE',  ( 0.09842519685039434474, -0.5400638737290845981, -0.3530559997133363437 ) ) ;
#68243 = CARTESIAN_POINT ( 'NONE',  ( 0.3996062992125986590, -0.1070741851644053111, -2.158792650918635037 ) ) ;
#68244 = CARTESIAN_POINT ( 'NONE',  ( -0.6036745406824141069, -0.6046776061558809534, -0.2411417322834644161 ) ) ;
#68245 = CIRCLE ( 'NONE', #57444, 0.2952755905511810774 ) ;
#68246 = CARTESIAN_POINT ( 'NONE',  ( 1.686351706036745890, 0.2952755905511811885, 0.1292274648535926551 ) ) ;
#68247 = CARTESIAN_POINT ( 'NONE',  ( 0.7152230971128616943, -0.08942795157527998196, 0.3641732283464567121 ) ) ;
#68248 = CARTESIAN_POINT ( 'NONE',  ( 1.345144356955381593, -0.3162353388693409650, -0.4822834645669289433 ) ) ;
#68249 = CARTESIAN_POINT ( 'NONE',  ( 0.1265901696524990294, -0.4724409448818896462, -1.106955380577427706 ) ) ;
#68250 = CARTESIAN_POINT ( 'NONE',  ( 0.5643044619422579178, -0.004921259842519576551, 0.3153832671262227771 ) ) ;
#68251 = CARTESIAN_POINT ( 'NONE',  ( 0.9973753280839902091, 0.2306618581243847221, -0.2411417322834647770 ) ) ;
#68252 = CARTESIAN_POINT ( 'NONE',  ( 0.1058382717557499880, 0.3949938075777409408, -0.5426509186351705649 ) ) ;
#68253 = CARTESIAN_POINT ( 'NONE',  ( -0.5905511811023615998, 0.2952755905511811885, 0.000000000000000000 ) ) ;
#68254 = CARTESIAN_POINT ( 'NONE',  ( 2.556891438210028067, 2.729656593086051242, 0.5314960629921260393 ) ) ;
#68255 = CARTESIAN_POINT ( 'NONE',  ( 1.148293963254593653, 0.1771653543307087075, -0.09757992244046823083 ) ) ;
#68256 = CARTESIAN_POINT ( 'NONE',  ( -0.7020997375328076329, -0.3162353388693409650, -0.4822834645669289433 ) ) ;
#68257 = CARTESIAN_POINT ( 'NONE',  ( 0.2034120734908142214, 0.2952755905511810774, -0.1292274648535930714 ) ) ;
#68258 = CARTESIAN_POINT ( 'NONE',  ( 0.1312335958005257930, 0.1539470093639521697, -0.1968503937007875793 ) ) ;
#68259 = CARTESIAN_POINT ( 'NONE',  ( 0.2362204724409456558, -0.1870078740157480879, -0.4822834645669291653 ) ) ;
#68260 = CARTESIAN_POINT ( 'NONE',  ( -0.01312335958005186876, -0.004921259842519870586, -0.3153832671262229437 ) ) ;
#68261 = CARTESIAN_POINT ( 'NONE',  ( -2.585397804484597550, 1.422882880004781914, 0.4606469518571247312 ) ) ;
#68262 = CARTESIAN_POINT ( 'NONE',  ( 0.06561679790026316017, -0.3690944881889763329, 0.3153832671262228327 ) ) ;
#68263 = CARTESIAN_POINT ( 'NONE',  ( 0.6167979002624678353, -0.3690944881889763329, 0.3153832671262228327 ) ) ;
#68264 = CARTESIAN_POINT ( 'NONE',  ( 1.443709154632419265E-16, 0.4177165354330708569, 1.178877988035069047 ) ) ;
#68265 = CARTESIAN_POINT ( 'NONE',  ( -0.1998031496062991630, -0.3460692066303959202, -1.559711286089239035 ) ) ;
#68266 = CARTESIAN_POINT ( 'NONE',  ( 0.3149606299212606708, -0.1870078740157480879, -0.4822834645669291653 ) ) ;
#68267 = CARTESIAN_POINT ( 'NONE',  ( 0.3392501089628018329, 0.1958661417322835607, -0.9107611548556429071 ) ) ;
#68268 = CARTESIAN_POINT ( 'NONE',  ( 0.000000000000000000, 2.410722045565656378E-17, -0.1968503937007874405 ) ) ;
#68269 = CARTESIAN_POINT ( 'NONE',  ( 0.09032602383071736130, 0.02791078216816225699, 0.4328096321851905293 ) ) ;
#68270 = CARTESIAN_POINT ( 'NONE',  ( -0.4986876640419942164, -0.5023911411419708095, 0.1820866141732285504 ) ) ;
#68271 = EDGE_CURVE ( 'NONE', #9475, #76877, #2249, .T. ) ;
#68272 = CARTESIAN_POINT ( 'NONE',  ( 0.2493438320209980519, 0.05413385826771666132, 0.4176697321401328100 ) ) ;
#68273 = CARTESIAN_POINT ( 'NONE',  ( 0.9842519685039378130, -0.5511811023622047445, 6.969142054262312111E-17 ) ) ;
#68274 = CARTESIAN_POINT ( 'NONE',  ( -1.489501312335957062, -0.2845877964562161244, -0.3641732283464567121 ) ) ;
#68275 = CARTESIAN_POINT ( 'NONE',  ( -1.607611548556429737, -0.6692913385826771977, 0.1292274648535927661 ) ) ;
#68276 = CARTESIAN_POINT ( 'NONE',  ( 0.1509186351706045259, -0.05778040916215560624, -0.4822834645669293319 ) ) ;
#68277 = CARTESIAN_POINT ( 'NONE',  ( 1.259842519685040019, -0.1870078740157480879, -0.4822834645669291653 ) ) ;
#68278 = CARTESIAN_POINT ( 'NONE',  ( 1.614173228346457378, 0.7794589730112001513, -0.1372047244094476148 ) ) ;
#68279 = CARTESIAN_POINT ( 'NONE',  ( 0.2296587926509192634, -0.05778040916215560624, -0.4822834645669293319 ) ) ;
#68280 = CARTESIAN_POINT ( 'NONE',  ( 1.509186351706037543, 0.05413385826771666132, 0.4176697321401328100 ) ) ;
#68281 = CARTESIAN_POINT ( 'NONE',  ( 1.161417322834646493, -0.5400638737290844871, 0.3530559997133364547 ) ) ;
#68282 = DIRECTION ( 'NONE',  ( 1.000000000000000000, 0.000000000000000000, 0.000000000000000000 ) ) ;
#68283 = CARTESIAN_POINT ( 'NONE',  ( 0.7742782152230979209, -0.004921259842519870586, -0.3153832671262229437 ) ) ;
#68284 = CARTESIAN_POINT ( 'NONE',  ( 1.437007874015748810, -0.5400638737290845981, -0.3530559997133363437 ) ) ;
#68285 = CARTESIAN_POINT ( 'NONE',  ( -0.1049868766404193215, 0.1283753931104746893, -0.1820866141732285504 ) ) ;
#68286 = CARTESIAN_POINT ( 'NONE',  ( -0.1443569553805765515, -0.4281496062992127816, -0.4176697321401328100 ) ) ;
#68287 = CARTESIAN_POINT ( 'NONE',  ( 0.8792650918635177559, -0.4281496062992127816, -0.4176697321401328100 ) ) ;
#68288 = CARTESIAN_POINT ( 'NONE',  ( -0.5446194225721777693, -0.05778040916215522460, 0.4822834645669289988 ) ) ;
#68289 = CARTESIAN_POINT ( 'NONE',  ( -0.3917322834645671770, 0.1049643490035302024, -2.076790969325146730 ) ) ;
#68290 = CARTESIAN_POINT ( 'NONE',  ( -0.3477690288713905509, -0.5511811023622046335, 0.09757992244046803654 ) ) ;
#68291 = CARTESIAN_POINT ( 'NONE',  ( 0.9645669291338588858, 0.1660481256975885056, 0.3530559997133364547 ) ) ;
#68292 = CARTESIAN_POINT ( 'NONE',  ( 0.8005249343832028242, -0.3690944881889765550, -0.3153832671262227771 ) ) ;
#68293 = CARTESIAN_POINT ( 'NONE',  ( -1.735579908797700410, 1.274882798674454421, 0.3961561098831279382 ) ) ;
#68295 = CARTESIAN_POINT ( 'NONE',  ( 1.614173228346457378, 0.2952755905511811885, 0.000000000000000000 ) ) ;
#68294 = FACE_OUTER_BOUND ( 'NONE', #10543, .T. ) ;
#68296 = DIRECTION ( 'NONE',  ( 0.000000000000000000, 0.000000000000000000, -1.000000000000000000 ) ) ;
#68297 = CIRCLE ( 'NONE', #19861, 3.307086614173228689 ) ;
#68298 = CARTESIAN_POINT ( 'NONE',  ( -1.305774278215222184, 0.2952755905511811885, 0.1292274648535926551 ) ) ;
#68299 = CARTESIAN_POINT ( 'NONE',  ( -0.3740157480314953431, -0.5400638737290845981, -0.3530559997133363437 ) ) ;
#68300 = CARTESIAN_POINT ( 'NONE',  ( -0.3996062992125986035, -0.1070741851644056997, -2.880577427821522374 ) ) ;
#68301 = CARTESIAN_POINT ( 'NONE',  ( 0.3949938075777409408, 0.1058382717557500574, -2.801837270341207553 ) ) ;
#68302 = ORIENTED_EDGE ( 'NONE', *, *, #61363, .F. ) ;
#68303 = CARTESIAN_POINT ( 'NONE',  ( 0.4068241469816281097, -0.004921259842519576551, 0.3153832671262227771 ) ) ;
#68304 = CARTESIAN_POINT ( 'NONE',  ( -0.1958661417322836718, 0.3392501089628017219, -1.580052493438320216 ) ) ;
#68305 = CARTESIAN_POINT ( 'NONE',  ( 1.102362204724410155, -0.1870078740157479769, 0.4822834645669291653 ) ) ;
#68306 = CARTESIAN_POINT ( 'NONE',  ( -0.4724409448818895907, -0.1265901696524993070, -2.565616797900262647 ) ) ;
#68307 = SURFACE_STYLE_USAGE ( .BOTH. , #16967 ) ;
#68308 = CARTESIAN_POINT ( 'NONE',  ( 0.000000000000000000, 1.062992125984252745, 1.122047244094488194 ) ) ;
#68309 = CARTESIAN_POINT ( 'NONE',  ( 1.246719160104987623, -0.3690944881889763329, 0.3153832671262228327 ) ) ;
#68310 = CARTESIAN_POINT ( 'NONE',  ( 0.4658792650918641698, -0.05778040916215560624, -0.4822834645669293319 ) ) ;
#68311 = CARTESIAN_POINT ( 'NONE',  ( 4.797336870675655290E-17, -0.3917322834645669549, -0.4737339650580559280 ) ) ;
#68312 = CARTESIAN_POINT ( 'NONE',  ( -0.03280839895013062252, 0.2952755905511810774, -0.1292274648535930714 ) ) ;
#68313 = CARTESIAN_POINT ( 'NONE',  ( -0.8792650918635160906, -0.004921259842519870586, -0.3153832671262229437 ) ) ;
#68314 = CARTESIAN_POINT ( 'NONE',  ( 0.3018372703412079971, -0.4281496062992124485, 0.4176697321401328655 ) ) ;
#68315 = CARTESIAN_POINT ( 'NONE',  ( 0.1443569553805781891, -0.4281496062992124485, 0.4176697321401328655 ) ) ;
#68316 = DIRECTION ( 'NONE',  ( 0.000000000000000000, 1.000000000000000000, 0.000000000000000000 ) ) ;
#68317 = CARTESIAN_POINT ( 'NONE',  ( -0.3996062992125986035, -0.1070741851644056997, -2.880577427821522374 ) ) ;
#68318 = CARTESIAN_POINT ( 'NONE',  ( -0.1958661417322836995, 0.3392501089628017219, -1.427184670112547682 ) ) ;
#68319 = CARTESIAN_POINT ( 'NONE',  ( 0.6692913385826778638, -0.6692913385826771977, 8.415575281601705876E-17 ) ) ;
#68320 = CARTESIAN_POINT ( 'NONE',  ( -0.2427821522309703550, -0.05778040916215560624, -0.4822834645669293319 ) ) ;
#68321 = CARTESIAN_POINT ( 'NONE',  ( -1.266404199475064773, -0.05778040916215560624, -0.4822834645669293319 ) ) ;
#68322 = CARTESIAN_POINT ( 'NONE',  ( 0.9580052493438326877, 0.05413385826771666132, 0.4176697321401328100 ) ) ;
#68323 = CARTESIAN_POINT ( 'NONE',  ( 0.6364829396325465405, -0.3162353388693409650, -0.4822834645669289433 ) ) ;
#68324 = CARTESIAN_POINT ( 'NONE',  ( -0.3392501089628017219, -0.1958661417322836718, -0.7670603674540683592 ) ) ;
#68325 = CARTESIAN_POINT ( 'NONE',  ( -0.1574803149606292529, -0.1870078740157479769, 0.4822834645669291653 ) ) ;
#68326 = CARTESIAN_POINT ( 'NONE',  ( 0.1181102362204730916, 0.2952755905511811885, 0.000000000000000000 ) ) ;
#68327 = CARTESIAN_POINT ( 'NONE',  ( -0.4068241469816264999, -0.4281496062992124485, 0.4176697321401328655 ) ) ;
#68328 = CARTESIAN_POINT ( 'NONE',  ( 0.2887139107611556010, 0.1283753931104746893, -0.1820866141732285504 ) ) ;
#68329 = CARTESIAN_POINT ( 'NONE',  ( 1.686351706036745890, 0.1771653543307087630, 0.09757992244046791164 ) ) ;
#68330 = CARTESIAN_POINT ( 'NONE',  ( -0.5314960629921122726, 2.755905511811024056, -3.937007874015763687 ) ) ;
#68331 = CARTESIAN_POINT ( 'NONE',  ( 0.4461942257217855201, -0.6046776061558807314, 0.2411417322834647770 ) ) ;
#68332 = CARTESIAN_POINT ( 'NONE',  ( 1.568241469816273437, -0.3162353388693405765, 0.4822834645669290543 ) ) ;
#68333 = CARTESIAN_POINT ( 'NONE',  ( 0.2867679344610365999, 0.2867679344610365999, -2.177165354330708347 ) ) ;
#68334 = EDGE_LOOP ( 'NONE', ( #15071, #44159, #50148, #52015 ) ) ;
#68335 = ORIENTED_EDGE ( 'NONE', *, *, #56918, .F. ) ;
#68336 = CARTESIAN_POINT ( 'NONE',  ( 0.7020997375328090762, -0.3162353388693405765, 0.4822834645669290543 ) ) ;
#68337 = CARTESIAN_POINT ( 'NONE',  ( 0.2690288713910767848, -0.5511811023622048555, -0.09757992244046775898 ) ) ;
#68339 = CYLINDRICAL_SURFACE ( 'NONE', #73365, 0.4724409448818898682 ) ;
#68338 = FACE_OUTER_BOUND ( 'NONE', #13781, .T. ) ;
#68340 = CARTESIAN_POINT ( 'NONE',  ( 0.1049643490035304938, -0.3917322834645669549, -0.9573490813648293241 ) ) ;
#68341 = DIRECTION ( 'NONE',  ( 0.8050726085550550248, 2.493067783899190563E-16, -0.5931762764595016613 ) ) ;
#68342 = CARTESIAN_POINT ( 'NONE',  ( 0.3046215029598646207, 2.057429365980579055E-15, -0.4281989832122139461 ) ) ;
#68343 = CARTESIAN_POINT ( 'NONE',  ( 4.893765752498283308E-17, -0.3996062992125985480, -2.360236220472441193 ) ) ;
#68344 = CARTESIAN_POINT ( 'NONE',  ( 0.4527559055118117182, -0.5400638737290844871, 0.3530559997133364547 ) ) ;
#68345 = CARTESIAN_POINT ( 'NONE',  ( -0.8661417322834640276, -0.1870078740157479769, 0.4822834645669291653 ) ) ;
#68346 = CARTESIAN_POINT ( 'NONE',  ( -0.8661417322834640276, -0.1870078740157480879, -0.4822834645669291653 ) ) ;
#68347 = CARTESIAN_POINT ( 'NONE',  ( 0.6102362204724416372, -0.5400638737290844871, 0.3530559997133364547 ) ) ;
#68348 = CARTESIAN_POINT ( 'NONE',  ( 1.502624671916010790, -0.3162353388693409650, -0.4822834645669289433 ) ) ;
#68349 = CARTESIAN_POINT ( 'NONE',  ( 1.601049868766404982, -0.5023911411419708095, -0.1820866141732282451 ) ) ;
#68350 = PRODUCT_CONTEXT ( 'NONE', #65425, 'mechanical' ) ;
#68351 = CARTESIAN_POINT ( 'NONE',  ( 1.305774278215223960, -0.5511811023622046335, 0.09757992244046803654 ) ) ;
#68352 = CARTESIAN_POINT ( 'NONE',  ( -0.8661417322834640276, -0.1870078740157479769, 0.4822834645669291653 ) ) ;
#68353 = CARTESIAN_POINT ( 'NONE',  ( 1.555118110236221041, 0.1660481256975883668, -0.3530559997133364547 ) ) ;
#68354 =( BOUNDED_CURVE ( )  B_SPLINE_CURVE ( 1, ( #24990, #43109 ),
 .UNSPECIFIED., .F., .F. ) 
 B_SPLINE_CURVE_WITH_KNOTS ( ( 2, 2 ),
 ( 3.469446951953614189E-18, 0.002000000000000006981 ),
 .UNSPECIFIED. ) 
 CURVE ( )  GEOMETRIC_REPRESENTATION_ITEM ( )  RATIONAL_B_SPLINE_CURVE ( ( 0.9875488213027523443, 0.9875488213027523443 ) ) 
 REPRESENTATION_ITEM ( '' )  );
#68355 = PLANE ( 'NONE',  #40927 ) ;
#68356 = CARTESIAN_POINT ( 'NONE',  ( 0.1771653543307093182, -0.5400638737290845981, -0.3530559997133363437 ) ) ;
#68358 = CARTESIAN_POINT ( 'NONE',  ( -1.614173228346457378, 1.543375672658094944, 0.1372047244094476981 ) ) ;
#68357 = CARTESIAN_POINT ( 'NONE',  ( 1.003937007874016407, -0.5400638737290844871, 0.3530559997133364547 ) ) ;
#68359 = CARTESIAN_POINT ( 'NONE',  ( -1.371391076115484831, 0.1771653543307087075, -0.09757992244046823083 ) ) ;
#68360 = CARTESIAN_POINT ( 'NONE',  ( 0.1837270341207357105, -0.6046776061558809534, -0.2411417322834644161 ) ) ;
#68361 = CARTESIAN_POINT ( 'NONE',  ( 1.128608923884514947, 0.1283753931104748280, 0.1820866141732283561 ) ) ;
#68362 = EDGE_CURVE ( 'NONE', #47808, #60445, #5481, .T. ) ;
#68363 = CARTESIAN_POINT ( 'NONE',  ( 0.1958661417322836162, -0.3392501089628018329, -1.746699844323147843 ) ) ;
#68364 = CARTESIAN_POINT ( 'NONE',  ( -1.030183727034119867, -0.08942795157528024563, -0.3641732283464568787 ) ) ;
#68365 = CARTESIAN_POINT ( 'NONE',  ( 1.384514435695538559, 0.2952755905511810774, -0.1292274648535930714 ) ) ;
#68366 = CARTESIAN_POINT ( 'NONE',  ( 0.4177787735907000366, 0.3937007874015748254, -1.559171609364239375 ) ) ;
#68367 = CARTESIAN_POINT ( 'NONE',  ( -0.2624671916010490880, 0.1283753931104746893, -0.1820866141732285504 ) ) ;
#68368 = CARTESIAN_POINT ( 'NONE',  ( -0.2034120734908131112, -0.6692913385826773087, -0.1292274648535924053 ) ) ;
#68369 = CARTESIAN_POINT ( 'NONE',  ( -1.148293963254592542, 0.1771653543307087630, 0.09757992244046791164 ) ) ;
#68370 = CARTESIAN_POINT ( 'NONE',  ( -0.6430446194225716283, -0.4281496062992124485, 0.4176697321401328655 ) ) ;
#68371 = CARTESIAN_POINT ( 'NONE',  ( 1.430446194225722500, -0.4281496062992127816, -0.4176697321401328100 ) ) ;
#68372 = CARTESIAN_POINT ( 'NONE',  ( -0.3917322834645671770, 0.1049643490035302024, -0.3445075047582172312 ) ) ;
#68373 = CARTESIAN_POINT ( 'NONE',  ( 0.4493346515394942009, 1.385193209801244940, -1.573425852207795961 ) ) ;
#68374 = CARTESIAN_POINT ( 'NONE',  ( 1.305774278215223960, 0.2952755905511810774, -0.1292274648535930714 ) ) ;
#68375 = CARTESIAN_POINT ( 'NONE',  ( -0.4724409448818895907, -0.1265901696524993070, -1.854986876640420057 ) ) ;
#68376 = CARTESIAN_POINT ( 'NONE',  ( -1.010498687664041384, -0.4281496062992127816, -0.4176697321401328100 ) ) ;
#68377 = CARTESIAN_POINT ( 'NONE',  ( -1.128608923884513837, 0.1283753931104746893, -0.1820866141732285504 ) ) ;
#68378 = CARTESIAN_POINT ( 'NONE',  ( -0.5052493438320203589, -0.5511811023622046335, 0.09757992244046803654 ) ) ;
#68379 = CARTESIAN_POINT ( 'NONE',  ( -0.5387615594602663815, -2.294479370626195693E-15, 0.3464511005275217603 ) ) ;
#68380 = CARTESIAN_POINT ( 'NONE',  ( 0.01312335958005323398, -0.4281496062992127816, -0.4176697321401328100 ) ) ;
#68381 = CARTESIAN_POINT ( 'NONE',  ( -0.1443569553805765515, -0.3690944881889765550, -0.3153832671262227771 ) ) ;
#68382 = CARTESIAN_POINT ( 'NONE',  ( -1.122047244094487306, -0.4536011799217367080, 0.2665933059059888421 ) ) ;
#68383 = CARTESIAN_POINT ( 'NONE',  ( -1.686351706036744558, 0.2952755905511810774, -0.1292274648535930714 ) ) ;
#68384 = CARTESIAN_POINT ( 'NONE',  ( 1.496062992125984703, -0.1870078740157480601, -0.3641732283464567677 ) ) ;
#68385 = CARTESIAN_POINT ( 'NONE',  ( 0.8923884514435703741, 0.2306618581243848609, 0.2411417322834645549 ) ) ;
#68386 = CARTESIAN_POINT ( 'NONE',  ( 0.4724409448818898682, 0.000000000000000000, -2.755905511811024056 ) ) ;
#68387 = CARTESIAN_POINT ( 'NONE',  ( 0.3083989501312343062, -0.08942795157528024563, -0.3641732283464568787 ) ) ;
#68388 = CARTESIAN_POINT ( 'NONE',  ( 0.9973753280839902091, -0.6046776061558807314, 0.2411417322834647770 ) ) ;
#68389 = CARTESIAN_POINT ( 'NONE',  ( 1.049868766404200127, -0.5023911411419708095, -0.1820866141732282451 ) ) ;
#68390 = VERTEX_POINT ( 'NONE', #28328 ) ;
#68391 = CARTESIAN_POINT ( 'NONE',  ( -1.391076115485563314, -0.6046776061558809534, -0.2411417322834644161 ) ) ;
#68392 = CARTESIAN_POINT ( 'NONE',  ( -1.062992125984250968, -0.6692913385826771977, 8.415575281601705876E-17 ) ) ;
#68393 = CARTESIAN_POINT ( 'NONE',  ( -0.006561679790025524116, -0.3162353388693405765, 0.4822834645669290543 ) ) ;
#68394 = CARTESIAN_POINT ( 'NONE',  ( -2.167227123902250696, 1.572090529166658479, -0.4732185887570802274 ) ) ;
#68395 = CARTESIAN_POINT ( 'NONE',  ( 0.3460692066303959202, -0.1998031496062991630, -2.386482939632545985 ) ) ;
#68396 = CARTESIAN_POINT ( 'NONE',  ( 0.7283464566929140904, -0.5400638737290845981, -0.3530559997133363437 ) ) ;
#68397 = CARTESIAN_POINT ( 'NONE',  ( 1.568241469816273437, -0.2845877964562159024, 0.3641732283464567677 ) ) ;
#68398 = CARTESIAN_POINT ( 'NONE',  ( 0.09186351706036827158, 0.05413385826771666132, 0.4176697321401328100 ) ) ;
#68399 = CARTESIAN_POINT ( 'NONE',  ( 0.9186351706036751663, -0.6046776061558807314, 0.2411417322834647770 ) ) ;
#68400 = CARTESIAN_POINT ( 'NONE',  ( 0.2925321140481932369, 0.2925321140481932369, -1.712598425196850460 ) ) ;
#68401 = CARTESIAN_POINT ( 'NONE',  ( 0.1974969037888704704, 0.3420746716998660508, -1.089238845144357093 ) ) ;
#68402 = CARTESIAN_POINT ( 'NONE',  ( 4.893765752498283924E-17, -0.3996062992125986035, -2.598425196850393970 ) ) ;
#68403 = CARTESIAN_POINT ( 'NONE',  ( 0.1049643490035303689, 0.3917322834645670104, -0.4580052493438320216 ) ) ;
#68404 = CARTESIAN_POINT ( 'NONE',  ( -0.4133858267716528645, 0.07958543189024071263, -0.2665933059059888421 ) ) ;
#68405 = CARTESIAN_POINT ( 'NONE',  ( -0.8333333333333323711, -0.6692913385826773087, -0.1292274648535924053 ) ) ;
#68406 = CARTESIAN_POINT ( 'NONE',  ( 0.3871391076115492380, -0.05778040916215560624, -0.4822834645669293319 ) ) ;
#68407 = CARTESIAN_POINT ( 'NONE',  ( 0.1058382717557500852, -0.3949938075777408852, -2.366797900262467280 ) ) ;
#68408 = CARTESIAN_POINT ( 'NONE',  ( -1.653543307086613234, -0.1870078740157479769, 0.4822834645669291653 ) ) ;
#68409 = CARTESIAN_POINT ( 'NONE',  ( 1.292650918635171564, 0.2952755905511811885, 0.1292274648535926551 ) ) ;
#68410 = CARTESIAN_POINT ( 'NONE',  ( -0.4724409448818899238, 0.1265901696524986686, -2.552493438320210029 ) ) ;
#68411 = CARTESIAN_POINT ( 'NONE',  ( 0.2925321140481932369, -0.2925321140481932369, -1.830708661417322913 ) ) ;
#68412 = CARTESIAN_POINT ( 'NONE',  ( 0.2460629921259843422, 0.000000000000000000, 0.000000000000000000 ) ) ;
#68413 = CARTESIAN_POINT ( 'NONE',  ( 1.082677165354331228, -0.5400638737290844871, 0.3530559997133364547 ) ) ;
#68414 = CARTESIAN_POINT ( 'NONE',  ( 1.318897637795276356, 0.07958543189024071263, -0.2665933059059888421 ) ) ;
#68416 = CARTESIAN_POINT ( 'NONE',  ( -1.423884514435694859, -0.05778040916215560624, -0.4822834645669293319 ) ) ;
#68415 = CARTESIAN_POINT ( 'NONE',  ( 1.522309711286089939, 0.2306618581243848609, 0.2411417322834645549 ) ) ;
#68417 = CARTESIAN_POINT ( 'NONE',  ( -0.1049643490035306742, 0.3917322834645668994, -2.763760211777216202 ) ) ;
#68418 = CARTESIAN_POINT ( 'NONE',  ( 0.000000000000000000, 2.755905511811024056, 0.000000000000000000 ) ) ;
#68419 = CARTESIAN_POINT ( 'NONE',  ( 0.8070866141732289112, -0.5400638737290845981, -0.3530559997133363437 ) ) ;
#68420 = CARTESIAN_POINT ( 'NONE',  ( 1.404199475065617708, -0.004921259842519870586, -0.3153832671262229437 ) ) ;
#68421 = CARTESIAN_POINT ( 'NONE',  ( -0.6889763779527552368, -0.5400638737290845981, -0.3530559997133363437 ) ) ;
#68422 = CARTESIAN_POINT ( 'NONE',  ( -0.5380577427821514602, -0.4281496062992127816, -0.4176697321401328100 ) ) ;
#68423 = CARTESIAN_POINT ( 'NONE',  ( -1.653543307086613234, -0.1870078740157479769, 0.4822834645669291653 ) ) ;
#68424 = CARTESIAN_POINT ( 'NONE',  ( 0.3917322834645669549, 0.1049643490035304660, -0.05183727034120744204 ) ) ;
#68425 = CARTESIAN_POINT ( 'NONE',  ( 0.2362204724409456558, -0.1870078740157480879, -0.4822834645669291653 ) ) ;
#68426 = CARTESIAN_POINT ( 'NONE',  ( 0.3917322834645670104, 2.398668435337828261E-17, -2.472440944881889813 ) ) ;
#68427 = CARTESIAN_POINT ( 'NONE',  ( -1.496062992125983815, -0.1870078740157479769, 0.3641732283464567677 ) ) ;
#68428 = ORIENTED_EDGE ( 'NONE', *, *, #74844, .T. ) ;
#68429 = CARTESIAN_POINT ( 'NONE',  ( 0.3949938075777409408, 0.1058382717557500574, -2.801837270341207553 ) ) ;
#68430 = ORIENTED_EDGE ( 'NONE', *, *, #20213, .T. ) ;
#68431 = CARTESIAN_POINT ( 'NONE',  ( 0.000000000000000000, 0.000000000000000000, 3.858267716535433323 ) ) ;
#68432 = CARTESIAN_POINT ( 'NONE',  ( -1.430446194225721390, -0.4281496062992124485, 0.4176697321401328655 ) ) ;
#68433 = CARTESIAN_POINT ( 'NONE',  ( 0.1998031496062992740, 0.3460692066303959757, -0.9317585301837270073 ) ) ;
#68434 = CARTESIAN_POINT ( 'NONE',  ( 1.574803149606299746, -0.1870078740157480601, -0.3641732283464567677 ) ) ;
#68435 = CARTESIAN_POINT ( 'NONE',  ( -0.09842519685039295696, 0.1012011053420775880, -0.2882089793578257453 ) ) ;
#68436 = LINE ( 'NONE', #18731, #54422 ) ;
#68437 = CARTESIAN_POINT ( 'NONE',  ( -0.2977726995931780918, 1.789762378577807400, 0.09694807015762342550 ) ) ;
#68438 = CARTESIAN_POINT ( 'NONE',  ( -0.1049643490035307020, 0.3917322834645669549, -0.5636482939632546652 ) ) ;
#68439 = CARTESIAN_POINT ( 'NONE',  ( -0.1181102362204717315, -0.5511811023622047445, 6.969142054262312111E-17 ) ) ;
#68440 = CARTESIAN_POINT ( 'NONE',  ( -1.364829396325458521, 0.1283753931104746893, -0.1820866141732285504 ) ) ;
#68441 = CARTESIAN_POINT ( 'NONE',  ( -1.482939632545930975, 0.05413385826771666132, 0.4176697321401328100 ) ) ;
#68442 = CARTESIAN_POINT ( 'NONE',  ( 0.5971128608923890191, -0.6692913385826771977, 0.1292274648535927661 ) ) ;
#68443 = CARTESIAN_POINT ( 'NONE',  ( -1.345144356955379816, -0.3162353388693405765, 0.4822834645669290543 ) ) ;
#68444 = CARTESIAN_POINT ( 'NONE',  ( -0.1958661417322836718, 0.3392501089628017219, -0.3202099737532808077 ) ) ;
#68445 = ORIENTED_EDGE ( 'NONE', *, *, #39193, .T. ) ;
#68446 = CARTESIAN_POINT ( 'NONE',  ( -1.607611548556429737, 0.2952755905511810774, -0.1292274648535930714 ) ) ;
#68447 = CARTESIAN_POINT ( 'NONE',  ( 1.614173228346456712, 0.4405861044731111953, 0.1372047244094478646 ) ) ;
#68448 = CARTESIAN_POINT ( 'NONE',  ( -1.157146581871515012E-16, 0.4724409448818898682, -1.574803149606299302 ) ) ;
#68449 = CARTESIAN_POINT ( 'NONE',  ( 2.094141031014959520, 1.724409448818898127, 0.4359958488159723644 ) ) ;
#68450 = ADVANCED_FACE ( 'NONE', ( #73373 ), #79702, .F. ) ;
#68451 = CARTESIAN_POINT ( 'NONE',  ( 0.1049643490035304799, -0.3917322834645669549, -2.689632545931758489 ) ) ;
#68452 = CARTESIAN_POINT ( 'NONE',  ( -0.7545931758530176614, -0.6692913385826773087, -0.1292274648535924053 ) ) ;
#68453 = CARTESIAN_POINT ( 'NONE',  ( 1.496062992125985147, -0.1870078740157479769, 0.4822834645669291653 ) ) ;
#68455 = CARTESIAN_POINT ( 'NONE',  ( 1.614173228346457378, 0.9921945702958886448, -0.1372047244094476148 ) ) ;
#68454 = CARTESIAN_POINT ( 'NONE',  ( 0.000000000000000000, 2.716535433070866645, 0.000000000000000000 ) ) ;
#68456 = VECTOR ( 'NONE', #44881, 39.37007874015748143 ) ;
#68457 = CARTESIAN_POINT ( 'NONE',  ( -1.699475065616797398, 0.2952755905511811885, 0.1292274648535926551 ) ) ;
#68458 = CARTESIAN_POINT ( 'NONE',  ( -0.7217847769028863381, 0.05413385826771626580, -0.4176697321401330321 ) ) ;
#68459 = CARTESIAN_POINT ( 'NONE',  ( -0.2867679344610366554, 0.2867679344610365444, -0.2571985319871897824 ) ) ;
#68460 = CARTESIAN_POINT ( 'NONE',  ( -0.07874015748031421014, -0.1870078740157480601, -0.3641732283464567677 ) ) ;
#68461 = CARTESIAN_POINT ( 'NONE',  ( 4.797336870675656522E-17, -0.3917322834645670104, -0.4783464566929135353 ) ) ;
#68462 = CARTESIAN_POINT ( 'NONE',  ( -0.1706036745406816491, -0.004921259842519870586, -0.3153832671262229437 ) ) ;
#68463 = CARTESIAN_POINT ( 'NONE',  ( 0.5839895013123367340, -0.5511811023622048555, -0.09757992244046775898 ) ) ;
#68464 = CARTESIAN_POINT ( 'NONE',  ( 0.4002624671916016896, -0.3162353388693409650, -0.4822834645669289433 ) ) ;
#68465 = CARTESIAN_POINT ( 'NONE',  ( -0.8595800524934373854, -0.08942795157527998196, 0.3641732283464567121 ) ) ;
#68466 = CARTESIAN_POINT ( 'NONE',  ( 0.3917322834645669549, 0.1049643490035304660, -2.479002624671915900 ) ) ;
#68467 = CARTESIAN_POINT ( 'NONE',  ( -1.640419947506561060, 0.05413385826771666132, 0.4176697321401328100 ) ) ;
#68468 = CARTESIAN_POINT ( 'NONE',  ( -1.148293963254592542, 0.2952755905511811885, 0.1292274648535926551 ) ) ;
#68469 = CARTESIAN_POINT ( 'NONE',  ( 0.2362204724409451007, -0.4091458600556402980, -0.7985564304461942875 ) ) ;
#68470 = CARTESIAN_POINT ( 'NONE',  ( -0.03280839895013062252, -0.6692913385826771977, 0.1292274648535927661 ) ) ;
#68471 = CARTESIAN_POINT ( 'NONE',  ( -0.6627296587926501115, 0.2952755905511810774, -0.1292274648535930714 ) ) ;
#68472 = CARTESIAN_POINT ( 'NONE',  ( 1.358267716535433323, 0.07958543189024085140, 0.2665933059059887866 ) ) ;
#68473 = CARTESIAN_POINT ( 'NONE',  ( 0.1246719160104994284, -0.5511811023622046335, 0.09757992244046803654 ) ) ;
#68474 = CARTESIAN_POINT ( 'NONE',  ( -0.4265091863517051496, 0.2952755905511810774, -0.1292274648535930714 ) ) ;
#68475 = CARTESIAN_POINT ( 'NONE',  ( -0.8267716535433065062, 0.2952755905511811885, 0.000000000000000000 ) ) ;
#68476 = CARTESIAN_POINT ( 'NONE',  ( -3.900966923095589678, 2.677165354330708791, 0.5314960629921260393 ) ) ;
#68477 = CARTESIAN_POINT ( 'NONE',  ( -0.3458507752293909498, 0.3458507752293908388, -0.3346456692913385433 ) ) ;
#68478 = CARTESIAN_POINT ( 'NONE',  ( 0.3083989501312343062, -0.05778040916215560624, -0.4822834645669293319 ) ) ;
#68479 = ORIENTED_EDGE ( 'NONE', *, *, #80156, .F. ) ;
#68480 = CARTESIAN_POINT ( 'NONE',  ( 0.2925321140481932369, -0.2925321140481931814, -1.907480314960629197 ) ) ;
#68481 = CARTESIAN_POINT ( 'NONE',  ( 1.062992125984252745, -0.6692913385826771977, 8.415575281601705876E-17 ) ) ;
#68482 = CARTESIAN_POINT ( 'NONE',  ( -0.6036745406824141069, 0.1283753931104748280, 0.1820866141732283561 ) ) ;
#68483 = CARTESIAN_POINT ( 'NONE',  ( -0.7611548556430438595, 0.2306618581243848609, 0.2411417322834645549 ) ) ;
#68484 = CARTESIAN_POINT ( 'NONE',  ( 1.167979002624672580, -0.4281496062992124485, 0.4176697321401328655 ) ) ;
#68485 = CARTESIAN_POINT ( 'NONE',  ( 0.8333333333333340365, -0.6692913385826771977, 0.1292274648535927661 ) ) ;
#68486 = CARTESIAN_POINT ( 'NONE',  ( -1.535433070866141225, -0.6692913385826771977, 8.415575281601705876E-17 ) ) ;
#68487 = CARTESIAN_POINT ( 'NONE',  ( -1.082677165354329896, 0.07958543189024085140, 0.2665933059059887866 ) ) ;
#68488 = CARTESIAN_POINT ( 'NONE',  ( -0.1070741851644057135, 0.3996062992125984925, -0.3982939632545931530 ) ) ;
#68489 = CARTESIAN_POINT ( 'NONE',  ( -0.2925321140481930704, -0.2925321140481933480, -0.3740157480314960092 ) ) ;
#68490 = CARTESIAN_POINT ( 'NONE',  ( 4.837279021331060870E-17, -0.3949938075777409963, 0.07874015748031490403 ) ) ;
#68491 = CARTESIAN_POINT ( 'NONE',  ( 1.489501312335958172, -0.2845877964562159024, 0.3641732283464567677 ) ) ;
#68492 = CARTESIAN_POINT ( 'NONE',  ( 1.003937007874016185, 0.07958543189024071263, -0.2665933059059888421 ) ) ;
#68493 = CARTESIAN_POINT ( 'NONE',  ( 0.6889763779527563470, 0.1660481256975883668, -0.3530559997133364547 ) ) ;
#68494 = CARTESIAN_POINT ( 'NONE',  ( 0.4600214019799526155, 2.784432375088962958E-17, -0.3464511005275205946 ) ) ;
#68495 = CARTESIAN_POINT ( 'NONE',  ( -0.1974969037888704149, -0.3420746716998661063, -1.087270341207349000 ) ) ;
#68496 = CARTESIAN_POINT ( 'NONE',  ( 0.6430446194225729606, -0.3690944881889765550, -0.3153832671262227771 ) ) ;
#68497 = CARTESIAN_POINT ( 'NONE',  ( -0.2362204724409440182, -0.1870078740157479769, 0.4822834645669291653 ) ) ;
#68498 = CARTESIAN_POINT ( 'NONE',  ( -0.7742782152230962556, -0.4281496062992127816, -0.4176697321401328100 ) ) ;
#68499 = CARTESIAN_POINT ( 'NONE',  ( 1.377952755905512472, 0.2952755905511811885, 0.000000000000000000 ) ) ;
#68500 = CARTESIAN_POINT ( 'NONE',  ( -1.157146581871515012E-16, 0.4724409448818898682, -1.259842519685039353 ) ) ;
#68501 = CARTESIAN_POINT ( 'NONE',  ( -0.1070741851644057135, 0.3996062992125985480, -2.211286089238845065 ) ) ;
#68502 = CARTESIAN_POINT ( 'NONE',  ( 0.09842519685039434474, -0.4536011799217368745, -0.2665933059059886201 ) ) ;
#68503 = ORIENTED_EDGE ( 'NONE', *, *, #50047, .T. ) ;
#68504 = CARTESIAN_POINT ( 'NONE',  ( -0.1049643490035307158, 0.3917322834645670104, -0.6332214155193720551 ) ) ;
#68505 = ORIENTED_EDGE ( 'NONE', *, *, #69856, .T. ) ;
#68506 = CARTESIAN_POINT ( 'NONE',  ( -1.023622047244094002, -0.1870078740157480879, -0.4822834645669291653 ) ) ;
#68507 = CARTESIAN_POINT ( 'NONE',  ( 8.195543980992789655E-16, -0.1870078740157480879, -0.4822834645669291653 ) ) ;
#68508 = CARTESIAN_POINT ( 'NONE',  ( -0.2099737532808391705, 0.2306618581243848609, 0.2411417322834645549 ) ) ;
#68509 = CARTESIAN_POINT ( 'NONE',  ( 0.7020997375328090762, -0.3162353388693405765, 0.4822834645669290543 ) ) ;
#68510 = CARTESIAN_POINT ( 'NONE',  ( -0.2690288713910754526, -0.6692913385826771977, 0.1292274648535927661 ) ) ;
#68511 = CARTESIAN_POINT ( 'NONE',  ( -1.384514435695537005, -0.6692913385826773087, -0.1292274648535924053 ) ) ;
#68512 = CARTESIAN_POINT ( 'NONE',  ( -0.5708661417322828946, 0.1660481256975883668, -0.3530559997133364547 ) ) ;
#68513 = CARTESIAN_POINT ( 'NONE',  ( 0.8333333333333340365, 0.2952755905511810774, -0.1292274648535930714 ) ) ;
#68514 = CARTESIAN_POINT ( 'NONE',  ( 0.6692913385826777528, 0.2952755905511811885, 0.000000000000000000 ) ) ;
#68515 = CARTESIAN_POINT ( 'NONE',  ( 0.1049643490035303689, 0.3917322834645670104, -0.9304461942257216123 ) ) ;
#68516 = CARTESIAN_POINT ( 'NONE',  ( -0.4133858267716528645, -0.4536011799217367080, 0.2665933059059888421 ) ) ;
#68517 = VERTEX_POINT ( 'NONE', #41776 ) ;
#68518 = CARTESIAN_POINT ( 'NONE',  ( -0.3420746716998661618, 0.1974969037888702206, -1.286089238845144367 ) ) ;
#68519 = ORIENTED_EDGE ( 'NONE', *, *, #4442, .T. ) ;
#68520 = CARTESIAN_POINT ( 'NONE',  ( -1.076115485564303809, 0.1283753931104748280, 0.1820866141732283561 ) ) ;
#68521 = CARTESIAN_POINT ( 'NONE',  ( -0.5905511811023613777, -0.6692913385826771977, 8.415575281601705876E-17 ) ) ;
#68522 = CARTESIAN_POINT ( 'NONE',  ( -1.385122803245538714, 1.251927150221335605, 0.3798795596076748882 ) ) ;
#68523 = CARTESIAN_POINT ( 'NONE',  ( -0.5314960629921254842, -0.5400638737290845981, -0.3530559997133363437 ) ) ;
#68524 = CARTESIAN_POINT ( 'NONE',  ( -0.7152230971128602510, -0.05778040916215560624, -0.4822834645669293319 ) ) ;
#68525 = CARTESIAN_POINT ( 'NONE',  ( -1.463254593175852492, 0.2952755905511811885, 0.1292274648535926551 ) ) ;
#68526 = CARTESIAN_POINT ( 'NONE',  ( -1.706036745406823485, 0.2306618581243848609, 0.2411417322834645549 ) ) ;
#68527 = CARTESIAN_POINT ( 'NONE',  ( 0.8792650918635177559, -0.004921259842519576551, 0.3153832671262227771 ) ) ;
#68528 = CARTESIAN_POINT ( 'NONE',  ( 0.4091458600556403535, 0.2362204724409449896, -0.3654855643044619407 ) ) ;
#68529 = CARTESIAN_POINT ( 'NONE',  ( 4.797336870675656522E-17, -0.3917322834645670104, 0.1515748031496061965 ) ) ;
#68530 = CARTESIAN_POINT ( 'NONE',  ( 0.1706036745406830368, -0.004921259842519576551, 0.3153832671262227771 ) ) ;
#68531 = CARTESIAN_POINT ( 'NONE',  ( -0.4330708661417315697, -0.6692913385826771977, 8.415575281601705876E-17 ) ) ;
#68532 = PLANE ( 'NONE',  #49623 ) ;
#68533 = CARTESIAN_POINT ( 'NONE',  ( -0.2427821522309703550, -0.3162353388693405765, 0.4822834645669290543 ) ) ;
#68534 = ORIENTED_EDGE ( 'NONE', *, *, #33608, .T. ) ;
#68535 = CARTESIAN_POINT ( 'NONE',  ( 0.3996062992125986035, 2.446882876249141962E-17, -2.165354330708661568 ) ) ;
#68536 = DIRECTION ( 'NONE',  ( 0.000000000000000000, 0.000000000000000000, -1.000000000000000000 ) ) ;
#68537 = ORIENTED_EDGE ( 'NONE', *, *, #68192, .F. ) ;
#68538 = CARTESIAN_POINT ( 'NONE',  ( -0.3996062992125986590, 0.1070741851644051723, -1.684383202099737353 ) ) ;
#68539 = CARTESIAN_POINT ( 'NONE',  ( -0.02899565511876225909, 0.3969271875946638328, -2.755905511811026276 ) ) ;
#68540 = CARTESIAN_POINT ( 'NONE',  ( -0.7414698162729651543, 0.1771653543307087075, -0.09757992244046823083 ) ) ;
#68541 = CARTESIAN_POINT ( 'NONE',  ( -0.7939632545931754048, -0.3162353388693405765, 0.4822834645669290543 ) ) ;
#68542 = CARTESIAN_POINT ( 'NONE',  ( -0.4091458600556405756, 0.2362204724409446288, -0.4986876640419947715 ) ) ;
#68543 = CARTESIAN_POINT ( 'NONE',  ( -0.2508763215440125705, 1.134457504807420802, 3.929027568737346154 ) ) ;
#68544 = CARTESIAN_POINT ( 'NONE',  ( 0.1049643490035304938, -0.3917322834645669549, -2.532152230971127960 ) ) ;
#68545 = CARTESIAN_POINT ( 'NONE',  ( 1.194225721784777594, 0.05413385826771666132, 0.4176697321401328100 ) ) ;
#68546 = CARTESIAN_POINT ( 'NONE',  ( 0.3083989501312343062, -0.3162353388693405765, 0.4822834645669290543 ) ) ;
#68547 = CARTESIAN_POINT ( 'NONE',  ( 0.6036745406824154392, 0.2306618581243847221, -0.2411417322834647770 ) ) ;
#68548 = CARTESIAN_POINT ( 'NONE',  ( -0.5446194225721777693, -0.08942795157527998196, 0.3641732283464567121 ) ) ;
#68549 = CARTESIAN_POINT ( 'NONE',  ( -0.1902887139107604098, -0.6692913385826771977, 0.1292274648535927661 ) ) ;
#68550 = CARTESIAN_POINT ( 'NONE',  ( 0.4724409448818896462, 0.1265901696524990294, -2.248687664041994605 ) ) ;
#68551 = CARTESIAN_POINT ( 'NONE',  ( -0.7086614173228339419, -0.1870078740157480879, -0.4822834645669291653 ) ) ;
#68552 = CARTESIAN_POINT ( 'NONE',  ( -0.2891555358219911054, 0.2891555358219909388, -2.143700787401574548 ) ) ;
#68553 = CARTESIAN_POINT ( 'NONE',  ( 1.358267716535433323, -0.4536011799217368745, -0.2665933059059886201 ) ) ;
#68554 = CARTESIAN_POINT ( 'NONE',  ( -0.3740157480314953431, -0.4536011799217368745, -0.2665933059059886201 ) ) ;
#68555 = CARTESIAN_POINT ( 'NONE',  ( 1.154855643044620184, -0.5023911411419708095, 0.1820866141732285504 ) ) ;
#68556 = CARTESIAN_POINT ( 'NONE',  ( -1.712598425196849572, 0.1660481256975885056, 0.3530559997133364547 ) ) ;
#68557 = CARTESIAN_POINT ( 'NONE',  ( -1.154855643044618851, 0.1283753931104748280, 0.1820866141732283561 ) ) ;
#68558 = CARTESIAN_POINT ( 'NONE',  ( 0.4091458600556404646, -0.2362204724409448231, -2.229002624671915900 ) ) ;
#68559 = CARTESIAN_POINT ( 'NONE',  ( -1.318897637795274802, -0.5400638737290845981, -0.3530559997133363437 ) ) ;
#68560 = CARTESIAN_POINT ( 'NONE',  ( -0.3412073490813641308, 0.2306618581243847221, -0.2411417322834647770 ) ) ;
#68561 = ADVANCED_BREP_SHAPE_REPRESENTATION ( '', ( #61376, #22098 ), #65120 ) ;
#68562 = CARTESIAN_POINT ( 'NONE',  ( -2.169549780153866347, 1.520054044952883876, 0.4741688556381176700 ) ) ;
#68563 = CARTESIAN_POINT ( 'NONE',  ( -0.09842519685039295696, -0.4536011799217367080, 0.2665933059059888421 ) ) ;
#68564 = CARTESIAN_POINT ( 'NONE',  ( -1.620734908136482577, -0.5511811023622048555, -0.09757992244046775898 ) ) ;
#68565 = CARTESIAN_POINT ( 'NONE',  ( 0.5577427821522316087, -0.05778040916215522460, 0.4822834645669289988 ) ) ;
#68566 = CARTESIAN_POINT ( 'NONE',  ( -1.535433070866141225, 0.1771653543307087630, 0.000000000000000000 ) ) ;
#68567 = CARTESIAN_POINT ( 'NONE',  ( 1.397637795275591177, -0.4536011799217367080, 0.2665933059059888421 ) ) ;
#68568 = CARTESIAN_POINT ( 'NONE',  ( -0.7349081364829390672, 0.2306618581243847221, -0.2411417322834647770 ) ) ;
#68569 = CARTESIAN_POINT ( 'NONE',  ( -0.2427821522309703550, -0.2845877964562159024, 0.3641732283464567677 ) ) ;
#68570 = CARTESIAN_POINT ( 'NONE',  ( -0.8785612751854012803, -2.613618158232546091E-15, -0.3464511005275220379 ) ) ;
#68571 = CARTESIAN_POINT ( 'NONE',  ( 0.1312335958005255154, -0.5023911411419708095, 0.1820866141732285504 ) ) ;
#68572 = EDGE_CURVE ( 'NONE', #28439, #79831, #42610, .T. ) ;
#68573 = CARTESIAN_POINT ( 'NONE',  ( -0.2887139107611542133, -0.6046776061558809534, -0.2411417322834644161 ) ) ;
#68574 = CARTESIAN_POINT ( 'NONE',  ( 0.1998031496062992463, 0.3460692066303959202, -0.8510498687664042050 ) ) ;
#68575 = EDGE_CURVE ( 'NONE', #50999, #18885, #42871, .T. ) ;
#68576 = CARTESIAN_POINT ( 'NONE',  ( -0.3392501089628019995, 0.1958661417322832277, -2.315616797900262647 ) ) ;
#68577 = CARTESIAN_POINT ( 'NONE',  ( 0.6036745406824153282, -0.5023911411419708095, 0.1820866141732285504 ) ) ;
#68578 = CARTESIAN_POINT ( 'NONE',  ( -0.5118110236220466680, 0.2952755905511811885, 0.000000000000000000 ) ) ;
#68579 = CARTESIAN_POINT ( 'NONE',  ( -0.6036745406824141069, -0.6046776061558809534, -0.2411417322834644161 ) ) ;
#68580 = CARTESIAN_POINT ( 'NONE',  ( -0.8398950131233585692, 0.1283753931104748280, 0.1820866141732283561 ) ) ;
#68581 = CARTESIAN_POINT ( 'NONE',  ( 2.787279214012418738, 1.535433070866142113, 0.000000000000000000 ) ) ;
#68582 = CARTESIAN_POINT ( 'NONE',  ( -0.5380577427821514602, -0.004921259842519576551, 0.3153832671262227771 ) ) ;
#68583 = CARTESIAN_POINT ( 'NONE',  ( -0.08530183727034056085, -0.3162353388693405765, 0.4822834645669290543 ) ) ;
#68584 = CARTESIAN_POINT ( 'NONE',  ( -0.9711286089238838626, -0.5023911411419708095, 0.1820866141732285504 ) ) ;
#68585 = CARTESIAN_POINT ( 'NONE',  ( 0.1998031496062994128, -0.3460692066303957537, -1.585958005249344049 ) ) ;
#68586 = CARTESIAN_POINT ( 'NONE',  ( -1.541994750656167090, -0.6692913385826773087, -0.1292274648535924053 ) ) ;
#68587 = CARTESIAN_POINT ( 'NONE',  ( -0.4724409448818898682, -8.678599364036362592E-17, -2.244094488188976388 ) ) ;
#68588 = ORIENTED_EDGE ( 'NONE', *, *, #34764, .T. ) ;
#68589 = CARTESIAN_POINT ( 'NONE',  ( -1.633858267716534529, -0.4536011799217368745, -0.2665933059059886201 ) ) ;
#68590 = CARTESIAN_POINT ( 'NONE',  ( -0.4658792650918627265, -0.05778040916215522460, 0.4822834645669289988 ) ) ;
#68591 = CARTESIAN_POINT ( 'NONE',  ( -1.154855643044618851, 0.2306618581243848609, 0.2411417322834645549 ) ) ;
#68592 = CARTESIAN_POINT ( 'NONE',  ( -0.2867679344610364334, -0.2867679344610367109, -1.561023622047243986 ) ) ;
#68593 = FACE_OUTER_BOUND ( 'NONE', #44236, .T. ) ;
#68594 = EDGE_CURVE ( 'NONE', #44792, #19641, #54676, .T. ) ;
#68595 = CARTESIAN_POINT ( 'NONE',  ( 0.8792650918635177559, 0.05413385826771666132, 0.4176697321401328100 ) ) ;
#68596 = CARTESIAN_POINT ( 'NONE',  ( 0.4921259842519691285, -0.5400638737290845981, -0.3530559997133363437 ) ) ;
#68597 = FACE_OUTER_BOUND ( 'NONE', #63023, .T. ) ;
#68598 = CARTESIAN_POINT ( 'NONE',  ( -0.3460692066303957537, -0.1998031496062994405, -2.333989501312335957 ) ) ;
#68599 = CARTESIAN_POINT ( 'NONE',  ( 0.9973753280839902091, 0.1283753931104746893, -0.1820866141732285504 ) ) ;
#68600 = CARTESIAN_POINT ( 'NONE',  ( -0.3996062992125987146, 0.1070741851644051862, -0.9776902887139107268 ) ) ;
#68601 = ORIENTED_EDGE ( 'NONE', *, *, #41459, .F. ) ;
#68602 = CARTESIAN_POINT ( 'NONE',  ( -0.8858267716535425107, -0.4536011799217367080, 0.2665933059059888421 ) ) ;
#68603 = CARTESIAN_POINT ( 'NONE',  ( 0.3392501089628018329, 0.1958661417322835607, -2.485564304461941987 ) ) ;
#68604 = ORIENTED_EDGE ( 'NONE', *, *, #63199, .T. ) ;
#68605 = CARTESIAN_POINT ( 'NONE',  ( 0.5577427821522314977, -0.3162353388693409650, -0.4822834645669289433 ) ) ;
#68606 = CARTESIAN_POINT ( 'NONE',  ( -0.5905511811023615998, 0.2952755905511811885, 0.000000000000000000 ) ) ;
#68607 = CARTESIAN_POINT ( 'NONE',  ( -0.9842519685039360366, 0.2952755905511811885, 0.000000000000000000 ) ) ;
#68608 = CARTESIAN_POINT ( 'NONE',  ( 0.9711286089238851948, -0.6046776061558809534, -0.2411417322834644161 ) ) ;
#68609 = CARTESIAN_POINT ( 'NONE',  ( -1.437007874015747477, 0.07958543189024071263, -0.2665933059059888421 ) ) ;
#68610 = CARTESIAN_POINT ( 'NONE',  ( -1.614173228346457378, 0.9921945702958913094, 0.1372047244094476981 ) ) ;
#68611 = CARTESIAN_POINT ( 'NONE',  ( 0.05905511811023709395, -0.5400638737290844871, 0.3530559997133364547 ) ) ;
#68612 = CARTESIAN_POINT ( 'NONE',  ( -1.049868766404198794, -0.6046776061558807314, 0.2411417322834647770 ) ) ;
#68613 = CARTESIAN_POINT ( 'NONE',  ( 0.2867679344610365999, 0.2867679344610365999, -1.950111917813961426 ) ) ;
#68614 = CARTESIAN_POINT ( 'NONE',  ( -1.594488188976377119, 0.1660481256975883668, -0.3530559997133364547 ) ) ;
#68615 = DIRECTION ( 'NONE',  ( 1.000000000000000000, -1.445602896647338917E-16, 0.000000000000000000 ) ) ;
#68616 = CARTESIAN_POINT ( 'NONE',  ( 0.3917322834645670104, -0.1049643490035303411, 0.05380577427821527092 ) ) ;
#68617 = CARTESIAN_POINT ( 'NONE',  ( 0.8005249343832028242, -0.3690944881889765550, -0.3153832671262227771 ) ) ;
#68618 = ORIENTED_EDGE ( 'NONE', *, *, #80156, .T. ) ;
#68619 = CARTESIAN_POINT ( 'NONE',  ( 0.3420746716998659953, 0.1974969037888705536, -0.2887139107611549349 ) ) ;
#68620 = CARTESIAN_POINT ( 'NONE',  ( -1.030183727034119867, -0.3162353388693405765, 0.4822834645669290543 ) ) ;
#68621 = ORIENTED_EDGE ( 'NONE', *, *, #81623, .F. ) ;
#68622 = CARTESIAN_POINT ( 'NONE',  ( 5.463695987328526437E-16, -0.1870078740157479769, 0.3641732283464567677 ) ) ;
#68623 = CARTESIAN_POINT ( 'NONE',  ( -1.515748031496062076, 0.1660481256975883668, -0.3530559997133364547 ) ) ;
#68624 = CARTESIAN_POINT ( 'NONE',  ( 0.5643044619422579178, -0.4281496062992127816, -0.4176697321401328100 ) ) ;
#68625 = CARTESIAN_POINT ( 'NONE',  ( 0.5577427821522314977, -0.3162353388693409650, -0.4822834645669289433 ) ) ;
#68626 = CARTESIAN_POINT ( 'NONE',  ( -0.7874015748031489847, -0.1870078740157479769, 0.4822834645669291653 ) ) ;
#68627 = CARTESIAN_POINT ( 'NONE',  ( -0.1049643490035307158, 0.3917322834645670104, -1.420622990322521373 ) ) ;
#68628 = CARTESIAN_POINT ( 'NONE',  ( -0.8005249343832011588, 0.05413385826771626580, -0.4176697321401330321 ) ) ;
#68629 = CARTESIAN_POINT ( 'NONE',  ( -0.3917322834645671215, 0.1049643490035301469, -2.637139107611548461 ) ) ;
#68630 = CARTESIAN_POINT ( 'NONE',  ( 1.325459317585302665, -0.004921259842519870586, -0.3153832671262229437 ) ) ;
#68631 = CARTESIAN_POINT ( 'NONE',  ( -0.9776902887139098386, 0.2952755905511810774, -0.1292274648535930714 ) ) ;
#68632 = CARTESIAN_POINT ( 'NONE',  ( 1.049868766404200349, 0.2306618581243848609, 0.2411417322834645549 ) ) ;
#68633 = CARTESIAN_POINT ( 'NONE',  ( 1.391076115485564868, 0.2306618581243847221, -0.2411417322834647770 ) ) ;
#68634 = AXIS2_PLACEMENT_3D ( 'NONE', #3112, #58364, #14199 ) ;
#68635 = CARTESIAN_POINT ( 'NONE',  ( 0.3996062992125986035, 0.1070741851644054776, -0.7545931758530182165 ) ) ;
#68636 = CARTESIAN_POINT ( 'NONE',  ( -1.469816272965878357, -0.6046776061558809534, -0.2411417322834644161 ) ) ;
#68637 = CARTESIAN_POINT ( 'NONE',  ( -0.1998031496062991630, -0.3460692066303959202, -0.4573490813648293796 ) ) ;
#68638 = CARTESIAN_POINT ( 'NONE',  ( 0.3346456692913390985, 0.1660481256975885056, 0.3530559997133364547 ) ) ;
#68639 = CARTESIAN_POINT ( 'NONE',  ( 0.3996062992125986035, 0.1070741851644054776, -2.329396325459317296 ) ) ;
#68640 = CARTESIAN_POINT ( 'NONE',  ( -1.417322834645668772, -0.1870078740157480601, -0.3641732283464567677 ) ) ;
#68641 = CARTESIAN_POINT ( 'NONE',  ( 0.5118110236220480003, -0.5511811023622047445, 6.969142054262312111E-17 ) ) ;
#68642 = CARTESIAN_POINT ( 'NONE',  ( 1.095800524934383846, -0.3162353388693405765, 0.4822834645669290543 ) ) ;
#68643 = CARTESIAN_POINT ( 'NONE',  ( 0.2362204724409451007, -0.4091458600556402980, -1.270997375328083878 ) ) ;
#68645 = EDGE_CURVE ( 'NONE', #19973, #19878, #39623, .T. ) ;
#68644 = CARTESIAN_POINT ( 'NONE',  ( 0.6299212598425204535, -0.1870078740157480601, -0.3641732283464567677 ) ) ;
#68646 = CARTESIAN_POINT ( 'NONE',  ( 0.7086614173228352742, -0.1870078740157480879, -0.4822834645669291653 ) ) ;
#68647 = CARTESIAN_POINT ( 'NONE',  ( 0.1058382717557500852, -0.3949938075777408852, -0.4770341207349081403 ) ) ;
#68648 = CARTESIAN_POINT ( 'NONE',  ( -0.8398950131233589023, -0.6046776061558809534, -0.2411417322834644161 ) ) ;
#68649 = CARTESIAN_POINT ( 'NONE',  ( -1.646051170424378096, 0.000000000000000000, -0.3464511005275205946 ) ) ;
#68650 = CARTESIAN_POINT ( 'NONE',  ( 1.089238845144357537, -0.3690944881889763329, 0.3153832671262228327 ) ) ;
#68651 = CARTESIAN_POINT ( 'NONE',  ( -0.6036745406824141069, 0.2306618581243848609, 0.2411417322834645549 ) ) ;
#68652 = CARTESIAN_POINT ( 'NONE',  ( 0.1902887139107617975, 0.2952755905511811885, 0.1292274648535926551 ) ) ;
#68653 = AXIS2_PLACEMENT_3D ( 'NONE', #55941, #14682, #59270 ) ;
#68654 = CARTESIAN_POINT ( 'NONE',  ( 0.4744094488189011805, 1.537401574803149984, -1.016821367227981998 ) ) ;
#68655 = CARTESIAN_POINT ( 'NONE',  ( 0.1640419947506569498, -0.05778040916215522460, 0.4822834645669289988 ) ) ;
#68656 = CARTESIAN_POINT ( 'NONE',  ( 0.006561679790026889343, -0.2845877964562161244, -0.3641732283464567121 ) ) ;
#68657 = CARTESIAN_POINT ( 'NONE',  ( -2.873826567705916712, 1.063196196511239089, -0.01636564761922175773 ) ) ;
#68658 = CARTESIAN_POINT ( 'NONE',  ( 0.1115485564304470323, 0.1771653543307087630, 0.09757992244046791164 ) ) ;
#68659 = CARTESIAN_POINT ( 'NONE',  ( 0.8727034120734912248, -0.2845877964562161244, -0.3641732283464567121 ) ) ;
#68660 = DIRECTION ( 'NONE',  ( 0.000000000000000000, 0.000000000000000000, 1.000000000000000000 ) ) ;
#68661 = ADVANCED_FACE ( 'NONE', ( #62805 ), #3907, .F. ) ;
#68662 = CARTESIAN_POINT ( 'NONE',  ( -0.3460692066303957537, -0.1998031496062994405, -1.704068241469816281 ) ) ;
#68663 = CARTESIAN_POINT ( 'NONE',  ( 0.1837270341207357105, -0.6046776061558809534, -0.2411417322834644161 ) ) ;
#68664 = CARTESIAN_POINT ( 'NONE',  ( 0.3917322834645670104, -0.1049643490035303411, -1.363517060367453793 ) ) ;
#68665 = CARTESIAN_POINT ( 'NONE',  ( 1.607611548556431069, -0.5511811023622048555, -0.09757992244046775898 ) ) ;
#68666 = CARTESIAN_POINT ( 'NONE',  ( -0.1324727617108180378, -0.3692639355350240127, -1.489137855930807863E-17 ) ) ;
#68667 = CARTESIAN_POINT ( 'NONE',  ( -0.3215223097112853146, -0.2845877964562159024, 0.3641732283464567677 ) ) ;
#68668 = CARTESIAN_POINT ( 'NONE',  ( -0.4921259842519677963, 0.1660481256975883668, -0.3530559997133364547 ) ) ;
#68669 = CARTESIAN_POINT ( 'NONE',  ( 0.8267716535433078384, -0.5511811023622047445, 6.969142054262312111E-17 ) ) ;
#68670 = CARTESIAN_POINT ( 'NONE',  ( 0.03140460581128053097, 1.062992125984252301, -1.122047244094487972 ) ) ;
#68671 = CARTESIAN_POINT ( 'NONE',  ( 1.318897637795276356, 0.07958543189024071263, -0.2665933059059888421 ) ) ;
#68672 = CARTESIAN_POINT ( 'NONE',  ( 0.01312335958005323398, -0.4281496062992127816, -0.4176697321401328100 ) ) ;
#68673 = CARTESIAN_POINT ( 'NONE',  ( 0.9908136482939640111, -0.6692913385826771977, 0.1292274648535927661 ) ) ;
#68674 = CARTESIAN_POINT ( 'NONE',  ( 0.1807872349014829905, 1.098494004316914019, -1.883123530778055610 ) ) ;
#68675 = CARTESIAN_POINT ( 'NONE',  ( 0.2821522309711292364, -0.6692913385826771977, 0.1292274648535927661 ) ) ;
#68676 = CARTESIAN_POINT ( 'NONE',  ( 1.161417322834646493, -0.5400638737290844871, 0.3530559997133364547 ) ) ;
#68677 = CARTESIAN_POINT ( 'NONE',  ( 0.5052493438320218022, -0.6692913385826773087, -0.1292274648535924053 ) ) ;
#68678 = CARTESIAN_POINT ( 'NONE',  ( -0.4724409448818896462, -0.1265901696524993070, -0.2801837270341207553 ) ) ;
#68679 = CARTESIAN_POINT ( 'NONE',  ( 0.8398950131233602345, -0.5023911411419708095, 0.1820866141732285504 ) ) ;
#68680 = CARTESIAN_POINT ( 'NONE',  ( 1.279527559055118724, -0.5400638737290845981, -0.3530559997133363437 ) ) ;
#68681 = CARTESIAN_POINT ( 'NONE',  ( 0.05249343832021075018, 0.1283753931104746893, -0.1820866141732285504 ) ) ;
#68682 = CARTESIAN_POINT ( 'NONE',  ( -0.2296587926509179312, -0.05778040916215522460, 0.4822834645669289988 ) ) ;
#68683 = CARTESIAN_POINT ( 'NONE',  ( 0.4790026246719167324, -0.05778040916215522460, 0.4822834645669289988 ) ) ;
#68684 = CARTESIAN_POINT ( 'NONE',  ( -0.6496062992125976043, 0.1660481256975883668, -0.3530559997133364547 ) ) ;
#68685 = CARTESIAN_POINT ( 'NONE',  ( -0.3215223097112853146, -0.2845877964562159024, 0.3641732283464567677 ) ) ;
#68686 = VECTOR ( 'NONE', #80258, 39.37007874015748143 ) ;
#68687 = CARTESIAN_POINT ( 'NONE',  ( 0.6299212598425204535, -0.1870078740157479769, 0.4822834645669291653 ) ) ;
#68688 = CARTESIAN_POINT ( 'NONE',  ( 1.122047244094488860, -0.4536011799217368745, -0.2665933059059886201 ) ) ;
#68689 = CARTESIAN_POINT ( 'NONE',  ( -0.04593175853018302557, 0.2952755905511811885, 0.1292274648535926551 ) ) ;
#68690 = CARTESIAN_POINT ( 'NONE',  ( 0.3129921259842521897, 0.7086614173228346081, 0.000000000000000000 ) ) ;
#68692 = CARTESIAN_POINT ( 'NONE',  ( 1.568241469816273437, -0.3162353388693405765, 0.4822834645669290543 ) ) ;
#68691 = CARTESIAN_POINT ( 'NONE',  ( -1.043307086614172929, 0.1660481256975883391, -0.3530559997133364547 ) ) ;
#68693 = CARTESIAN_POINT ( 'NONE',  ( 0.1049643490035304799, -0.3917322834645669549, -1.967191601049868899 ) ) ;
#68694 = CARTESIAN_POINT ( 'NONE',  ( -1.443569553805773564, 0.2306618581243847221, -0.2411417322834647770 ) ) ;
#68695 = CARTESIAN_POINT ( 'NONE',  ( -0.3608923884514428360, -0.6692913385826773087, -0.1292274648535924053 ) ) ;
#68696 =( BOUNDED_SURFACE ( )  B_SPLINE_SURFACE ( 1, 2, ( 
 ( #39790, #65485, #65052, #58728, #1091, #27155, #7817, #52819, #78530, #20854, #72206, #14559, #27577, #53234, #66304, #57879, #2335, #54486, #74284, #80197, #54904, #35555, #60395, #67551, #80610, #42270, #47756, #15804, #10310, #73454, #41455, #60804, #9468, #61219, #67139, #3573, #47339, #34735, #74702, #34315, #16628, #28822, #35142, #3158, #35975, #29650, #41041, #9063, #67967, #22515, #73872, #29240, #61645, #55312, #48176, #17047, #16212, #41859, #9886, #42688, #22921, #48587, #3986, #81021, #73029, #23333, #49003, #27991, #53651, #79359, #8643, #59976, #21678, #15379, #66726, #2746, #28406, #54064, #79780, #22095, #30061, #4393, #81432, #4800, #11132, #12366, #50642, #69198, #51050, #68787, #56141, #62884, #30477, #5219, #70011, #31711, #75115, #43914, #17460, #69611, #36789, #24970, #62465, #43090, #37612, #19081, #81846, #24158, #49826, #38025, #57371, #63287, #18273, #83066, #11957, #25387, #76751, #75526, #43500, #30883, #82251, #5627, #68385, #76346, #63700, #24570, #36381, #50236, #17866, #31294, #11547, #37203, #10724, #49420, #56550, #75932, #56958, #82655, #18676, #44321, #6039, #62055, #55722, #23747, #27064, #7293, #7723, #71689, #13207, #20340, #33392, #78435, #572, #51889, #46412, #26225, #77593, #13617, #45577, #14040, #19927, #39697, #149, #70856, #27480, #70426, #52723, #64955, #71270, #39271, #72106, #65804, #77167, #45153, #20762, #32963, #26652, #65388, #14464, #8137, #998, #53138, #58630, #52306, #78012, #78849, #45992, #59054, #40116, #33802, #25804, #1408, #59467, #64122, #6457, #32127, #1819, #44730, #12782, #38439, #57785, #51465, #19499, #38854, #64534, #6871, #32540, #58205, #34217, #40946, #47245, #48482, #3472, #22000, #3886, #21582, #8963, #15703, #66625, #41360, #22824, #67869, #27898, #80098, #53559, #22417, #72934, #61121, #15286, #79267, #73776, #55208, #34637, #60301, #2651, #74183, #10207, #16112, #54387, #35875, #48074, #61542, #29546, #28308, #79683, #67041, #35044, #41756, #21176, #29139, #16530, #60709, #72523, #3058, #53970, #67451, #47660, #73355, #46831, #2234, #9373, #28726, #9785, #54805, #35456, #14872, #80509, #42175, #40533, #66212, #8551, #59880, #16944, #48900, #82148, #24053, #11024, #12262, #74601, #42586, #68286, #69094, #49311, #5523, #11442, #43394, #62357, #36278, #56035, #24464, #69908, #44218, #37920, #68682, #63596, #61950, #37098, #42988, #23641, #81327, #36681, #10622, #4290, #29952, #31188, #56853, #82551, #5933, #11856, #17359, #4694, #30368, #81743, #50537, #24869, #50129, #17763, #80916, #75829, #62783, #55617, #75013, #49723, #31603, #56446, #23229, #75420, #5117, #30784, #18170, #43803, #69507, #37509, #63184, #76241, #18575, #6763, #32858, #77485, #57263, #32022, #12676, #76645, #8036, #32435, #82962, #58952, #38335, #39592, #77061, #64010, #52202, #14362, #25280, #52623, #64848, #26959, #18976, #58526, #58098, #1310, #65280, #57682, #7619, #892, #13507, #39163, #44, #463, #19820, #50948, #70747, #44625, #33292, #71167, #64429, #19395, #78328, #26549, #26120, #51781, #7186, #45469, #46313, #70321, #77906, #20237, #45885, #71583, #13934, #38752, #6351, #20659, #72006, #40019, #65707, #25697, #45046, #51358, #13099, #79582, #79168, #59778, #34116, #72834, #53037, #72424, #27375, #41666, #9690, #67357, #22727, #47979, #53460, #47144, #21485, #34536, #3375, #61024, #34951, #53869, #33700, #60614, #73254, #78749, #1719, #40429, #48386, #9280, #16431, #21074, #46732, #8446, #14774, #66110, #2132, #66948, #54286, #35361, #27800, #66527, #2963, #21897, #59360, #15184, #40841, #8858, #67772, #60201, #2552, #29038, #28210, #16020, #47560, #15602, #28629, #74085, #41262, #54709, #80003, #80415, #22316, #73679, #42077, #37419, #18073, #10526, #75733, #68993, #49625, #75318, #68187, #36583, #30270, #61442, #23545, #44126, #43708, #23957, #17263, #29857, #5430, #11343, #42892, #62262, #43296, #4598, #82458, #10110, #55933, #17665, #37003, #62681, #68586, #42483, #69411, #24366, #3789, #11765, #81648, #5023, #30691, #74918, #50036, #29453, #55111, #56354, #82053, #49213, #24773, #80820 ),
 ( #63092, #48803, #36181, #76143, #35772, #31091, #56758, #10927, #50442, #18484, #23135, #61853, #4194, #74501, #16849, #55520, #81228, #71486, #7516, #26020, #52519, #6666, #38653, #32338, #78227, #364, #51679, #13833, #39492, #50854, #64330, #77382, #5833, #31506, #57166, #12997, #45787, #77808, #7087, #44944, #58000, #76554, #19713, #20139, #20560, #82865, #25187, #18882, #6247, #12576, #65179, #52099, #70641, #69818, #70220, #57585, #45372, #31924, #71067, #33184, #58853, #44531, #13411, #38233, #39066, #63911, #26446, #83276, #25599, #64749, #12167, #51262, #76964, #19293, #1210, #26860, #32758, #58425, #37824, #786, #63500, #55736, #53360, #21386, #40738, #61232, #67980, #81444, #3998, #17060, #3586, #14258, #29252, #59675, #10323, #20971, #47041, #36392, #27275, #46630, #72326, #14673, #78649, #52936, #40330, #61657, #54916, #35987, #35569, #39916, #8758, #29662, #80622, #55324, #74296, #66009, #22934, #81033, #23345, #2030, #79070, #15080, #48600, #46212, #16642, #42282, #49016, #42699, #8347, #66422, #74713, #65605, #7936, #33597, #72734, #68396, #10735, #62066, #4405, #30073, #34013, #71907, #59262, #1619, #27696, #43102, #36802, #43511, #49838, #51062, #6050, #24581, #6467, #24169, #11560, #18285, #69211, #43928, #25398, #70436, #30489, #82667, #56154, #24982, #75537, #63710, #17877, #81857, #76358, #57794, #37217, #62896, #5231, #76762, #12793, #18690, #56969, #38449, #50656, #64133, #32137, #30895, #82263, #69624, #37624, #44333, #23759, #31722, #19092, #63300, #75126, #5638, #56562, #70024, #50248, #75944, #49432, #4813, #11969, #31305, #12377, #38035, #57383, #83077, #44741, #17471, #68798, #11143, #62478, #1008, #52733, #26661, #33401, #14052, #58215, #71698, #59063, #78444, #19937, #71279, #46423, #45586, #13628, #7303, #64967, #39706, #39280, #65398, #13217, #581, #59476, #25814, #27074, #58640, #32972, #52315, #72115, #40127, #64544, #6881, #20770, #78022, #20350, #7734, #14473, #65813, #46002, #1829, #1418, #8146, #33811, #27489, #77177, #161, #51474, #19508, #45162, #70867, #38863, #32551, #26235, #51897, #77603, #82525, #77036, #31161, #56828, #44195, #76214, #18952, #24843, #70294, #30760, #18143, #58071, #17737, #57656, #12239, #50510, #18550, #19368, #13069, #24437, #75801, #18, #69885, #57234, #12646, #45018, #38724, #31578, #437, #37895, #63571, #5906, #26092, #82935, #25257, #70718, #64401, #56422, #50921, #76621, #11416, #37071, #62756, #44599, #51332, #25672, #38308, #63982, #6319, #82122, #31996, #6737, #75391, #5092, #50104, #43777, #11833, #69480, #32408, #43366, #69066, #37486, #63160, #5499, #46282, #71556, #71978, #53432, #15153, #58498, #27348, #862, #53006, #52174, #8417, #77877, #26519, #21044, #2524, #45858, #20208, #13905, #21457, #40810, #46703, #1690, #66495, #78719, #8829, #60169, #58923, #26931, #14332, #65680, #72396, #51752, #34085, #47115, #8007, #19790, #33671, #65252, #14746, #39563, #52592, #34506, #32830, #7589, #33261, #1282, #78299, #20631, #39990, #66081, #59333, #40400, #77455, #59748, #2102, #27767, #72804, #45442, #79140, #71138, #13480, #39137, #64818, #7159, #35332, #3344, #22698, #42048, #48773, #36560, #68155, #81203, #67744, #79553, #10077, #41638, #74472, #2936, #29008, #17236, #9251, #28600, #54257, #79973, #60586, #34923, #22286, #42455, #35741, #16819, #16402, #21866, #74055, #10499, #61409, #36153, #55081, #47947, #3758, #61826, #4166, #67329, #60995, #29830, #9662, #54674, #80386, #48357, #80790, #29423, #23105, #66919, #73649, #10902, #53840, #55493, #23518, #49187, #74890, #42866, #68559, #15991, #62237, #28182, #47531, #73222, #15573, #41232, #34279, #65859, #59940, #39332, #53197, #46473, #20403, #79324, #2296, #65018, #21643, #14523, #59523, #40175, #52786, #27956, #7353, #33022, #72580, #8193, #1467, #2709, #58691, #1056, #26710, #1880, #39754, #47303, #27540, #33859, #78495, #52366, #72167, #14928, #60362, #34699, #28370, #59110, #54031, #78073, #78910, #33450, #14102, #71749, #27122, #46055, #65451, #7782, #72993, #53615, #20818, #15346, #21231, #46887, #40587, #66269 ) ),
 .UNSPECIFIED., .F., .F., .F. ) 
 B_SPLINE_SURFACE_WITH_KNOTS ( ( 2, 2 ),
 ( 3, 2, 2, 2, 2, 2, 2, 2, 2, 2, 2, 2, 2, 2, 2, 2, 2, 2, 2, 2, 2, 2, 2, 2, 2, 2, 2, 2, 2, 2, 2, 2, 2, 2, 2, 2, 2, 2, 2, 2, 2, 2, 2, 2, 2, 2, 2, 2, 2, 2, 2, 2, 2, 2, 2, 2, 2, 2, 2, 2, 2, 2, 2, 2, 2, 2, 2, 2, 2, 2, 2, 2, 2, 2, 2, 2, 2, 2, 2, 2, 2, 2, 2, 2, 2, 2, 2, 2, 2, 2, 2, 2, 2, 2, 2, 2, 2, 2, 2, 2, 2, 2, 2, 2, 2, 2, 2, 2, 2, 2, 2, 2, 2, 2, 2, 2, 2, 2, 2, 2, 2, 2, 2, 2, 2, 2, 2, 2, 2, 2, 2, 2, 2, 2, 2, 2, 2, 2, 2, 2, 2, 2, 2, 2, 2, 2, 2, 2, 2, 2, 2, 2, 2, 2, 2, 2, 2, 2, 2, 2, 2, 2, 2, 2, 2, 2, 2, 2, 2, 2, 2, 2, 2, 2, 2, 2, 2, 2, 2, 2, 2, 2, 2, 2, 2, 2, 2, 2, 2, 2, 2, 2, 2, 2, 2, 2, 2, 2, 2, 2, 2, 2, 2, 2, 2, 2, 2, 2, 2, 2, 2, 2, 2, 2, 2, 2, 2, 2, 2, 2, 2, 2, 2, 2, 2, 2, 2, 2, 2, 2, 2, 2, 2, 2, 2, 2, 2, 2, 2, 2, 2, 2, 2, 2, 2, 2, 2, 2, 2, 2, 2, 2, 2, 2, 2, 3 ),
 ( 0.000000000000000000, 1.000000000000000000 ),
 ( 0.000000000000000000, 0.003787878787878787984, 0.007575757575757575968, 0.01136363636363636395, 0.01515151515151515194, 0.01893939393939393992, 0.02272727272727272790, 0.02651515151515151589, 0.03030303030303030387, 0.03409090909090908839, 0.03787878787878787984, 0.04166666666666666435, 0.04545454545454545581, 0.04924242424242424032, 0.05303030303030303177, 0.05681818181818181629, 0.06060606060606060774, 0.06439393939393939226, 0.06818181818181817677, 0.07196969696969697516, 0.07575757575757575968, 0.07954545454545454419, 0.08333333333333332871, 0.08712121212121212710, 0.09090909090909091161, 0.09469696969696969613, 0.09848484848484848064, 0.1022727272727272790, 0.1060606060606060635, 0.1098484848484848481, 0.1136363636363636326, 0.1174242424242424310, 0.1212121212121212155, 0.1250000000000000000, 0.1287878787878787845, 0.1325757575757575690, 0.1363636363636363535, 0.1401515151515151381, 0.1439393939393939503, 0.1477272727272727348, 0.1515151515151515194, 0.1553030303030303039, 0.1590909090909090884, 0.1628787878787878729, 0.1666666666666666574, 0.1704545454545454419, 0.1742424242424242542, 0.1780303030303030387, 0.1818181818181818232, 0.1856060606060606077, 0.1893939393939393923, 0.1931818181818181768, 0.1969696969696969613, 0.2007575757575757458, 0.2045454545454545581, 0.2083333333333333426, 0.2121212121212121271, 0.2159090909090909116, 0.2196969696969696961, 0.2234848484848484806, 0.2272727272727272652, 0.2310606060606060497, 0.2348484848484848619, 0.2386363636363636465, 0.2424242424242424310, 0.2462121212121212155, 0.2500000000000000000, 0.2537878787878787845, 0.2575757575757575690, 0.2613636363636363535, 0.2651515151515151381, 0.2689393939393939226, 0.2727272727272727071, 0.2765151515151514916, 0.2803030303030302761, 0.2840909090909091161, 0.2878787878787879007, 0.2916666666666666852, 0.2954545454545454697, 0.2992424242424242542, 0.3030303030303030387, 0.3068181818181818232, 0.3106060606060606077, 0.3143939393939393923, 0.3181818181818181768, 0.3219696969696969613, 0.3257575757575757458, 0.3295454545454545303, 0.3333333333333333148, 0.3371212121212120993, 0.3409090909090908839, 0.3446969696969697239, 0.3484848484848485084, 0.3522727272727272929, 0.3560606060606060774, 0.3598484848484848619, 0.3636363636363636465, 0.3674242424242424310, 0.3712121212121212155, 0.3750000000000000000, 0.3787878787878787845, 0.3825757575757575690, 0.3863636363636363535, 0.3901515151515151381, 0.3939393939393939226, 0.3977272727272727071, 0.4015151515151514916, 0.4053030303030302761, 0.4090909090909091161, 0.4128787878787879007, 0.4166666666666666852, 0.4204545454545454697, 0.4242424242424242542, 0.4280303030303030387, 0.4318181818181818232, 0.4356060606060606077, 0.4393939393939393923, 0.4431818181818181768, 0.4469696969696969613, 0.4507575757575757458, 0.4545454545454545303, 0.4583333333333333148, 0.4621212121212120993, 0.4659090909090908839, 0.4696969696969697239, 0.4734848484848485084, 0.4772727272727272929, 0.4810606060606060774, 0.4848484848484848619, 0.4886363636363636465, 0.4924242424242424310, 0.4962121212121212155, 0.5000000000000000000, 0.5037878787878787845, 0.5075757575757575690, 0.5113636363636363535, 0.5151515151515151381, 0.5189393939393939226, 0.5227272727272727071, 0.5265151515151514916, 0.5303030303030302761, 0.5340909090909090606, 0.5378787878787878451, 0.5416666666666666297, 0.5454545454545454142, 0.5492424242424241987, 0.5530303030303029832, 0.5568181818181817677, 0.5606060606060605522, 0.5643939393939394478, 0.5681818181818182323, 0.5719696969696970168, 0.5757575757575758013, 0.5795454545454545858, 0.5833333333333333703, 0.5871212121212121549, 0.5909090909090909394, 0.5946969696969697239, 0.5984848484848485084, 0.6022727272727272929, 0.6060606060606060774, 0.6098484848484848619, 0.6136363636363636465, 0.6174242424242424310, 0.6212121212121212155, 0.6250000000000000000, 0.6287878787878787845, 0.6325757575757575690, 0.6363636363636363535, 0.6401515151515151381, 0.6439393939393939226, 0.6477272727272727071, 0.6515151515151514916, 0.6553030303030302761, 0.6590909090909090606, 0.6628787878787878451, 0.6666666666666666297, 0.6704545454545454142, 0.6742424242424241987, 0.6780303030303029832, 0.6818181818181817677, 0.6856060606060605522, 0.6893939393939394478, 0.6931818181818182323, 0.6969696969696970168, 0.7007575757575758013, 0.7045454545454545858, 0.7083333333333333703, 0.7121212121212121549, 0.7159090909090909394, 0.7196969696969697239, 0.7234848484848485084, 0.7272727272727272929, 0.7310606060606060774, 0.7348484848484848619, 0.7386363636363636465, 0.7424242424242424310, 0.7462121212121212155, 0.7500000000000000000, 0.7537878787878787845, 0.7575757575757575690, 0.7613636363636363535, 0.7651515151515151381, 0.7689393939393939226, 0.7727272727272727071, 0.7765151515151514916, 0.7803030303030302761, 0.7840909090909090606, 0.7878787878787878451, 0.7916666666666666297, 0.7954545454545454142, 0.7992424242424241987, 0.8030303030303029832, 0.8068181818181817677, 0.8106060606060605522, 0.8143939393939394478, 0.8181818181818182323, 0.8219696969696970168, 0.8257575757575758013, 0.8295454545454545858, 0.8333333333333333703, 0.8371212121212121549, 0.8409090909090909394, 0.8446969696969697239, 0.8484848484848485084, 0.8522727272727272929, 0.8560606060606060774, 0.8598484848484848619, 0.8636363636363636465, 0.8674242424242424310, 0.8712121212121212155, 0.8750000000000000000, 0.8787878787878787845, 0.8825757575757575690, 0.8863636363636363535, 0.8901515151515151381, 0.8939393939393939226, 0.8977272727272727071, 0.9015151515151514916, 0.9053030303030302761, 0.9090909090909090606, 0.9128787878787878451, 0.9166666666666666297, 0.9204545454545454142, 0.9242424242424241987, 0.9280303030303029832, 0.9318181818181817677, 0.9356060606060605522, 0.9393939393939394478, 0.9431818181818182323, 0.9469696969696970168, 0.9507575757575758013, 0.9545454545454545858, 0.9583333333333333703, 0.9621212121212121549, 0.9659090909090909394 ),
 .UNSPECIFIED. ) 
 GEOMETRIC_REPRESENTATION_ITEM ( )  RATIONAL_B_SPLINE_SURFACE ( (
 ( 1.000000000000000000, 0.9659258262890683122, 1.000000000000000000, 0.9659258262890683122, 1.000000000000000000, 0.9659258262890683122, 1.000000000000000000, 0.9659258262890683122, 1.000000000000000000, 0.9659258262890683122, 1.000000000000000000, 0.9659258262890683122, 1.000000000000000000, 0.9659258262890683122, 1.000000000000000000, 0.9659258262890683122, 1.000000000000000000, 0.9659258262890683122, 1.000000000000000000, 0.9659258262890683122, 1.000000000000000000, 0.9659258262890683122, 1.000000000000000000, 0.9659258262890683122, 1.000000000000000000, 0.9659258262890683122, 1.000000000000000000, 0.9659258262890683122, 1.000000000000000000, 0.9659258262890683122, 1.000000000000000000, 0.9659258262890683122, 1.000000000000000000, 0.9659258262890683122, 1.000000000000000000, 0.9659258262890683122, 1.000000000000000000, 0.9659258262890683122, 1.000000000000000000, 0.9659258262890683122, 1.000000000000000000, 0.9659258262890683122, 1.000000000000000000, 0.9659258262890683122, 1.000000000000000000, 0.9659258262890683122, 1.000000000000000000, 0.9659258262890683122, 1.000000000000000000, 0.9659258262890683122, 1.000000000000000000, 0.9659258262890683122, 1.000000000000000000, 0.9659258262890683122, 1.000000000000000000, 0.9659258262890683122, 1.000000000000000000, 0.9659258262890683122, 1.000000000000000000, 0.9659258262890683122, 1.000000000000000000, 0.9659258262890683122, 1.000000000000000000, 0.9659258262890683122, 1.000000000000000000, 0.9659258262890683122, 1.000000000000000000, 0.9659258262890683122, 1.000000000000000000, 0.9659258262890683122, 1.000000000000000000, 0.9659258262890683122, 1.000000000000000000, 0.9659258262890683122, 1.000000000000000000, 0.9659258262890683122, 1.000000000000000000, 0.9659258262890683122, 1.000000000000000000, 0.9659258262890683122, 1.000000000000000000, 0.9659258262890683122, 1.000000000000000000, 0.9659258262890683122, 1.000000000000000000, 0.9659258262890683122, 1.000000000000000000, 0.9659258262890683122, 1.000000000000000000, 0.9659258262890683122, 1.000000000000000000, 0.9659258262890683122, 1.000000000000000000, 0.9659258262890683122, 1.000000000000000000, 0.9659258262890683122, 1.000000000000000000, 0.9659258262890683122, 1.000000000000000000, 0.9659258262890683122, 1.000000000000000000, 0.9659258262890683122, 1.000000000000000000, 0.9659258262890683122, 1.000000000000000000, 0.9659258262890683122, 1.000000000000000000, 0.9659258262890683122, 1.000000000000000000, 0.9659258262890683122, 1.000000000000000000, 0.9659258262890683122, 1.000000000000000000, 0.9659258262890683122, 1.000000000000000000, 0.9659258262890683122, 1.000000000000000000, 0.9659258262890683122, 1.000000000000000000, 0.9659258262890683122, 1.000000000000000000, 0.9659258262890683122, 1.000000000000000000, 0.9659258262890683122, 1.000000000000000000, 0.9659258262890683122, 1.000000000000000000, 0.9659258262890683122, 1.000000000000000000, 0.9659258262890683122, 1.000000000000000000, 0.9659258262890683122, 1.000000000000000000, 0.9659258262890683122, 1.000000000000000000, 0.9659258262890683122, 1.000000000000000000, 0.9659258262890683122, 1.000000000000000000, 0.9659258262890683122, 1.000000000000000000, 0.9659258262890683122, 1.000000000000000000, 0.9659258262890683122, 1.000000000000000000, 0.9659258262890683122, 1.000000000000000000, 0.9659258262890683122, 1.000000000000000000, 0.9659258262890683122, 1.000000000000000000, 0.9659258262890683122, 1.000000000000000000, 0.9659258262890683122, 1.000000000000000000, 0.9659258262890683122, 1.000000000000000000, 0.9659258262890683122, 1.000000000000000000, 0.9659258262890683122, 1.000000000000000000, 0.9659258262890683122, 1.000000000000000000, 0.9659258262890683122, 1.000000000000000000, 0.9659258262890683122, 1.000000000000000000, 0.9659258262890683122, 1.000000000000000000, 0.9659258262890683122, 1.000000000000000000, 0.9659258262890683122, 1.000000000000000000, 0.9659258262890683122, 1.000000000000000000, 0.9659258262890683122, 1.000000000000000000, 0.9659258262890683122, 1.000000000000000000, 0.9659258262890683122, 1.000000000000000000, 0.9659258262890683122, 1.000000000000000000, 0.9659258262890683122, 1.000000000000000000, 0.9659258262890683122, 1.000000000000000000, 0.9659258262890683122, 1.000000000000000000, 0.9659258262890683122, 1.000000000000000000, 0.9659258262890683122, 1.000000000000000000, 0.9659258262890683122, 1.000000000000000000, 0.9659258262890683122, 1.000000000000000000, 0.9659258262890683122, 1.000000000000000000, 0.9659258262890683122, 1.000000000000000000, 0.9659258262890683122, 1.000000000000000000, 0.9659258262890683122, 1.000000000000000000, 0.9659258262890683122, 1.000000000000000000, 0.9659258262890683122, 1.000000000000000000, 0.9659258262890683122, 1.000000000000000000, 0.9659258262890683122, 1.000000000000000000, 0.9659258262890683122, 1.000000000000000000, 0.9659258262890683122, 1.000000000000000000, 0.9659258262890683122, 1.000000000000000000, 0.9659258262890683122, 1.000000000000000000, 0.9659258262890683122, 1.000000000000000000, 0.9659258262890683122, 1.000000000000000000, 0.9659258262890683122, 1.000000000000000000, 0.9659258262890683122, 1.000000000000000000, 0.9659258262890683122, 1.000000000000000000, 0.9659258262890683122, 1.000000000000000000, 0.9659258262890683122, 1.000000000000000000, 0.9659258262890683122, 1.000000000000000000, 0.9659258262890683122, 1.000000000000000000, 0.9659258262890683122, 1.000000000000000000, 0.9659258262890683122, 1.000000000000000000, 0.9659258262890683122, 1.000000000000000000, 0.9659258262890683122, 1.000000000000000000, 0.9659258262890683122, 1.000000000000000000, 0.9659258262890683122, 1.000000000000000000, 0.9659258262890683122, 1.000000000000000000, 0.9659258262890683122, 1.000000000000000000, 0.9659258262890683122, 1.000000000000000000, 0.9659258262890683122, 1.000000000000000000, 0.9659258262890683122, 1.000000000000000000, 0.9659258262890683122, 1.000000000000000000, 0.9659258262890683122, 1.000000000000000000, 0.9659258262890683122, 1.000000000000000000, 0.9659258262890683122, 1.000000000000000000, 0.9659258262890683122, 1.000000000000000000, 0.9659258262890683122, 1.000000000000000000, 0.9659258262890683122, 1.000000000000000000, 0.9659258262890683122, 1.000000000000000000, 0.9659258262890683122, 1.000000000000000000, 0.9659258262890683122, 1.000000000000000000, 0.9659258262890683122, 1.000000000000000000, 0.9659258262890683122, 1.000000000000000000, 0.9659258262890683122, 1.000000000000000000, 0.9659258262890683122, 1.000000000000000000, 0.9659258262890683122, 1.000000000000000000, 0.9659258262890683122, 1.000000000000000000, 0.9659258262890683122, 1.000000000000000000, 0.9659258262890683122, 1.000000000000000000, 0.9659258262890683122, 1.000000000000000000, 0.9659258262890683122, 1.000000000000000000, 0.9659258262890683122, 1.000000000000000000, 0.9659258262890683122, 1.000000000000000000, 0.9659258262890683122, 1.000000000000000000, 0.9659258262890683122, 1.000000000000000000, 0.9659258262890683122, 1.000000000000000000, 0.9659258262890683122, 1.000000000000000000, 0.9659258262890683122, 1.000000000000000000, 0.9659258262890683122, 1.000000000000000000, 0.9659258262890683122, 1.000000000000000000, 0.9659258262890683122, 1.000000000000000000, 0.9659258262890683122, 1.000000000000000000, 0.9659258262890683122, 1.000000000000000000, 0.9659258262890683122, 1.000000000000000000, 0.9659258262890683122, 1.000000000000000000, 0.9659258262890683122, 1.000000000000000000, 0.9659258262890683122, 1.000000000000000000, 0.9659258262890683122, 1.000000000000000000, 0.9659258262890683122, 1.000000000000000000, 0.9659258262890683122, 1.000000000000000000, 0.9659258262890683122, 1.000000000000000000, 0.9659258262890683122, 1.000000000000000000, 0.9659258262890683122, 1.000000000000000000, 0.9659258262890683122, 1.000000000000000000, 0.9659258262890683122, 1.000000000000000000, 0.9659258262890683122, 1.000000000000000000, 0.9659258262890683122, 1.000000000000000000, 0.9659258262890683122, 1.000000000000000000, 0.9659258262890683122, 1.000000000000000000, 0.9659258262890683122, 1.000000000000000000, 0.9659258262890683122, 1.000000000000000000, 0.9659258262890683122, 1.000000000000000000, 0.9659258262890683122, 1.000000000000000000, 0.9659258262890683122, 1.000000000000000000, 0.9659258262890683122, 1.000000000000000000, 0.9659258262890683122, 1.000000000000000000, 0.9659258262890683122, 1.000000000000000000, 0.9659258262890683122, 1.000000000000000000, 0.9659258262890683122, 1.000000000000000000, 0.9659258262890683122, 1.000000000000000000, 0.9659258262890683122, 1.000000000000000000, 0.9659258262890683122, 1.000000000000000000, 0.9659258262890683122, 1.000000000000000000, 0.9659258262890683122, 1.000000000000000000, 0.9659258262890683122, 1.000000000000000000, 0.9659258262890683122, 1.000000000000000000, 0.9659258262890683122, 1.000000000000000000, 0.9659258262890683122, 1.000000000000000000, 0.9659258262890683122, 1.000000000000000000, 0.9659258262890683122, 1.000000000000000000, 0.9659258262890683122, 1.000000000000000000, 0.9659258262890683122, 1.000000000000000000, 0.9659258262890683122, 1.000000000000000000, 0.9659258262890683122, 1.000000000000000000, 0.9659258262890683122, 1.000000000000000000, 0.9659258262890683122, 1.000000000000000000, 0.9659258262890683122, 1.000000000000000000, 0.9659258262890683122, 1.000000000000000000, 0.9659258262890683122, 1.000000000000000000, 0.9659258262890683122, 1.000000000000000000, 0.9659258262890683122, 1.000000000000000000, 0.9659258262890683122, 1.000000000000000000, 0.9659258262890683122, 1.000000000000000000, 0.9659258262890683122, 1.000000000000000000, 0.9659258262890683122, 1.000000000000000000, 0.9659258262890683122, 1.000000000000000000, 0.9659258262890683122, 1.000000000000000000, 0.9659258262890683122, 1.000000000000000000, 0.9659258262890683122, 1.000000000000000000, 0.9659258262890683122, 1.000000000000000000, 0.9659258262890683122, 1.000000000000000000, 0.9659258262890683122, 1.000000000000000000, 0.9659258262890683122, 1.000000000000000000, 0.9659258262890683122, 1.000000000000000000, 0.9659258262890683122, 1.000000000000000000, 0.9659258262890683122, 1.000000000000000000, 0.9659258262890683122, 1.000000000000000000, 0.9659258262890683122, 1.000000000000000000, 0.9659258262890683122, 1.000000000000000000, 0.9659258262890683122, 1.000000000000000000, 0.9659258262890683122, 1.000000000000000000, 0.9659258262890683122, 1.000000000000000000, 0.9659258262890683122, 1.000000000000000000, 0.9659258262890683122, 1.000000000000000000, 0.9659258262890683122, 1.000000000000000000, 0.9659258262890683122, 1.000000000000000000, 0.9659258262890683122, 1.000000000000000000, 0.9659258262890683122, 1.000000000000000000, 0.9659258262890683122, 1.000000000000000000, 0.9659258262890683122, 1.000000000000000000, 0.9659258262890683122, 1.000000000000000000, 0.9659258262890683122, 1.000000000000000000, 0.9659258262890683122, 1.000000000000000000, 0.9659258262890683122, 1.000000000000000000, 0.9659258262890683122, 1.000000000000000000, 0.9659258262890683122, 1.000000000000000000, 0.9659258262890683122, 1.000000000000000000, 0.9659258262890683122, 1.000000000000000000, 0.9659258262890683122, 1.000000000000000000, 0.9659258262890683122, 1.000000000000000000, 0.9659258262890683122, 1.000000000000000000, 0.9659258262890683122, 1.000000000000000000, 0.9659258262890683122, 1.000000000000000000, 0.9659258262890683122, 1.000000000000000000, 0.9659258262890683122, 1.000000000000000000, 0.9659258262890683122, 1.000000000000000000),
 ( 1.000000000000000000, 0.9659258262890683122, 1.000000000000000000, 0.9659258262890683122, 1.000000000000000000, 0.9659258262890683122, 1.000000000000000000, 0.9659258262890683122, 1.000000000000000000, 0.9659258262890683122, 1.000000000000000000, 0.9659258262890683122, 1.000000000000000000, 0.9659258262890683122, 1.000000000000000000, 0.9659258262890683122, 1.000000000000000000, 0.9659258262890683122, 1.000000000000000000, 0.9659258262890683122, 1.000000000000000000, 0.9659258262890683122, 1.000000000000000000, 0.9659258262890683122, 1.000000000000000000, 0.9659258262890683122, 1.000000000000000000, 0.9659258262890683122, 1.000000000000000000, 0.9659258262890683122, 1.000000000000000000, 0.9659258262890683122, 1.000000000000000000, 0.9659258262890683122, 1.000000000000000000, 0.9659258262890683122, 1.000000000000000000, 0.9659258262890683122, 1.000000000000000000, 0.9659258262890683122, 1.000000000000000000, 0.9659258262890683122, 1.000000000000000000, 0.9659258262890683122, 1.000000000000000000, 0.9659258262890683122, 1.000000000000000000, 0.9659258262890683122, 1.000000000000000000, 0.9659258262890683122, 1.000000000000000000, 0.9659258262890683122, 1.000000000000000000, 0.9659258262890683122, 1.000000000000000000, 0.9659258262890683122, 1.000000000000000000, 0.9659258262890683122, 1.000000000000000000, 0.9659258262890683122, 1.000000000000000000, 0.9659258262890683122, 1.000000000000000000, 0.9659258262890683122, 1.000000000000000000, 0.9659258262890683122, 1.000000000000000000, 0.9659258262890683122, 1.000000000000000000, 0.9659258262890683122, 1.000000000000000000, 0.9659258262890683122, 1.000000000000000000, 0.9659258262890683122, 1.000000000000000000, 0.9659258262890683122, 1.000000000000000000, 0.9659258262890683122, 1.000000000000000000, 0.9659258262890683122, 1.000000000000000000, 0.9659258262890683122, 1.000000000000000000, 0.9659258262890683122, 1.000000000000000000, 0.9659258262890683122, 1.000000000000000000, 0.9659258262890683122, 1.000000000000000000, 0.9659258262890683122, 1.000000000000000000, 0.9659258262890683122, 1.000000000000000000, 0.9659258262890683122, 1.000000000000000000, 0.9659258262890683122, 1.000000000000000000, 0.9659258262890683122, 1.000000000000000000, 0.9659258262890683122, 1.000000000000000000, 0.9659258262890683122, 1.000000000000000000, 0.9659258262890683122, 1.000000000000000000, 0.9659258262890683122, 1.000000000000000000, 0.9659258262890683122, 1.000000000000000000, 0.9659258262890683122, 1.000000000000000000, 0.9659258262890683122, 1.000000000000000000, 0.9659258262890683122, 1.000000000000000000, 0.9659258262890683122, 1.000000000000000000, 0.9659258262890683122, 1.000000000000000000, 0.9659258262890683122, 1.000000000000000000, 0.9659258262890683122, 1.000000000000000000, 0.9659258262890683122, 1.000000000000000000, 0.9659258262890683122, 1.000000000000000000, 0.9659258262890683122, 1.000000000000000000, 0.9659258262890683122, 1.000000000000000000, 0.9659258262890683122, 1.000000000000000000, 0.9659258262890683122, 1.000000000000000000, 0.9659258262890683122, 1.000000000000000000, 0.9659258262890683122, 1.000000000000000000, 0.9659258262890683122, 1.000000000000000000, 0.9659258262890683122, 1.000000000000000000, 0.9659258262890683122, 1.000000000000000000, 0.9659258262890683122, 1.000000000000000000, 0.9659258262890683122, 1.000000000000000000, 0.9659258262890683122, 1.000000000000000000, 0.9659258262890683122, 1.000000000000000000, 0.9659258262890683122, 1.000000000000000000, 0.9659258262890683122, 1.000000000000000000, 0.9659258262890683122, 1.000000000000000000, 0.9659258262890683122, 1.000000000000000000, 0.9659258262890683122, 1.000000000000000000, 0.9659258262890683122, 1.000000000000000000, 0.9659258262890683122, 1.000000000000000000, 0.9659258262890683122, 1.000000000000000000, 0.9659258262890683122, 1.000000000000000000, 0.9659258262890683122, 1.000000000000000000, 0.9659258262890683122, 1.000000000000000000, 0.9659258262890683122, 1.000000000000000000, 0.9659258262890683122, 1.000000000000000000, 0.9659258262890683122, 1.000000000000000000, 0.9659258262890683122, 1.000000000000000000, 0.9659258262890683122, 1.000000000000000000, 0.9659258262890683122, 1.000000000000000000, 0.9659258262890683122, 1.000000000000000000, 0.9659258262890683122, 1.000000000000000000, 0.9659258262890683122, 1.000000000000000000, 0.9659258262890683122, 1.000000000000000000, 0.9659258262890683122, 1.000000000000000000, 0.9659258262890683122, 1.000000000000000000, 0.9659258262890683122, 1.000000000000000000, 0.9659258262890683122, 1.000000000000000000, 0.9659258262890683122, 1.000000000000000000, 0.9659258262890683122, 1.000000000000000000, 0.9659258262890683122, 1.000000000000000000, 0.9659258262890683122, 1.000000000000000000, 0.9659258262890683122, 1.000000000000000000, 0.9659258262890683122, 1.000000000000000000, 0.9659258262890683122, 1.000000000000000000, 0.9659258262890683122, 1.000000000000000000, 0.9659258262890683122, 1.000000000000000000, 0.9659258262890683122, 1.000000000000000000, 0.9659258262890683122, 1.000000000000000000, 0.9659258262890683122, 1.000000000000000000, 0.9659258262890683122, 1.000000000000000000, 0.9659258262890683122, 1.000000000000000000, 0.9659258262890683122, 1.000000000000000000, 0.9659258262890683122, 1.000000000000000000, 0.9659258262890683122, 1.000000000000000000, 0.9659258262890683122, 1.000000000000000000, 0.9659258262890683122, 1.000000000000000000, 0.9659258262890683122, 1.000000000000000000, 0.9659258262890683122, 1.000000000000000000, 0.9659258262890683122, 1.000000000000000000, 0.9659258262890683122, 1.000000000000000000, 0.9659258262890683122, 1.000000000000000000, 0.9659258262890683122, 1.000000000000000000, 0.9659258262890683122, 1.000000000000000000, 0.9659258262890683122, 1.000000000000000000, 0.9659258262890683122, 1.000000000000000000, 0.9659258262890683122, 1.000000000000000000, 0.9659258262890683122, 1.000000000000000000, 0.9659258262890683122, 1.000000000000000000, 0.9659258262890683122, 1.000000000000000000, 0.9659258262890683122, 1.000000000000000000, 0.9659258262890683122, 1.000000000000000000, 0.9659258262890683122, 1.000000000000000000, 0.9659258262890683122, 1.000000000000000000, 0.9659258262890683122, 1.000000000000000000, 0.9659258262890683122, 1.000000000000000000, 0.9659258262890683122, 1.000000000000000000, 0.9659258262890683122, 1.000000000000000000, 0.9659258262890683122, 1.000000000000000000, 0.9659258262890683122, 1.000000000000000000, 0.9659258262890683122, 1.000000000000000000, 0.9659258262890683122, 1.000000000000000000, 0.9659258262890683122, 1.000000000000000000, 0.9659258262890683122, 1.000000000000000000, 0.9659258262890683122, 1.000000000000000000, 0.9659258262890683122, 1.000000000000000000, 0.9659258262890683122, 1.000000000000000000, 0.9659258262890683122, 1.000000000000000000, 0.9659258262890683122, 1.000000000000000000, 0.9659258262890683122, 1.000000000000000000, 0.9659258262890683122, 1.000000000000000000, 0.9659258262890683122, 1.000000000000000000, 0.9659258262890683122, 1.000000000000000000, 0.9659258262890683122, 1.000000000000000000, 0.9659258262890683122, 1.000000000000000000, 0.9659258262890683122, 1.000000000000000000, 0.9659258262890683122, 1.000000000000000000, 0.9659258262890683122, 1.000000000000000000, 0.9659258262890683122, 1.000000000000000000, 0.9659258262890683122, 1.000000000000000000, 0.9659258262890683122, 1.000000000000000000, 0.9659258262890683122, 1.000000000000000000, 0.9659258262890683122, 1.000000000000000000, 0.9659258262890683122, 1.000000000000000000, 0.9659258262890683122, 1.000000000000000000, 0.9659258262890683122, 1.000000000000000000, 0.9659258262890683122, 1.000000000000000000, 0.9659258262890683122, 1.000000000000000000, 0.9659258262890683122, 1.000000000000000000, 0.9659258262890683122, 1.000000000000000000, 0.9659258262890683122, 1.000000000000000000, 0.9659258262890683122, 1.000000000000000000, 0.9659258262890683122, 1.000000000000000000, 0.9659258262890683122, 1.000000000000000000, 0.9659258262890683122, 1.000000000000000000, 0.9659258262890683122, 1.000000000000000000, 0.9659258262890683122, 1.000000000000000000, 0.9659258262890683122, 1.000000000000000000, 0.9659258262890683122, 1.000000000000000000, 0.9659258262890683122, 1.000000000000000000, 0.9659258262890683122, 1.000000000000000000, 0.9659258262890683122, 1.000000000000000000, 0.9659258262890683122, 1.000000000000000000, 0.9659258262890683122, 1.000000000000000000, 0.9659258262890683122, 1.000000000000000000, 0.9659258262890683122, 1.000000000000000000, 0.9659258262890683122, 1.000000000000000000, 0.9659258262890683122, 1.000000000000000000, 0.9659258262890683122, 1.000000000000000000, 0.9659258262890683122, 1.000000000000000000, 0.9659258262890683122, 1.000000000000000000, 0.9659258262890683122, 1.000000000000000000, 0.9659258262890683122, 1.000000000000000000, 0.9659258262890683122, 1.000000000000000000, 0.9659258262890683122, 1.000000000000000000, 0.9659258262890683122, 1.000000000000000000, 0.9659258262890683122, 1.000000000000000000, 0.9659258262890683122, 1.000000000000000000, 0.9659258262890683122, 1.000000000000000000, 0.9659258262890683122, 1.000000000000000000, 0.9659258262890683122, 1.000000000000000000, 0.9659258262890683122, 1.000000000000000000, 0.9659258262890683122, 1.000000000000000000, 0.9659258262890683122, 1.000000000000000000, 0.9659258262890683122, 1.000000000000000000, 0.9659258262890683122, 1.000000000000000000, 0.9659258262890683122, 1.000000000000000000, 0.9659258262890683122, 1.000000000000000000, 0.9659258262890683122, 1.000000000000000000, 0.9659258262890683122, 1.000000000000000000, 0.9659258262890683122, 1.000000000000000000, 0.9659258262890683122, 1.000000000000000000, 0.9659258262890683122, 1.000000000000000000, 0.9659258262890683122, 1.000000000000000000, 0.9659258262890683122, 1.000000000000000000, 0.9659258262890683122, 1.000000000000000000, 0.9659258262890683122, 1.000000000000000000, 0.9659258262890683122, 1.000000000000000000, 0.9659258262890683122, 1.000000000000000000, 0.9659258262890683122, 1.000000000000000000, 0.9659258262890683122, 1.000000000000000000, 0.9659258262890683122, 1.000000000000000000, 0.9659258262890683122, 1.000000000000000000, 0.9659258262890683122, 1.000000000000000000, 0.9659258262890683122, 1.000000000000000000, 0.9659258262890683122, 1.000000000000000000, 0.9659258262890683122, 1.000000000000000000, 0.9659258262890683122, 1.000000000000000000, 0.9659258262890683122, 1.000000000000000000, 0.9659258262890683122, 1.000000000000000000, 0.9659258262890683122, 1.000000000000000000, 0.9659258262890683122, 1.000000000000000000, 0.9659258262890683122, 1.000000000000000000, 0.9659258262890683122, 1.000000000000000000, 0.9659258262890683122, 1.000000000000000000, 0.9659258262890683122, 1.000000000000000000, 0.9659258262890683122, 1.000000000000000000, 0.9659258262890683122, 1.000000000000000000, 0.9659258262890683122, 1.000000000000000000, 0.9659258262890683122, 1.000000000000000000, 0.9659258262890683122, 1.000000000000000000, 0.9659258262890683122, 1.000000000000000000, 0.9659258262890683122, 1.000000000000000000, 0.9659258262890683122, 1.000000000000000000, 0.9659258262890683122, 1.000000000000000000, 0.9659258262890683122, 1.000000000000000000, 0.9659258262890683122, 1.000000000000000000, 0.9659258262890683122, 1.000000000000000000, 0.9659258262890683122, 1.000000000000000000, 0.9659258262890683122, 1.000000000000000000, 0.9659258262890683122, 1.000000000000000000, 0.9659258262890683122, 1.000000000000000000) ) ) 
 REPRESENTATION_ITEM ( '' )  SURFACE ( )  );
#68697 = CARTESIAN_POINT ( 'NONE',  ( -0.4724409448818899238, 0.1265901696524986686, -0.3477690288713909950 ) ) ;
#68698 = CARTESIAN_POINT ( 'NONE',  ( -0.3949938075777409408, -0.1058382717557502933, -2.565616797900262647 ) ) ;
#68699 = ORIENTED_EDGE ( 'NONE', *, *, #50172, .T. ) ;
#68700 = CARTESIAN_POINT ( 'NONE',  ( 0.2230971128608932319, -0.3690944881889763329, 0.3153832671262228327 ) ) ;
#68701 = CARTESIAN_POINT ( 'NONE',  ( -0.3392501089628019995, 0.1958661417322832277, -1.435695538057742970 ) ) ;
#68702 = CARTESIAN_POINT ( 'NONE',  ( 0.5577427821522314977, -0.3162353388693409650, -0.4822834645669289433 ) ) ;
#68703 = CARTESIAN_POINT ( 'NONE',  ( 0.4724409448818897572, -0.1265901696524988906, -2.631233595800525293 ) ) ;
#68704 = CARTESIAN_POINT ( 'NONE',  ( 0.000000000000000000, 0.000000000000000000, -1.929133858267716661 ) ) ;
#68706 = AXIS2_PLACEMENT_3D ( 'NONE', #54774, #23609, #40909 ) ;
#68705 = CARTESIAN_POINT ( 'NONE',  ( -1.732283464566928277, -0.1870078740157479769, 0.3641732283464567677 ) ) ;
#68707 = CARTESIAN_POINT ( 'NONE',  ( 1.227034120734908917, 0.2952755905511810774, -0.1292274648535930714 ) ) ;
#68708 = CARTESIAN_POINT ( 'NONE',  ( 1.154855643044620184, 0.1283753931104746893, -0.1820866141732285504 ) ) ;
#68709 = CARTESIAN_POINT ( 'NONE',  ( 0.02624671916010564918, -0.6046776061558809534, -0.2411417322834644161 ) ) ;
#68710 = CARTESIAN_POINT ( 'NONE',  ( 0.1958661417322836162, -0.3392501089628018329, -0.6443376395987383543 ) ) ;
#68711 = CARTESIAN_POINT ( 'NONE',  ( -0.3543307086614165824, 0.2952755905511811885, 0.000000000000000000 ) ) ;
#68712 = CARTESIAN_POINT ( 'NONE',  ( -1.017060367454067249, -0.2845877964562161244, -0.3641732283464567121 ) ) ;
#68713 = CARTESIAN_POINT ( 'NONE',  ( 0.2427821522309716595, -0.3162353388693409650, -0.4822834645669289433 ) ) ;
#68714 = CARTESIAN_POINT ( 'NONE',  ( 0.1377952755905518800, -0.5400638737290844871, 0.3530559997133364547 ) ) ;
#68715 = CARTESIAN_POINT ( 'NONE',  ( -1.193035393573954606, -4.754953748228849300E-15, -0.3627989612356167792 ) ) ;
#68716 = CARTESIAN_POINT ( 'NONE',  ( 6.265965269058076312E-17, 1.062992125984252745, -1.850393700787401619 ) ) ;
#68717 = CARTESIAN_POINT ( 'NONE',  ( -0.3917322834645670659, -7.196005306013484475E-17, -1.925872334154542509 ) ) ;
#68718 = CARTESIAN_POINT ( 'NONE',  ( 0.3018372703412079971, 0.05413385826771626580, -0.4176697321401330321 ) ) ;
#68719 = CARTESIAN_POINT ( 'NONE',  ( -0.4527559055118102749, 0.1660481256975885056, 0.3530559997133364547 ) ) ;
#68720 = CARTESIAN_POINT ( 'NONE',  ( -1.417322834645668772, -0.1870078740157480879, -0.4822834645669291653 ) ) ;
#68721 = EDGE_CURVE ( 'NONE', #32199, #58583, #13072, .T. ) ;
#68722 = CARTESIAN_POINT ( 'NONE',  ( 1.207349081364829990, -0.6046776061558809534, -0.2411417322834644161 ) ) ;
#68723 = CARTESIAN_POINT ( 'NONE',  ( 0.4921259842519691285, -0.5400638737290845981, -0.3530559997133363437 ) ) ;
#68724 = CARTESIAN_POINT ( 'NONE',  ( 0.1958661417322834775, 0.3392501089628018884, -1.016404199475065662 ) ) ;
#68725 = CARTESIAN_POINT ( 'NONE',  ( -0.9383202099737524282, -0.05778040916215522460, 0.4822834645669289988 ) ) ;
#68726 = CARTESIAN_POINT ( 'NONE',  ( 0.1509186351706045259, -0.05778040916215560624, -0.4822834645669293319 ) ) ;
#68727 = CARTESIAN_POINT ( 'NONE',  ( -0.4396325459317577122, -0.6692913385826773087, -0.1292274648535924053 ) ) ;
#68728 = EDGE_CURVE ( 'NONE', #2780, #59692, #11463, .T. ) ;
#68729 = CARTESIAN_POINT ( 'NONE',  ( 0.4002624671916016896, -0.08942795157527998196, 0.3641732283464567121 ) ) ;
#68730 = CARTESIAN_POINT ( 'NONE',  ( -1.699475065616797398, 0.2952755905511811885, 0.1292274648535926551 ) ) ;
#68731 = CARTESIAN_POINT ( 'NONE',  ( -0.4672528563079629271, 1.453807508635540868, -2.571216978929444785 ) ) ;
#68732 = CARTESIAN_POINT ( 'NONE',  ( 0.1837270341207354329, 0.2306618581243848609, 0.2411417322834645549 ) ) ;
#68733 = DIRECTION ( 'NONE',  ( -0.000000000000000000, -1.000000000000000000, -0.000000000000000000 ) ) ;
#68734 = CARTESIAN_POINT ( 'NONE',  ( 1.377952755905512472, -0.6692913385826771977, 8.415575281601705876E-17 ) ) ;
#68735 = CARTESIAN_POINT ( 'NONE',  ( -0.2867679344610364334, -0.2867679344610367109, -2.728346456692912536 ) ) ;
#68736 = ORIENTED_EDGE ( 'NONE', *, *, #42480, .T. ) ;
#68737 = ORIENTED_EDGE ( 'NONE', *, *, #45798, .F. ) ;
#68738 = CARTESIAN_POINT ( 'NONE',  ( 0.6167979002624679463, 0.05413385826771626580, -0.4176697321401330321 ) ) ;
#68739 = CARTESIAN_POINT ( 'NONE',  ( 0.2230971128608929543, -0.004921259842519870586, -0.3153832671262229437 ) ) ;
#68741 = CARTESIAN_POINT ( 'NONE',  ( -1.604771003085130099, 1.595806277125121797, 0.1466069496707745612 ) ) ;
#68740 = DIRECTION ( 'NONE',  ( 1.047444401652940007E-14, 0.000000000000000000, -1.000000000000000000 ) ) ;
#68742 = CARTESIAN_POINT ( 'NONE',  ( -0.3392501089628017219, -0.1958661417322836718, -0.6095800524934383846 ) ) ;
#68743 = CARTESIAN_POINT ( 'NONE',  ( -0.4724409448818895907, -0.1265901696524993070, 0.1922572178477690297 ) ) ;
#68744 = CARTESIAN_POINT ( 'NONE',  ( 0.000000000000000000, 2.185039370078740273, 0.000000000000000000 ) ) ;
#68745 = CARTESIAN_POINT ( 'NONE',  ( 0.1998031496062994128, -0.3460692066303957537, -2.530839895013123453 ) ) ;
#68746 = CARTESIAN_POINT ( 'NONE',  ( 0.4068241469816279987, -0.4281496062992127816, -0.4176697321401328100 ) ) ;
#68747 = CARTESIAN_POINT ( 'NONE',  ( -0.6692913385826764205, 0.2952755905511811885, 0.000000000000000000 ) ) ;
#68748 = CARTESIAN_POINT ( 'NONE',  ( -1.338582677165353729, -0.1870078740157480879, -0.4822834645669291653 ) ) ;
#68749 = CARTESIAN_POINT ( 'NONE',  ( 0.8464566929133865436, 0.1660481256975883668, -0.3530559997133364547 ) ) ;
#68750 = VECTOR ( 'NONE', #38496, 39.37007874015748854 ) ;
#68751 = CARTESIAN_POINT ( 'NONE',  ( 1.541994750656168645, -0.6692913385826771977, 0.1292274648535927661 ) ) ;
#68752 = CARTESIAN_POINT ( 'NONE',  ( 1.568241469816273659, -0.08942795157528024563, -0.3641732283464568787 ) ) ;
#68753 = CARTESIAN_POINT ( 'NONE',  ( 1.089238845144357759, -0.004921259842519870586, -0.3153832671262229437 ) ) ;
#68754 = CARTESIAN_POINT ( 'NONE',  ( -0.8530183727034112984, 0.05413385826771666132, 0.4176697321401328100 ) ) ;
#68755 = CARTESIAN_POINT ( 'NONE',  ( 0.1998031496062992463, 0.3460692066303959202, -0.5360892388451443669 ) ) ;
#68756 = CARTESIAN_POINT ( 'NONE',  ( 1.496062992125985147, -0.1870078740157479769, 0.4822834645669291653 ) ) ;
#68757 = CARTESIAN_POINT ( 'NONE',  ( 0.3392501089628018329, 0.1958661417322835607, -0.1233595800524933950 ) ) ;
#68758 = CARTESIAN_POINT ( 'NONE',  ( -0.2952755905511803003, -0.5400638737290845981, -0.3530559997133363437 ) ) ;
#68760 = CARTESIAN_POINT ( 'NONE',  ( 0.000000000000000000, 0.000000000000000000, 0.1574803149606299191 ) ) ;
#68759 = CARTESIAN_POINT ( 'NONE',  ( 1.135170603674541256, -0.6692913385826773087, -0.1292274648535924053 ) ) ;
#68761 = CARTESIAN_POINT ( 'NONE',  ( -1.207349081364828880, 0.1283753931104746893, -0.1820866141732285504 ) ) ;
#68762 = CARTESIAN_POINT ( 'NONE',  ( 0.3477690288713918276, -0.6692913385826773087, -0.1292274648535924053 ) ) ;
#68763 = CARTESIAN_POINT ( 'NONE',  ( 1.003937007874016185, 0.07958543189024071263, -0.2665933059059888421 ) ) ;
#68764 = CARTESIAN_POINT ( 'NONE',  ( 0.3917322834645669549, 2.398668435337827645E-17, -1.457985933561992686 ) ) ;
#68765 = CARTESIAN_POINT ( 'NONE',  ( -1.279527559055116948, -0.4536011799217367080, 0.2665933059059888421 ) ) ;
#68766 = CARTESIAN_POINT ( 'NONE',  ( 0.7677165354330716118, 0.1660481256975883668, -0.3530559997133364547 ) ) ;
#68767 = CARTESIAN_POINT ( 'NONE',  ( -0.03443470937339727228, 0.2755905511811023723, -1.438590695389362573 ) ) ;
#68768 = CARTESIAN_POINT ( 'NONE',  ( -0.4199475065616791736, 0.1283753931104746893, -0.1820866141732285504 ) ) ;
#68769 = CARTESIAN_POINT ( 'NONE',  ( -0.2099737532808391705, -0.6046776061558809534, -0.2411417322834644161 ) ) ;
#68770 = CARTESIAN_POINT ( 'NONE',  ( -1.154855643044618851, 0.1283753931104748280, 0.1820866141732283561 ) ) ;
#68771 = CARTESIAN_POINT ( 'NONE',  ( -0.8202099737532801971, -0.6692913385826771977, 0.1292274648535927661 ) ) ;
#68772 = CARTESIAN_POINT ( 'NONE',  ( 1.220472440944882608, 0.2952755905511811885, 0.000000000000000000 ) ) ;
#68773 = CARTESIAN_POINT ( 'NONE',  ( 0.2867679344610366554, 0.2867679344610366554, -0.6069746963592669298 ) ) ;
#68774 = CARTESIAN_POINT ( 'NONE',  ( -1.023622047244093558, -0.1870078740157479769, 0.3641732283464567677 ) ) ;
#68775 = CARTESIAN_POINT ( 'NONE',  ( 1.096712450468791955, 1.126169283821023770, 0.2385660781250339146 ) ) ;
#68776 = CARTESIAN_POINT ( 'NONE',  ( 1.299212598425197429, 0.2952755905511811885, 0.000000000000000000 ) ) ;
#68777 = CARTESIAN_POINT ( 'NONE',  ( 0.3458507752293908943, -0.3458507752293908943, -2.222440944881889813 ) ) ;
#68778 = CARTESIAN_POINT ( 'NONE',  ( -1.181102362204723644, -0.1870078740157480879, -0.4822834645669291653 ) ) ;
#68779 = CARTESIAN_POINT ( 'NONE',  ( -1.220472440944881054, -0.5511811023622047445, 6.969142054262312111E-17 ) ) ;
#68780 = CARTESIAN_POINT ( 'NONE',  ( -0.4330708661417315697, 0.1771653543307087630, 0.000000000000000000 ) ) ;
#68781 = FACE_OUTER_BOUND ( 'NONE', #63614, .T. ) ;
#68782 = CARTESIAN_POINT ( 'NONE',  ( -0.05249343832020911260, 0.2306618581243848609, 0.2411417322834645549 ) ) ;
#68783 = CARTESIAN_POINT ( 'NONE',  ( -0.1312335958005241554, -0.5023911411419708095, -0.1820866141732282451 ) ) ;
#68784 = CARTESIAN_POINT ( 'NONE',  ( -1.292650918635170010, -0.5511811023622046335, 0.09757992244046803654 ) ) ;
#68785 = CARTESIAN_POINT ( 'NONE',  ( -1.666666666666665853, 0.05413385826771626580, -0.4176697321401330321 ) ) ;
#68786 = CARTESIAN_POINT ( 'NONE',  ( 1.181102362204724976, -0.1870078740157480601, -0.3641732283464567677 ) ) ;
#68787 = CARTESIAN_POINT ( 'NONE',  ( 1.108923884514436686, -0.3162353388693409650, -0.4822834645669289433 ) ) ;
#68788 = DIRECTION ( 'NONE',  ( 0.000000000000000000, 0.000000000000000000, -1.000000000000000000 ) ) ;
#68789 = CARTESIAN_POINT ( 'NONE',  ( 0.5511811023622055217, -0.1870078740157479769, 0.3641732283464567677 ) ) ;
#68790 = CARTESIAN_POINT ( 'NONE',  ( 1.089238845144357759, 0.05413385826771626580, -0.4176697321401330321 ) ) ;
#68791 = CARTESIAN_POINT ( 'NONE',  ( 0.8398950131233602345, 0.1283753931104746893, -0.1820866141732285504 ) ) ;
#68792 = ORIENTED_EDGE ( 'NONE', *, *, #82940, .F. ) ;
#68793 = CARTESIAN_POINT ( 'NONE',  ( -1.003937007874014853, 0.1660481256975885056, 0.3530559997133364547 ) ) ;
#68794 = CARTESIAN_POINT ( 'NONE',  ( -1.089238845144356427, -0.4281496062992127816, -0.4176697321401328100 ) ) ;
#68795 = CARTESIAN_POINT ( 'NONE',  ( -0.2296587926509179312, -0.3162353388693409650, -0.4822834645669289433 ) ) ;
#68796 = CARTESIAN_POINT ( 'NONE',  ( -0.1998031496062994683, 0.3460692066303958092, -0.01312335958005251234 ) ) ;
#68797 = CARTESIAN_POINT ( 'NONE',  ( 0.1070741851644054776, -0.3996062992125984925, -2.524278215223096478 ) ) ;
#68798 = CARTESIAN_POINT ( 'NONE',  ( 0.2624671916010504757, -0.6046776061558809534, -0.2411417322834644161 ) ) ;
#68799 = CARTESIAN_POINT ( 'NONE',  ( -1.666666666666665853, 0.05413385826771626580, -0.4176697321401330321 ) ) ;
#68800 = CARTESIAN_POINT ( 'NONE',  ( -0.03280839895013062252, 0.2952755905511810774, -0.1292274648535930714 ) ) ;
#68801 = CARTESIAN_POINT ( 'NONE',  ( 0.9383202099737536495, -0.3162353388693405765, 0.4822834645669290543 ) ) ;
#68802 = CARTESIAN_POINT ( 'NONE',  ( -0.1998031496062991907, -0.3460692066303959757, -1.955380577427821454 ) ) ;
#68803 = CARTESIAN_POINT ( 'NONE',  ( 0.1974969037888706369, -0.3420746716998659953, -1.509186351706036655 ) ) ;
#68804 = CARTESIAN_POINT ( 'NONE',  ( -0.3460692066303958092, -0.1998031496062994683, -2.729658792650918375 ) ) ;
#68805 = CARTESIAN_POINT ( 'NONE',  ( -0.2362204724409451284, 0.4091458600556402425, -2.532808398950130879 ) ) ;
#68806 = CARTESIAN_POINT ( 'NONE',  ( 0.1049643490035303689, 0.3917322834645670104, -0.6154855643044617741 ) ) ;
#68807 = CARTESIAN_POINT ( 'NONE',  ( -0.6364829396325453192, -0.2845877964562159024, 0.3641732283464567677 ) ) ;
#68808 = CARTESIAN_POINT ( 'NONE',  ( -0.9055118110236215490, 0.2952755905511811885, 0.000000000000000000 ) ) ;
#68809 = CARTESIAN_POINT ( 'NONE',  ( 0.4790026246719167324, -0.05778040916215522460, 0.4822834645669289988 ) ) ;
#68810 = VECTOR ( 'NONE', #44200, 39.37007874015748143 ) ;
#68811 = CARTESIAN_POINT ( 'NONE',  ( -0.1058382717557503072, 0.3949938075777408852, -2.130577427821521930 ) ) ;
#68812 = CARTESIAN_POINT ( 'NONE',  ( 1.062992125984252745, 0.2952755905511811885, 0.000000000000000000 ) ) ;
#68813 = CARTESIAN_POINT ( 'NONE',  ( -1.594488188976377119, 0.1660481256975883668, -0.3530559997133364547 ) ) ;
#68814 = CARTESIAN_POINT ( 'NONE',  ( 1.332020997375328974, -0.05778040916215560624, -0.4822834645669293319 ) ) ;
#68815 = CARTESIAN_POINT ( 'NONE',  ( -0.4724409448818898682, -8.678599364036362592E-17, -2.559055118110236560 ) ) ;
#68816 = CARTESIAN_POINT ( 'NONE',  ( -0.2925321140481932924, 0.2925321140481931814, -2.224409448818897239 ) ) ;
#68817 = CARTESIAN_POINT ( 'NONE',  ( -0.03757601356356682354, 0.4709442531824372113, -2.755905511811023612 ) ) ;
#68818 = CARTESIAN_POINT ( 'NONE',  ( 1.082677165354331228, -0.5400638737290844871, 0.3530559997133364547 ) ) ;
#68819 = EDGE_CURVE ( 'NONE', #70238, #23460, #51667, .T. ) ;
#68820 = CARTESIAN_POINT ( 'NONE',  ( 0.6299212598425204535, -0.1870078740157479769, 0.4822834645669291653 ) ) ;
#68821 = CARTESIAN_POINT ( 'NONE',  ( 1.430446194225722500, -0.004921259842519576551, 0.3153832671262227771 ) ) ;
#68823 = CARTESIAN_POINT ( 'NONE',  ( -1.568241469816272105, -0.3162353388693409650, -0.4822834645669289433 ) ) ;
#68822 = CARTESIAN_POINT ( 'NONE',  ( -1.581364829396324945, -0.08942795157528024563, -0.3641732283464568787 ) ) ;
#68824 = CARTESIAN_POINT ( 'NONE',  ( -0.3392501089628019439, 0.1958661417322832554, -2.783445251147295352 ) ) ;
#68825 = CARTESIAN_POINT ( 'NONE',  ( 0.9251968503937015864, 0.1660481256975883668, -0.3530559997133364547 ) ) ;
#68826 = DIRECTION ( 'NONE',  ( 0.000000000000000000, -1.000000000000000000, 0.000000000000000000 ) ) ;
#68827 = CARTESIAN_POINT ( 'NONE',  ( -0.3412073490813641308, -0.6046776061558807314, 0.2411417322834647770 ) ) ;
#68828 = CARTESIAN_POINT ( 'NONE',  ( -0.3674540682414692561, -0.6046776061558809534, -0.2411417322834644161 ) ) ;
#68829 = CARTESIAN_POINT ( 'NONE',  ( 1.515748031496063186, -0.5400638737290845981, -0.3530559997133363437 ) ) ;
#68830 = CARTESIAN_POINT ( 'NONE',  ( -0.3392501089628017219, -0.1958661417322836718, -0.2946194225721785465 ) ) ;
#68831 = CARTESIAN_POINT ( 'NONE',  ( 0.2867679344610365999, 0.2867679344610365999, -1.704724409448818978 ) ) ;
#68832 =( BOUNDED_CURVE ( )  B_SPLINE_CURVE ( 2, ( #49601, #76117, #17639, #56328, #75295, #44101, #55080, #18458, #69794, #12140, #68558, #10498, #75708 ),
 .UNSPECIFIED., .F., .F. ) 
 B_SPLINE_CURVE_WITH_KNOTS ( ( 3, 2, 2, 2, 2, 2, 3 ),
 ( 0.7625000000000000666, 0.7666666666666668295, 0.7708333333333334814, 0.7750000000000001332, 0.7791666666666667851, 0.7833333333333334370, 0.7875000000000000888 ),
 .UNSPECIFIED. ) 
 CURVE ( )  GEOMETRIC_REPRESENTATION_ITEM ( )  RATIONAL_B_SPLINE_CURVE ( ( 0.9999999999999991118, 0.9659258262890692004, 1.000000000000000000, 0.9659258262890683122, 1.000000000000000000, 0.9659258262890683122, 1.000000000000000000, 0.9659258262890683122, 1.000000000000000000, 0.9659258262890683122, 1.000000000000000000, 0.9659258262890674240, 1.000000000000000888 ) ) 
 REPRESENTATION_ITEM ( '' )  );
#68833 = CARTESIAN_POINT ( 'NONE',  ( 0.1049643490035304938, -0.3917322834645669549, -2.124671916010498762 ) ) ;
#68834 = CARTESIAN_POINT ( 'NONE',  ( 1.666666666666667185, 0.05413385826771666132, 0.4176697321401328100 ) ) ;
#68835 = EDGE_LOOP ( 'NONE', ( #44965, #50039, #7885, #34267 ) ) ;
#68836 = CARTESIAN_POINT ( 'NONE',  ( 0.2891555358219910499, 0.2891555358219910499, -2.657480314960630530 ) ) ;
#68837 = VERTEX_POINT ( 'NONE', #11879 ) ;
#68838 = CARTESIAN_POINT ( 'NONE',  ( 0.000000000000000000, 0.000000000000000000, 0.000000000000000000 ) ) ;
#68839 = CARTESIAN_POINT ( 'NONE',  ( 1.253280839895013710, -0.2845877964562159024, 0.3641732283464567677 ) ) ;
#68840 = CARTESIAN_POINT ( 'NONE',  ( 0.3460692066303959202, 0.1998031496062993295, -1.233595800524934338 ) ) ;
#68841 = CARTESIAN_POINT ( 'NONE',  ( 0.5636006452641431075, 3.421639014772782816E-16, 0.3464511005275203726 ) ) ;
#68842 = CARTESIAN_POINT ( 'NONE',  ( 0.4847769261806178509, 1.968503937007873850, 0.4915354330708653907 ) ) ;
#68843 = DIRECTION ( 'NONE',  ( 1.000000000000000000, 0.000000000000000000, 0.000000000000000000 ) ) ;
#68844 = LINE ( 'NONE', #11607, #60639 ) ;
#68845 = CARTESIAN_POINT ( 'NONE',  ( -0.1958661417322836718, 0.3392501089628017219, -0.4127296587926510552 ) ) ;
#68846 = CARTESIAN_POINT ( 'NONE',  ( -0.6496062992125976043, 0.07958543189024071263, -0.2665933059059888421 ) ) ;
#68847 = CARTESIAN_POINT ( 'NONE',  ( -1.076115485564303809, 0.1283753931104748280, 0.1820866141732283561 ) ) ;
#68848 = CARTESIAN_POINT ( 'NONE',  ( 0.7152230971128614723, -0.3162353388693409650, -0.4822834645669289433 ) ) ;
#68849 = CARTESIAN_POINT ( 'NONE',  ( -1.200787401574802349, -0.5400638737290844871, 0.3530559997133364547 ) ) ;
#68850 = CARTESIAN_POINT ( 'NONE',  ( 0.3392501089628018329, 0.1958661417322835607, -0.1233595800524933950 ) ) ;
#68851 = ORIENTED_EDGE ( 'NONE', *, *, #55159, .T. ) ;
#68852 = CARTESIAN_POINT ( 'NONE',  ( 1.535433070866142335, -0.6692913385826771977, 8.415575281601705876E-17 ) ) ;
#68853 = CARTESIAN_POINT ( 'NONE',  ( 3.937007874015748143, 1.724409448818898127, 0.6299212598425202314 ) ) ;
#68854 = CARTESIAN_POINT ( 'NONE',  ( -0.4724409448818898682, -8.678599364036362592E-17, -1.771653543307086576 ) ) ;
#68855 = CARTESIAN_POINT ( 'NONE',  ( -1.586052503253847057, 1.574803149606300412, 0.1653254495020574921 ) ) ;
#68856 = CARTESIAN_POINT ( 'NONE',  ( -0.3458507752293909498, 0.3458507752293908388, -0.9645669291338581086 ) ) ;
#68857 = CARTESIAN_POINT ( 'NONE',  ( -0.7086614173228339419, -0.1870078740157479769, 0.4822834645669291653 ) ) ;
#68858 = CARTESIAN_POINT ( 'NONE',  ( 1.227034120734908917, 0.2952755905511810774, -0.1292274648535930714 ) ) ;
#68860 = CARTESIAN_POINT ( 'NONE',  ( -0.5314960629921146040, 2.755905511811024056, -3.264097702071374840 ) ) ;
#68859 = FACE_OUTER_BOUND ( 'NONE', #73273, .T. ) ;
#68861 = CARTESIAN_POINT ( 'NONE',  ( -1.640419947506561060, -0.4281496062992127816, -0.4176697321401328100 ) ) ;
#68862 = CARTESIAN_POINT ( 'NONE',  ( -1.325459317585300889, -0.4281496062992127816, -0.4176697321401328100 ) ) ;
#68863 = CARTESIAN_POINT ( 'NONE',  ( -0.3392501089628019439, 0.1958661417322832554, -0.4212405267378459550 ) ) ;
#68864 = CARTESIAN_POINT ( 'NONE',  ( 0.01968503937007930540, 0.07958543189024085140, 0.2665933059059887866 ) ) ;
#68865 = CARTESIAN_POINT ( 'NONE',  ( 0.2867679344610366554, 0.2867679344610366554, -1.009842519685039353 ) ) ;
#68866 = CARTESIAN_POINT ( 'NONE',  ( -0.08530183727034056085, -0.2845877964562159024, 0.3641732283464567677 ) ) ;
#68867 = CARTESIAN_POINT ( 'NONE',  ( 0.4265091863517067039, -0.5511811023622048555, -0.09757992244046775898 ) ) ;
#68868 = CARTESIAN_POINT ( 'NONE',  ( 0.3871391076115492380, -0.05778040916215560624, -0.4822834645669293319 ) ) ;
#68869 = CIRCLE ( 'NONE', #75610, 0.1771653543307085410 ) ;
#68870 = CARTESIAN_POINT ( 'NONE',  ( -0.5905511811023613777, -0.5511811023622047445, 6.969142054262312111E-17 ) ) ;
#68871 = CARTESIAN_POINT ( 'NONE',  ( 0.1958661417322836440, -0.3392501089628017219, -2.131233595800524849 ) ) ;
#68872 = CARTESIAN_POINT ( 'NONE',  ( 1.581364829396326277, -0.05778040916215522460, 0.4822834645669289988 ) ) ;
#68873 = CARTESIAN_POINT ( 'NONE',  ( -0.8202099737532799750, 0.2952755905511810774, -0.1292274648535930714 ) ) ;
#68874 = CARTESIAN_POINT ( 'NONE',  ( -0.1265901696524986964, -0.4724409448818899238, -0.9363517060367454459 ) ) ;
#68875 = CARTESIAN_POINT ( 'NONE',  ( -0.1443569553805768291, 0.05413385826771666132, 0.4176697321401328100 ) ) ;
#68876 = CARTESIAN_POINT ( 'NONE',  ( -0.7020997375328074108, -0.05778040916215522460, 0.4822834645669289988 ) ) ;
#68877 = CARTESIAN_POINT ( 'NONE',  ( 1.161417322834646493, -0.4536011799217367080, 0.2665933059059888421 ) ) ;
#68878 = CARTESIAN_POINT ( 'NONE',  ( 0.03280839895013198948, 0.1771653543307087630, 0.09757992244046791164 ) ) ;
#68879 = CARTESIAN_POINT ( 'NONE',  ( -0.3083989501312330295, -0.05778040916215522460, 0.4822834645669289988 ) ) ;
#68880 = CARTESIAN_POINT ( 'NONE',  ( -0.9514435695538050464, -0.05778040916215560624, -0.4822834645669293319 ) ) ;
#68881 = CARTESIAN_POINT ( 'NONE',  ( 1.614173228346457378, 0.7166040191147859950, -0.1372047244094476148 ) ) ;
#68882 = CARTESIAN_POINT ( 'NONE',  ( -0.4724409448818899238, 0.1265901696524986964, -0.3477690288713910505 ) ) ;
#68883 = CARTESIAN_POINT ( 'NONE',  ( -0.4724409448818890911, -0.1870078740157480879, -0.4822834645669291653 ) ) ;
#68884 = ORIENTED_EDGE ( 'NONE', *, *, #55811, .T. ) ;
#68885 = CARTESIAN_POINT ( 'NONE',  ( 0.2925321140481932369, 0.2925321140481932369, -1.946850393700787274 ) ) ;
#68886 = CARTESIAN_POINT ( 'NONE',  ( 1.043307086614173818, -0.5400638737290845981, -0.3530559997133363437 ) ) ;
#68887 = CARTESIAN_POINT ( 'NONE',  ( -0.8464566929133852113, -0.4536011799217368745, -0.2665933059059886201 ) ) ;
#68888 = CARTESIAN_POINT ( 'NONE',  ( -0.5905511811023615998, 0.2952755905511811885, 0.000000000000000000 ) ) ;
#68889 = CARTESIAN_POINT ( 'NONE',  ( 1.082677165354331228, 0.1660481256975883668, -0.3530559997133364547 ) ) ;
#68890 = CARTESIAN_POINT ( 'NONE',  ( 0.7677165354330716118, 0.1660481256975883668, -0.3530559997133364547 ) ) ;
#68891 = CARTESIAN_POINT ( 'NONE',  ( -1.489501312335957062, -0.05778040916215522460, 0.4822834645669289988 ) ) ;
#68892 = CARTESIAN_POINT ( 'NONE',  ( -1.003937007874015297, -0.4536011799217368745, -0.2665933059059886201 ) ) ;
#68893 = CARTESIAN_POINT ( 'NONE',  ( -0.2925321140481930149, -0.2925321140481933480, -0.2933070866141732624 ) ) ;
#68894 = CARTESIAN_POINT ( 'NONE',  ( 0.1998031496062994405, -0.3460692066303958092, -0.5643044619422572516 ) ) ;
#68895 = CARTESIAN_POINT ( 'NONE',  ( -0.1974969037888703871, -0.3420746716998661063, -0.3805774278215224293 ) ) ;
#68896 = CARTESIAN_POINT ( 'NONE',  ( 1.568241469816273659, -0.08942795157528024563, -0.3641732283464568787 ) ) ;
#68897 = CARTESIAN_POINT ( 'NONE',  ( 0.8070866141732288002, 0.07958543189024085140, 0.2665933059059887866 ) ) ;
#68898 = CARTESIAN_POINT ( 'NONE',  ( 0.3543307086614179147, 0.2952755905511811885, 0.000000000000000000 ) ) ;
#68899 = CARTESIAN_POINT ( 'NONE',  ( -1.614173228346456712, 2.094556775020298467, -0.1372047244094478091 ) ) ;
#68900 = CARTESIAN_POINT ( 'NONE',  ( -0.1058382717557503072, 0.3949938075777408852, -0.8707349081364829102 ) ) ;
#68901 = CARTESIAN_POINT ( 'NONE',  ( 0.6167979002624679463, -0.004921259842519870586, -0.3153832671262229437 ) ) ;
#68902 = EDGE_CURVE ( 'NONE', #15218, #58335, #36704, .T. ) ;
#68903 = CARTESIAN_POINT ( 'NONE',  ( -0.5183727034120726440, 0.2952755905511811885, 0.1292274648535926551 ) ) ;
#68904 = CARTESIAN_POINT ( 'NONE',  ( -0.8333333333333323711, 0.2952755905511811885, 0.1292274648535926551 ) ) ;
#68905 = CARTESIAN_POINT ( 'NONE',  ( 1.128608923884515169, -0.6046776061558809534, -0.2411417322834644161 ) ) ;
#68906 = CARTESIAN_POINT ( 'NONE',  ( 0.4724409448818896462, 0.1265901696524990294, -1.069553805774278166 ) ) ;
#68907 = CARTESIAN_POINT ( 'NONE',  ( 0.1998031496062994405, -0.3460692066303958092, -2.139107611548556331 ) ) ;
#68908 = CARTESIAN_POINT ( 'NONE',  ( -0.2690288713910754526, 0.1771653543307087075, -0.09757992244046823083 ) ) ;
#68909 = ORIENTED_EDGE ( 'NONE', *, *, #31514, .F. ) ;
#68910 = CARTESIAN_POINT ( 'NONE',  ( 0.3917322834645670659, 2.398668435337828261E-17, -0.9022502869104481737 ) ) ;
#68911 = ORIENTED_EDGE ( 'NONE', *, *, #13087, .T. ) ;
#68912 = VECTOR ( 'NONE', #77032, 39.37007874015748143 ) ;
#68913 = EDGE_CURVE ( 'NONE', #66690, #56483, #43353, .T. ) ;
#68914 = CARTESIAN_POINT ( 'NONE',  ( -1.049868766404198794, 0.2306618581243847221, -0.2411417322834647770 ) ) ;
#68915 = CARTESIAN_POINT ( 'NONE',  ( -0.1181102362204717315, -0.6692913385826771977, 8.415575281601705876E-17 ) ) ;
#68916 = CARTESIAN_POINT ( 'NONE',  ( -0.2427821522309703550, -0.3162353388693405765, 0.4822834645669290543 ) ) ;
#68917 = CARTESIAN_POINT ( 'NONE',  ( 0.4199475065616805614, 0.2306618581243848609, 0.2411417322834645549 ) ) ;
#68918 = CARTESIAN_POINT ( 'NONE',  ( -0.4330708661417315697, -0.6692913385826771977, 8.415575281601705876E-17 ) ) ;
#68919 = CARTESIAN_POINT ( 'NONE',  ( -1.174540682414697335, -0.05778040916215522460, 0.4822834645669289988 ) ) ;
#68920 = CARTESIAN_POINT ( 'NONE',  ( -0.9186351706036736120, 0.2306618581243848609, 0.2411417322834645549 ) ) ;
#68921 = CARTESIAN_POINT ( 'NONE',  ( 0.8792650918635177559, -0.4281496062992127816, -0.4176697321401328100 ) ) ;
#68922 = CARTESIAN_POINT ( 'NONE',  ( 0.5118110236220478892, 0.2952755905511811885, 0.000000000000000000 ) ) ;
#68923 = CARTESIAN_POINT ( 'NONE',  ( -0.1958661417322834220, -0.3392501089628018884, -0.8451443569553805935 ) ) ;
#68924 = CARTESIAN_POINT ( 'NONE',  ( -0.2493438320209966919, -0.3690944881889763329, 0.3153832671262228327 ) ) ;
#68925 = EDGE_LOOP ( 'NONE', ( #36858, #35793, #42809, #62702 ) ) ;
#68926 = CARTESIAN_POINT ( 'NONE',  ( 0.1974969037888704704, 0.3420746716998660508, -1.561679790026246684 ) ) ;
#68927 = ORIENTED_EDGE ( 'NONE', *, *, #60948, .T. ) ;
#68928 = CARTESIAN_POINT ( 'NONE',  ( -1.371391076115484831, 0.1771653543307087075, -0.09757992244046823083 ) ) ;
#68929 = CARTESIAN_POINT ( 'NONE',  ( -1.010498687664041384, 0.05413385826771666132, 0.4176697321401328100 ) ) ;
#68930 = CARTESIAN_POINT ( 'NONE',  ( -0.7742782152230962556, -0.4281496062992127816, -0.4176697321401328100 ) ) ;
#68931 = CARTESIAN_POINT ( 'NONE',  ( 0.2925321140481932369, -0.2925321140481932369, 0.05905511811023619884 ) ) ;
#68932 = CARTESIAN_POINT ( 'NONE',  ( -0.4986876640419942164, -0.6046776061558807314, 0.2411417322834647770 ) ) ;
#68933 = CARTESIAN_POINT ( 'NONE',  ( -0.7545931758530177724, 0.2952755905511811885, 0.1292274648535926551 ) ) ;
#68934 = CARTESIAN_POINT ( 'NONE',  ( 0.000000000000000000, 1.929133858267716661, -2.362204724409448620 ) ) ;
#68935 = CARTESIAN_POINT ( 'NONE',  ( -1.640419947506561060, -0.4281496062992127816, -0.4176697321401328100 ) ) ;
#68936 = CARTESIAN_POINT ( 'NONE',  ( 0.5052493438320218022, -0.5511811023622048555, -0.09757992244046775898 ) ) ;
#68937 = CARTESIAN_POINT ( 'NONE',  ( 3.912791665790199769, 1.724409448818897905, 0.4359958488159722534 ) ) ;
#68938 = CARTESIAN_POINT ( 'NONE',  ( -0.1049643490035307020, 0.3917322834645669549, -0.09120734908136493568 ) ) ;
#68939 = CARTESIAN_POINT ( 'NONE',  ( -0.03937007874015669567, -0.5511811023622047445, 6.969142054262312111E-17 ) ) ;
#68940 = CARTESIAN_POINT ( 'NONE',  ( -0.2624671916010490880, -0.6046776061558807314, 0.2411417322834647770 ) ) ;
#68941 = LINE ( 'NONE', #72890, #16076 ) ;
#68942 = CARTESIAN_POINT ( 'NONE',  ( -0.05249343832020911260, 0.2306618581243848609, 0.2411417322834645549 ) ) ;
#68943 = ORIENTED_EDGE ( 'NONE', *, *, #22956, .F. ) ;
#68944 = CARTESIAN_POINT ( 'NONE',  ( -0.3996062992125987146, 0.1070741851644051862, -1.922572178477689908 ) ) ;
#68945 = CARTESIAN_POINT ( 'NONE',  ( -0.8333333333333321491, 0.2066929133858267931, 0.1054918080437490802 ) ) ;
#68946 = ORIENTED_EDGE ( 'NONE', *, *, #40920, .F. ) ;
#68947 = CARTESIAN_POINT ( 'NONE',  ( -0.1070741851644051862, -0.3996062992125986590, -1.723753280839894986 ) ) ;
#68948 = CARTESIAN_POINT ( 'NONE',  ( -0.03056273350765576630, 0.3973686378485519755, -2.755905511811022723 ) ) ;
#68949 = CARTESIAN_POINT ( 'NONE',  ( -0.8333333333333323711, -0.5511811023622048555, -0.09757992244046775898 ) ) ;
#68950 = CARTESIAN_POINT ( 'NONE',  ( -0.8661417322834640276, -0.1870078740157480879, -0.4822834645669291653 ) ) ;
#68951 = CARTESIAN_POINT ( 'NONE',  ( -0.2362204724409447953, -0.4091458600556404646, -0.2230971128608923715 ) ) ;
#68952 = DIRECTION ( 'NONE',  ( -0.000000000000000000, -1.000000000000000000, -0.000000000000000000 ) ) ;
#68953 = CARTESIAN_POINT ( 'NONE',  ( 4.797336870675656522E-17, -0.3917322834645670104, 0.08661417322834651100 ) ) ;
#68954 = CARTESIAN_POINT ( 'NONE',  ( 1.253280839895013710, -0.05778040916215560624, -0.4822834645669293319 ) ) ;
#68955 = CARTESIAN_POINT ( 'NONE',  ( 0.5183727034120741983, 0.2952755905511810774, -0.1292274648535930714 ) ) ;
#68956 = CARTESIAN_POINT ( 'NONE',  ( 0.3937007874015754361, -0.1870078740157479769, 0.4822834645669291653 ) ) ;
#68957 = CARTESIAN_POINT ( 'NONE',  ( -0.9711286089238838626, 0.1283753931104746893, -0.1820866141732285504 ) ) ;
#68958 = CARTESIAN_POINT ( 'NONE',  ( -0.3083989501312330295, -0.05778040916215522460, 0.4822834645669289988 ) ) ;
#68959 = CARTESIAN_POINT ( 'NONE',  ( -0.4724409448818898682, -8.678599364036362592E-17, -2.478346456692913868 ) ) ;
#68960 = CARTESIAN_POINT ( 'NONE',  ( -0.8202099737532801971, -0.6692913385826771977, 0.1292274648535927661 ) ) ;
#68961 = CARTESIAN_POINT ( 'NONE',  ( 0.2891555358219910499, 0.2891555358219910499, -2.261811023622047667 ) ) ;
#68962 = CARTESIAN_POINT ( 'NONE',  ( 1.135170603674541256, 0.1771653543307087630, 0.09757992244046791164 ) ) ;
#68963 = CARTESIAN_POINT ( 'NONE',  ( -0.4921259842519677963, -0.4536011799217367080, 0.2665933059059888421 ) ) ;
#68964 = AXIS2_PLACEMENT_3D ( 'NONE', #22298, #34519, #9265 ) ;
#68965 = CARTESIAN_POINT ( 'NONE',  ( 1.364829396325460076, 0.1283753931104748280, 0.1820866141732283561 ) ) ;
#68966 = CARTESIAN_POINT ( 'NONE',  ( 1.601049868766404982, 0.1283753931104748280, 0.1820866141732283561 ) ) ;
#68967 = CARTESIAN_POINT ( 'NONE',  ( -1.017060367454067249, -0.08942795157527998196, 0.3641732283464567121 ) ) ;
#68968 = LINE ( 'NONE', #16818, #68174 ) ;
#68969 = CARTESIAN_POINT ( 'NONE',  ( 0.4986876640419954376, -0.5023911411419708095, -0.1820866141732282451 ) ) ;
#68970 = CARTESIAN_POINT ( 'NONE',  ( -0.4658792650918627265, -0.3162353388693409650, -0.4822834645669289433 ) ) ;
#68971 = CARTESIAN_POINT ( 'NONE',  ( -2.787279214012418738, 2.401574803149606474, 0.000000000000000000 ) ) ;
#68972 = CARTESIAN_POINT ( 'NONE',  ( -0.2034120734908128059, 0.1771653543307087630, 0.09757992244046791164 ) ) ;
#68973 = CARTESIAN_POINT ( 'NONE',  ( 0.3458507752293908943, 0.3458507752293908943, -1.001968503937007871 ) ) ;
#68974 = CARTESIAN_POINT ( 'NONE',  ( 0.8464566929133866546, -0.5400638737290844871, 0.3530559997133364547 ) ) ;
#68975 = CARTESIAN_POINT ( 'NONE',  ( 1.968503937007874072, 0.000000000000000000, 5.701968306260621233 ) ) ;
#68976 = B_SPLINE_CURVE_WITH_KNOTS ( 'NONE', 3,
 ( #60787, #34716, #9868, #81000, #3140, #48158, #80180, #22901, #61625, #74682, #21660, #3967, #35537, #54046, #41840, #61199, #28803, #54467, #23314, #17028, #42667, #16609, #62035, #67530, #41436, #22077, #29630, #3556, #74266, #79760, #47320, #2725 ),
 .UNSPECIFIED., .F., .F.,
 ( 4, 2, 2, 2, 2, 2, 2, 2, 2, 2, 2, 2, 2, 2, 2, 4 ),
 ( 3.680777123389603761E-21, 0.002389845404268378572, 0.003584768106402557667, 0.004779690808536737195, 0.007169536212805114467, 0.008364458914939303102, 0.009559381617073493473, 0.01075430431920768211, 0.01135176567027477643, 0.01194922702134187248, 0.01314414972347606979, 0.01433907242561027057, 0.01553399512774447135, 0.01672891782987866865, 0.01792384053201287117, 0.01911876323414707021 ),
 .UNSPECIFIED. ) ;
#68977 = VECTOR ( 'NONE', #31925, 39.37007874015748143 ) ;
#68978 = CARTESIAN_POINT ( 'NONE',  ( 1.279527559055118724, 0.07958543189024085140, 0.2665933059059887866 ) ) ;
#68979 = CARTESIAN_POINT ( 'NONE',  ( -1.049868766404198794, 0.2306618581243847221, -0.2411417322834647770 ) ) ;
#68980 = CARTESIAN_POINT ( 'NONE',  ( -0.3740157480314953431, 0.07958543189024085140, 0.2665933059059887866 ) ) ;
#68981 = DIRECTION ( 'NONE',  ( 0.000000000000000000, -1.000000000000000000, 0.000000000000000000 ) ) ;
#68982 = CARTESIAN_POINT ( 'NONE',  ( 0.1574803149606306130, -0.1870078740157479769, 0.3641732283464567677 ) ) ;
#68983 = CARTESIAN_POINT ( 'NONE',  ( -0.4593175853018364174, -0.4281496062992127816, -0.4176697321401328100 ) ) ;
#68984 = CARTESIAN_POINT ( 'NONE',  ( -0.2925321140481930149, -0.2925321140481933480, -0.9232283464566929387 ) ) ;
#68985 = CARTESIAN_POINT ( 'NONE',  ( 0.1958661417322834775, 0.3392501089628018884, -2.276246719160105236 ) ) ;
#68986 = CARTESIAN_POINT ( 'NONE',  ( 0.7611548556430451917, -0.5023911411419708095, 0.1820866141732285504 ) ) ;
#68987 = CARTESIAN_POINT ( 'NONE',  ( -0.3937007874015740483, -0.1870078740157479769, 0.4822834645669291653 ) ) ;
#68988 = CARTESIAN_POINT ( 'NONE',  ( -0.6496062992125976043, 0.1660481256975883668, -0.3530559997133364547 ) ) ;
#68989 = CARTESIAN_POINT ( 'NONE',  ( -0.9448818897637790704, -0.1870078740157480601, -0.3641732283464567677 ) ) ;
#68990 = CARTESIAN_POINT ( 'NONE',  ( -3.926394065941670508, 1.160970718358689702, 0.2891465379911152822 ) ) ;
#68991 = CARTESIAN_POINT ( 'NONE',  ( -0.1509186351706028884, -0.3162353388693409650, -0.4822834645669289433 ) ) ;
#68992 = CARTESIAN_POINT ( 'NONE',  ( -1.095800524934382292, -0.08942795157527998196, 0.3641732283464567121 ) ) ;
#68993 = CARTESIAN_POINT ( 'NONE',  ( -1.377952755905511140, -0.6692913385826771977, 8.415575281601705876E-17 ) ) ;
#68994 = CARTESIAN_POINT ( 'NONE',  ( -3.264097702071373064, 2.755905511811024056, 0.5314960629921260393 ) ) ;
#68995 = VERTEX_POINT ( 'NONE', #56470 ) ;
#68996 = CARTESIAN_POINT ( 'NONE',  ( -1.463254593175852492, -0.5511811023622048555, -0.09757992244046775898 ) ) ;
#68997 = CARTESIAN_POINT ( 'NONE',  ( -1.555118110236219930, 0.1660481256975885056, 0.3530559997133364547 ) ) ;
#68998 = CARTESIAN_POINT ( 'NONE',  ( -0.9120734908136475250, 0.2952755905511811885, 0.1292274648535926551 ) ) ;
#68999 = B_SPLINE_CURVE_WITH_KNOTS ( 'NONE', 3,
 ( #14387, #27824, #73702, #1745, #21510, #16042, #47168, #15209, #41688, #9715, #29064, #54735 ),
 .UNSPECIFIED., .F., .F.,
 ( 4, 2, 2, 2, 2, 4 ),
 ( 7.152448122690996019E-18, 0.001328432419540397699, 0.002656864839080788025, 0.003985297258621178784, 0.004649513468391363973, 0.005313729678161549161 ),
 .UNSPECIFIED. ) ;
#69000 = CARTESIAN_POINT ( 'NONE',  ( -1.620734908136482577, 0.2952755905511811885, 0.1292274648535926551 ) ) ;
#69001 = CARTESIAN_POINT ( 'NONE',  ( -0.3917322834645670104, -7.196005306013484475E-17, -1.383858267716535417 ) ) ;
#69002 = PLANE ( 'NONE',  #66012 ) ;
#69003 = CARTESIAN_POINT ( 'NONE',  ( 1.108923884514436686, -0.3162353388693409650, -0.4822834645669289433 ) ) ;
#69004 = CARTESIAN_POINT ( 'NONE',  ( 0.5774278215223104249, 0.2306618581243848609, 0.2411417322834645549 ) ) ;
#69005 = FACE_OUTER_BOUND ( 'NONE', #29307, .T. ) ;
#69006 = CARTESIAN_POINT ( 'NONE',  ( 0.3996062992125985480, 2.446882876249141654E-17, -2.399606299212598604 ) ) ;
#69007 = CARTESIAN_POINT ( 'NONE',  ( 1.135170603674541256, 0.1771653543307087630, 0.09757992244046791164 ) ) ;
#69008 = CARTESIAN_POINT ( 'NONE',  ( 0.1070741851644054915, -0.3996062992125986035, -1.030183727034120533 ) ) ;
#69009 = ORIENTED_EDGE ( 'NONE', *, *, #34103, .T. ) ;
#69010 = CARTESIAN_POINT ( 'NONE',  ( -0.7611548556430438595, -0.5023911411419708095, -0.1820866141732282451 ) ) ;
#69011 = CARTESIAN_POINT ( 'NONE',  ( 0.2867679344610365999, 0.2867679344610365999, -2.649606299212598604 ) ) ;
#69012 = ORIENTED_EDGE ( 'NONE', *, *, #12663, .F. ) ;
#69013 = CARTESIAN_POINT ( 'NONE',  ( 0.5511811023622054106, -0.1870078740157480879, -0.4822834645669291653 ) ) ;
#69014 = CARTESIAN_POINT ( 'NONE',  ( -0.3346456692913377662, -0.5400638737290844871, 0.3530559997133364547 ) ) ;
#69015 = CARTESIAN_POINT ( 'NONE',  ( -1.102362204724408601, -0.1870078740157480879, -0.4822834645669291653 ) ) ;
#69016 = CARTESIAN_POINT ( 'NONE',  ( 0.9776902887139113929, -0.6692913385826773087, -0.1292274648535924053 ) ) ;
#69017 = CIRCLE ( 'NONE', #73052, 0.2952755905511810774 ) ;
#69018 = CARTESIAN_POINT ( 'NONE',  ( -1.607611548556429737, 0.1771653543307087075, -0.09757992244046823083 ) ) ;
#69019 = DIRECTION ( 'NONE',  ( -0.000000000000000000, 1.000000000000000000, -0.000000000000000000 ) ) ;
#69020 = CARTESIAN_POINT ( 'NONE',  ( -0.1640419947506553400, -0.05778040916215560624, -0.4822834645669293319 ) ) ;
#69021 = CARTESIAN_POINT ( 'NONE',  ( -1.253280839895012377, -0.3162353388693409650, -0.4822834645669289433 ) ) ;
#69022 = CARTESIAN_POINT ( 'NONE',  ( -1.561679790026246017, -0.4281496062992127816, -0.4176697321401328100 ) ) ;
#69023 = CARTESIAN_POINT ( 'NONE',  ( 0.4314295484911171985, 1.339559522712171491, -2.637768908735144358 ) ) ;
#69024 = CARTESIAN_POINT ( 'NONE',  ( -9.594673741351313045E-17, 0.3917322834645670104, -2.761811023622046779 ) ) ;
#69025 = CARTESIAN_POINT ( 'NONE',  ( 0.9842519685039378130, -0.5511811023622047445, 6.969142054262312111E-17 ) ) ;
#69026 = ORIENTED_EDGE ( 'NONE', *, *, #66425, .T. ) ;
#69027 = CARTESIAN_POINT ( 'NONE',  ( 0.2891555358219910499, -0.2891555358219909944, -0.2559055118110237226 ) ) ;
#69028 = CARTESIAN_POINT ( 'NONE',  ( -0.7874015748031489847, -0.1870078740157480879, -0.4822834645669291653 ) ) ;
#69029 = VERTEX_POINT ( 'NONE', #75444 ) ;
#69030 = CARTESIAN_POINT ( 'NONE',  ( -0.01312335958005186876, -0.3690944881889763329, 0.3153832671262228327 ) ) ;
#69031 = CARTESIAN_POINT ( 'NONE',  ( 0.4724409448818895907, 0.1265901696524994180, -0.1246719160104987345 ) ) ;
#69032 = CARTESIAN_POINT ( 'NONE',  ( 0.5905511811023629321, -0.6692913385826771977, 8.415575281601705876E-17 ) ) ;
#69033 = CARTESIAN_POINT ( 'NONE',  ( 0.4002624671916016896, -0.3162353388693409650, -0.4822834645669289433 ) ) ;
#69034 = CARTESIAN_POINT ( 'NONE',  ( -0.4002624671916004129, -0.05778040916215560624, -0.4822834645669293319 ) ) ;
#69035 = AXIS2_PLACEMENT_3D ( 'NONE', #12810, #30911, #11985 ) ;
#69036 = CARTESIAN_POINT ( 'NONE',  ( -0.3917322834645670104, -0.1049643490035307020, -1.302512754102049142 ) ) ;
#69037 = CARTESIAN_POINT ( 'NONE',  ( -1.364829396325458521, -0.6046776061558807314, 0.2411417322834647770 ) ) ;
#69038 = CARTESIAN_POINT ( 'NONE',  ( 0.2867679344610365999, -0.2867679344610365444, -2.860236220472440749 ) ) ;
#69039 = CARTESIAN_POINT ( 'NONE',  ( 1.351706036745407458, -0.3690944881889765550, -0.3153832671262227771 ) ) ;
#69040 = CARTESIAN_POINT ( 'NONE',  ( -1.207349081364828436, -0.6046776061558807314, 0.2411417322834647770 ) ) ;
#69041 = CARTESIAN_POINT ( 'NONE',  ( 0.7217847769028878924, 0.05413385826771666132, 0.4176697321401328100 ) ) ;
#69042 = CARTESIAN_POINT ( 'NONE',  ( 1.108923884514436686, -0.3162353388693409650, -0.4822834645669289433 ) ) ;
#69043 = EDGE_CURVE ( 'NONE', #78537, #40878, #62735, .T. ) ;
#69044 = CARTESIAN_POINT ( 'NONE',  ( 0.1070741851644053527, 0.3996062992125986590, -0.7808398950131233418 ) ) ;
#69045 = CARTESIAN_POINT ( 'NONE',  ( -1.213910761154854745, 0.2952755905511810774, -0.1292274648535930714 ) ) ;
#69046 = CARTESIAN_POINT ( 'NONE',  ( -0.1998031496062991630, -0.3460692066303959202, -0.1423884514435695414 ) ) ;
#69047 = CARTESIAN_POINT ( 'NONE',  ( 0.2559055118110243332, -0.5400638737290845981, -0.3530559997133363437 ) ) ;
#69048 = CARTESIAN_POINT ( 'NONE',  ( -0.3996062992125986035, -7.340648628747425578E-17, -2.086614173228346303 ) ) ;
#69049 = CARTESIAN_POINT ( 'NONE',  ( 0.2867679344610365999, -0.2867679344610365444, -1.600393700787401619 ) ) ;
#69050 = CARTESIAN_POINT ( 'NONE',  ( -1.397637795275589623, -0.4536011799217368745, -0.2665933059059886201 ) ) ;
#69051 = CARTESIAN_POINT ( 'NONE',  ( 0.4658792650918641698, -0.08942795157528024563, -0.3641732283464568787 ) ) ;
#69052 = CARTESIAN_POINT ( 'NONE',  ( 1.017060367454068581, -0.05778040916215560624, -0.4822834645669293319 ) ) ;
#69053 = CARTESIAN_POINT ( 'NONE',  ( 0.4724409448818898682, 2.892866454678787531E-17, -0.9822834645669291653 ) ) ;
#69054 = CARTESIAN_POINT ( 'NONE',  ( 0.8005249343832028242, -0.3690944881889765550, -0.3153832671262227771 ) ) ;
#69055 = CARTESIAN_POINT ( 'NONE',  ( 0.3871391076115492380, -0.05778040916215560624, -0.4822834645669293319 ) ) ;
#69056 = CARTESIAN_POINT ( 'NONE',  ( 4.837279021331061486E-17, -0.3949938075777409963, -0.9429133858267715329 ) ) ;
#69057 = CARTESIAN_POINT ( 'NONE',  ( -0.7349081364829390672, 0.2306618581243847221, -0.2411417322834647770 ) ) ;
#69058 = DIRECTION ( 'NONE',  ( -3.491481338843132961E-15, -0.000000000000000000, 1.000000000000000000 ) ) ;
#69059 = DIMENSIONAL_EXPONENTS ( 1.000000000000000000, 0.000000000000000000, 0.000000000000000000, 0.000000000000000000, 0.000000000000000000, 0.000000000000000000, 0.000000000000000000 ) ;
#69060 = CARTESIAN_POINT ( 'NONE',  ( 1.108923884514436242, -0.08942795157527998196, 0.3641732283464567121 ) ) ;
#69061 = CARTESIAN_POINT ( 'NONE',  ( 0.01968503937007930540, 0.1660481256975885056, 0.3530559997133364547 ) ) ;
#69062 = CARTESIAN_POINT ( 'NONE',  ( 0.1181102362204730916, 0.2066929133858268208, 0.000000000000000000 ) ) ;
#69063 = CARTESIAN_POINT ( 'NONE',  ( -0.1246719160104980823, 0.2952755905511811885, 0.1292274648535926551 ) ) ;
#69064 = CARTESIAN_POINT ( 'NONE',  ( -0.06561679790026180015, -0.004921259842519576551, 0.3153832671262227771 ) ) ;
#69065 = CARTESIAN_POINT ( 'NONE',  ( -2.610466197084866824, 1.379671404989095018, -0.4476723508032712240 ) ) ;
#69066 = CARTESIAN_POINT ( 'NONE',  ( -0.5052493438320203589, -0.6692913385826771977, 0.1292274648535927661 ) ) ;
#69067 = CARTESIAN_POINT ( 'NONE',  ( 0.7480314960629927956, -0.5511811023622047445, 6.969142054262312111E-17 ) ) ;
#69068 = FACE_OUTER_BOUND ( 'NONE', #18725, .T. ) ;
#69069 = CARTESIAN_POINT ( 'NONE',  ( -0.1070741851644051862, -0.3996062992125986590, -1.723753280839895208 ) ) ;
#69070 = CARTESIAN_POINT ( 'NONE',  ( 0.4921259842519691285, -0.5400638737290845981, -0.3530559997133363437 ) ) ;
#69071 = EDGE_CURVE ( 'NONE', #48388, #24500, #24891, .T. ) ;
#69072 = CARTESIAN_POINT ( 'NONE',  ( 0.1049643490035304938, -0.3917322834645669549, -1.494750656167978642 ) ) ;
#69073 = CARTESIAN_POINT ( 'NONE',  ( 1.246719160104987623, -0.004921259842519870586, -0.3153832671262229437 ) ) ;
#69074 = CARTESIAN_POINT ( 'NONE',  ( -0.1698998578625667832, -2.609869883881465018E-15, -0.3464511005275220379 ) ) ;
#69075 = CARTESIAN_POINT ( 'NONE',  ( -0.2165354330708654795, -0.4536011799217368745, -0.2665933059059886201 ) ) ;
#69076 = CARTESIAN_POINT ( 'NONE',  ( -0.9120734908136475250, 0.1771653543307087630, 0.09757992244046791164 ) ) ;
#69077 = CARTESIAN_POINT ( 'NONE',  ( -0.1246719160104980823, -0.6692913385826773087, -0.1292274648535924053 ) ) ;
#69078 = CARTESIAN_POINT ( 'NONE',  ( 1.036745406824147731, -0.004921259842519576551, 0.3153832671262227771 ) ) ;
#69079 = CARTESIAN_POINT ( 'NONE',  ( 0.3853249588699879657, 1.260224081467387958, -1.053849663494103250 ) ) ;
#69080 = CARTESIAN_POINT ( 'NONE',  ( -1.660104986876639543, -0.05778040916215560624, -0.4822834645669293319 ) ) ;
#69081 = AXIS2_PLACEMENT_3D ( 'NONE', #68838, #62936, #10364 ) ;
#69082 = CARTESIAN_POINT ( 'NONE',  ( 0.03937007874015833325, -0.6692913385826771977, 8.415575281601705876E-17 ) ) ;
#69083 = ADVANCED_FACE ( 'NONE', ( #45494 ), #32883, .F. ) ;
#69084 = CARTESIAN_POINT ( 'NONE',  ( 0.5577427821522316087, -0.05778040916215522460, 0.4822834645669289988 ) ) ;
#69085 = LINE ( 'NONE', #12665, #58504 ) ;
#69086 = CARTESIAN_POINT ( 'NONE',  ( 0.2755905511811031494, -0.6692913385826771977, 8.415575281601705876E-17 ) ) ;
#69087 = CARTESIAN_POINT ( 'NONE',  ( -9.594673741351313045E-17, 0.3917322834645670104, -1.187007874015748143 ) ) ;
#69088 = CARTESIAN_POINT ( 'NONE',  ( 0.6824146981627303710, -0.6046776061558807314, 0.2411417322834647770 ) ) ;
#69089 = CARTESIAN_POINT ( 'NONE',  ( 0.6824146981627303710, -0.6046776061558807314, 0.2411417322834647770 ) ) ;
#69090 = DIRECTION ( 'NONE',  ( 0.000000000000000000, 1.000000000000000000, -0.000000000000000000 ) ) ;
#69091 = CARTESIAN_POINT ( 'NONE',  ( 0.2821522309711292364, 0.1771653543307087075, -0.09757992244046823083 ) ) ;
#69092 = CARTESIAN_POINT ( 'NONE',  ( 1.200787401574803681, 0.1660481256975885056, 0.3530559997133364547 ) ) ;
#69093 = CARTESIAN_POINT ( 'NONE',  ( 0.006561679790026889343, -0.08942795157527998196, 0.3641732283464567121 ) ) ;
#69094 = CARTESIAN_POINT ( 'NONE',  ( -0.1509186351706028884, -0.3162353388693409650, -0.4822834645669289433 ) ) ;
#69095 = CARTESIAN_POINT ( 'NONE',  ( 0.3018372703412079971, -0.4281496062992124485, 0.4176697321401328655 ) ) ;
#69096 = CARTESIAN_POINT ( 'NONE',  ( -0.7808398950131222316, -0.3162353388693409650, -0.4822834645669289433 ) ) ;
#69097 = CARTESIAN_POINT ( 'NONE',  ( -0.4658792650918627265, -0.08942795157527998196, 0.3641732283464567121 ) ) ;
#69098 = CARTESIAN_POINT ( 'NONE',  ( 1.010498687664042716, 0.05413385826771626580, -0.4176697321401330321 ) ) ;
#69099 = CARTESIAN_POINT ( 'NONE',  ( 1.135170603674541256, -0.5511811023622048555, -0.09757992244046775898 ) ) ;
#69100 = CARTESIAN_POINT ( 'NONE',  ( 0.2034120734908144990, -0.6692913385826771977, 0.1292274648535927661 ) ) ;
#69101 = DIRECTION ( 'NONE',  ( -0.000000000000000000, 1.000000000000000000, -0.000000000000000000 ) ) ;
#69103 = CARTESIAN_POINT ( 'NONE',  ( -9.787531504996567848E-17, 0.3996062992125986035, -1.102362204724409489 ) ) ;
#69102 = LINE ( 'NONE', #17770, #45960 ) ;
#69104 = CARTESIAN_POINT ( 'NONE',  ( 1.614173228346457378, -0.6692913385826771977, 8.415575281601705876E-17 ) ) ;
#69105 = CARTESIAN_POINT ( 'NONE',  ( 0.1181102362204724532, 0.09842519685039372024, 0.000000000000000000 ) ) ;
#69106 = CARTESIAN_POINT ( 'NONE',  ( -1.240157480314959759, -0.5400638737290845981, -0.3530559997133363437 ) ) ;
#69107 = CARTESIAN_POINT ( 'NONE',  ( -0.8595800524934373854, -0.3162353388693409650, -0.4822834645669289433 ) ) ;
#69108 = CARTESIAN_POINT ( 'NONE',  ( -0.4724409448818895907, -0.1265901696524993070, -0.3608923884514435576 ) ) ;
#69109 = CARTESIAN_POINT ( 'NONE',  ( 0.1058382717557500713, -0.3949938075777409408, -2.919947506561680228 ) ) ;
#69110 = ORIENTED_EDGE ( 'NONE', *, *, #31423, .F. ) ;
#69111 = CARTESIAN_POINT ( 'NONE',  ( 0.5118110236220480003, -0.5511811023622047445, 6.969142054262312111E-17 ) ) ;
#69112 = CARTESIAN_POINT ( 'NONE',  ( -0.1049643490035302024, -0.3917322834645671215, -1.481627296587926690 ) ) ;
#69113 = CARTESIAN_POINT ( 'NONE',  ( 0.4855643044619428750, 0.05413385826771666132, 0.4176697321401328100 ) ) ;
#69114 = CARTESIAN_POINT ( 'NONE',  ( 0.2362204724409451007, -0.4091458600556402980, -2.454068241469816058 ) ) ;
#69115 = CARTESIAN_POINT ( 'NONE',  ( 0.9564677561141817774, 0.02791078216816225699, 0.4328096321851905293 ) ) ;
#69116 = DIRECTION ( 'NONE',  ( 1.000000000000000000, 0.000000000000000000, 0.000000000000000000 ) ) ;
#69117 = CARTESIAN_POINT ( 'NONE',  ( 1.181102362204725198, -0.1870078740157479769, 0.4822834645669291653 ) ) ;
#69118 = CARTESIAN_POINT ( 'NONE',  ( 1.200787401574803681, -0.4536011799217368745, -0.2665933059059886201 ) ) ;
#69119 = CARTESIAN_POINT ( 'NONE',  ( -0.09186351706036663400, -0.4281496062992124485, 0.4176697321401328655 ) ) ;
#69120 = CARTESIAN_POINT ( 'NONE',  ( -0.1958661417322834497, -0.3392501089628018884, -0.6180909204386334510 ) ) ;
#69121 = CARTESIAN_POINT ( 'NONE',  ( -0.4658792650918627265, -0.3162353388693409650, -0.4822834645669289433 ) ) ;
#69122 = CARTESIAN_POINT ( 'NONE',  ( -0.7939632545931754048, -0.2845877964562159024, 0.3641732283464567677 ) ) ;
#69123 = CARTESIAN_POINT ( 'NONE',  ( 0.2755905511811031494, -0.6692913385826771977, 8.415575281601705876E-17 ) ) ;
#69124 = CARTESIAN_POINT ( 'NONE',  ( -0.2821522309711278487, 0.2952755905511811885, 0.1292274648535926551 ) ) ;
#69125 = CARTESIAN_POINT ( 'NONE',  ( 1.614173228346457378, -0.6692913385826771977, 8.415575281601705876E-17 ) ) ;
#69126 = CARTESIAN_POINT ( 'NONE',  ( -0.03411923929626390489, 1.063910482648554146, -1.851245305700470967 ) ) ;
#69127 = EDGE_LOOP ( 'NONE', ( #30981, #81068, #11652, #16578 ) ) ;
#69128 = CARTESIAN_POINT ( 'NONE',  ( -0.3917322834645670104, -0.1049643490035307020, -2.089914328905198904 ) ) ;
#69129 = CARTESIAN_POINT ( 'NONE',  ( 0.5183727034120741983, -0.6692913385826771977, 0.1292274648535927661 ) ) ;
#69130 = CARTESIAN_POINT ( 'NONE',  ( -0.3280839895013117347, -0.4281496062992124485, 0.4176697321401328655 ) ) ;
#69131 = CARTESIAN_POINT ( 'NONE',  ( -1.633858267716534529, 0.1660481256975885056, 0.3530559997133364547 ) ) ;
#69132 = CARTESIAN_POINT ( 'NONE',  ( 0.7611548556430451917, -0.6046776061558807314, 0.2411417322834647770 ) ) ;
#69133 = CARTESIAN_POINT ( 'NONE',  ( 0.5643044619422579178, 0.05413385826771666132, 0.4176697321401328100 ) ) ;
#69134 = CARTESIAN_POINT ( 'NONE',  ( 0.3917322834645669549, 0.1049643490035304660, -1.311679790026246906 ) ) ;
#69135 = CARTESIAN_POINT ( 'NONE',  ( -0.6889763779527552368, -0.5400638737290845981, -0.3530559997133363437 ) ) ;
#69136 = CARTESIAN_POINT ( 'NONE',  ( 0.1574803149606306130, -0.1870078740157480879, -0.4822834645669291653 ) ) ;
#69137 = CARTESIAN_POINT ( 'NONE',  ( -0.2755905511811015396, -0.6692913385826771977, 8.415575281601705876E-17 ) ) ;
#69138 = VECTOR ( 'NONE', #67522, 39.37007874015748143 ) ;
#69139 = CARTESIAN_POINT ( 'NONE',  ( 0.3740157480314966754, -0.4536011799217367080, 0.2665933059059888421 ) ) ;
#69140 = CARTESIAN_POINT ( 'NONE',  ( -1.719160104986876103, 0.05413385826771666132, 0.4176697321401328100 ) ) ;
#69141 = DIRECTION ( 'NONE',  ( -0.000000000000000000, -1.000000000000000000, -1.408710688920637755E-15 ) ) ;
#69142 = ADVANCED_FACE ( 'NONE', ( #57704 ), #67, .F. ) ;
#69143 = CARTESIAN_POINT ( 'NONE',  ( -0.1771653543307080136, -0.5400638737290844871, 0.3530559997133364547 ) ) ;
#69144 = CARTESIAN_POINT ( 'NONE',  ( 0.3458507752293908943, -0.3458507752293908943, -0.9625984251968502381 ) ) ;
#69145 = CARTESIAN_POINT ( 'NONE',  ( 1.469816272965879911, 0.2306618581243847221, -0.2411417322834647770 ) ) ;
#69146 = CARTESIAN_POINT ( 'NONE',  ( -0.2867679344610365999, 0.2867679344610364889, -2.688976377952755570 ) ) ;
#69147 = ORIENTED_EDGE ( 'NONE', *, *, #50692, .F. ) ;
#69148 = ORIENTED_EDGE ( 'NONE', *, *, #12912, .T. ) ;
#69149 = CARTESIAN_POINT ( 'NONE',  ( 0.8267716535433078384, -0.6692913385826771977, 8.415575281601705876E-17 ) ) ;
#69150 = CARTESIAN_POINT ( 'NONE',  ( -0.05249343832020938322, -0.5023911411419708095, -0.1820866141732282451 ) ) ;
#69152 = CARTESIAN_POINT ( 'NONE',  ( -1.614173228346457378, 1.606230626554505658, 0.1372047244094476981 ) ) ;
#69151 = DIRECTION ( 'NONE',  ( 1.000000000000000000, 0.000000000000000000, 1.047444401652940007E-14 ) ) ;
#69153 = CARTESIAN_POINT ( 'NONE',  ( 0.1958661417322834775, 0.3392501089628018884, -1.173884514435695525 ) ) ;
#69154 = CARTESIAN_POINT ( 'NONE',  ( 0.1265901696524990294, -0.4724409448818896462, 0.1528871391076115360 ) ) ;
#69155 = DIRECTION ( 'NONE',  ( -1.000000000000000000, -0.000000000000000000, -0.000000000000000000 ) ) ;
#69156 = CARTESIAN_POINT ( 'NONE',  ( 0.1070741851644053388, 0.3996062992125986035, -2.747375328083988766 ) ) ;
#69157 = CARTESIAN_POINT ( 'NONE',  ( 0.3346456692913390985, 0.1660481256975885056, 0.3530559997133364547 ) ) ;
#69158 = CARTESIAN_POINT ( 'NONE',  ( -1.318897637795274802, 0.1660481256975885056, 0.3530559997133364547 ) ) ;
#69159 = CARTESIAN_POINT ( 'NONE',  ( -1.233595800524933894, 0.2306618581243848609, 0.2411417322834645549 ) ) ;
#69160 = CARTESIAN_POINT ( 'NONE',  ( 0.3674540682414705883, 0.2306618581243847221, -0.2411417322834647770 ) ) ;
#69161 = CARTESIAN_POINT ( 'NONE',  ( 1.128608923884514947, 0.2306618581243848609, 0.2411417322834645549 ) ) ;
#69162 = CARTESIAN_POINT ( 'NONE',  ( 1.463254593175853824, -0.5511811023622046335, 0.09757992244046803654 ) ) ;
#69163 = CARTESIAN_POINT ( 'NONE',  ( 1.345144356955381593, -0.08942795157527998196, 0.3641732283464567121 ) ) ;
#69164 = CARTESIAN_POINT ( 'NONE',  ( -1.010498687664041384, 0.05413385826771666132, 0.4176697321401328100 ) ) ;
#69165 = CARTESIAN_POINT ( 'NONE',  ( -0.1998031496062994405, 0.3460692066303957537, -0.5623359580052492701 ) ) ;
#69166 = CARTESIAN_POINT ( 'NONE',  ( 1.607611548556431069, -0.6692913385826773087, -0.1292274648535924053 ) ) ;
#69167 = CARTESIAN_POINT ( 'NONE',  ( -0.3392501089628019995, 0.1958661417322832277, -0.1758530183727033402 ) ) ;
#69168 = CARTESIAN_POINT ( 'NONE',  ( -0.1377952755905504645, -0.5400638737290845981, -0.3530559997133363437 ) ) ;
#69170 = CARTESIAN_POINT ( 'NONE',  ( -0.01711686753222916441, 1.062992125984252301, 1.850393700787401619 ) ) ;
#69169 = CARTESIAN_POINT ( 'NONE',  ( 1.095800524934383846, -0.05778040916215560624, -0.4822834645669293319 ) ) ;
#69171 = CARTESIAN_POINT ( 'NONE',  ( -1.391076115485563758, 0.1283753931104748280, 0.1820866141732283561 ) ) ;
#69172 = CARTESIAN_POINT ( 'NONE',  ( 0.2952755905511819101, 0.1660481256975883668, -0.3530559997133364547 ) ) ;
#69173 = CARTESIAN_POINT ( 'NONE',  ( 0.8005249343832027131, -0.004921259842519576551, 0.3153832671262227771 ) ) ;
#69174 = CARTESIAN_POINT ( 'NONE',  ( -1.338582677165353729, -0.1870078740157480601, -0.3641732283464567677 ) ) ;
#69175 = CARTESIAN_POINT ( 'NONE',  ( 1.128608923884515169, -0.6046776061558809534, -0.2411417322834644161 ) ) ;
#69176 = CARTESIAN_POINT ( 'NONE',  ( -0.5411721830064186722, -2.191421614605370878E-15, 0.4445507791589071167 ) ) ;
#69177 = CARTESIAN_POINT ( 'NONE',  ( -0.5839895013123351797, 0.1771653543307087075, -0.09757992244046823083 ) ) ;
#69178 = CARTESIAN_POINT ( 'NONE',  ( -0.8070866141732276899, -0.5400638737290844871, 0.3530559997133364547 ) ) ;
#69179 = CARTESIAN_POINT ( 'NONE',  ( 1.469816272965879911, -0.6046776061558807314, 0.2411417322834647770 ) ) ;
#69180 = CARTESIAN_POINT ( 'NONE',  ( -0.7611548556430438595, 0.2306618581243848609, 0.2411417322834645549 ) ) ;
#69181 = CARTESIAN_POINT ( 'NONE',  ( 1.561679790026247350, 0.05413385826771626580, -0.4176697321401330321 ) ) ;
#69182 = CARTESIAN_POINT ( 'NONE',  ( 0.3392501089628018329, 0.1958661417322835607, -0.9153736464905005699 ) ) ;
#69183 = CARTESIAN_POINT ( 'NONE',  ( -0.7480314960629914633, -0.5511811023622047445, 6.969142054262312111E-17 ) ) ;
#69184 = CARTESIAN_POINT ( 'NONE',  ( 1.121720580570839010, 1.063763119642385124, -0.03131331025603343449 ) ) ;
#69185 = B_SPLINE_CURVE_WITH_KNOTS ( 'NONE', 3,
 ( #18566, #49714, #5513, #44209 ),
 .UNSPECIFIED., .F., .F.,
 ( 4, 4 ),
 ( 3.210432057660995851E-07, 0.001287787053612100526 ),
 .UNSPECIFIED. ) ;
#69186 = CARTESIAN_POINT ( 'NONE',  ( 1.266404199475066328, -0.05778040916215522460, 0.4822834645669289988 ) ) ;
#69187 = CARTESIAN_POINT ( 'NONE',  ( 0.1265901696524990294, -0.4724409448818896462, -1.894356955380577023 ) ) ;
#69188 = CARTESIAN_POINT ( 'NONE',  ( -0.09023630363247998887, 1.809133623825372073E-16, -0.3791483426435173776 ) ) ;
#69189 = CARTESIAN_POINT ( 'NONE',  ( 1.666666666666667185, 0.05413385826771666132, 0.4176697321401328100 ) ) ;
#69190 = CARTESIAN_POINT ( 'NONE',  ( -1.161417322834644716, -0.4536011799217368745, -0.2665933059059886201 ) ) ;
#69191 = ADVANCED_FACE ( 'NONE', ( #64873 ), #81635, .F. ) ;
#69193 = CARTESIAN_POINT ( 'NONE',  ( 0.7998211177050879028, 0.000000000000000000, 0.3464511005275205946 ) ) ;
#69192 =( BOUNDED_CURVE ( )  B_SPLINE_CURVE ( 2, ( #5946, #37110, #24477, #56459, #82562, #62794, #24881, #68693, #56046, #50549, #30379, #37932, #76253, #50143, #75840, #31615, #50959, #62368, #81754, #63609, #18182, #82974, #12274, #49323, #75024, #76656, #70333, #25293, #36693, #75433, #57276, #44636, #5536, #17370, #12689, #55629, #38348, #4706, #81338, #17773, #23652, #24065, #44230, #69920, #43814, #11868, #37521, #29964, #43000, #11035, #43405, #31201, #77919, #19833, #58965, #14786, #72436, #46744, #65719, #45058, #6776, #26131, #13110, #1322, #1732, #46325, #39605, #71596, #78760, #78341, #52216, #59373, #33712, #14374, #32448, #72018, #65294, #45899, #13948, #64440, #40442, #58110, #40031, #33304, #39177, #64861, #8050, #27388, #38763, #476, #53049, #7199, #51793, #26971, #77497, #13521, #70759, #52636, #21085, #20672, #6363, #32035, #57694, #7633, #77073, #56, #25710, #51370, #45482, #19407, #71179, #32871, #58539, #905, #26562, #20250, #35783, #59789, #54298, #2143, #80012, #27811, #53471, #22327, #79594, #35372, #74512, #48813, #23144 ),
 .UNSPECIFIED., .F., .F. ) 
 B_SPLINE_CURVE_WITH_KNOTS ( ( 3, 2, 2, 2, 2, 2, 2, 2, 2, 2, 2, 2, 2, 2, 2, 2, 2, 2, 2, 2, 2, 2, 2, 2, 2, 2, 2, 2, 2, 2, 2, 2, 2, 2, 2, 2, 2, 2, 2, 2, 2, 2, 2, 2, 2, 2, 2, 2, 2, 2, 2, 2, 2, 2, 2, 2, 2, 2, 2, 2, 2, 2, 2, 2, 3 ),
 ( 0.6649931759405284248, 0.6666666666666666297, 0.6708333333333332815, 0.6750000000000000444, 0.6791666666666666963, 0.6833333333333333481, 0.6875000000000000000, 0.6916666666666666519, 0.6958333333333333037, 0.6999999999999999556, 0.7041666666666667185, 0.7083333333333333703, 0.7125000000000000222, 0.7166666666666666741, 0.7208333333333333259, 0.7249999999999999778, 0.7291666666666666297, 0.7333333333333332815, 0.7375000000000000444, 0.7416666666666666963, 0.7458333333333333481, 0.7500000000000000000, 0.7541666666666666519, 0.7583333333333333037, 0.7624999999999999556, 0.7666666666666667185, 0.7708333333333333703, 0.7750000000000000222, 0.7791666666666666741, 0.7833333333333333259, 0.7874999999999999778, 0.7916666666666666297, 0.7958333333333332815, 0.8000000000000000444, 0.8041666666666666963, 0.8083333333333333481, 0.8125000000000000000, 0.8166666666666666519, 0.8208333333333333037, 0.8249999999999999556, 0.8291666666666667185, 0.8333333333333333703, 0.8375000000000000222, 0.8416666666666666741, 0.8458333333333333259, 0.8499999999999999778, 0.8541666666666666297, 0.8583333333333332815, 0.8625000000000000444, 0.8666666666666666963, 0.8708333333333333481, 0.8750000000000000000, 0.8791666666666666519, 0.8833333333333333037, 0.8874999999999999556, 0.8916666666666667185, 0.8958333333333333703, 0.9000000000000000222, 0.9041666666666666741, 0.9083333333333333259, 0.9124999999999999778, 0.9166666666666666297, 0.9208333333333332815, 0.9250000000000000444, 0.9274931759404547726 ),
 .UNSPECIFIED. ) 
 CURVE ( )  GEOMETRIC_REPRESENTATION_ITEM ( )  RATIONAL_B_SPLINE_CURVE ( ( 0.9836222570913433216, 0.9863145247105440383, 1.000000000000000000, 0.9659258262890683122, 1.000000000000000000, 0.9659258262890683122, 1.000000000000000000, 0.9659258262890683122, 1.000000000000000000, 0.9659258262890683122, 1.000000000000000000, 0.9659258262890683122, 1.000000000000000000, 0.9659258262890683122, 1.000000000000000000, 0.9659258262890683122, 1.000000000000000000, 0.9659258262890683122, 1.000000000000000000, 0.9659258262890683122, 1.000000000000000000, 0.9659258262890683122, 1.000000000000000000, 0.9659258262890683122, 1.000000000000000000, 0.9659258262890683122, 1.000000000000000000, 0.9659258262890683122, 1.000000000000000000, 0.9659258262890683122, 1.000000000000000000, 0.9659258262890683122, 1.000000000000000000, 0.9659258262890683122, 1.000000000000000000, 0.9659258262890683122, 1.000000000000000000, 0.9659258262890683122, 1.000000000000000000, 0.9659258262890683122, 1.000000000000000000, 0.9659258262890683122, 1.000000000000000000, 0.9659258262890683122, 1.000000000000000000, 0.9659258262890683122, 1.000000000000000000, 0.9659258262890683122, 1.000000000000000000, 0.9659258262890683122, 1.000000000000000000, 0.9659258262890683122, 1.000000000000000000, 0.9659258262890683122, 1.000000000000000000, 0.9659258262890683122, 1.000000000000000000, 0.9659258262890683122, 1.000000000000000000, 0.9659258262890683122, 1.000000000000000000, 0.9659258262890683122, 1.000000000000000000, 0.9659258262890683122, 1.000000000000000000, 0.9659258262890683122, 1.000000000000000000, 0.9659258262890683122, 1.000000000000000000, 0.9659258262890683122, 1.000000000000000000, 0.9659258262890683122, 1.000000000000000000, 0.9659258262890683122, 1.000000000000000000, 0.9659258262890683122, 1.000000000000000000, 0.9659258262890683122, 1.000000000000000000, 0.9659258262890683122, 1.000000000000000000, 0.9659258262890683122, 1.000000000000000000, 0.9659258262890683122, 1.000000000000000000, 0.9659258262890683122, 1.000000000000000000, 0.9659258262890683122, 1.000000000000000000, 0.9659258262890683122, 1.000000000000000000, 0.9659258262890683122, 1.000000000000000000, 0.9659258262890683122, 1.000000000000000000, 0.9659258262890683122, 1.000000000000000000, 0.9659258262890683122, 1.000000000000000000, 0.9659258262890683122, 1.000000000000000000, 0.9659258262890683122, 1.000000000000000000, 0.9659258262890683122, 1.000000000000000000, 0.9659258262890683122, 1.000000000000000000, 0.9659258262890683122, 1.000000000000000000, 0.9659258262890683122, 1.000000000000000000, 0.9659258262890683122, 1.000000000000000000, 0.9659258262890683122, 1.000000000000000000, 0.9659258262890683122, 1.000000000000000000, 0.9659258262890683122, 1.000000000000000000, 0.9659258262890683122, 1.000000000000000000, 0.9659258262890683122, 1.000000000000000000, 0.9659258262890683122, 1.000000000000000000, 0.9659258262890683122, 1.000000000000000000, 0.9796113015791271250, 0.9836222570911059560 ) ) 
 REPRESENTATION_ITEM ( '' )  );
#69194 = CARTESIAN_POINT ( 'NONE',  ( -0.4724409448818890911, -0.1870078740157480879, -0.4822834645669291653 ) ) ;
#69195 = CARTESIAN_POINT ( 'NONE',  ( 0.1246719160104994284, 0.1771653543307087075, -0.09757992244046823083 ) ) ;
#69196 = CARTESIAN_POINT ( 'NONE',  ( -0.9776902887139098386, -0.5511811023622046335, 0.09757992244046803654 ) ) ;
#69197 = CARTESIAN_POINT ( 'NONE',  ( 1.410761154855643795, -0.2845877964562159024, 0.3641732283464567677 ) ) ;
#69198 = CARTESIAN_POINT ( 'NONE',  ( 1.122047244094488860, -0.5400638737290845981, -0.3530559997133363437 ) ) ;
#69199 = CARTESIAN_POINT ( 'NONE',  ( 1.928577636452524918E-17, 0.7086614173228346081, 0.1574803149606299746 ) ) ;
#69200 = CARTESIAN_POINT ( 'NONE',  ( 0.4790026246719168435, -0.2845877964562161244, -0.3641732283464567121 ) ) ;
#69201 = AXIS2_PLACEMENT_3D ( 'NONE', #56616, #69679, #12022 ) ;
#69202 = CARTESIAN_POINT ( 'NONE',  ( 0.4396325459317593221, 0.2952755905511810774, -0.1292274648535930714 ) ) ;
#69203 = ADVANCED_FACE ( 'NONE', ( #7646 ), #6373, .F. ) ;
#69204 = CARTESIAN_POINT ( 'NONE',  ( 0.8989501312335963501, -0.5511811023622048555, -0.09757992244046775898 ) ) ;
#69205 = VERTEX_POINT ( 'NONE', #44648 ) ;
#69206 = CARTESIAN_POINT ( 'NONE',  ( -1.240157480314959759, -0.5400638737290845981, -0.3530559997133363437 ) ) ;
#69207 = CARTESIAN_POINT ( 'NONE',  ( -1.286089238845143479, 0.2306618581243847221, -0.2411417322834647770 ) ) ;
#69208 = CARTESIAN_POINT ( 'NONE',  ( 5.463695987328526437E-16, -0.1870078740157479769, 0.4822834645669291653 ) ) ;
#69209 = DIRECTION ( 'NONE',  ( -1.000000000000000000, 0.000000000000000000, 0.000000000000000000 ) ) ;
#69210 = CARTESIAN_POINT ( 'NONE',  ( -0.1998031496062994405, 0.3460692066303957537, -2.767060367454068359 ) ) ;
#69211 = CARTESIAN_POINT ( 'NONE',  ( 0.5905511811023629321, -0.6692913385826771977, 8.415575281601705876E-17 ) ) ;
#69212 = CARTESIAN_POINT ( 'NONE',  ( -1.627296587926508442, -0.6046776061558809534, -0.2411417322834644161 ) ) ;
#69213 = CARTESIAN_POINT ( 'NONE',  ( -0.1574803149606292529, -0.1870078740157480879, -0.4822834645669291653 ) ) ;
#69214 = CARTESIAN_POINT ( 'NONE',  ( 0.1837270341207354329, 0.2306618581243848609, 0.2411417322834645549 ) ) ;
#69215 = CARTESIAN_POINT ( 'NONE',  ( 0.3460692066303959202, 0.1998031496062993295, -2.178477690288713742 ) ) ;
#69216 = AXIS2_PLACEMENT_3D ( 'NONE', #47295, #72572, #35512 ) ;
#69217 = CARTESIAN_POINT ( 'NONE',  ( -0.3949938075777409408, -0.1058382717557502933, -1.620734908136483243 ) ) ;
#69218 = CARTESIAN_POINT ( 'NONE',  ( -0.1998031496062994683, 0.3460692066303958092, -2.690288713910760965 ) ) ;
#69219 = DIRECTION ( 'NONE',  ( 3.096699300667737957E-16, -1.000000000000000000, 0.000000000000000000 ) ) ;
#69220 = CARTESIAN_POINT ( 'NONE',  ( -0.1958661417322836718, 0.3392501089628017219, -0.6351706036745405903 ) ) ;
#69221 = CARTESIAN_POINT ( 'NONE',  ( -0.3805774278215216522, -0.3690944881889765550, -0.3153832671262227771 ) ) ;
#69222 = CARTESIAN_POINT ( 'NONE',  ( -0.5446194225721777693, -0.3162353388693409650, -0.4822834645669289433 ) ) ;
#69223 = CARTESIAN_POINT ( 'NONE',  ( 0.3083989501312343062, -0.3162353388693405765, 0.4822834645669290543 ) ) ;
#69224 = CARTESIAN_POINT ( 'NONE',  ( 0.3949938075777409963, 2.418639510665530743E-17, -2.399606299212599048 ) ) ;
#69225 = EDGE_CURVE ( 'NONE', #21842, #65017, #45070, .T. ) ;
#69226 = CARTESIAN_POINT ( 'NONE',  ( 0.7611548556430454138, 0.2306618581243847221, -0.2411417322834647770 ) ) ;
#69227 = CARTESIAN_POINT ( 'NONE',  ( 1.515748031496063186, -0.5400638737290845981, -0.3530559997133363437 ) ) ;
#69228 = CARTESIAN_POINT ( 'NONE',  ( 0.6889763779527563470, 0.1660481256975883668, -0.3530559997133364547 ) ) ;
#69229 = CARTESIAN_POINT ( 'NONE',  ( 0.3458507752293908943, 0.3458507752293908943, -2.814960629921259727 ) ) ;
#69230 = CARTESIAN_POINT ( 'NONE',  ( -0.3996062992125986035, -7.340648628747425578E-17, -2.244094488188976388 ) ) ;
#69231 = CARTESIAN_POINT ( 'NONE',  ( 1.653543307086614789, -0.1870078740157479769, 0.4822834645669291653 ) ) ;
#69232 = CARTESIAN_POINT ( 'NONE',  ( 0.7217847769028878924, -0.4281496062992127816, -0.4176697321401328100 ) ) ;
#69233 = CARTESIAN_POINT ( 'NONE',  ( 0.4658792650918640033, -0.3162353388693405765, 0.4822834645669290543 ) ) ;
#69234 = EDGE_CURVE ( 'NONE', #65182, #77311, #2322, .T. ) ;
#69235 = CARTESIAN_POINT ( 'NONE',  ( 1.108923884514436242, -0.08942795157527998196, 0.3641732283464567121 ) ) ;
#69237 = CARTESIAN_POINT ( 'NONE',  ( -1.496062992125983815, -0.1870078740157479769, 0.4822834645669291653 ) ) ;
#69236 = CARTESIAN_POINT ( 'NONE',  ( -1.555118110236219930, -0.4536011799217368745, -0.2665933059059886201 ) ) ;
#69238 = CARTESIAN_POINT ( 'NONE',  ( 4.797336870675656522E-17, -0.3917322834645670104, -0.1633858267716536417 ) ) ;
#69239 = CARTESIAN_POINT ( 'NONE',  ( -2.787279214012418738, 0.000000000000000000, 0.000000000000000000 ) ) ;
#69240 = CARTESIAN_POINT ( 'NONE',  ( 0.8333333333333340365, -0.6692913385826771977, 0.1292274648535927661 ) ) ;
#69241 = CARTESIAN_POINT ( 'NONE',  ( 1.463254593175853824, -0.5511811023622046335, 0.09757992244046803654 ) ) ;
#69242 = CARTESIAN_POINT ( 'NONE',  ( -0.5839895013123351797, 0.2952755905511810774, -0.1292274648535930714 ) ) ;
#69243 = CARTESIAN_POINT ( 'NONE',  ( -0.9317585301837263412, 0.05413385826771666132, 0.4176697321401328100 ) ) ;
#69244 = CARTESIAN_POINT ( 'NONE',  ( 1.213910761154856299, -0.6692913385826773087, -0.1292274648535924053 ) ) ;
#69245 = B_SPLINE_CURVE_WITH_KNOTS ( 'NONE', 3,
 ( #35216, #60879, #3230, #43984 ),
 .UNSPECIFIED., .F., .F.,
 ( 4, 4 ),
 ( 3.593986969204291827E-07, 0.001287825409103184960 ),
 .UNSPECIFIED. ) ;
#69246 = CARTESIAN_POINT ( 'NONE',  ( 4.797336870675656522E-17, -0.3917322834645670104, -0.4783464566929135353 ) ) ;
#69247 = CARTESIAN_POINT ( 'NONE',  ( 0.3392501089628018329, 0.1958661417322835607, -1.383202099737532942 ) ) ;
#69248 = CARTESIAN_POINT ( 'NONE',  ( 0.1049643490035304938, -0.3917322834645669549, -2.912073490813647858 ) ) ;
#69249 = EDGE_CURVE ( 'NONE', #4549, #9936, #45298, .T. ) ;
#69250 = CARTESIAN_POINT ( 'NONE',  ( 1.640419947506562393, -0.4281496062992124485, 0.4176697321401328655 ) ) ;
#69251 = VERTEX_POINT ( 'NONE', #63619 ) ;
#69252 = CARTESIAN_POINT ( 'NONE',  ( -0.3420746716998659953, -0.1974969037888706647, -2.887139107611548461 ) ) ;
#69253 = ORIENTED_EDGE ( 'NONE', *, *, #64052, .T. ) ;
#69254 = CARTESIAN_POINT ( 'NONE',  ( 3.937007874015748143, 1.724409448818898127, 0.6299212598425202314 ) ) ;
#69255 = CARTESIAN_POINT ( 'NONE',  ( 1.456692913385827515, 0.1771653543307087630, 0.000000000000000000 ) ) ;
#69256 = CARTESIAN_POINT ( 'NONE',  ( 4.893765752498283924E-17, -0.3996062992125986035, -1.338582677165354173 ) ) ;
#69257 = CARTESIAN_POINT ( 'NONE',  ( 1.692913385826772421, 0.1771653543307087630, 0.000000000000000000 ) ) ;
#69258 = CARTESIAN_POINT ( 'NONE',  ( -0.1443569553805768291, 0.009842519685039463617, 0.3409548833797002576 ) ) ;
#69259 = LINE ( 'NONE', #75169, #66525 ) ;
#69260 = FACE_OUTER_BOUND ( 'NONE', #7955, .T. ) ;
#69261 = CARTESIAN_POINT ( 'NONE',  ( 4.797336870675656522E-17, -0.3917322834645670104, -0.4783464566929135353 ) ) ;
#69262 = CARTESIAN_POINT ( 'NONE',  ( -0.9055118110236215490, -0.5511811023622047445, 6.969142054262312111E-17 ) ) ;
#69263 = CARTESIAN_POINT ( 'NONE',  ( -1.213910761154854745, 0.1771653543307087075, -0.09757992244046823083 ) ) ;
#69264 = CARTESIAN_POINT ( 'NONE',  ( -1.286089238845143479, 0.2306618581243847221, -0.2411417322834647770 ) ) ;
#69265 = CARTESIAN_POINT ( 'NONE',  ( 0.2887139107611556010, -0.6046776061558807314, 0.2411417322834647770 ) ) ;
#69266 = CARTESIAN_POINT ( 'NONE',  ( -1.397637795275589623, -0.5400638737290845981, -0.3530559997133363437 ) ) ;
#69267 = ORIENTED_EDGE ( 'NONE', *, *, #9067, .F. ) ;
#69268 = CARTESIAN_POINT ( 'NONE',  ( 1.574803149606299746, -0.1870078740157479769, 0.4822834645669291653 ) ) ;
#69269 = CARTESIAN_POINT ( 'NONE',  ( -1.161417322834644716, 0.1012011053420777407, 0.2882089793578256898 ) ) ;
#69270 = CARTESIAN_POINT ( 'NONE',  ( 0.1265901696524989462, 0.4724409448818897572, -2.198162729658792447 ) ) ;
#69271 = CARTESIAN_POINT ( 'NONE',  ( -0.4359958488159582091, 1.724409448818897905, -3.937007874015763687 ) ) ;
#69272 = CARTESIAN_POINT ( 'NONE',  ( -0.6430446194225712953, -0.004921259842519870586, -0.3153832671262229437 ) ) ;
#69273 = CARTESIAN_POINT ( 'NONE',  ( -1.056430446194224881, -0.6692913385826771977, 0.1292274648535927661 ) ) ;
#69274 = CARTESIAN_POINT ( 'NONE',  ( 1.207349081364829990, 0.2306618581243848609, 0.2411417322834645549 ) ) ;
#69275 = AXIS2_PLACEMENT_3D ( 'NONE', #83053, #44310, #38428 ) ;
#69276 = ORIENTED_EDGE ( 'NONE', *, *, #76445, .T. ) ;
#69278 = CARTESIAN_POINT ( 'NONE',  ( -1.603475055217291612, 1.606158680897942670, 0.04573490813648253134 ) ) ;
#69277 = CARTESIAN_POINT ( 'NONE',  ( 0.4091458600556404646, -0.2362204724409448231, -2.309711286089239035 ) ) ;
#69279 = CARTESIAN_POINT ( 'NONE',  ( 1.568241469816273659, -0.05778040916215560624, -0.4822834645669293319 ) ) ;
#69280 = CARTESIAN_POINT ( 'NONE',  ( -1.404199475065615932, 0.05413385826771666132, 0.4176697321401328100 ) ) ;
#69281 = CARTESIAN_POINT ( 'NONE',  ( 0.3917322834645668994, 0.1049643490035304522, -0.3621854086276097839 ) ) ;
#69282 = CARTESIAN_POINT ( 'NONE',  ( 0.1902887139107617975, 0.1771653543307087630, 0.09757992244046791164 ) ) ;
#69283 = CARTESIAN_POINT ( 'NONE',  ( -0.2867679344610366554, 0.2867679344610365444, -0.7342519685039371469 ) ) ;
#69284 = CARTESIAN_POINT ( 'NONE',  ( -0.2559055118110227234, -0.4536011799217367080, 0.2665933059059888421 ) ) ;
#69285 = CARTESIAN_POINT ( 'NONE',  ( 0.3674540682414705883, 0.1283753931104746893, -0.1820866141732285504 ) ) ;
#69286 = CARTESIAN_POINT ( 'NONE',  ( 0.7283464566929140904, -0.5400638737290845981, -0.3530559997133363437 ) ) ;
#69287 = CARTESIAN_POINT ( 'NONE',  ( -0.6496062992125976043, 0.07958543189024071263, -0.2665933059059888421 ) ) ;
#69288 = CARTESIAN_POINT ( 'NONE',  ( 0.3392501089628018884, -0.1958661417322834220, -2.616797900262466836 ) ) ;
#69289 = CARTESIAN_POINT ( 'NONE',  ( 1.095800524934383846, -0.3162353388693405765, 0.4822834645669290543 ) ) ;
#69290 = CARTESIAN_POINT ( 'NONE',  ( -1.108923884514435132, -0.05778040916215560624, -0.4822834645669293319 ) ) ;
#69291 = CARTESIAN_POINT ( 'NONE',  ( 0.4724409448818897572, -0.1265901696524988906, -0.9757217847769029673 ) ) ;
#69292 = CARTESIAN_POINT ( 'NONE',  ( 0.2230971128608929543, 0.05413385826771626580, -0.4176697321401330321 ) ) ;
#69293 = EDGE_CURVE ( 'NONE', #42318, #55143, #25587, .T. ) ;
#69294 = CARTESIAN_POINT ( 'NONE',  ( -0.3215223097112853146, -0.05778040916215560624, -0.4822834645669293319 ) ) ;
#69295 = CARTESIAN_POINT ( 'NONE',  ( 1.404199475065617708, -0.004921259842519870586, -0.3153832671262229437 ) ) ;
#69296 = CARTESIAN_POINT ( 'NONE',  ( 0.2493438320209980519, -0.3690944881889765550, -0.3153832671262227771 ) ) ;
#69297 = CARTESIAN_POINT ( 'NONE',  ( -0.1377952755905504645, 0.1660481256975885056, 0.3530559997133364547 ) ) ;
#69298 = CARTESIAN_POINT ( 'NONE',  ( -1.128608923884513837, 0.2306618581243847221, -0.2411417322834647770 ) ) ;
#69299 = CARTESIAN_POINT ( 'NONE',  ( 1.968503937007874072, 2.049113738730800541E-17, 5.859448621221250875 ) ) ;
#69300 = CARTESIAN_POINT ( 'NONE',  ( 1.692913385826772421, 0.1771653543307087630, 0.000000000000000000 ) ) ;
#69301 = CARTESIAN_POINT ( 'NONE',  ( -0.2230971128608915943, 0.05413385826771666132, 0.4176697321401328100 ) ) ;
#69302 = CARTESIAN_POINT ( 'NONE',  ( -1.102362204724408601, -0.1870078740157479769, 0.4822834645669291653 ) ) ;
#69303 = VERTEX_POINT ( 'NONE', #25304 ) ;
#69304 = CARTESIAN_POINT ( 'NONE',  ( 0.1070741851644054776, -0.3996062992125984925, -2.051837270341206665 ) ) ;
#69305 = CARTESIAN_POINT ( 'NONE',  ( 0.9711286089238851948, 0.2306618581243848609, 0.2411417322834645549 ) ) ;
#69306 = CARTESIAN_POINT ( 'NONE',  ( -0.5183727034120726440, -0.5511811023622048555, -0.09757992244046775898 ) ) ;
#69307 = CARTESIAN_POINT ( 'NONE',  ( -0.5839895013123351797, 0.2952755905511810774, -0.1292274648535930714 ) ) ;
#69308 = CARTESIAN_POINT ( 'NONE',  ( 1.286089238845145033, -0.6046776061558809534, -0.2411417322834644161 ) ) ;
#69309 = CARTESIAN_POINT ( 'NONE',  ( 0.8530183727034128527, -0.4281496062992124485, 0.4176697321401328655 ) ) ;
#69310 = CARTESIAN_POINT ( 'NONE',  ( -0.3438254193631122835, 0.3704879858182167918, -0.01311675794578955577 ) ) ;
#69311 = CARTESIAN_POINT ( 'NONE',  ( -1.259842519685038686, -0.1870078740157479769, 0.3641732283464567677 ) ) ;
#69312 = CARTESIAN_POINT ( 'NONE',  ( -0.1070741851644051862, -0.3996062992125986035, -0.6213910761154856077 ) ) ;
#69313 = CARTESIAN_POINT ( 'NONE',  ( 0.3460692066303959202, 0.1998031496062993295, -1.076115485564304475 ) ) ;
#69314 = CARTESIAN_POINT ( 'NONE',  ( 0.1974969037888706369, -0.3420746716998659953, -0.4068241469816273326 ) ) ;
#69315 = CARTESIAN_POINT ( 'NONE',  ( 0.3535010496217478315, 1.220715222164475922, -1.393813936465888359 ) ) ;
#69316 = CARTESIAN_POINT ( 'NONE',  ( 1.286089238845145033, -0.5023911411419708095, -0.1820866141732282451 ) ) ;
#69317 = CARTESIAN_POINT ( 'NONE',  ( 0.9120734908136489683, -0.5511811023622046335, 0.09757992244046803654 ) ) ;
#69318 = CARTESIAN_POINT ( 'NONE',  ( 0.6824146981627303710, 0.2306618581243847221, -0.2411417322834647770 ) ) ;
#69319 = CARTESIAN_POINT ( 'NONE',  ( 0.3503937007874015630, 0.3733313776025732333, -0.4921259842519685179 ) ) ;
#69320 = CARTESIAN_POINT ( 'NONE',  ( -0.3420746716998662729, 0.1974969037888702206, -1.362860892388451539 ) ) ;
#69321 = CARTESIAN_POINT ( 'NONE',  ( 0.9514435695538062676, -0.2845877964562161244, -0.3641732283464567121 ) ) ;
#69322 =( BOUNDED_CURVE ( )  B_SPLINE_CURVE ( 2, ( #63192, #37106, #13106, #11449, #44226, #45054, #70329, #81750, #51366, #18178, #64018, #62790, #37928 ),
 .UNSPECIFIED., .F., .F. ) 
 B_SPLINE_CURVE_WITH_KNOTS ( ( 3, 2, 2, 2, 2, 2, 3 ),
 ( 0.8217605387524145044, 0.8219696969696970168, 0.8257575757575758013, 0.8295454545454545858, 0.8333333333333333703, 0.8371212121212121549, 0.8373303703384946672 ),
 .UNSPECIFIED. ) 
 CURVE ( )  GEOMETRIC_REPRESENTATION_ITEM ( )  RATIONAL_B_SPLINE_CURVE ( ( 0.9964447847208419695, 0.9981185001348091834, 1.000000000000000000, 0.9659258262890683122, 1.000000000000000000, 0.9659258262890683122, 1.000000000000000000, 0.9659258262890683122, 1.000000000000000000, 0.9659258262890683122, 1.000000000000000000, 0.9981185001348091834, 0.9964447847208420805 ) ) 
 REPRESENTATION_ITEM ( '' )  );
#69323 = CARTESIAN_POINT ( 'NONE',  ( -0.1509186351706028884, -0.3162353388693409650, -0.4822834645669289433 ) ) ;
#69324 = CARTESIAN_POINT ( 'NONE',  ( -1.305774278215222184, 0.2952755905511811885, 0.1292274648535926551 ) ) ;
#69325 = CARTESIAN_POINT ( 'NONE',  ( 1.082677165354331228, 0.1660481256975883668, -0.3530559997133364547 ) ) ;
#69326 = CARTESIAN_POINT ( 'NONE',  ( 0.1265901696524989462, 0.4724409448818897572, -1.095800524934382958 ) ) ;
#69327 = CYLINDRICAL_SURFACE ( 'NONE', #59993, 0.5118110236220471121 ) ;
#69328 = AXIS2_PLACEMENT_3D ( 'NONE', #60262, #23089, #59012 ) ;
#69329 = CARTESIAN_POINT ( 'NONE',  ( 0.01968503937007930540, 0.07958543189024085140, 0.2665933059059887866 ) ) ;
#69330 = ORIENTED_EDGE ( 'NONE', *, *, #29978, .F. ) ;
#69331 = VERTEX_POINT ( 'NONE', #57287 ) ;
#69332 = CARTESIAN_POINT ( 'NONE',  ( -0.9776902887139098386, -0.6692913385826771977, 0.1292274648535927661 ) ) ;
#69333 = CARTESIAN_POINT ( 'NONE',  ( -0.5314960629921250401, 0.1660481256975885056, 0.3530559997133364547 ) ) ;
#69334 = CARTESIAN_POINT ( 'NONE',  ( -0.3740157480314953431, 0.1660481256975885056, 0.3530559997133364547 ) ) ;
#69335 = CARTESIAN_POINT ( 'NONE',  ( 0.4265091863517067594, 0.2952755905511811885, 0.1292274648535926551 ) ) ;
#69336 = CARTESIAN_POINT ( 'NONE',  ( -0.5446194225721777693, -0.05778040916215522460, 0.4822834645669289988 ) ) ;
#69337 = CARTESIAN_POINT ( 'NONE',  ( -1.502624671916009680, -0.3162353388693405765, 0.4822834645669290543 ) ) ;
#69338 = CARTESIAN_POINT ( 'NONE',  ( -0.7742782152230965886, 0.05413385826771666132, 0.4176697321401328100 ) ) ;
#69339 = CARTESIAN_POINT ( 'NONE',  ( 0.5643044619422579178, -0.4281496062992127816, -0.4176697321401328100 ) ) ;
#69340 = CARTESIAN_POINT ( 'NONE',  ( 4.797336870675656522E-17, -0.3917322834645670104, -1.015748031496062964 ) ) ;
#69341 = CARTESIAN_POINT ( 'NONE',  ( -0.2362204724409440182, -0.1870078740157479769, 0.3641732283464567677 ) ) ;
#69342 = VERTEX_POINT ( 'NONE', #19419 ) ;
#69343 = CARTESIAN_POINT ( 'NONE',  ( -0.2891555358219911054, 0.2891555358219909388, -1.437007874015748143 ) ) ;
#69344 = ORIENTED_EDGE ( 'NONE', *, *, #20359, .F. ) ;
#69345 = CARTESIAN_POINT ( 'NONE',  ( -1.154855643044618851, -0.5023911411419708095, -0.1820866141732282451 ) ) ;
#69346 = CARTESIAN_POINT ( 'NONE',  ( -0.9251968503937002541, -0.5400638737290845981, -0.3530559997133363437 ) ) ;
#69347 = CARTESIAN_POINT ( 'NONE',  ( -0.8398950131233585692, 0.2306618581243848609, 0.2411417322834645549 ) ) ;
#69348 = CARTESIAN_POINT ( 'NONE',  ( -0.3996062992125987146, 0.1070741851644051862, -0.03280839895013124008 ) ) ;
#69349 = CARTESIAN_POINT ( 'NONE',  ( -0.7611548556430438595, 0.2306618581243848609, 0.2411417322834645549 ) ) ;
#69350 = CARTESIAN_POINT ( 'NONE',  ( -0.9908136482939626788, -0.6692913385826773087, -0.1292274648535924053 ) ) ;
#69351 = CARTESIAN_POINT ( 'NONE',  ( -1.541994750656167090, -0.6692913385826773087, -0.1292274648535924053 ) ) ;
#69352 = DIRECTION ( 'NONE',  ( 1.000000000000000000, -1.445602896647338917E-16, 0.000000000000000000 ) ) ;
#69353 = CARTESIAN_POINT ( 'NONE',  ( 0.7020997375328090762, -0.2845877964562159024, 0.3641732283464567677 ) ) ;
#69354 = DIRECTION ( 'NONE',  ( -3.491481338843132961E-15, -0.000000000000000000, 1.000000000000000000 ) ) ;
#69355 = CARTESIAN_POINT ( 'NONE',  ( -0.1049643490035307020, 0.3917322834645669549, 0.2237532808398949025 ) ) ;
#69356 = CARTESIAN_POINT ( 'NONE',  ( 0.2230971128608929543, -0.004921259842519870586, -0.3153832671262229437 ) ) ;
#69357 = CARTESIAN_POINT ( 'NONE',  ( -0.3149606299212590610, -0.1870078740157480879, -0.4822834645669291653 ) ) ;
#69358 = CARTESIAN_POINT ( 'NONE',  ( 1.351706036745407458, -0.4281496062992127816, -0.4176697321401328100 ) ) ;
#69359 = CARTESIAN_POINT ( 'NONE',  ( -0.006561679790025524116, -0.05778040916215560624, -0.4822834645669293319 ) ) ;
#69360 = VERTEX_POINT ( 'NONE', #32460 ) ;
#69361 = CARTESIAN_POINT ( 'NONE',  ( 0.2925321140481932369, -0.2925321140481932369, -1.988188976377952777 ) ) ;
#69362 = CARTESIAN_POINT ( 'NONE',  ( 0.2469196488504588338, 2.056812631849083806E-16, 0.4118484887281962381 ) ) ;
#69363 = ORIENTED_EDGE ( 'NONE', *, *, #76206, .F. ) ;
#69364 = CARTESIAN_POINT ( 'NONE',  ( -0.2925321140481930149, -0.2925321140481933480, -1.710629921259842812 ) ) ;
#69365 = CARTESIAN_POINT ( 'NONE',  ( -0.1474713956048439301, -2.191421614605370878E-15, 0.4445507791589071167 ) ) ;
#69366 = CARTESIAN_POINT ( 'NONE',  ( -1.181102362204723644, -0.1870078740157480601, -0.3641732283464567677 ) ) ;
#69367 = CARTESIAN_POINT ( 'NONE',  ( -1.548556430446193399, 0.2306618581243848609, 0.2411417322834645549 ) ) ;
#69368 = CARTESIAN_POINT ( 'NONE',  ( 0.1265901696524989462, 0.4724409448818897572, -0.3083989501312335846 ) ) ;
#69369 = LINE ( 'NONE', #44086, #26423 ) ;
#69370 = CARTESIAN_POINT ( 'NONE',  ( -0.3917322834645669549, -0.1049643490035306603, 0.1194225721784776956 ) ) ;
#69371 = CARTESIAN_POINT ( 'NONE',  ( 1.476377952755906442, -0.5400638737290844871, 0.3530559997133364547 ) ) ;
#69372 = AXIS2_PLACEMENT_3D ( 'NONE', #20102, #75794, #43770 ) ;
#69373 = CARTESIAN_POINT ( 'NONE',  ( 0.3149606299212603933, -0.1870078740157479769, 0.4822834645669291653 ) ) ;
#69374 = CARTESIAN_POINT ( 'NONE',  ( 0.2821522309711292364, 0.2952755905511810774, -0.1292274648535930714 ) ) ;
#69375 = CARTESIAN_POINT ( 'NONE',  ( -0.9514435695538050464, -0.08942795157528024563, -0.3641732283464568787 ) ) ;
#69376 = CARTESIAN_POINT ( 'NONE',  ( -0.1509186351706028884, -0.05778040916215522460, 0.4822834645669289988 ) ) ;
#69377 = CARTESIAN_POINT ( 'NONE',  ( -0.2362204724409447953, -0.4091458600556404646, -2.347112860892388575 ) ) ;
#69378 = CARTESIAN_POINT ( 'NONE',  ( -0.9908136482939626788, -0.6692913385826773087, -0.1292274648535924053 ) ) ;
#69379 = CARTESIAN_POINT ( 'NONE',  ( -0.1058382717557497660, -0.3949938075777411073, -2.196194225721785021 ) ) ;
#69380 = CARTESIAN_POINT ( 'NONE',  ( 1.450131233595801428, 0.1771653543307087630, 0.09757992244046791164 ) ) ;
#69381 = CARTESIAN_POINT ( 'NONE',  ( -0.2559055118110230564, 0.07958543189024071263, -0.2665933059059888421 ) ) ;
#69382 = CARTESIAN_POINT ( 'NONE',  ( 1.174540682414699111, -0.2845877964562159024, 0.3641732283464567677 ) ) ;
#69383 = CARTESIAN_POINT ( 'NONE',  ( -1.541994750656167090, 0.2952755905511811885, 0.1292274648535926551 ) ) ;
#69384 = CARTESIAN_POINT ( 'NONE',  ( -1.187664041994749731, -0.2845877964562159024, 0.3641732283464567677 ) ) ;
#69385 = CARTESIAN_POINT ( 'NONE',  ( 0.4687286201624460968, 1.750728371878951917, 0.5180200956804293932 ) ) ;
#69386 = CARTESIAN_POINT ( 'NONE',  ( 0.6627296587926517768, -0.5511811023622048555, -0.09757992244046775898 ) ) ;
#69387 = CARTESIAN_POINT ( 'NONE',  ( -0.9448818897637790704, -0.1870078740157480879, -0.4822834645669291653 ) ) ;
#69388 = VECTOR ( 'NONE', #19146, 39.37007874015748143 ) ;
#69389 = CARTESIAN_POINT ( 'NONE',  ( -1.882930639362831116, 1.098283573398308954, 0.1802708669123980201 ) ) ;
#69390 = CARTESIAN_POINT ( 'NONE',  ( -0.07874015748031421014, -0.1870078740157479769, 0.3641732283464567677 ) ) ;
#69391 = CARTESIAN_POINT ( 'NONE',  ( -1.476377952755905110, -0.4536011799217368745, -0.2665933059059886201 ) ) ;
#69392 = ADVANCED_FACE ( 'NONE', ( #58122 ), #25003, .T. ) ;
#69393 = CARTESIAN_POINT ( 'NONE',  ( 0.7086614173228353852, -0.1870078740157479769, 0.4822834645669291653 ) ) ;
#69394 = CARTESIAN_POINT ( 'NONE',  ( 0.6430446194225728496, 0.05413385826771666132, 0.4176697321401328100 ) ) ;
#69395 = CARTESIAN_POINT ( 'NONE',  ( 1.410761154855643795, -0.2845877964562159024, 0.3641732283464567677 ) ) ;
#69396 = CARTESIAN_POINT ( 'NONE',  ( -0.8070866141732276899, -0.5400638737290844871, 0.3530559997133364547 ) ) ;
#69397 = CARTESIAN_POINT ( 'NONE',  ( -0.2230971128608915943, -0.004921259842519576551, 0.3153832671262227771 ) ) ;
#69398 = CARTESIAN_POINT ( 'NONE',  ( -0.7330015572057683171, 1.982446682556143980, 0.5178628694646268960 ) ) ;
#69399 = CARTESIAN_POINT ( 'NONE',  ( 0.3543307086614179147, 0.1771653543307087630, 0.000000000000000000 ) ) ;
#69400 = CARTESIAN_POINT ( 'NONE',  ( -1.102362204724408601, -0.1870078740157479769, 0.4822834645669291653 ) ) ;
#69401 = CARTESIAN_POINT ( 'NONE',  ( -0.5643044619422565855, -0.4281496062992124485, 0.4176697321401328655 ) ) ;
#69402 = CARTESIAN_POINT ( 'NONE',  ( 0.3996062992125984925, 0.1070741851644054637, -0.8313648293963252778 ) ) ;
#69403 = CARTESIAN_POINT ( 'NONE',  ( 0.1049643490035303689, 0.3917322834645670104, -2.440288713910760521 ) ) ;
#69404 = CARTESIAN_POINT ( 'NONE',  ( 0.4593175853018379162, -0.3690944881889763329, 0.3153832671262228327 ) ) ;
#69405 = CARTESIAN_POINT ( 'NONE',  ( -0.4790026246719152336, -0.05778040916215560624, -0.4822834645669293319 ) ) ;
#69406 = CARTESIAN_POINT ( 'NONE',  ( -0.7414698162729651543, -0.6692913385826771977, 0.1292274648535927661 ) ) ;
#69407 = CARTESIAN_POINT ( 'NONE',  ( -0.9908136482939626788, 0.1771653543307087630, 0.09757992244046791164 ) ) ;
#69408 = CARTESIAN_POINT ( 'NONE',  ( -3.936915166329627347, 1.063759665227983708, -0.03114301994267879015 ) ) ;
#69409 = CARTESIAN_POINT ( 'NONE',  ( 0.1312335958005257930, 0.2306618581243847221, -0.2411417322834647770 ) ) ;
#69410 = CARTESIAN_POINT ( 'NONE',  ( -1.574803149606298636, -0.1870078740157479769, 0.3641732283464567677 ) ) ;
#69411 = CARTESIAN_POINT ( 'NONE',  ( -1.555118110236219930, -0.5400638737290845981, -0.3530559997133363437 ) ) ;
#69412 = PLANE ( 'NONE',  #11193 ) ;
#69413 = ORIENTED_EDGE ( 'NONE', *, *, #32546, .F. ) ;
#69414 = DIRECTION ( 'NONE',  ( -0.000000000000000000, -1.000000000000000000, -0.000000000000000000 ) ) ;
#69415 = CARTESIAN_POINT ( 'NONE',  ( -1.430446194225721390, -0.4281496062992124485, 0.4176697321401328655 ) ) ;
#69416 = CARTESIAN_POINT ( 'NONE',  ( -0.9580052493438311334, -0.4281496062992124485, 0.4176697321401328655 ) ) ;
#69417 = CARTESIAN_POINT ( 'NONE',  ( 1.541994750656168645, -0.6692913385826771977, 0.1292274648535927661 ) ) ;
#69418 = CARTESIAN_POINT ( 'NONE',  ( 0.1049643490035303689, 0.3917322834645670104, -2.125328083989501682 ) ) ;
#69419 = CARTESIAN_POINT ( 'NONE',  ( 0.1789624963018512649, 0.3486222174624337145, -1.220472440944881276 ) ) ;
#69420 = CARTESIAN_POINT ( 'NONE',  ( 1.141732283464567788, -0.6692913385826771977, 8.415575281601705876E-17 ) ) ;
#69421 = CARTESIAN_POINT ( 'NONE',  ( 0.5839895013123367340, 0.2952755905511811885, 0.1292274648535926551 ) ) ;
#69422 = CARTESIAN_POINT ( 'NONE',  ( -2.554262525012222174, 1.537401574803149984, 0.4744094488188970171 ) ) ;
#69423 = AXIS2_PLACEMENT_3D ( 'NONE', #46617, #8746, #40316 ) ;
#69425 = CARTESIAN_POINT ( 'NONE',  ( 0.2925321140481931814, 0.2925321140481931814, -2.261811023622047223 ) ) ;
#69424 = CIRCLE ( 'NONE', #82942, 3.937007874015748143 ) ;
#69426 = CARTESIAN_POINT ( 'NONE',  ( 1.187664041994751285, -0.2845877964562161244, -0.3641732283464567121 ) ) ;
#69427 = CARTESIAN_POINT ( 'NONE',  ( 0.2925321140481932369, 0.2925321140481932369, -1.082677165354330562 ) ) ;
#69428 = ORIENTED_EDGE ( 'NONE', *, *, #890, .F. ) ;
#69429 = CARTESIAN_POINT ( 'NONE',  ( 0.1958661417322834775, 0.3392501089628018884, -2.656167979002624691 ) ) ;
#69430 = EDGE_LOOP ( 'NONE', ( #45304, #55361 ) ) ;
#69431 = CARTESIAN_POINT ( 'NONE',  ( 0.4855643044619428750, 0.05413385826771666132, 0.4176697321401328100 ) ) ;
#69432 = CARTESIAN_POINT ( 'NONE',  ( -0.6299212598425188991, -0.1870078740157479769, 0.4822834645669291653 ) ) ;
#69433 = CARTESIAN_POINT ( 'NONE',  ( 1.548556430446194954, -0.6046776061558807314, 0.2411417322834647770 ) ) ;
#69434 = CARTESIAN_POINT ( 'NONE',  ( 0.9842519685039378130, -0.6692913385826771977, 8.415575281601705876E-17 ) ) ;
#69435 = CARTESIAN_POINT ( 'NONE',  ( 1.679790026246720025, 0.2306618581243848609, 0.2411417322834645549 ) ) ;
#69436 = CARTESIAN_POINT ( 'NONE',  ( -1.306827173596996738, 0.000000000000000000, -0.4445507791589060620 ) ) ;
#69437 = CARTESIAN_POINT ( 'NONE',  ( 0.07874015748031558404, -0.1870078740157479769, 0.4822834645669291653 ) ) ;
#69438 = CARTESIAN_POINT ( 'NONE',  ( -1.135170603674539924, 0.2952755905511810774, -0.1292274648535930714 ) ) ;
#69439 = CARTESIAN_POINT ( 'NONE',  ( -1.509186351706035767, -0.4281496062992124485, 0.4176697321401328655 ) ) ;
#69440 = B_SPLINE_CURVE_WITH_KNOTS ( 'NONE', 3,
 ( #44109, #19272, #63891, #12148, #57566, #75302, #37805, #5816, #75715, #83258 ),
 .UNSPECIFIED., .F., .F.,
 ( 4, 2, 2, 2, 4 ),
 ( 0.000000000000000000, 0.001551611299846697217, 0.002327416949770047885, 0.002715319774731722677, 0.003103222599693397903 ),
 .UNSPECIFIED. ) ;
#69441 = CARTESIAN_POINT ( 'NONE',  ( 1.397637795275591177, 0.1660481256975883668, -0.3530559997133364547 ) ) ;
#69442 = CARTESIAN_POINT ( 'NONE',  ( 0.1049643490035304938, -0.3917322834645669549, -2.847112860892388131 ) ) ;
#69443 = CARTESIAN_POINT ( 'NONE',  ( 0.9645669291338591078, -0.4536011799217368745, -0.2665933059059886201 ) ) ;
#69444 = ORIENTED_EDGE ( 'NONE', *, *, #3777, .F. ) ;
#69445 = CARTESIAN_POINT ( 'NONE',  ( -0.2891555358219908833, -0.2891555358219912164, -0.3740157480314962313 ) ) ;
#69446 = ORIENTED_EDGE ( 'NONE', *, *, #46038, .F. ) ;
#69448 = VECTOR ( 'NONE', #65223, 39.37007874015748143 ) ;
#69447 = CARTESIAN_POINT ( 'NONE',  ( 0.03937007874015806264, 0.1771653543307087630, 0.000000000000000000 ) ) ;
#69449 = CARTESIAN_POINT ( 'NONE',  ( 0.1181102362204724532, 0.09842519685039372024, -1.432673802628665356E-17 ) ) ;
#69450 = CARTESIAN_POINT ( 'NONE',  ( 0.7611548556430451917, -0.6046776061558807314, 0.2411417322834647770 ) ) ;
#69451 = CARTESIAN_POINT ( 'NONE',  ( 0.4658792650918640033, -0.3162353388693405765, 0.4822834645669290543 ) ) ;
#69452 = CARTESIAN_POINT ( 'NONE',  ( -0.5446194225721777693, -0.3162353388693409650, -0.4822834645669289433 ) ) ;
#69453 = CARTESIAN_POINT ( 'NONE',  ( 0.3392501089628018329, 0.1958661417322835607, -1.702775221293650443 ) ) ;
#69454 = CARTESIAN_POINT ( 'NONE',  ( -1.003937007874014853, 0.1660481256975885056, 0.3530559997133364547 ) ) ;
#69455 = CARTESIAN_POINT ( 'NONE',  ( -0.1049643490035302024, -0.3917322834645671215, -2.519028871391075786 ) ) ;
#69456 = CARTESIAN_POINT ( 'NONE',  ( 1.358267716535433323, -0.4536011799217368745, -0.2665933059059886201 ) ) ;
#69457 = CARTESIAN_POINT ( 'NONE',  ( -0.9317585301837263412, -0.4281496062992127816, -0.4176697321401328100 ) ) ;
#69458 = CARTESIAN_POINT ( 'NONE',  ( 0.8792650918635177559, 0.05413385826771666132, 0.4176697321401328100 ) ) ;
#69459 = CARTESIAN_POINT ( 'NONE',  ( 0.9973753280839902091, -0.6046776061558807314, 0.2411417322834647770 ) ) ;
#69460 = CARTESIAN_POINT ( 'NONE',  ( -0.3996062992125987146, 0.1070741851644051862, -0.8202099737532806412 ) ) ;
#69461 = CARTESIAN_POINT ( 'NONE',  ( -1.305774278215222184, -0.6692913385826773087, -0.1292274648535924053 ) ) ;
#69462 = CARTESIAN_POINT ( 'NONE',  ( 0.1998031496062994128, -0.3460692066303957537, -0.3261154855643044748 ) ) ;
#69463 = CARTESIAN_POINT ( 'NONE',  ( 0.4133858267716541968, -0.5400638737290845981, -0.3530559997133363437 ) ) ;
#69464 = CARTESIAN_POINT ( 'NONE',  ( 0.2925321140481932369, -0.2925321140481932369, -2.460629921259842146 ) ) ;
#69465 = CARTESIAN_POINT ( 'NONE',  ( -0.3917322834645670104, -7.196005306013484475E-17, -1.698818897637795367 ) ) ;
#69466 = CARTESIAN_POINT ( 'NONE',  ( 1.312335958005250269, -0.6046776061558807314, 0.2411417322834647770 ) ) ;
#69467 = CARTESIAN_POINT ( 'NONE',  ( 0.2099737532808405305, -0.5023911411419708095, 0.1820866141732285504 ) ) ;
#69468 = CARTESIAN_POINT ( 'NONE',  ( 0.8136482939632553313, 0.2306618581243848609, 0.2411417322834645549 ) ) ;
#69469 = CARTESIAN_POINT ( 'NONE',  ( 0.4724409448818896462, 0.1265901696524990294, -0.9888451443569553634 ) ) ;
#69470 = CARTESIAN_POINT ( 'NONE',  ( 0.8858267716535438430, 0.07958543189024085140, 0.2665933059059887866 ) ) ;
#69471 = CARTESIAN_POINT ( 'NONE',  ( 0.4199475065616803948, -0.6046776061558809534, -0.2411417322834644161 ) ) ;
#69472 = CARTESIAN_POINT ( 'NONE',  ( -0.3420746716998662729, 0.1974969037888702206, -0.8904199475065616154 ) ) ;
#69473 = CARTESIAN_POINT ( 'NONE',  ( -0.8989501312335946848, 0.2952755905511810774, -0.1292274648535930714 ) ) ;
#69474 = LINE ( 'NONE', #62323, #63351 ) ;
#69475 = CARTESIAN_POINT ( 'NONE',  ( 0.7677165354330716118, -0.4536011799217367080, 0.2665933059059888421 ) ) ;
#69476 = CARTESIAN_POINT ( 'NONE',  ( 0.09186351706036827158, 0.009842519685039467087, 0.3409548833797002021 ) ) ;
#69477 = CARTESIAN_POINT ( 'NONE',  ( -0.3608923884514428360, -0.6692913385826773087, -0.1292274648535924053 ) ) ;
#69478 = CARTESIAN_POINT ( 'NONE',  ( 0.1246719160104994284, 0.1771653543307087075, -0.09757992244046823083 ) ) ;
#69479 = CARTESIAN_POINT ( 'NONE',  ( -2.759487654322792416, 1.189595890467141759, 0.3229789317950594874 ) ) ;
#69480 = CARTESIAN_POINT ( 'NONE',  ( -0.4855643044619415427, -0.4281496062992124485, 0.4176697321401328655 ) ) ;
#69481 = CARTESIAN_POINT ( 'NONE',  ( 0.5577427821522314977, -0.2845877964562161244, -0.3641732283464567121 ) ) ;
#69482 = VECTOR ( 'NONE', #78552, 39.37007874015748143 ) ;
#69483 = CARTESIAN_POINT ( 'NONE',  ( -0.1998031496062991630, -0.3460692066303959202, -1.717191601049869121 ) ) ;
#69484 = CARTESIAN_POINT ( 'NONE',  ( 0.3018372703412079971, 0.05413385826771626580, -0.4176697321401330321 ) ) ;
#69485 = EDGE_CURVE ( 'NONE', #19643, #38994, #63312, .T. ) ;
#69486 = CIRCLE ( 'NONE', #31855, 3.858267716535433323 ) ;
#69487 = AXIS2_PLACEMENT_3D ( 'NONE', #82602, #11074, #62833 ) ;
#69488 = CARTESIAN_POINT ( 'NONE',  ( 1.069553805774278832, 0.1771653543307087075, -0.09757992244046823083 ) ) ;
#69489 = CARTESIAN_POINT ( 'NONE',  ( 0.1771653543307093459, 0.1660481256975885056, 0.3530559997133364547 ) ) ;
#69490 = CARTESIAN_POINT ( 'NONE',  ( -0.5052493438320203589, -0.5511811023622046335, 0.09757992244046803654 ) ) ;
#69491 = CARTESIAN_POINT ( 'NONE',  ( -0.6627296587926503335, -0.5511811023622046335, 0.09757992244046803654 ) ) ;
#69492 = CARTESIAN_POINT ( 'NONE',  ( -0.3674540682414689785, 0.2306618581243848609, 0.2411417322834645549 ) ) ;
#69493 = CARTESIAN_POINT ( 'NONE',  ( 0.3674540682414705883, 0.2306618581243847221, -0.2411417322834647770 ) ) ;
#69494 = CARTESIAN_POINT ( 'NONE',  ( 0.9055118110236227702, 0.1771653543307087630, 0.000000000000000000 ) ) ;
#69495 = CARTESIAN_POINT ( 'NONE',  ( 0.4490240974115876638, 1.383493637049404423, -1.028295962660220608 ) ) ;
#69496 = CARTESIAN_POINT ( 'NONE',  ( 1.456692913385827515, 0.1771653543307087630, 0.000000000000000000 ) ) ;
#69497 = CARTESIAN_POINT ( 'NONE',  ( 0.8398950131233602345, -0.6046776061558807314, 0.2411417322834647770 ) ) ;
#69498 = CARTESIAN_POINT ( 'NONE',  ( 0.4732434500808813116, 1.503067092966738683, -2.167287614618209179 ) ) ;
#69499 = CARTESIAN_POINT ( 'NONE',  ( -0.4199475065616791736, 0.2306618581243847221, -0.2411417322834647770 ) ) ;
#69500 = CARTESIAN_POINT ( 'NONE',  ( 0.2867679344610365999, 0.2867679344610365999, -1.167322834645669438 ) ) ;
#69501 = CARTESIAN_POINT ( 'NONE',  ( 0.8595800524934390507, -0.3162353388693405765, 0.4822834645669290543 ) ) ;
#69502 = CARTESIAN_POINT ( 'NONE',  ( 0.6496062992125991586, -0.5400638737290845981, -0.3530559997133363437 ) ) ;
#69503 = CARTESIAN_POINT ( 'NONE',  ( -0.4744094488188831948, 1.521917890488208469, -3.908320185825792770 ) ) ;
#69504 = CARTESIAN_POINT ( 'NONE',  ( 0.5118110236220480003, -0.5511811023622047445, 6.969142054262312111E-17 ) ) ;
#69505 = CARTESIAN_POINT ( 'NONE',  ( 1.095800524934383846, -0.05778040916215560624, -0.4822834645669293319 ) ) ;
#69506 = CARTESIAN_POINT ( 'NONE',  ( 0.09186351706036799403, -0.3690944881889765550, -0.3153832671262227771 ) ) ;
#69507 = CARTESIAN_POINT ( 'NONE',  ( -0.4790026246719152336, -0.05778040916215560624, -0.4822834645669293319 ) ) ;
#69508 = DIRECTION ( 'NONE',  ( -1.000000000000000000, 0.000000000000000000, -0.000000000000000000 ) ) ;
#69509 = CARTESIAN_POINT ( 'NONE',  ( 0.1312335958005255154, -0.6046776061558807314, 0.2411417322834647770 ) ) ;
#69510 = CARTESIAN_POINT ( 'NONE',  ( -0.9514435695538050464, -0.05778040916215560624, -0.4822834645669293319 ) ) ;
#69511 = CARTESIAN_POINT ( 'NONE',  ( -0.1443569553805768291, -0.004921259842519576551, 0.3153832671262227771 ) ) ;
#69512 = CARTESIAN_POINT ( 'NONE',  ( 0.5183727034120741983, 0.2952755905511810774, -0.1292274648535930714 ) ) ;
#69513 = CARTESIAN_POINT ( 'NONE',  ( 0.7939632545931766261, -0.2845877964562161244, -0.3641732283464567121 ) ) ;
#69514 = CARTESIAN_POINT ( 'NONE',  ( -0.4133858267716528645, -0.5400638737290844871, 0.3530559997133364547 ) ) ;
#69515 = CARTESIAN_POINT ( 'NONE',  ( 0.3458507752293908943, -0.3458507752293908943, -0.5708661417322833387 ) ) ;
#69517 = CARTESIAN_POINT ( 'NONE',  ( 1.220472440944882386, -0.6692913385826771977, 8.415575281601705876E-17 ) ) ;
#69516 = CARTESIAN_POINT ( 'NONE',  ( -2.154527559055123831, 0.03937007874015747977, 0.4677827689124697264 ) ) ;
#69518 = CARTESIAN_POINT ( 'NONE',  ( 1.561679790026247350, 0.05413385826771626580, -0.4176697321401330321 ) ) ;
#69519 = DIRECTION ( 'NONE',  ( 1.000000000000000000, -1.445602896647338917E-16, 0.000000000000000000 ) ) ;
#69520 = CARTESIAN_POINT ( 'NONE',  ( -1.640419947506561060, 0.05413385826771666132, 0.4176697321401328100 ) ) ;
#69521 = CARTESIAN_POINT ( 'NONE',  ( -0.7283464566929126471, 0.1660481256975883668, -0.3530559997133364547 ) ) ;
#69522 = CARTESIAN_POINT ( 'NONE',  ( -1.157146581871515012E-16, 0.4724409448818898682, -0.3149606299212598381 ) ) ;
#69523 = CARTESIAN_POINT ( 'NONE',  ( -0.2891555358219911054, 0.2891555358219909388, -2.696850393700787496 ) ) ;
#69524 = ORIENTED_EDGE ( 'NONE', *, *, #29978, .T. ) ;
#69525 = CARTESIAN_POINT ( 'NONE',  ( 0.3346456692913393205, -0.4536011799217368745, -0.2665933059059886201 ) ) ;
#69526 = CARTESIAN_POINT ( 'NONE',  ( -0.2867679344610365999, 0.2867679344610364889, -1.271653543307086798 ) ) ;
#69527 = CARTESIAN_POINT ( 'NONE',  ( 0.7480314960629927956, -0.6692913385826771977, 8.415575281601705876E-17 ) ) ;
#69528 = CARTESIAN_POINT ( 'NONE',  ( 0.3458507752293908943, -0.3458507752293908943, -2.460629921259842146 ) ) ;
#69529 = DIRECTION ( 'NONE',  ( -0.000000000000000000, -0.000000000000000000, -1.000000000000000000 ) ) ;
#69530 = CARTESIAN_POINT ( 'NONE',  ( -0.4396325459317577122, -0.5511811023622048555, -0.09757992244046775898 ) ) ;
#69531 = CARTESIAN_POINT ( 'NONE',  ( -0.3503937007874015630, -0.5120078740157480990, -0.4921259842519685179 ) ) ;
#69532 = CARTESIAN_POINT ( 'NONE',  ( 0.9776902887139113929, -0.6692913385826773087, -0.1292274648535924053 ) ) ;
#69533 = CARTESIAN_POINT ( 'NONE',  ( 1.528871391076116026, -0.5511811023622048555, -0.09757992244046775898 ) ) ;
#69534 = CARTESIAN_POINT ( 'NONE',  ( 0.07874015748031558404, -0.1870078740157479769, 0.4822834645669291653 ) ) ;
#69535 = CARTESIAN_POINT ( 'NONE',  ( -0.2867679344610366554, 0.2867679344610365444, -0.8871197918297093477 ) ) ;
#69536 = CARTESIAN_POINT ( 'NONE',  ( -0.5839895013123351797, -0.6692913385826771977, 0.1292274648535927661 ) ) ;
#69537 = CARTESIAN_POINT ( 'NONE',  ( -1.496062992125983815, -0.1870078740157480601, -0.3641732283464567677 ) ) ;
#69538 = CARTESIAN_POINT ( 'NONE',  ( -0.4461942257217840213, 0.2306618581243848609, 0.2411417322834645549 ) ) ;
#69539 = DIRECTION ( 'NONE',  ( 0.000000000000000000, -1.000000000000000000, -0.000000000000000000 ) ) ;
#69540 = VECTOR ( 'NONE', #28181, 39.37007874015748143 ) ;
#69541 = CARTESIAN_POINT ( 'NONE',  ( -0.5314960629921324786, 2.716535433070866645, 1.854472803289050509 ) ) ;
#69542 = ORIENTED_EDGE ( 'NONE', *, *, #57357, .T. ) ;
#69543 = CARTESIAN_POINT ( 'NONE',  ( 0.2867679344610366554, 0.2867679344610366554, -2.024297531004936701 ) ) ;
#69544 = CARTESIAN_POINT ( 'NONE',  ( 0.2559055118110243332, 0.1660481256975885056, 0.3530559997133364547 ) ) ;
#69545 = ORIENTED_EDGE ( 'NONE', *, *, #46095, .F. ) ;
#69546 = AXIS2_PLACEMENT_3D ( 'NONE', #80844, #82078, #35799 ) ;
#69547 = CARTESIAN_POINT ( 'NONE',  ( -0.5380577427821514602, -0.4281496062992127816, -0.4176697321401328100 ) ) ;
#69548 = CARTESIAN_POINT ( 'NONE',  ( -1.535433070866141225, -0.6692913385826771977, 8.415575281601705876E-17 ) ) ;
#69549 = CARTESIAN_POINT ( 'NONE',  ( 0.8136482939632553313, 0.2306618581243848609, 0.2411417322834645549 ) ) ;
#69550 = CARTESIAN_POINT ( 'NONE',  ( 0.1837270341207357105, -0.6046776061558809534, -0.2411417322834644161 ) ) ;
#69551 = CARTESIAN_POINT ( 'NONE',  ( -0.3917322834645671215, 0.1049643490035301469, -1.219816272965879023 ) ) ;
#69552 = CARTESIAN_POINT ( 'NONE',  ( -0.6036745406824141069, 0.2306618581243848609, 0.2411417322834645549 ) ) ;
#69553 = CARTESIAN_POINT ( 'NONE',  ( 0.1771653543307093182, -0.5400638737290845981, -0.3530559997133363437 ) ) ;
#69554 = CARTESIAN_POINT ( 'NONE',  ( -0.6364829396325453192, -0.05778040916215560624, -0.4822834645669293319 ) ) ;
#69555 = CARTESIAN_POINT ( 'NONE',  ( 0.5052493438320218022, -0.5511811023622048555, -0.09757992244046775898 ) ) ;
#69556 = CARTESIAN_POINT ( 'NONE',  ( -0.2843957880255121307, -0.07959014333740668801, 5.860354325783371010 ) ) ;
#69557 = CARTESIAN_POINT ( 'NONE',  ( 0.02624671916010564918, 0.2306618581243848609, 0.2411417322834645549 ) ) ;
#69558 = CARTESIAN_POINT ( 'NONE',  ( 0.4724409448818898127, -0.1265901696524988629, -0.9757217847769029673 ) ) ;
#69559 = CARTESIAN_POINT ( 'NONE',  ( 1.587926509186352142, 0.05413385826771666132, 0.4176697321401328100 ) ) ;
#69560 = CARTESIAN_POINT ( 'NONE',  ( 0.2867679344610365999, -0.2867679344610365444, -2.610236220472441193 ) ) ;
#69561 = ORIENTED_EDGE ( 'NONE', *, *, #1707, .T. ) ;
#69562 = EDGE_LOOP ( 'NONE', ( #36952, #49558, #59895, #47289 ) ) ;
#69563 = CARTESIAN_POINT ( 'NONE',  ( 0.6036745406824154392, 0.2306618581243847221, -0.2411417322834647770 ) ) ;
#69564 = CARTESIAN_POINT ( 'NONE',  ( -0.03937007874015669567, -0.5511811023622047445, 6.969142054262312111E-17 ) ) ;
#69566 = CARTESIAN_POINT ( 'NONE',  ( 0.2362204724409451007, -0.4091458600556402980, -0.4068241469816273326 ) ) ;
#69565 = CARTESIAN_POINT ( 'NONE',  ( 1.345144356955381593, -0.08942795157527998196, 0.3641732283464567121 ) ) ;
#69567 = CARTESIAN_POINT ( 'NONE',  ( 0.1958661417322836440, -0.3392501089628017219, -1.121391076115485719 ) ) ;
#69568 = CARTESIAN_POINT ( 'NONE',  ( 0.4724409448818898682, 2.892866454678787531E-17, 0.1200787401574803098 ) ) ;
#69569 = DIRECTION ( 'NONE',  ( 0.000000000000000000, -1.000000000000000000, -0.000000000000000000 ) ) ;
#69570 = CARTESIAN_POINT ( 'NONE',  ( -0.1070741851644056997, 0.3996062992125984925, -2.760498687664041384 ) ) ;
#69571 = CARTESIAN_POINT ( 'NONE',  ( 0.3280839895013130669, 0.05413385826771666132, 0.4176697321401328100 ) ) ;
#69572 = CARTESIAN_POINT ( 'NONE',  ( -1.364829396325458521, -0.6046776061558807314, 0.2411417322834647770 ) ) ;
#69573 = CARTESIAN_POINT ( 'NONE',  ( -1.299212598425196097, -0.6692913385826771977, 8.415575281601705876E-17 ) ) ;
#69574 = CARTESIAN_POINT ( 'NONE',  ( 0.4658792650918640033, -0.3162353388693405765, 0.4822834645669290543 ) ) ;
#69575 = CARTESIAN_POINT ( 'NONE',  ( 1.003937007874016185, 0.1660481256975883668, -0.3530559997133364547 ) ) ;
#69576 = CARTESIAN_POINT ( 'NONE',  ( 1.377952755905512472, 0.1771653543307087630, 0.000000000000000000 ) ) ;
#69577 = CONTEXT_DEPENDENT_SHAPE_REPRESENTATION ( #11088, #19737 ) ;
#69578 = CARTESIAN_POINT ( 'NONE',  ( 1.148293963254593875, -0.5511811023622046335, 0.09757992244046803654 ) ) ;
#69579 = CARTESIAN_POINT ( 'NONE',  ( -0.9842519685039360366, 0.2952755905511811885, 0.000000000000000000 ) ) ;
#69580 = CARTESIAN_POINT ( 'NONE',  ( 0.1070741851644054776, -0.3996062992125984925, -0.3195538057742782212 ) ) ;
#69581 = CARTESIAN_POINT ( 'NONE',  ( 1.509186351706037543, 0.05413385826771666132, 0.4176697321401328100 ) ) ;
#69582 = CARTESIAN_POINT ( 'NONE',  ( -0.3917322834645670104, -7.196005306013484475E-17, -0.03149606299212594218 ) ) ;
#69583 = CARTESIAN_POINT ( 'NONE',  ( -0.2559055118110227234, -0.5400638737290844871, 0.3530559997133364547 ) ) ;
#69585 = CARTESIAN_POINT ( 'NONE',  ( -1.614173228346457378, 1.267785121476993293, 0.1372047244094476981 ) ) ;
#69584 = CARTESIAN_POINT ( 'NONE',  ( 0.9448818897637802916, -0.1870078740157480879, -0.4822834645669291653 ) ) ;
#69586 = CARTESIAN_POINT ( 'NONE',  ( -1.541994750656167090, 0.1771653543307087630, 0.09757992244046791164 ) ) ;
#69587 = CARTESIAN_POINT ( 'NONE',  ( 0.1181102362204730916, 0.2952755905511811885, 0.000000000000000000 ) ) ;
#69588 = CARTESIAN_POINT ( 'NONE',  ( 0.6758530183727039509, 0.1771653543307087075, -0.09757992244046823083 ) ) ;
#69589 = CARTESIAN_POINT ( 'NONE',  ( -1.496062992125983815, -0.1870078740157480601, -0.3641732283464567677 ) ) ;
#69590 = CARTESIAN_POINT ( 'NONE',  ( 1.043307086614173818, 0.1660481256975885056, 0.3530559997133364547 ) ) ;
#69591 = DIRECTION ( 'NONE',  ( 0.000000000000000000, 0.000000000000000000, 1.000000000000000000 ) ) ;
#69592 = CARTESIAN_POINT ( 'NONE',  ( -0.3937007874015740483, -0.1870078740157480601, -0.3641732283464567677 ) ) ;
#69593 = CARTESIAN_POINT ( 'NONE',  ( -0.7283464566929126471, 0.1660481256975883668, -0.3530559997133364547 ) ) ;
#69594 = CARTESIAN_POINT ( 'NONE',  ( 1.430446194225722500, -0.4281496062992127816, -0.4176697321401328100 ) ) ;
#69595 = CARTESIAN_POINT ( 'NONE',  ( -0.9580052493438311334, -0.4281496062992124485, 0.4176697321401328655 ) ) ;
#69596 = CARTESIAN_POINT ( 'NONE',  ( 1.391076115485564868, 0.2306618581243847221, -0.2411417322834647770 ) ) ;
#69597 = CARTESIAN_POINT ( 'NONE',  ( 4.797336870675656522E-17, -0.3917322834645670659, -1.020360523130920738 ) ) ;
#69598 = CARTESIAN_POINT ( 'NONE',  ( -1.181102362204723644, -0.1870078740157479769, 0.3641732283464567677 ) ) ;
#69599 = CARTESIAN_POINT ( 'NONE',  ( 1.053828262837742225, 1.260305573253202915, 0.3853833445747810726 ) ) ;
#69600 = CARTESIAN_POINT ( 'NONE',  ( 1.233595800524935227, -0.6046776061558807314, 0.2411417322834647770 ) ) ;
#69601 = VECTOR ( 'NONE', #67865, 39.37007874015748143 ) ;
#69602 = CARTESIAN_POINT ( 'NONE',  ( -0.2362204724409451284, 0.4091458600556402425, -2.294619422572178102 ) ) ;
#69603 = CARTESIAN_POINT ( 'NONE',  ( -1.450131233595799651, -0.6692913385826771977, 0.1292274648535927661 ) ) ;
#69604 = CARTESIAN_POINT ( 'NONE',  ( -1.371391076115484609, -0.5511811023622046335, 0.09757992244046803654 ) ) ;
#69605 = CARTESIAN_POINT ( 'NONE',  ( -1.062992125984250968, 0.1771653543307087630, 0.000000000000000000 ) ) ;
#69606 = DIRECTION ( 'NONE',  ( 0.000000000000000000, 0.000000000000000000, 1.000000000000000000 ) ) ;
#69607 = CARTESIAN_POINT ( 'NONE',  ( -0.4855643044619415427, 0.05413385826771626580, -0.4176697321401330321 ) ) ;
#69608 = CARTESIAN_POINT ( 'NONE',  ( -0.09842519685039295696, -0.4536011799217367080, 0.2665933059059888421 ) ) ;
#69609 = CARTESIAN_POINT ( 'NONE',  ( -1.384514435695537005, 0.1771653543307087630, 0.09757992244046791164 ) ) ;
#69610 = CARTESIAN_POINT ( 'NONE',  ( 1.279527559055118724, 0.07958543189024085140, 0.2665933059059887866 ) ) ;
#69611 = CARTESIAN_POINT ( 'NONE',  ( 1.043307086614173818, 0.1660481256975885056, 0.3530559997133364547 ) ) ;
#69612 = CARTESIAN_POINT ( 'NONE',  ( 1.496062992125984703, -0.1870078740157480879, -0.4822834645669291653 ) ) ;
#69613 = CARTESIAN_POINT ( 'NONE',  ( 0.2362204724409456558, -0.1870078740157479769, 0.3641732283464567677 ) ) ;
#69614 = CARTESIAN_POINT ( 'NONE',  ( 0.3280839895013130669, -0.4281496062992127816, -0.4176697321401328100 ) ) ;
#69615 = EDGE_CURVE ( 'NONE', #21108, #43005, #76666, .T. ) ;
#69616 = CARTESIAN_POINT ( 'NONE',  ( 1.181102362204724976, -0.1870078740157480601, -0.3641732283464567677 ) ) ;
#69617 = ORIENTED_EDGE ( 'NONE', *, *, #35805, .F. ) ;
#69618 = CARTESIAN_POINT ( 'NONE',  ( 1.463254593175853824, 0.2952755905511810774, -0.1292274648535930714 ) ) ;
#69619 = EDGE_CURVE ( 'NONE', #22657, #11962, #39805, .T. ) ;
#69620 = CARTESIAN_POINT ( 'NONE',  ( -1.489501312335957062, -0.05778040916215522460, 0.4822834645669289988 ) ) ;
#69621 = CARTESIAN_POINT ( 'NONE',  ( -0.2821522309711278487, 0.2952755905511811885, 0.1292274648535926551 ) ) ;
#69622 = CARTESIAN_POINT ( 'NONE',  ( 0.1998031496062992740, 0.3460692066303959757, -0.1443569553805774397 ) ) ;
#69623 = CARTESIAN_POINT ( 'NONE',  ( -0.1070741851644056997, 0.3996062992125984925, -2.760498687664041384 ) ) ;
#69624 = CARTESIAN_POINT ( 'NONE',  ( 0.4133858267716541968, -0.5400638737290845981, -0.3530559997133363437 ) ) ;
#69625 = CARTESIAN_POINT ( 'NONE',  ( 1.115485564304462551, -0.004921259842519576551, 0.3153832671262227771 ) ) ;
#69626 = CARTESIAN_POINT ( 'NONE',  ( -0.1771653543307080136, 0.1660481256975883668, -0.3530559997133364547 ) ) ;
#69627 = CARTESIAN_POINT ( 'NONE',  ( 0.4527559055118117182, -0.5400638737290844871, 0.3530559997133364547 ) ) ;
#69628 = CARTESIAN_POINT ( 'NONE',  ( 0.1998031496062994405, -0.3460692066303958092, -2.296587926509186417 ) ) ;
#69629 = CARTESIAN_POINT ( 'NONE',  ( 0.1974969037888704704, 0.3420746716998660508, -1.404199475065616820 ) ) ;
#69630 = CARTESIAN_POINT ( 'NONE',  ( -0.2894808532238192234, 1.161235014983161173, 1.084132210936307628 ) ) ;
#69631 = CARTESIAN_POINT ( 'NONE',  ( -0.1265901696524993347, 0.4724409448818896462, -2.526246719160104792 ) ) ;
#69632 = CARTESIAN_POINT ( 'NONE',  ( 0.2867679344610366554, -0.2867679344610365444, -0.7204724409448818312 ) ) ;
#69633 = CARTESIAN_POINT ( 'NONE',  ( -0.3543307086614165824, -0.5511811023622047445, 6.969142054262312111E-17 ) ) ;
#69634 = CARTESIAN_POINT ( 'NONE',  ( -0.9317585301837263412, 0.05413385826771666132, 0.4176697321401328100 ) ) ;
#69635 = CARTESIAN_POINT ( 'NONE',  ( -0.1058382717557503072, 0.3949938075777408852, -2.445538057742782101 ) ) ;
#69636 = CARTESIAN_POINT ( 'NONE',  ( 0.9711286089238851948, -0.6046776061558809534, -0.2411417322834644161 ) ) ;
#69637 = EDGE_CURVE ( 'NONE', #80330, #11040, #51862, .T. ) ;
#69638 = CARTESIAN_POINT ( 'NONE',  ( -1.515748031496062076, -0.5400638737290844871, 0.3530559997133364547 ) ) ;
#69639 = CARTESIAN_POINT ( 'NONE',  ( 0.7874015748031503170, -0.1870078740157479769, 0.4822834645669291653 ) ) ;
#69640 = CARTESIAN_POINT ( 'NONE',  ( 0.4091458600556404646, -0.2362204724409448231, -2.939632545931758489 ) ) ;
#69641 = CARTESIAN_POINT ( 'NONE',  ( 0.1998031496062992740, 0.3460692066303959757, -2.349081364829396446 ) ) ;
#69642 = CYLINDRICAL_SURFACE ( 'NONE', #39931, 0.4724409448818898682 ) ;
#69643 = EDGE_CURVE ( 'NONE', #66355, #46160, #38263, .T. ) ;
#69644 = CARTESIAN_POINT ( 'NONE',  ( 1.089238845144357537, -0.4281496062992124485, 0.4176697321401328655 ) ) ;
#69645 = CARTESIAN_POINT ( 'NONE',  ( 0.3805774278215230400, 0.05413385826771626580, -0.4176697321401330321 ) ) ;
#69646 = CARTESIAN_POINT ( 'NONE',  ( 1.377952755905512472, -0.5511811023622047445, 6.969142054262312111E-17 ) ) ;
#69647 = CARTESIAN_POINT ( 'NONE',  ( 1.266404199475066328, -0.3162353388693409650, -0.4822834645669289433 ) ) ;
#69648 = CARTESIAN_POINT ( 'NONE',  ( -0.1958661417322834220, -0.3392501089628018884, -0.3077427821522311091 ) ) ;
#69649 = CARTESIAN_POINT ( 'NONE',  ( -1.604771003085130321, 1.278209470906376932, 0.1466069496707743947 ) ) ;
#69650 = CARTESIAN_POINT ( 'NONE',  ( 0.8661417322834653598, -0.1870078740157479769, 0.4822834645669291653 ) ) ;
#69651 = CARTESIAN_POINT ( 'NONE',  ( 1.581364829396326277, -0.2845877964562161244, -0.3641732283464567121 ) ) ;
#69652 = CARTESIAN_POINT ( 'NONE',  ( -0.4921259842519677963, -0.5400638737290844871, 0.3530559997133364547 ) ) ;
#69653 = CARTESIAN_POINT ( 'NONE',  ( -1.154855643044618851, -0.6046776061558809534, -0.2411417322834644161 ) ) ;
#69654 = CARTESIAN_POINT ( 'NONE',  ( 1.194225721784777594, -0.4281496062992127816, -0.4176697321401328100 ) ) ;
#69655 = CARTESIAN_POINT ( 'NONE',  ( 0.2867679344610365999, -0.2867679344610365444, -0.4980314960629922405 ) ) ;
#69656 = CARTESIAN_POINT ( 'NONE',  ( 0.1958661417322836440, -0.3392501089628017219, -1.501312335958005173 ) ) ;
#69657 = CARTESIAN_POINT ( 'NONE',  ( 0.2867679344610365999, -0.2867679344610365444, -2.767716535433069946 ) ) ;
#69658 = CARTESIAN_POINT ( 'NONE',  ( 1.430446194225722500, -0.4281496062992127816, -0.4176697321401328100 ) ) ;
#69659 = ORIENTED_EDGE ( 'NONE', *, *, #32546, .T. ) ;
#69660 = CARTESIAN_POINT ( 'NONE',  ( 0.1058382717557499880, 0.3949938075777411073, -2.670603674540682260 ) ) ;
#69661 = ORIENTED_EDGE ( 'NONE', *, *, #27842, .T. ) ;
#69662 = CARTESIAN_POINT ( 'NONE',  ( -0.02624671916010427875, 0.1539470093639521697, -0.1968503937007875793 ) ) ;
#69663 = VECTOR ( 'NONE', #43707, 39.37007874015748143 ) ;
#69664 = CARTESIAN_POINT ( 'NONE',  ( 1.397637795275591177, -0.4536011799217367080, 0.2665933059059888421 ) ) ;
#69665 = CARTESIAN_POINT ( 'NONE',  ( 0.1070741851644054915, -0.3996062992125986035, -1.502624671916010346 ) ) ;
#69666 = CARTESIAN_POINT ( 'NONE',  ( 1.423884514435696413, -0.2845877964562161244, -0.3641732283464567121 ) ) ;
#69667 = CARTESIAN_POINT ( 'NONE',  ( -1.646051170424378096, 0.4405861044731112508, -0.5309055118110234117 ) ) ;
#69668 = DIRECTION ( 'NONE',  ( 0.000000000000000000, 0.000000000000000000, -1.000000000000000000 ) ) ;
#69669 = CARTESIAN_POINT ( 'NONE',  ( -0.03146197511274030634, 1.953969648464710884, 0.3118041613806297740 ) ) ;
#69670 = CARTESIAN_POINT ( 'NONE',  ( -0.3392501089628017219, -0.1958661417322836718, -0.4520997375328084655 ) ) ;
#69671 = CARTESIAN_POINT ( 'NONE',  ( -0.6430446194225712953, -0.004921259842519870586, -0.3153832671262229437 ) ) ;
#69672 = CARTESIAN_POINT ( 'NONE',  ( -1.305774278215222184, -0.5511811023622048555, -0.09757992244046775898 ) ) ;
#69673 = CARTESIAN_POINT ( 'NONE',  ( -1.161417322834644716, 0.1660481256975885056, 0.3530559997133364547 ) ) ;
#69674 = CARTESIAN_POINT ( 'NONE',  ( 0.1968503937007881344, 0.2952755905511811885, 0.000000000000000000 ) ) ;
#69675 = CARTESIAN_POINT ( 'NONE',  ( -1.633858267716534529, 0.1660481256975885056, 0.3530559997133364547 ) ) ;
#69676 = ORIENTED_EDGE ( 'NONE', *, *, #62649, .F. ) ;
#69677 = CARTESIAN_POINT ( 'NONE',  ( 1.594488188976378673, 0.1660481256975885056, 0.3530559997133364547 ) ) ;
#69678 = FACE_OUTER_BOUND ( 'NONE', #74834, .T. ) ;
#69679 = DIRECTION ( 'NONE',  ( 0.000000000000000000, 0.000000000000000000, 1.000000000000000000 ) ) ;
#69680 = CARTESIAN_POINT ( 'NONE',  ( -1.157146581871515012E-16, 0.4724409448818898682, -2.047244094488188892 ) ) ;
#69681 = DIRECTION ( 'NONE',  ( -3.096699300667737957E-16, 1.000000000000000000, -0.000000000000000000 ) ) ;
#69682 = CARTESIAN_POINT ( 'NONE',  ( -0.4724409448818890911, -0.1870078740157480601, -0.3641732283464567677 ) ) ;
#69683 = CARTESIAN_POINT ( 'NONE',  ( -1.312335958005248715, 0.2306618581243848609, 0.2411417322834645549 ) ) ;
#69684 = CARTESIAN_POINT ( 'NONE',  ( 0.9776902887139113929, -0.6692913385826773087, -0.1292274648535924053 ) ) ;
#69685 = ORIENTED_EDGE ( 'NONE', *, *, #30068, .F. ) ;
#69687 = LINE ( 'NONE', #77240, #49224 ) ;
#69686 = CARTESIAN_POINT ( 'NONE',  ( 0.5314960629921061663, 2.755905511811024056, 1.895394334970797345 ) ) ;
#69688 = CARTESIAN_POINT ( 'NONE',  ( 1.371391076115485941, 0.2952755905511811885, 0.1292274648535926551 ) ) ;
#69689 = CARTESIAN_POINT ( 'NONE',  ( -1.076115485564303809, 0.2306618581243848609, 0.2411417322834645549 ) ) ;
#69690 = CARTESIAN_POINT ( 'NONE',  ( 0.1958661417322836162, -0.3392501089628018329, -0.3293770096774785161 ) ) ;
#69691 = CARTESIAN_POINT ( 'NONE',  ( -0.2099737532808391705, -0.5023911411419708095, -0.1820866141732282451 ) ) ;
#69692 = CARTESIAN_POINT ( 'NONE',  ( 4.797336870675656522E-17, -0.3917322834645670104, -0.9507874015748032370 ) ) ;
#69693 = CARTESIAN_POINT ( 'NONE',  ( -0.5511811023622038563, -0.1870078740157479769, 0.3641732283464567677 ) ) ;
#69694 = CARTESIAN_POINT ( 'NONE',  ( 0.7020997375328090762, -0.08942795157528024563, -0.3641732283464568787 ) ) ;
#69695 = CARTESIAN_POINT ( 'NONE',  ( 0.08530183727034192087, -0.3162353388693409650, -0.4822834645669289433 ) ) ;
#69696 = CARTESIAN_POINT ( 'NONE',  ( -0.6627296587926501115, 0.1771653543307087075, -0.09757992244046823083 ) ) ;
#69697 = CARTESIAN_POINT ( 'NONE',  ( 0.3917322834645670104, 2.398668435337828261E-17, -2.787401574803149096 ) ) ;
#69698 = CARTESIAN_POINT ( 'NONE',  ( 0.9645669291338588858, 0.1660481256975885056, 0.3530559997133364547 ) ) ;
#69699 = ADVANCED_FACE ( 'NONE', ( #39189 ), #60097, .F. ) ;
#69700 = CARTESIAN_POINT ( 'NONE',  ( -1.122047244094487306, 0.1660481256975883668, -0.3530559997133364547 ) ) ;
#69701 = CARTESIAN_POINT ( 'NONE',  ( 0.4724409448818896462, 0.1265901696524990294, -0.6738845144356955252 ) ) ;
#69702 = CARTESIAN_POINT ( 'NONE',  ( -0.1968503937007867743, -0.6692913385826771977, 8.415575281601705876E-17 ) ) ;
#69703 = CARTESIAN_POINT ( 'NONE',  ( -0.8202099737532799750, 0.2952755905511810774, -0.1292274648535930714 ) ) ;
#69704 = CARTESIAN_POINT ( 'NONE',  ( 1.181102362204725198, -0.1870078740157479769, 0.3641732283464567677 ) ) ;
#69705 = CARTESIAN_POINT ( 'NONE',  ( 0.1115485564304467270, -0.5511811023622048555, -0.09757992244046775898 ) ) ;
#69706 = CARTESIAN_POINT ( 'NONE',  ( -0.5577427821522301654, -0.05778040916215560624, -0.4822834645669293319 ) ) ;
#69707 = CARTESIAN_POINT ( 'NONE',  ( -1.148293963254592542, 0.2952755905511811885, 0.1292274648535926551 ) ) ;
#69708 = CARTESIAN_POINT ( 'NONE',  ( 0.3937007874015751585, 1.535433070866141447, 0.000000000000000000 ) ) ;
#69709 = DIRECTION ( 'NONE',  ( 0.000000000000000000, 0.4999999999999998335, -0.8660254037844385966 ) ) ;
#69710 = CARTESIAN_POINT ( 'NONE',  ( -0.3740157480314953431, 0.1660481256975885056, 0.3530559997133364547 ) ) ;
#69711 = CARTESIAN_POINT ( 'NONE',  ( -0.9514435695538050464, -0.3162353388693405765, 0.4822834645669290543 ) ) ;
#69712 = ORIENTED_EDGE ( 'NONE', *, *, #36661, .T. ) ;
#69713 = CARTESIAN_POINT ( 'NONE',  ( -9.787531504996566615E-17, 0.3996062992125985480, -1.809055118110236560 ) ) ;
#69714 = CARTESIAN_POINT ( 'NONE',  ( 1.200787401574803681, -0.5400638737290845981, -0.3530559997133363437 ) ) ;
#69715 = CARTESIAN_POINT ( 'NONE',  ( -0.5118110236220466680, -0.5511811023622047445, 6.969142054262312111E-17 ) ) ;
#69716 = CARTESIAN_POINT ( 'NONE',  ( -0.8202099737532801971, -0.6692913385826771977, 0.1292274648535927661 ) ) ;
#69717 = CARTESIAN_POINT ( 'NONE',  ( 1.489501312335958172, -0.3162353388693405765, 0.4822834645669290543 ) ) ;
#69718 = CARTESIAN_POINT ( 'NONE',  ( 0.9448818897637802916, -0.1870078740157480879, -0.4822834645669291653 ) ) ;
#69719 = CARTESIAN_POINT ( 'NONE',  ( 1.489501312335958172, -0.05778040916215560624, -0.4822834645669293319 ) ) ;
#69720 = CARTESIAN_POINT ( 'NONE',  ( -0.9908136482939626788, -0.5511811023622048555, -0.09757992244046775898 ) ) ;
#69721 = CARTESIAN_POINT ( 'NONE',  ( -0.1070741851644057135, 0.3996062992125984925, -0.8707349081364829102 ) ) ;
#69722 = CARTESIAN_POINT ( 'NONE',  ( 0.3996062992125986590, -0.1070741851644053111, -0.8989501312335956840 ) ) ;
#69723 = CARTESIAN_POINT ( 'NONE',  ( -0.1058382717557497937, -0.3949938075777411628, -0.3871391076115485719 ) ) ;
#69724 = CARTESIAN_POINT ( 'NONE',  ( 0.08477834984147555875, 1.070319560067212850, 2.867229352980811274 ) ) ;
#69725 = CARTESIAN_POINT ( 'NONE',  ( 1.358267716535433323, 0.07958543189024085140, 0.2665933059059887866 ) ) ;
#69726 = CARTESIAN_POINT ( 'NONE',  ( 0.6758530183727039509, 0.1771653543307087075, -0.09757992244046823083 ) ) ;
#69727 = CARTESIAN_POINT ( 'NONE',  ( 0.4790026246719167324, -0.05778040916215522460, 0.4822834645669289988 ) ) ;
#69728 = DIRECTION ( 'NONE',  ( 1.000000000000000000, -0.000000000000000000, -0.000000000000000000 ) ) ;
#69729 = CARTESIAN_POINT ( 'NONE',  ( 0.1974969037888704704, 0.3420746716998660508, -1.166010498687664265 ) ) ;
#69730 = CARTESIAN_POINT ( 'NONE',  ( 0.8989501312335964611, 0.1771653543307087630, 0.09757992244046791164 ) ) ;
#69731 = EDGE_CURVE ( 'NONE', #67621, #57500, #76107, .T. ) ;
#69732 = CARTESIAN_POINT ( 'NONE',  ( -0.4265091863517051496, -0.6692913385826771977, 0.1292274648535927661 ) ) ;
#69733 = CARTESIAN_POINT ( 'NONE',  ( -1.187664041994749731, -0.3162353388693405765, 0.4822834645669290543 ) ) ;
#69734 = CARTESIAN_POINT ( 'NONE',  ( 1.200787401574803681, 0.1660481256975885056, 0.3530559997133364547 ) ) ;
#69735 = CARTESIAN_POINT ( 'NONE',  ( 0.2362204724409451007, -0.4091458600556402980, -1.509186351706036655 ) ) ;
#69736 = CARTESIAN_POINT ( 'NONE',  ( -3.937007874015748143, 2.165354330708661568, 0.6299212598425196763 ) ) ;
#69737 = CARTESIAN_POINT ( 'NONE',  ( -0.1443569553805768291, -0.004921259842519576551, 0.3153832671262227771 ) ) ;
#69738 = VERTEX_POINT ( 'NONE', #28877 ) ;
#69739 = ORIENTED_EDGE ( 'NONE', *, *, #35062, .T. ) ;
#69740 = CARTESIAN_POINT ( 'NONE',  ( -0.8727034120734901146, -0.05778040916215560624, -0.4822834645669293319 ) ) ;
#69741 = CARTESIAN_POINT ( 'NONE',  ( -0.5118110236220466680, 0.2952755905511811885, 0.000000000000000000 ) ) ;
#69742 = CARTESIAN_POINT ( 'NONE',  ( -0.7545931758530176614, -0.6692913385826773087, -0.1292274648535924053 ) ) ;
#69743 = CARTESIAN_POINT ( 'NONE',  ( 0.3674540682414705883, -0.6046776061558807314, 0.2411417322834647770 ) ) ;
#69744 = CARTESIAN_POINT ( 'NONE',  ( -0.4133858267716528645, -0.5400638737290844871, 0.3530559997133364547 ) ) ;
#69745 = CARTESIAN_POINT ( 'NONE',  ( -1.541994750656167090, -0.6692913385826773087, -0.1292274648535924053 ) ) ;
#69746 = CARTESIAN_POINT ( 'NONE',  ( -1.010498687664041384, -0.4281496062992127816, -0.4176697321401328100 ) ) ;
#69747 = CARTESIAN_POINT ( 'NONE',  ( 0.7020997375328090762, -0.05778040916215560624, -0.4822834645669293319 ) ) ;
#69748 = CARTESIAN_POINT ( 'NONE',  ( -9.594673741351313045E-17, 0.3917322834645670104, -1.251968503937008093 ) ) ;
#69749 = CARTESIAN_POINT ( 'NONE',  ( -0.5118110236220466680, 0.1771653543307087630, 0.000000000000000000 ) ) ;
#69750 = EDGE_LOOP ( 'NONE', ( #49250, #47162, #30835, #15299, #44253, #5867, #56963 ) ) ;
#69751 = CARTESIAN_POINT ( 'NONE',  ( 0.2891555358219910499, 0.2891555358219910499, -1.397637795275590733 ) ) ;
#69752 = VERTEX_POINT ( 'NONE', #80255 ) ;
#69753 = CARTESIAN_POINT ( 'NONE',  ( -1.437007874015747477, -0.4536011799217367080, 0.2665933059059888421 ) ) ;
#69754 = CARTESIAN_POINT ( 'NONE',  ( -0.9514435695538050464, -0.05778040916215560624, -0.4822834645669293319 ) ) ;
#69755 = CARTESIAN_POINT ( 'NONE',  ( -1.003937007874014853, 0.1660481256975885056, 0.3530559997133364547 ) ) ;
#69756 = CARTESIAN_POINT ( 'NONE',  ( -9.787531504996567848E-17, 0.3996062992125986035, -0.1574803149606299191 ) ) ;
#69757 = CARTESIAN_POINT ( 'NONE',  ( -1.305774278215222184, -0.6692913385826773087, -0.1292274648535924053 ) ) ;
#69758 = CARTESIAN_POINT ( 'NONE',  ( -0.7808398950131225646, -0.05778040916215522460, 0.4822834645669289988 ) ) ;
#69759 = DIRECTION ( 'NONE',  ( -0.000000000000000000, -1.000000000000000000, -0.000000000000000000 ) ) ;
#69760 = EDGE_CURVE ( 'NONE', #35306, #69836, #57339, .T. ) ;
#69761 = CYLINDRICAL_SURFACE ( 'NONE', #60388, 0.3149606299212597826 ) ;
#69762 = CARTESIAN_POINT ( 'NONE',  ( 0.5249343832021005074, -0.5023911411419708095, 0.1820866141732285504 ) ) ;
#69763 = CARTESIAN_POINT ( 'NONE',  ( -0.4843739873036757571, -1.316179764993976518E-15, -0.3627985898453525149 ) ) ;
#69764 = CARTESIAN_POINT ( 'NONE',  ( -0.3917322834645669549, -0.1049643490035306603, 0.02690288713910752097 ) ) ;
#69765 = CARTESIAN_POINT ( 'NONE',  ( 0.1312335958005255154, -0.5023911411419708095, 0.1820866141732285504 ) ) ;
#69766 = CARTESIAN_POINT ( 'NONE',  ( -0.4986876640419939388, 0.2306618581243847221, -0.2411417322834647770 ) ) ;
#69767 = ADVANCED_FACE ( 'NONE', ( #11187 ), #36434, .T. ) ;
#69768 = CARTESIAN_POINT ( 'NONE',  ( 1.240157480314961314, -0.5400638737290844871, 0.3530559997133364547 ) ) ;
#69769 = CARTESIAN_POINT ( 'NONE',  ( -0.6561679790026240244, 0.2306618581243847221, -0.2411417322834647770 ) ) ;
#69770 = VERTEX_POINT ( 'NONE', #3628 ) ;
#69771 = CARTESIAN_POINT ( 'NONE',  ( -0.1070741851644056997, 0.3996062992125986035, -2.053805774278214979 ) ) ;
#69772 = CARTESIAN_POINT ( 'NONE',  ( 0.2486400153428833526, 3.421639014772782816E-16, 0.3464511005275203726 ) ) ;
#69773 = ORIENTED_EDGE ( 'NONE', *, *, #511, .T. ) ;
#69774 = CARTESIAN_POINT ( 'NONE',  ( 0.1998031496062994128, -0.3460692066303957537, -1.585958005249344049 ) ) ;
#69775 = CARTESIAN_POINT ( 'NONE',  ( -0.4002624671916004129, -0.3162353388693405765, 0.4822834645669290543 ) ) ;
#69776 = CARTESIAN_POINT ( 'NONE',  ( 1.417322834645670104, -0.1870078740157479769, 0.4822834645669291653 ) ) ;
#69777 = CARTESIAN_POINT ( 'NONE',  ( -0.9711286089238838626, -0.5023911411419708095, 0.1820866141732285504 ) ) ;
#69778 = CARTESIAN_POINT ( 'NONE',  ( -1.233595800524933894, 0.2306618581243848609, 0.2411417322834645549 ) ) ;
#69779 = CARTESIAN_POINT ( 'NONE',  ( 0.2362204724409451007, -0.4091458600556402980, -1.036745406824147064 ) ) ;
#69780 = CARTESIAN_POINT ( 'NONE',  ( -0.5314960629921122726, 2.755905511811024056, -3.937007874015763687 ) ) ;
#69781 = CARTESIAN_POINT ( 'NONE',  ( 0.1049643490035304938, -0.3917322834645669549, -2.847112860892388131 ) ) ;
#69782 = CARTESIAN_POINT ( 'NONE',  ( 1.384514435695538559, 0.2952755905511810774, -0.1292274648535930714 ) ) ;
#69783 = CARTESIAN_POINT ( 'NONE',  ( -9.594673741351313045E-17, 0.3917322834645670104, -2.131889763779527769 ) ) ;
#69784 = CARTESIAN_POINT ( 'NONE',  ( 0.09842519685039434474, 0.1660481256975885056, 0.3530559997133364547 ) ) ;
#69785 = CARTESIAN_POINT ( 'NONE',  ( -0.9908136482939626788, 0.1771653543307087630, 0.09757992244046791164 ) ) ;
#69786 = CARTESIAN_POINT ( 'NONE',  ( -0.1706036745406816491, -0.4281496062992124485, 0.4176697321401328655 ) ) ;
#69787 = CARTESIAN_POINT ( 'NONE',  ( -0.3458507752293906723, -0.3458507752293910609, -2.655511811023622215 ) ) ;
#69788 = CARTESIAN_POINT ( 'NONE',  ( -0.8267716535433065062, -0.6692913385826771977, 8.415575281601705876E-17 ) ) ;
#69789 = CARTESIAN_POINT ( 'NONE',  ( -0.1058382717557497660, -0.3949938075777411073, -2.038713910761155379 ) ) ;
#69790 = CARTESIAN_POINT ( 'NONE',  ( 0.7283464566929140904, -0.4536011799217368745, -0.2665933059059886201 ) ) ;
#69791 = CARTESIAN_POINT ( 'NONE',  ( -0.1771653543307080136, -0.4536011799217367080, 0.2665933059059888421 ) ) ;
#69792 = CARTESIAN_POINT ( 'NONE',  ( 0.9448818897637802916, -0.1870078740157480601, -0.3641732283464567677 ) ) ;
#69793 = CARTESIAN_POINT ( 'NONE',  ( -1.364829396325458521, 0.2306618581243847221, -0.2411417322834647770 ) ) ;
#69794 = CARTESIAN_POINT ( 'NONE',  ( 0.2362204724409451007, -0.4091458600556402980, -2.215879265091863726 ) ) ;
#69795 = CARTESIAN_POINT ( 'NONE',  ( 0.7349081364829403995, 0.1283753931104748280, 0.1820866141732283561 ) ) ;
#69796 = CARTESIAN_POINT ( 'NONE',  ( -1.043307086614172041, -0.5400638737290844871, 0.3530559997133364547 ) ) ;
#69797 = CARTESIAN_POINT ( 'NONE',  ( -1.915796337058206955, 1.134406187872333938, 0.2508088161067916766 ) ) ;
#69798 = CARTESIAN_POINT ( 'NONE',  ( -0.03937007874015669567, 0.1771653543307087630, 0.000000000000000000 ) ) ;
#69799 = CARTESIAN_POINT ( 'NONE',  ( -1.541994750656167090, 0.1771653543307087630, 0.09757992244046791164 ) ) ;
#69800 = CARTESIAN_POINT ( 'NONE',  ( 0.5708661417322842269, 0.1660481256975885056, 0.3530559997133364547 ) ) ;
#69801 = CARTESIAN_POINT ( 'NONE',  ( 0.6986524979670498681, 8.471767977567108961E-16, -0.4445507791589058955 ) ) ;
#69802 = CARTESIAN_POINT ( 'NONE',  ( 1.305774278215223960, 0.1771653543307087075, -0.09757992244046823083 ) ) ;
#69803 = CARTESIAN_POINT ( 'NONE',  ( -1.240157480314959759, 0.1660481256975885056, 0.3530559997133364547 ) ) ;
#69804 = CARTESIAN_POINT ( 'NONE',  ( -0.1771653543307080136, 0.07958543189024071263, -0.2665933059059888421 ) ) ;
#69805 = CARTESIAN_POINT ( 'NONE',  ( -0.7137454485294959516, 2.001539355558159983, 0.4917280318828578523 ) ) ;
#69806 = CARTESIAN_POINT ( 'NONE',  ( 0.2362204724409456558, -0.1870078740157480601, -0.3641732283464567677 ) ) ;
#69807 = CARTESIAN_POINT ( 'NONE',  ( -1.279527559055116948, -0.5400638737290844871, 0.3530559997133364547 ) ) ;
#69808 = CARTESIAN_POINT ( 'NONE',  ( -0.5839895013123351797, -0.6692913385826771977, 0.1292274648535927661 ) ) ;
#69809 = CARTESIAN_POINT ( 'NONE',  ( 0.2925321140481932369, 0.2925321140481932369, -0.6870078740157479213 ) ) ;
#69810 = CARTESIAN_POINT ( 'NONE',  ( -0.1049643490035302024, -0.3917322834645671215, -2.046587926509185973 ) ) ;
#69811 = CARTESIAN_POINT ( 'NONE',  ( 0.6692913385826777528, 0.1771653543307087630, 0.000000000000000000 ) ) ;
#69812 = CARTESIAN_POINT ( 'NONE',  ( -0.2296587926509179312, -0.05778040916215522460, 0.4822834645669289988 ) ) ;
#69813 = CARTESIAN_POINT ( 'NONE',  ( -0.6102362204724400829, -0.5400638737290845981, -0.3530559997133363437 ) ) ;
#69814 = CARTESIAN_POINT ( 'NONE',  ( -1.010498687664041384, -0.004921259842519576551, 0.3153832671262227771 ) ) ;
#69815 = CARTESIAN_POINT ( 'NONE',  ( -0.4724409448818898682, -8.678599364036362592E-17, -0.1161417322834645827 ) ) ;
#69816 = CARTESIAN_POINT ( 'NONE',  ( -0.04593175853018302557, 0.2952755905511811885, 0.1292274648535926551 ) ) ;
#69817 = CARTESIAN_POINT ( 'NONE',  ( -1.686351706036744558, 0.1771653543307087075, -0.09757992244046823083 ) ) ;
#69818 = CARTESIAN_POINT ( 'NONE',  ( 1.266404199475066328, -0.05778040916215522460, 0.4822834645669289988 ) ) ;
#69819 = DIRECTION ( 'NONE',  ( -1.000000000000000000, -8.805702923740138355E-17, -0.000000000000000000 ) ) ;
#69820 = CARTESIAN_POINT ( 'NONE',  ( 0.1958661417322836718, -0.3392501089628017219, -1.978365772474752537 ) ) ;
#69821 = ORIENTED_EDGE ( 'NONE', *, *, #7492, .T. ) ;
#69822 = FACE_OUTER_BOUND ( 'NONE', #50363, .T. ) ;
#69823 = CARTESIAN_POINT ( 'NONE',  ( -1.502624671916009680, -0.05778040916215560624, -0.4822834645669293319 ) ) ;
#69824 = CARTESIAN_POINT ( 'NONE',  ( -1.062992125984250968, 0.2952755905511811885, 0.000000000000000000 ) ) ;
#69825 = CARTESIAN_POINT ( 'NONE',  ( 1.489501312335958172, -0.05778040916215560624, -0.4822834645669293319 ) ) ;
#69826 = CARTESIAN_POINT ( 'NONE',  ( -0.2867679344610365999, 0.2867679344610364889, -1.836614173228346747 ) ) ;
#69827 = CARTESIAN_POINT ( 'NONE',  ( -0.5314960629921172686, 2.755905511811024056, -2.503252890251017604 ) ) ;
#69828 = CARTESIAN_POINT ( 'NONE',  ( 0.7414698162729663755, 0.2952755905511811885, 0.1292274648535926551 ) ) ;
#69829 = CARTESIAN_POINT ( 'NONE',  ( 0.03937007874015833325, -0.6692913385826771977, 8.415575281601705876E-17 ) ) ;
#69830 = LINE ( 'NONE', #63515, #52977 ) ;
#69831 = DIRECTION ( 'NONE',  ( -3.114085624724525612E-16, 1.000000000000000000, 5.270319453084425600E-32 ) ) ;
#69832 = CARTESIAN_POINT ( 'NONE',  ( 1.351706036745407458, -0.3690944881889765550, -0.3153832671262227771 ) ) ;
#69833 = CARTESIAN_POINT ( 'NONE',  ( -0.1070741851644051862, -0.3996062992125987146, -0.7020997375328084100 ) ) ;
#69834 = ORIENTED_EDGE ( 'NONE', *, *, #10031, .F. ) ;
#69835 = CARTESIAN_POINT ( 'NONE',  ( 0.1049643490035304938, -0.3917322834645669549, -2.597112860892388131 ) ) ;
#69836 = VERTEX_POINT ( 'NONE', #43144 ) ;
#69837 = CARTESIAN_POINT ( 'NONE',  ( 0.2230971128608929543, 0.05413385826771626580, -0.4176697321401330321 ) ) ;
#69838 = CARTESIAN_POINT ( 'NONE',  ( -0.8595800524934373854, -0.3162353388693409650, -0.4822834645669289433 ) ) ;
#69839 = CARTESIAN_POINT ( 'NONE',  ( -1.417322834645668772, -0.1870078740157480879, -0.4822834645669291653 ) ) ;
#69840 = CARTESIAN_POINT ( 'NONE',  ( 0.5118110236220480003, -0.6692913385826771977, 8.415575281601705876E-17 ) ) ;
#69841 = CARTESIAN_POINT ( 'NONE',  ( 1.456692913385827515, -0.6692913385826771977, 8.415575281601705876E-17 ) ) ;
#69842 = CARTESIAN_POINT ( 'NONE',  ( 1.266404199475066328, -0.05778040916215522460, 0.4822834645669289988 ) ) ;
#69843 = CARTESIAN_POINT ( 'NONE',  ( -0.1377952755905504645, -0.5400638737290845981, -0.3530559997133363437 ) ) ;
#69844 = CARTESIAN_POINT ( 'NONE',  ( -1.325459317585300889, 0.05413385826771666132, 0.4176697321401328100 ) ) ;
#69845 = CYLINDRICAL_SURFACE ( 'NONE', #3076, 0.3937007874015748254 ) ;
#69846 = CARTESIAN_POINT ( 'NONE',  ( 1.528871391076116026, 0.2952755905511811885, 0.1292274648535926551 ) ) ;
#69847 = CARTESIAN_POINT ( 'NONE',  ( -9.594673741351313045E-17, 0.3917322834645670104, 0.007874015748031542791 ) ) ;
#69848 = CARTESIAN_POINT ( 'NONE',  ( 0.8398950131233602345, -0.5023911411419708095, 0.1820866141732285504 ) ) ;
#69849 = ORIENTED_EDGE ( 'NONE', *, *, #23437, .T. ) ;
#69850 = CARTESIAN_POINT ( 'NONE',  ( -0.1974969037888703871, -0.3420746716998661063, -0.2230971128608924547 ) ) ;
#69851 = VERTEX_POINT ( 'NONE', #29296 ) ;
#69852 = CARTESIAN_POINT ( 'NONE',  ( 0.05249343832021075018, 0.1283753931104746893, -0.1820866141732285504 ) ) ;
#69853 = LINE ( 'NONE', #70683, #30037 ) ;
#69854 = CARTESIAN_POINT ( 'NONE',  ( 0.5183727034120741983, 0.2952755905511810774, -0.1292274648535930714 ) ) ;
#69855 = CARTESIAN_POINT ( 'NONE',  ( 0.5708661417322841158, -0.5400638737290845981, -0.3530559997133363437 ) ) ;
#69856 = EDGE_CURVE ( 'NONE', #10035, #61855, #55777, .T. ) ;
#69857 = CARTESIAN_POINT ( 'NONE',  ( -0.4986876640419942164, -0.6046776061558807314, 0.2411417322834647770 ) ) ;
#69858 = CARTESIAN_POINT ( 'NONE',  ( 0.3917322834645670659, 2.398668435337828261E-17, -1.847132176674227688 ) ) ;
#69859 = CARTESIAN_POINT ( 'NONE',  ( -1.200787401574802349, -0.5400638737290844871, 0.3530559997133364547 ) ) ;
#69860 = CARTESIAN_POINT ( 'NONE',  ( -0.3392501089628019995, 0.1958661417322832277, -2.473097112860892288 ) ) ;
#69861 = CARTESIAN_POINT ( 'NONE',  ( 1.279527559055118724, 0.07958543189024085140, 0.2665933059059887866 ) ) ;
#69862 = CARTESIAN_POINT ( 'NONE',  ( -1.574803149606298192, -0.1870078740157480879, -0.4822834645669291653 ) ) ;
#69863 = CARTESIAN_POINT ( 'NONE',  ( 0.8070866141732289112, -0.5400638737290845981, -0.3530559997133363437 ) ) ;
#69864 = CARTESIAN_POINT ( 'NONE',  ( 1.292650918635171564, -0.6692913385826773087, -0.1292274648535924053 ) ) ;
#69865 = CARTESIAN_POINT ( 'NONE',  ( -0.2925321140481932924, 0.2925321140481931814, -0.8070866141732284671 ) ) ;
#69866 = CARTESIAN_POINT ( 'NONE',  ( -1.423884514435694859, -0.3162353388693405765, 0.4822834645669290543 ) ) ;
#69867 = CARTESIAN_POINT ( 'NONE',  ( -0.3996062992125986590, 0.1070741851644051723, -0.4245406824146981672 ) ) ;
#69868 = CARTESIAN_POINT ( 'NONE',  ( -0.1070741851644056997, 0.3996062992125984925, -0.08333333333333337034 ) ) ;
#69869 = CARTESIAN_POINT ( 'NONE',  ( 0.04593175853018440641, 0.2952755905511810774, -0.1292274648535930714 ) ) ;
#69870 = CARTESIAN_POINT ( 'NONE',  ( -0.3996062992125987146, 0.1070741851644051862, -2.867454068241469756 ) ) ;
#69871 = CARTESIAN_POINT ( 'NONE',  ( 0.1958661417322834775, 0.3392501089628018884, -1.646325459317585338 ) ) ;
#69872 = CARTESIAN_POINT ( 'NONE',  ( 1.286089238845145033, -0.6046776061558809534, -0.2411417322834644161 ) ) ;
#69873 = CARTESIAN_POINT ( 'NONE',  ( 0.2165354330708668673, -0.4536011799217367080, 0.2665933059059888421 ) ) ;
#69874 = CARTESIAN_POINT ( 'NONE',  ( 0.7217847769028878924, -0.4281496062992127816, -0.4176697321401328100 ) ) ;
#69875 = CARTESIAN_POINT ( 'NONE',  ( -0.4724409448818898682, -8.678599364036362592E-17, -1.690944881889763884 ) ) ;
#69876 = CARTESIAN_POINT ( 'NONE',  ( 0.4330708661417329575, 0.1771653543307087630, 0.000000000000000000 ) ) ;
#69877 = CARTESIAN_POINT ( 'NONE',  ( 0.4002624671916016896, -0.3162353388693409650, -0.4822834645669289433 ) ) ;
#69878 = CARTESIAN_POINT ( 'NONE',  ( -9.674558042662122972E-17, 0.3949938075777409963, -0.8641732283464566011 ) ) ;
#69879 = CARTESIAN_POINT ( 'NONE',  ( -0.6824146981627291497, -0.6046776061558809534, -0.2411417322834644161 ) ) ;
#69880 = CARTESIAN_POINT ( 'NONE',  ( 0.9580052493438326877, -0.004921259842519576551, 0.3153832671262227771 ) ) ;
#69881 = CARTESIAN_POINT ( 'NONE',  ( -1.128608923884513837, 0.2306618581243847221, -0.2411417322834647770 ) ) ;
#69882 = CARTESIAN_POINT ( 'NONE',  ( -0.1837270341207343505, -0.6046776061558807314, 0.2411417322834647770 ) ) ;
#69883 = CARTESIAN_POINT ( 'NONE',  ( 0.1968503937007881344, -0.5511811023622047445, 6.969142054262312111E-17 ) ) ;
#69884 = CARTESIAN_POINT ( 'NONE',  ( -2.704643427489245244, 1.253539720428387572, -0.3811758253792954521 ) ) ;
#69885 = CARTESIAN_POINT ( 'NONE',  ( -0.2559055118110230564, 0.1660481256975883668, -0.3530559997133364547 ) ) ;
#69886 = CARTESIAN_POINT ( 'NONE',  ( 0.2755905511811031494, -0.5511811023622047445, 6.969142054262312111E-17 ) ) ;
#69887 = CARTESIAN_POINT ( 'NONE',  ( 0.1070741851644054776, -0.3996062992125984925, -1.894356955380577023 ) ) ;
#69888 = CARTESIAN_POINT ( 'NONE',  ( 0.4199475065616805614, 0.2306618581243848609, 0.2411417322834645549 ) ) ;
#69889 = CARTESIAN_POINT ( 'NONE',  ( 1.325459317585302665, -0.3690944881889763329, 0.3153832671262228327 ) ) ;
#69890 = DIRECTION ( 'NONE',  ( 1.000000000000000000, 0.000000000000000000, 0.000000000000000000 ) ) ;
#69891 = CARTESIAN_POINT ( 'NONE',  ( -0.5314960629921254842, -0.4536011799217368745, -0.2665933059059886201 ) ) ;
#69892 = CARTESIAN_POINT ( 'NONE',  ( -0.5643044619422565855, -0.004921259842519870586, -0.3153832671262229437 ) ) ;
#69893 = CARTESIAN_POINT ( 'NONE',  ( -0.1837270341207340729, 0.2306618581243847221, -0.2411417322834647770 ) ) ;
#69894 = CARTESIAN_POINT ( 'NONE',  ( 0.3346456692913390985, 0.1660481256975885056, 0.3530559997133364547 ) ) ;
#69895 = CARTESIAN_POINT ( 'NONE',  ( 0.8727034120734913358, -0.08942795157527998196, 0.3641732283464567121 ) ) ;
#69896 = CARTESIAN_POINT ( 'NONE',  ( -1.620734908136482577, -0.5511811023622048555, -0.09757992244046775898 ) ) ;
#69897 = CARTESIAN_POINT ( 'NONE',  ( -1.692913385826770645, 0.2952755905511811885, 0.000000000000000000 ) ) ;
#69898 = CARTESIAN_POINT ( 'NONE',  ( 0.5774278215223104249, 0.2306618581243848609, 0.2411417322834645549 ) ) ;
#69899 = CARTESIAN_POINT ( 'NONE',  ( 0.2248261898302408024, 1.118407866122129724, -1.901322016725929931 ) ) ;
#69900 = CARTESIAN_POINT ( 'NONE',  ( -0.08530183727034056085, -0.05778040916215560624, -0.4822834645669293319 ) ) ;
#69901 = CARTESIAN_POINT ( 'NONE',  ( 0.3392501089628018329, 0.1958661417322835607, -1.003280839895013266 ) ) ;
#69902 = CARTESIAN_POINT ( 'NONE',  ( 1.095800524934383846, -0.05778040916215560624, -0.4822834645669293319 ) ) ;
#69903 = CARTESIAN_POINT ( 'NONE',  ( 0.6430446194225729606, -0.4281496062992127816, -0.4176697321401328100 ) ) ;
#69904 = CARTESIAN_POINT ( 'NONE',  ( -0.2375791879843439092, 1.126472371288131047, -3.929857012155298257 ) ) ;
#69905 = CARTESIAN_POINT ( 'NONE',  ( 0.3083989501312343062, -0.08942795157528024563, -0.3641732283464568787 ) ) ;
#69906 = CARTESIAN_POINT ( 'NONE',  ( 1.213910761154856299, 0.2952755905511811885, 0.1292274648535926551 ) ) ;
#69907 = CARTESIAN_POINT ( 'NONE',  ( -0.3346456692913377662, -0.4536011799217367080, 0.2665933059059888421 ) ) ;
#69908 = CARTESIAN_POINT ( 'NONE',  ( -0.2099737532808391705, 0.2306618581243848609, 0.2411417322834645549 ) ) ;
#69909 = FACE_OUTER_BOUND ( 'NONE', #46929, .T. ) ;
#69910 = CARTESIAN_POINT ( 'NONE',  ( 0.2034120734908142214, 0.2952755905511810774, -0.1292274648535930714 ) ) ;
#69911 = CARTESIAN_POINT ( 'NONE',  ( -0.8923884514435688198, -0.6046776061558807314, 0.2411417322834647770 ) ) ;
#69912 = CARTESIAN_POINT ( 'NONE',  ( -0.5643044619422565855, -0.004921259842519870586, -0.3153832671262229437 ) ) ;
#69913 = CARTESIAN_POINT ( 'NONE',  ( 0.3608923884514443348, 0.2952755905511810774, -0.1292274648535930714 ) ) ;
#69914 = CARTESIAN_POINT ( 'NONE',  ( -1.305774278215222184, -0.6692913385826773087, -0.1292274648535924053 ) ) ;
#69915 = CARTESIAN_POINT ( 'NONE',  ( -0.3608923884514428360, 0.2952755905511811885, 0.1292274648535926551 ) ) ;
#69916 = CARTESIAN_POINT ( 'NONE',  ( 1.854472803289052507, 2.716535433070866645, -0.5314960629921260393 ) ) ;
#69918 = CARTESIAN_POINT ( 'NONE',  ( 1.325459317585302665, 0.05413385826771626580, -0.4176697321401330321 ) ) ;
#69917 = CARTESIAN_POINT ( 'NONE',  ( 1.348312163386739204, 1.122131950691689140, 0.7386866130305692613 ) ) ;
#69919 = CARTESIAN_POINT ( 'NONE',  ( 1.102362204724410155, -0.1870078740157480879, -0.4822834645669291653 ) ) ;
#69920 = CARTESIAN_POINT ( 'NONE',  ( -0.1049643490035307020, 0.3917322834645669549, -2.203412073490813583 ) ) ;
#69921 = CARTESIAN_POINT ( 'NONE',  ( -1.620734908136482577, 0.2952755905511811885, 0.1292274648535926551 ) ) ;
#69922 = CARTESIAN_POINT ( 'NONE',  ( -1.049868766404198794, 0.2306618581243847221, -0.2411417322834647770 ) ) ;
#69923 = CARTESIAN_POINT ( 'NONE',  ( 0.3458507752293908943, 0.3458507752293908943, -0.4527559055118109965 ) ) ;
#69924 = CARTESIAN_POINT ( 'NONE',  ( 0.2891555358219910499, -0.2891555358219909944, -2.618110236220472675 ) ) ;
#69925 = VERTEX_POINT ( 'NONE', #24209 ) ;
#69926 = CARTESIAN_POINT ( 'NONE',  ( -0.03937007874015669567, 0.1771653543307087630, 0.000000000000000000 ) ) ;
#69927 = CARTESIAN_POINT ( 'NONE',  ( 4.797336870675656522E-17, -0.3917322834645670104, -1.488188976377952777 ) ) ;
#69928 = CARTESIAN_POINT ( 'NONE',  ( 0.7545931758530188826, -0.6692913385826771977, 0.1292274648535927661 ) ) ;
#69929 = CARTESIAN_POINT ( 'NONE',  ( -0.4091458600556402980, -0.2362204724409451284, -2.887139107611548461 ) ) ;
#69930 = DIRECTION ( 'NONE',  ( -0.000000000000000000, -1.000000000000000000, -0.000000000000000000 ) ) ;
#69931 = CARTESIAN_POINT ( 'NONE',  ( -0.5774278215223089816, -0.5023911411419708095, 0.1820866141732285504 ) ) ;
#69932 = CARTESIAN_POINT ( 'NONE',  ( 0.5314960629921372526, 2.716535433070866645, -3.224202737261813834 ) ) ;
#69933 = CARTESIAN_POINT ( 'NONE',  ( 1.062992125984252745, 0.2952755905511811885, 0.000000000000000000 ) ) ;
#69934 = CARTESIAN_POINT ( 'NONE',  ( 1.062992125984252745, -0.5511811023622047445, 6.969142054262312111E-17 ) ) ;
#69935 = CARTESIAN_POINT ( 'NONE',  ( -0.1902887139107604098, 0.2952755905511810774, -0.1292274648535930714 ) ) ;
#69936 = CARTESIAN_POINT ( 'NONE',  ( -0.3917322834645669549, -7.196005306013483243E-17, -0.9068048311997882749 ) ) ;
#69937 = CARTESIAN_POINT ( 'NONE',  ( -0.2427821522309703550, -0.3162353388693405765, 0.4822834645669290543 ) ) ;
#69938 = CARTESIAN_POINT ( 'NONE',  ( -1.371391076115484831, 0.1771653543307087075, -0.09757992244046823083 ) ) ;
#69939 = EDGE_CURVE ( 'NONE', #79831, #46664, #55367, .T. ) ;
#69940 = CARTESIAN_POINT ( 'NONE',  ( -0.3346456692913377662, -0.5400638737290844871, 0.3530559997133364547 ) ) ;
#69941 = DIRECTION ( 'NONE',  ( -3.096699300667737957E-16, 1.000000000000000000, -0.000000000000000000 ) ) ;
#69942 = FACE_OUTER_BOUND ( 'NONE', #72041, .T. ) ;
#69943 = EDGE_LOOP ( 'NONE', ( #54533, #38166, #68503 ) ) ;
#69944 = CARTESIAN_POINT ( 'NONE',  ( 0.1049643490035303967, 0.3917322834645670659, -1.879940575624358789 ) ) ;
#69945 = CARTESIAN_POINT ( 'NONE',  ( 0.2887139107611556010, 0.2306618581243847221, -0.2411417322834647770 ) ) ;
#69946 = VERTEX_POINT ( 'NONE', #80665 ) ;
#69947 = CARTESIAN_POINT ( 'NONE',  ( -0.9120734908136475250, 0.2952755905511811885, 0.1292274648535926551 ) ) ;
#69948 = CARTESIAN_POINT ( 'NONE',  ( -1.364829396325458521, -0.6046776061558807314, 0.2411417322834647770 ) ) ;
#69949 = CARTESIAN_POINT ( 'NONE',  ( 0.8267716535433077274, 0.2952755905511811885, 0.000000000000000000 ) ) ;
#69950 = EDGE_CURVE ( 'NONE', #10845, #4446, #49880, .T. ) ;
#69951 = CARTESIAN_POINT ( 'NONE',  ( -0.1246719160104980823, -0.6692913385826773087, -0.1292274648535924053 ) ) ;
#69952 = CARTESIAN_POINT ( 'NONE',  ( -0.2867679344610365999, 0.2867679344610364889, -1.521653543307086354 ) ) ;
#69953 = CARTESIAN_POINT ( 'NONE',  ( -0.5839895013123351797, 0.2952755905511810774, -0.1292274648535930714 ) ) ;
#69954 = CARTESIAN_POINT ( 'NONE',  ( -0.2887139107611542133, -0.6046776061558809534, -0.2411417322834644161 ) ) ;
#69955 = CARTESIAN_POINT ( 'NONE',  ( -0.8989501312335946848, -0.6692913385826771977, 0.1292274648535927661 ) ) ;
#69956 = CARTESIAN_POINT ( 'NONE',  ( 0.4265091863517067594, 0.1771653543307087630, 0.09757992244046791164 ) ) ;
#69957 = CARTESIAN_POINT ( 'NONE',  ( -0.2747288752779720178, -0.1086799599621181001, 5.842342907282080944 ) ) ;
#69958 = CARTESIAN_POINT ( 'NONE',  ( -0.01968503937007793844, -0.5400638737290844871, 0.3530559997133364547 ) ) ;
#69959 = DIRECTION ( 'NONE',  ( -0.000000000000000000, 1.000000000000000000, -0.000000000000000000 ) ) ;
#69960 = CARTESIAN_POINT ( 'NONE',  ( 1.089238845144357537, -0.4281496062992124485, 0.4176697321401328655 ) ) ;
#69961 = CARTESIAN_POINT ( 'NONE',  ( -0.3392501089628019995, 0.1958661417322832277, -2.695538057742782101 ) ) ;
#69962 = ORIENTED_EDGE ( 'NONE', *, *, #82449, .F. ) ;
#69963 = ORIENTED_EDGE ( 'NONE', *, *, #15090, .F. ) ;
#69964 = CARTESIAN_POINT ( 'NONE',  ( 0.1837270341207357105, -0.6046776061558809534, -0.2411417322834644161 ) ) ;
#69965 = CARTESIAN_POINT ( 'NONE',  ( -0.04593175853018302557, -0.5511811023622048555, -0.09757992244046775898 ) ) ;
#69967 = CARTESIAN_POINT ( 'NONE',  ( 0.4724409448818898682, 2.892866454678787531E-17, -0.4330708661417322913 ) ) ;
#69966 = CARTESIAN_POINT ( 'NONE',  ( 1.437007874015748810, -0.4536011799217368745, -0.2665933059059886201 ) ) ;
#69968 = CARTESIAN_POINT ( 'NONE',  ( 0.3392501089628018329, 0.1958661417322835607, -1.003280839895013266 ) ) ;
#69969 = CARTESIAN_POINT ( 'NONE',  ( -0.1265901696524986964, -0.4724409448818899238, 0.008530183727034111943 ) ) ;
#69970 = CARTESIAN_POINT ( 'NONE',  ( 0.3503937007874015630, -0.5120078740157480990, -0.4921259842519685179 ) ) ;
#69971 = CARTESIAN_POINT ( 'NONE',  ( -1.456692913385826182, 0.2952755905511811885, 0.000000000000000000 ) ) ;
#69972 = CARTESIAN_POINT ( 'NONE',  ( 0.1974969037888706092, -0.3420746716998660508, 0.1463254593175853102 ) ) ;
#69973 = CARTESIAN_POINT ( 'NONE',  ( 0.3805774278215230400, 0.05413385826771626580, -0.4176697321401330321 ) ) ;
#69974 = CARTESIAN_POINT ( 'NONE',  ( -1.108923884514435132, -0.05778040916215560624, -0.4822834645669293319 ) ) ;
#69975 = CARTESIAN_POINT ( 'NONE',  ( -1.148293963254592542, -0.6692913385826773087, -0.1292274648535924053 ) ) ;
#69976 = CARTESIAN_POINT ( 'NONE',  ( 0.1771653543307093182, 0.1660481256975885056, 0.3530559997133364547 ) ) ;
#69977 = CARTESIAN_POINT ( 'NONE',  ( 0.9776902887139113929, 0.2952755905511811885, 0.1292274648535926551 ) ) ;
#69978 = CARTESIAN_POINT ( 'NONE',  ( 1.548556430446194954, 0.1283753931104746893, -0.1820866141732285504 ) ) ;
#69979 = ITEM_DEFINED_TRANSFORMATION ( 'NONE', 'NONE', #82658,  #22098 ) ;
#69980 = CARTESIAN_POINT ( 'NONE',  ( 0.6955380577427828781, -0.3690944881889763329, 0.3153832671262228327 ) ) ;
#69981 = CARTESIAN_POINT ( 'NONE',  ( -0.8202099737532799750, 0.2952755905511810774, -0.1292274648535930714 ) ) ;
#69982 = CARTESIAN_POINT ( 'NONE',  ( 0.3996062992125984925, 0.1070741851644054637, -0.5164041994750655507 ) ) ;
#69983 = CARTESIAN_POINT ( 'NONE',  ( 1.450131233595801428, -0.6692913385826773087, -0.1292274648535924053 ) ) ;
#69984 = CARTESIAN_POINT ( 'NONE',  ( 0.3917322834645669549, 0.1049643490035304660, -0.4317585301837270628 ) ) ;
#69986 = DIRECTION ( 'NONE',  ( 1.000000000000000000, 0.000000000000000000, 0.000000000000000000 ) ) ;
#69985 = CARTESIAN_POINT ( 'NONE',  ( 0.6496062992125991586, -0.5400638737290845981, -0.3530559997133363437 ) ) ;
#69987 = CARTESIAN_POINT ( 'NONE',  ( -1.614173228346456268, -0.5511811023622047445, 6.969142054262312111E-17 ) ) ;
#69988 = CARTESIAN_POINT ( 'NONE',  ( -0.03280839895013062252, 0.2952755905511810774, -0.1292274648535930714 ) ) ;
#69989 = CARTESIAN_POINT ( 'NONE',  ( 1.056430446194226436, -0.5511811023622048555, -0.09757992244046775898 ) ) ;
#69990 = CARTESIAN_POINT ( 'NONE',  ( -1.476377952755905110, -0.4536011799217368745, -0.2665933059059886201 ) ) ;
#69991 = CARTESIAN_POINT ( 'NONE',  ( 1.154855643044620184, -0.6046776061558807314, 0.2411417322834647770 ) ) ;
#69992 = CARTESIAN_POINT ( 'NONE',  ( -0.5380577427821514602, 0.05413385826771666132, 0.4176697321401328100 ) ) ;
#69993 = CARTESIAN_POINT ( 'NONE',  ( -0.3412073490813641308, -0.5023911411419708095, 0.1820866141732285504 ) ) ;
#69994 = CARTESIAN_POINT ( 'NONE',  ( -0.3937007874015740483, -0.1870078740157480879, -0.4822834645669291653 ) ) ;
#69995 = CARTESIAN_POINT ( 'NONE',  ( 1.377952755905512472, 0.2952755905511811885, 0.000000000000000000 ) ) ;
#69996 = CARTESIAN_POINT ( 'NONE',  ( -1.108923884514435132, -0.3162353388693405765, 0.4822834645669290543 ) ) ;
#69997 = CARTESIAN_POINT ( 'NONE',  ( 1.253280839895013710, -0.05778040916215560624, -0.4822834645669293319 ) ) ;
#69998 = CARTESIAN_POINT ( 'NONE',  ( 0.3917322834645670659, -0.1049643490035303273, -0.7382082921597920011 ) ) ;
#69999 = CARTESIAN_POINT ( 'NONE',  ( -1.227034120734907141, -0.5511811023622048555, -0.09757992244046775898 ) ) ;
#70000 = DIRECTION ( 'NONE',  ( 0.000000000000000000, 1.000000000000000000, -0.000000000000000000 ) ) ;
#70001 = CARTESIAN_POINT ( 'NONE',  ( 0.8792650918635177559, -0.4281496062992127816, -0.4176697321401328100 ) ) ;
#70002 = CARTESIAN_POINT ( 'NONE',  ( -0.3458507752293906723, -0.3458507752293910609, -2.340551181102362488 ) ) ;
#70003 = CARTESIAN_POINT ( 'NONE',  ( -1.686351706036744558, 0.2952755905511810774, -0.1292274648535930714 ) ) ;
#70004 = CARTESIAN_POINT ( 'NONE',  ( -1.601049868766403650, 0.1283753931104746893, -0.1820866141732285504 ) ) ;
#70005 = CARTESIAN_POINT ( 'NONE',  ( -1.128608923884513837, -0.5023911411419708095, 0.1820866141732285504 ) ) ;
#70006 = CARTESIAN_POINT ( 'NONE',  ( 1.430446194225722500, -0.3690944881889765550, -0.3153832671262227771 ) ) ;
#70007 = CARTESIAN_POINT ( 'NONE',  ( -0.5839895013123351797, -0.6692913385826771977, 0.1292274648535927661 ) ) ;
#70008 = CARTESIAN_POINT ( 'NONE',  ( -0.1377952755905504645, -0.4536011799217368745, -0.2665933059059886201 ) ) ;
#70009 = CARTESIAN_POINT ( 'NONE',  ( -1.679790026246718693, 0.1283753931104746893, -0.1820866141732285504 ) ) ;
#70010 = CARTESIAN_POINT ( 'NONE',  ( 0.9055118110236227702, -0.5511811023622047445, 6.969142054262312111E-17 ) ) ;
#70011 = CARTESIAN_POINT ( 'NONE',  ( 1.076115485564305141, 0.2306618581243847221, -0.2411417322834647770 ) ) ;
#70012 = CARTESIAN_POINT ( 'NONE',  ( 1.384514435695538337, -0.6692913385826771977, 0.1292274648535927661 ) ) ;
#70013 = CARTESIAN_POINT ( 'NONE',  ( 0.2165354330708668673, -0.4536011799217367080, 0.2665933059059888421 ) ) ;
#70014 = EDGE_CURVE ( 'NONE', #32076, #27377, #4859, .T. ) ;
#70015 = CARTESIAN_POINT ( 'NONE',  ( 0.6364829396325465405, -0.3162353388693409650, -0.4822834645669289433 ) ) ;
#70016 = CIRCLE ( 'NONE', #33750, 1.968503937007874072 ) ;
#70017 = CARTESIAN_POINT ( 'NONE',  ( 0.4002624671916016896, -0.2845877964562161244, -0.3641732283464567121 ) ) ;
#70018 = ORIENTED_EDGE ( 'NONE', *, *, #46613, .T. ) ;
#70019 = CARTESIAN_POINT ( 'NONE',  ( -1.601049868766403650, 0.2306618581243847221, -0.2411417322834647770 ) ) ;
#70020 = CARTESIAN_POINT ( 'NONE',  ( -1.233595800524933894, -0.6046776061558809534, -0.2411417322834644161 ) ) ;
#70021 = CARTESIAN_POINT ( 'NONE',  ( -0.6364829396325453192, -0.3162353388693405765, 0.4822834645669290543 ) ) ;
#70022 = CARTESIAN_POINT ( 'NONE',  ( 0.2925321140481932369, 0.2925321140481932369, -0.4527559055118110520 ) ) ;
#70023 = CARTESIAN_POINT ( 'NONE',  ( 0.2925321140481932369, 0.2925321140481932369, -2.576771653543307394 ) ) ;
#70024 = CARTESIAN_POINT ( 'NONE',  ( 0.3477690288713918276, 0.2952755905511811885, 0.1292274648535926551 ) ) ;
#70025 = CARTESIAN_POINT ( 'NONE',  ( 0.9842519685039375910, 0.1771653543307087630, 0.000000000000000000 ) ) ;
#70026 = CARTESIAN_POINT ( 'NONE',  ( -0.3346456692913377662, 0.1660481256975883668, -0.3530559997133364547 ) ) ;
#70027 = CARTESIAN_POINT ( 'NONE',  ( 0.3083989501312343062, -0.3162353388693405765, 0.4822834645669290543 ) ) ;
#70028 = CARTESIAN_POINT ( 'NONE',  ( -0.3996062992125986035, -0.1070741851644056997, -2.250656167979002920 ) ) ;
#70029 = CARTESIAN_POINT ( 'NONE',  ( 0.2891555358219910499, -0.2891555358219909944, -1.358267716535433101 ) ) ;
#70030 = CARTESIAN_POINT ( 'NONE',  ( -0.4252145377707324814, 1.326453916767273977, 1.038386062493871886 ) ) ;
#70031 = DIRECTION ( 'NONE',  ( 1.000000000000000000, -0.000000000000000000, -0.000000000000000000 ) ) ;
#70032 = CARTESIAN_POINT ( 'NONE',  ( 0.3917322834645669549, 0.1049643490035304660, -0.4317585301837270073 ) ) ;
#70033 = CARTESIAN_POINT ( 'NONE',  ( -0.7086614173228339419, -0.1870078740157480601, -0.3641732283464567677 ) ) ;
#70034 = CARTESIAN_POINT ( 'NONE',  ( -1.220472440944881054, 0.2952755905511811885, 0.000000000000000000 ) ) ;
#70035 = CARTESIAN_POINT ( 'NONE',  ( 0.2891555358219910499, 0.2891555358219910499, -2.419291338582677753 ) ) ;
#70036 = CARTESIAN_POINT ( 'NONE',  ( 0.8464566929133866546, -0.5400638737290844871, 0.3530559997133364547 ) ) ;
#70037 = CARTESIAN_POINT ( 'NONE',  ( 1.482939632545932307, 0.05413385826771626580, -0.4176697321401330321 ) ) ;
#70038 = CARTESIAN_POINT ( 'NONE',  ( 0.9842519685039375910, 0.2952755905511811885, 0.000000000000000000 ) ) ;
#70039 = CARTESIAN_POINT ( 'NONE',  ( 0.4724409448818895907, 0.1265901696524994180, -0.04396325459317588363 ) ) ;
#70040 = CARTESIAN_POINT ( 'NONE',  ( 0.3996062992125986035, 2.446882876249141962E-17, -2.322834645669291209 ) ) ;
#70041 = DIRECTION ( 'NONE',  ( -1.000000000000000000, -0.000000000000000000, -0.000000000000000000 ) ) ;
#70042 = CARTESIAN_POINT ( 'NONE',  ( 0.9383202099737536495, -0.3162353388693405765, 0.4822834645669290543 ) ) ;
#70043 = CARTESIAN_POINT ( 'NONE',  ( 0.7742782152230978099, -0.4281496062992124485, 0.4176697321401328655 ) ) ;
#70044 = CARTESIAN_POINT ( 'NONE',  ( 0.8464566929133865436, 0.07958543189024071263, -0.2665933059059888421 ) ) ;
#70045 = CARTESIAN_POINT ( 'NONE',  ( 1.332020997375329197, -0.3162353388693405765, 0.4822834645669290543 ) ) ;
#70046 = CARTESIAN_POINT ( 'NONE',  ( -0.1958661417322834220, -0.3392501089628018884, 0.007217847769028785422 ) ) ;
#70047 = CARTESIAN_POINT ( 'NONE',  ( 1.043307086614173818, 0.1660481256975885056, 0.3530559997133364547 ) ) ;
#70048 = CARTESIAN_POINT ( 'NONE',  ( 0.4396325459317593221, 0.2952755905511810774, -0.1292274648535930714 ) ) ;
#70049 = CARTESIAN_POINT ( 'NONE',  ( 1.430446194225722500, -0.3690944881889765550, -0.3153832671262227771 ) ) ;
#70050 = CARTESIAN_POINT ( 'NONE',  ( -0.7152230971128602510, -0.05778040916215560624, -0.4822834645669293319 ) ) ;
#70051 = CARTESIAN_POINT ( 'NONE',  ( -1.167979002624671470, -0.4281496062992127816, -0.4176697321401328100 ) ) ;
#70052 = AXIS2_PLACEMENT_3D ( 'NONE', #51202, #36942, #70579 ) ;
#70053 = CARTESIAN_POINT ( 'NONE',  ( 1.174540682414699111, -0.05778040916215560624, -0.4822834645669293319 ) ) ;
#70054 = CARTESIAN_POINT ( 'NONE',  ( -0.1958661417322836718, 0.3392501089628017219, -0.5702099737532808632 ) ) ;
#70055 = CARTESIAN_POINT ( 'NONE',  ( 0.2867679344610365999, 0.2867679344610365999, -1.389763779527558807 ) ) ;
#70056 = CARTESIAN_POINT ( 'NONE',  ( 0.1958661417322834775, 0.3392501089628018884, -2.656167979002624691 ) ) ;
#70057 = EDGE_LOOP ( 'NONE', ( #29698, #72646, #47410, #4533 ) ) ;
#70058 = CARTESIAN_POINT ( 'NONE',  ( 0.3460692066303959202, 0.1998031496062993295, -0.1312335958005249603 ) ) ;
#70059 = ORIENTED_EDGE ( 'NONE', *, *, #24157, .T. ) ;
#70060 = DIRECTION ( 'NONE',  ( 0.000000000000000000, 0.000000000000000000, -1.000000000000000000 ) ) ;
#70061 = CARTESIAN_POINT ( 'NONE',  ( 1.351706036745407458, -0.3690944881889765550, -0.3153832671262227771 ) ) ;
#70062 = CARTESIAN_POINT ( 'NONE',  ( -0.3460692066303960868, 0.1998031496062990242, -1.286089238845144367 ) ) ;
#70063 = CARTESIAN_POINT ( 'NONE',  ( 1.345144356955381593, -0.08942795157527998196, 0.3641732283464567121 ) ) ;
#70064 = CARTESIAN_POINT ( 'NONE',  ( 0.4581548277944226255, 1.539554514980418620, -0.5309055118110237448 ) ) ;
#70065 = DIRECTION ( 'NONE',  ( 0.000000000000000000, 0.000000000000000000, -1.000000000000000000 ) ) ;
#70066 = DIRECTION ( 'NONE',  ( -8.881784197001252323E-16, -9.738798461624180871E-16, 1.000000000000000000 ) ) ;
#70067 = CARTESIAN_POINT ( 'NONE',  ( -9.594673741351313045E-17, 0.3917322834645670104, -0.8720472440944883052 ) ) ;
#70068 = CARTESIAN_POINT ( 'NONE',  ( -0.9383202099737524282, -0.2845877964562161244, -0.3641732283464567121 ) ) ;
#70069 = CARTESIAN_POINT ( 'NONE',  ( -1.646981627296586703, -0.2845877964562161244, -0.3641732283464567121 ) ) ;
#70070 = CARTESIAN_POINT ( 'NONE',  ( -1.194225721784776262, -0.4281496062992124485, 0.4176697321401328655 ) ) ;
#70071 = CARTESIAN_POINT ( 'NONE',  ( 0.1706036745406830368, 0.05413385826771666132, 0.4176697321401328100 ) ) ;
#70072 = CARTESIAN_POINT ( 'NONE',  ( -1.587926509186350810, 0.05413385826771626580, -0.4176697321401330321 ) ) ;
#70073 = ORIENTED_EDGE ( 'NONE', *, *, #64982, .F. ) ;
#70074 = ADVANCED_FACE ( 'NONE', ( #48232 ), #42496, .F. ) ;
#70075 = CARTESIAN_POINT ( 'NONE',  ( -0.5120078740157480990, 0.3045572308828553565, -0.01849200668098333056 ) ) ;
#70076 =( LENGTH_UNIT ( ) NAMED_UNIT ( * ) SI_UNIT ( $, .METRE. ) );
#70077 = CARTESIAN_POINT ( 'NONE',  ( 0.4091458600556403535, 0.2362204724409449896, -2.020997375328084100 ) ) ;
#70078 = CARTESIAN_POINT ( 'NONE',  ( 0.4128810003509036930, 1.303691442895980490, -1.728827638849821824 ) ) ;
#70079 = CARTESIAN_POINT ( 'NONE',  ( -0.5643044619422565855, -0.3690944881889763329, 0.3153832671262228327 ) ) ;
#70080 = CARTESIAN_POINT ( 'NONE',  ( -1.036745406824146176, -0.4281496062992124485, 0.4176697321401328655 ) ) ;
#70081 = CARTESIAN_POINT ( 'NONE',  ( 1.122047244094488860, -0.5400638737290845981, -0.3530559997133363437 ) ) ;
#70082 = ORIENTED_EDGE ( 'NONE', *, *, #12663, .T. ) ;
#70084 = CARTESIAN_POINT ( 'NONE',  ( -1.586052503253848611, 0.7480314960629931287, 0.1653254495020559378 ) ) ;
#70083 = CARTESIAN_POINT ( 'NONE',  ( 0.4724409448818915891, -0.1265901696524958653, -2.316272965879265566 ) ) ;
#70085 = CARTESIAN_POINT ( 'NONE',  ( 1.207349081364829990, 0.2306618581243848609, 0.2411417322834645549 ) ) ;
#70086 = CARTESIAN_POINT ( 'NONE',  ( -1.266404199475064773, -0.3162353388693405765, 0.4822834645669290543 ) ) ;
#70087 = CARTESIAN_POINT ( 'NONE',  ( 0.3917322834645668994, -0.1049643490035303134, -0.5065423640081871959 ) ) ;
#70088 = CARTESIAN_POINT ( 'NONE',  ( -0.4790026246719154557, -0.2845877964562159024, 0.3641732283464567677 ) ) ;
#70089 = CARTESIAN_POINT ( 'NONE',  ( 0.3917322834645669549, 0.1049643490035304660, -0.6817585301837267853 ) ) ;
#70090 = CARTESIAN_POINT ( 'NONE',  ( -0.4658792650918627265, -0.2845877964562161244, -0.3641732283464567121 ) ) ;
#70091 = CARTESIAN_POINT ( 'NONE',  ( 0.3149606299212603933, -0.1870078740157479769, 0.3641732283464567677 ) ) ;
#70092 = CARTESIAN_POINT ( 'NONE',  ( 0.2821522309711292364, -0.6692913385826771977, 0.1292274648535927661 ) ) ;
#70093 = CARTESIAN_POINT ( 'NONE',  ( -0.7874015748031489847, -0.1870078740157480601, -0.3641732283464567677 ) ) ;
#70094 = CARTESIAN_POINT ( 'NONE',  ( -0.3917322834645669549, -0.1049643490035306603, -2.715223097112861250 ) ) ;
#70095 = CARTESIAN_POINT ( 'NONE',  ( 0.9908136482939640111, 0.2952755905511810774, -0.1292274648535930714 ) ) ;
#70096 = ADVANCED_FACE ( 'NONE', ( #17103 ), #51958, .F. ) ;
#70097 = ADVANCED_FACE ( 'NONE', ( #26321 ), #68696, .F. ) ;
#70098 = CARTESIAN_POINT ( 'NONE',  ( -1.384514435695537005, -0.6692913385826773087, -0.1292274648535924053 ) ) ;
#70099 = CARTESIAN_POINT ( 'NONE',  ( 0.1265901696524989462, 0.4724409448818897572, -1.015091863517060267 ) ) ;
#70100 = CARTESIAN_POINT ( 'NONE',  ( -0.5774278215223089816, 0.2306618581243847221, -0.2411417322834647770 ) ) ;
#70101 = CARTESIAN_POINT ( 'NONE',  ( -1.102362204724408601, -0.1870078740157480879, -0.4822834645669291653 ) ) ;
#70102 = CARTESIAN_POINT ( 'NONE',  ( 1.115485564304462551, -0.3690944881889765550, -0.3153832671262227771 ) ) ;
#70103 = CARTESIAN_POINT ( 'NONE',  ( -0.2493438320209966919, -0.004921259842519870586, -0.3153832671262229437 ) ) ;
#70104 = CARTESIAN_POINT ( 'NONE',  ( -0.8070866141732276899, -0.5400638737290844871, 0.3530559997133364547 ) ) ;
#70105 = CARTESIAN_POINT ( 'NONE',  ( -1.266404199475064773, -0.05778040916215560624, -0.4822834645669293319 ) ) ;
#70106 = DIRECTION ( 'NONE',  ( -1.000000000000000000, 0.000000000000000000, 0.000000000000000000 ) ) ;
#70107 = CARTESIAN_POINT ( 'NONE',  ( 1.279527559055118724, -0.4536011799217368745, -0.2665933059059886201 ) ) ;
#70108 = CARTESIAN_POINT ( 'NONE',  ( -0.2559055118110227234, -0.5400638737290844871, 0.3530559997133364547 ) ) ;
#70109 = VECTOR ( 'NONE', #60764, 39.37007874015748143 ) ;
#70110 = CARTESIAN_POINT ( 'NONE',  ( -1.213910761154854745, 0.2952755905511810774, -0.1292274648535930714 ) ) ;
#70111 = ORIENTED_EDGE ( 'NONE', *, *, #23437, .F. ) ;
#70112 = CARTESIAN_POINT ( 'NONE',  ( 0.1070741851644054776, -0.3996062992125984925, -2.209317585301837195 ) ) ;
#70113 = CARTESIAN_POINT ( 'NONE',  ( -0.7086614173228339419, -0.1870078740157479769, 0.3641732283464567677 ) ) ;
#70114 = CARTESIAN_POINT ( 'NONE',  ( 1.207349081364829990, -0.6046776061558809534, -0.2411417322834644161 ) ) ;
#70115 = CARTESIAN_POINT ( 'NONE',  ( -1.122047244094487306, -0.4536011799217367080, 0.2665933059059888421 ) ) ;
#70116 = CARTESIAN_POINT ( 'NONE',  ( -0.1070741851644056997, 0.3996062992125984925, -1.185695538057742526 ) ) ;
#70117 = CARTESIAN_POINT ( 'NONE',  ( -0.8989501312335946848, 0.2952755905511810774, -0.1292274648535930714 ) ) ;
#70118 = CARTESIAN_POINT ( 'NONE',  ( 0.8661417322834653598, -0.1870078740157479769, 0.4822834645669291653 ) ) ;
#70119 = CARTESIAN_POINT ( 'NONE',  ( 0.9711286089238851948, -0.6046776061558809534, -0.2411417322834644161 ) ) ;
#70120 = CARTESIAN_POINT ( 'NONE',  ( 1.541994750656168645, -0.6692913385826771977, 0.1292274648535927661 ) ) ;
#70121 = CARTESIAN_POINT ( 'NONE',  ( -1.371391076115484831, 0.1771653543307087075, -0.09757992244046823083 ) ) ;
#70122 = CARTESIAN_POINT ( 'NONE',  ( -0.1998031496062994405, 0.3460692066303957537, -0.7198162729658792447 ) ) ;
#70123 = CARTESIAN_POINT ( 'NONE',  ( 0.1070741851644053527, 0.3996062992125986590, -0.7808398950131233418 ) ) ;
#70124 = CARTESIAN_POINT ( 'NONE',  ( -0.1974969037888703871, -0.3420746716998661063, -0.06561679790026252179 ) ) ;
#70125 = CARTESIAN_POINT ( 'NONE',  ( 0.000000000000000000, 0.000000000000000000, 2.362204724409448620 ) ) ;
#70126 = CARTESIAN_POINT ( 'NONE',  ( 1.174540682414699111, -0.2845877964562159024, 0.3641732283464567677 ) ) ;
#70127 = CARTESIAN_POINT ( 'NONE',  ( 0.8858267716535438430, -0.4536011799217368745, -0.2665933059059886201 ) ) ;
#70128 = CARTESIAN_POINT ( 'NONE',  ( 0.4068241469816279987, -0.4281496062992127816, -0.4176697321401328100 ) ) ;
#70129 = CARTESIAN_POINT ( 'NONE',  ( 1.614173228346457378, 0.2952755905511811885, 0.000000000000000000 ) ) ;
#70130 = CARTESIAN_POINT ( 'NONE',  ( -0.3420746716998662729, 0.1974969037888702206, -1.520341207349081181 ) ) ;
#70131 = CARTESIAN_POINT ( 'NONE',  ( 0.6692913385826778638, -0.5511811023622047445, 6.969142054262312111E-17 ) ) ;
#70132 = CARTESIAN_POINT ( 'NONE',  ( -0.2099737532808391705, 0.2306618581243848609, 0.2411417322834645549 ) ) ;
#70133 = CARTESIAN_POINT ( 'NONE',  ( -1.272965879265091305, 0.05413385826771626580, -0.4176697321401330321 ) ) ;
#70134 = CARTESIAN_POINT ( 'NONE',  ( 0.8333333333333340365, -0.6692913385826771977, 0.1292274648535927661 ) ) ;
#70135 = CARTESIAN_POINT ( 'NONE',  ( -0.4091458600556405756, 0.2362204724409446288, -1.443569553805774230 ) ) ;
#70136 = DIRECTION ( 'NONE',  ( 0.000000000000000000, 1.000000000000000000, 0.000000000000000000 ) ) ;
#70137 = ORIENTED_EDGE ( 'NONE', *, *, #31689, .F. ) ;
#70138 = ORIENTED_EDGE ( 'NONE', *, *, #73756, .T. ) ;
#70139 = CARTESIAN_POINT ( 'NONE',  ( -1.135170603674539924, -0.6692913385826771977, 0.1292274648535927661 ) ) ;
#70140 = CARTESIAN_POINT ( 'NONE',  ( -0.4986876640419939388, 0.2306618581243847221, -0.2411417322834647770 ) ) ;
#70142 = CARTESIAN_POINT ( 'NONE',  ( -0.6364829396325453192, -0.05778040916215560624, -0.4822834645669293319 ) ) ;
#70141 = CARTESIAN_POINT ( 'NONE',  ( -0.7480314960629914633, -0.5511811023622047445, 6.969142054262312111E-17 ) ) ;
#70143 = CARTESIAN_POINT ( 'NONE',  ( -9.594673741351310580E-17, 0.3917322834645669549, -1.812316642223410046 ) ) ;
#70144 = CARTESIAN_POINT ( 'NONE',  ( 0.5643044619422579178, 0.05413385826771666132, 0.4176697321401328100 ) ) ;
#70145 = CARTESIAN_POINT ( 'NONE',  ( -0.2493438320209966919, -0.4281496062992124485, 0.4176697321401328655 ) ) ;
#70146 = CARTESIAN_POINT ( 'NONE',  ( -1.620734908136482577, 0.2952755905511811885, 0.1292274648535926551 ) ) ;
#70147 = CARTESIAN_POINT ( 'NONE',  ( -0.7874015748031489847, -0.1870078740157479769, 0.4822834645669291653 ) ) ;
#70148 = CARTESIAN_POINT ( 'NONE',  ( 0.4002624671916016896, -0.3162353388693409650, -0.4822834645669289433 ) ) ;
#70149 = ADVANCED_FACE ( 'NONE', ( #8608 ), #2593, .F. ) ;
#70150 = CARTESIAN_POINT ( 'NONE',  ( 0.3917322834645670104, 2.398668435337828261E-17, -1.527559055118110409 ) ) ;
#70151 = CARTESIAN_POINT ( 'NONE',  ( -0.9776902887139098386, 0.1771653543307087075, -0.09757992244046823083 ) ) ;
#70152 = ORIENTED_EDGE ( 'NONE', *, *, #50364, .T. ) ;
#70153 = CARTESIAN_POINT ( 'NONE',  ( 0.2891555358219910499, -0.2891555358219909944, -1.673228346456693272 ) ) ;
#70154 = ORIENTED_EDGE ( 'NONE', *, *, #69615, .F. ) ;
#70155 = CARTESIAN_POINT ( 'NONE',  ( -1.443569553805773564, -0.5023911411419708095, 0.1820866141732285504 ) ) ;
#70156 = CARTESIAN_POINT ( 'NONE',  ( -1.036745406824146176, -0.4281496062992124485, 0.4176697321401328655 ) ) ;
#70157 = CARTESIAN_POINT ( 'NONE',  ( -0.6824146981627288167, 0.2306618581243848609, 0.2411417322834645549 ) ) ;
#70158 = CARTESIAN_POINT ( 'NONE',  ( -0.1070741851644056997, 0.3996062992125986035, -0.3215223097112860362 ) ) ;
#70159 = CARTESIAN_POINT ( 'NONE',  ( -1.030183727034119867, -0.05778040916215560624, -0.4822834645669293319 ) ) ;
#70160 = CARTESIAN_POINT ( 'NONE',  ( -1.095800524934382292, -0.05778040916215522460, 0.4822834645669289988 ) ) ;
#70161 = CARTESIAN_POINT ( 'NONE',  ( -1.220472440944881054, 2.362204724409448620, 0.5309055118110237448 ) ) ;
#70162 = PLANE ( 'NONE',  #57663 ) ;
#70163 = CARTESIAN_POINT ( 'NONE',  ( 0.6889763779527566800, -0.4536011799217367080, 0.2665933059059888421 ) ) ;
#70164 = DIRECTION ( 'NONE',  ( -3.491481338843132961E-15, 0.000000000000000000, 1.000000000000000000 ) ) ;
#70165 = CARTESIAN_POINT ( 'NONE',  ( 0.1958661417322834775, 0.3392501089628018884, 0.08595800524934374409 ) ) ;
#70166 = CARTESIAN_POINT ( 'NONE',  ( -0.5577427821522301654, -0.08942795157528024563, -0.3641732283464568787 ) ) ;
#70167 = CARTESIAN_POINT ( 'NONE',  ( -0.2493438320209966919, -0.4281496062992124485, 0.4176697321401328655 ) ) ;
#70168 = CARTESIAN_POINT ( 'NONE',  ( 1.548556430446194954, -0.6046776061558807314, 0.2411417322834647770 ) ) ;
#70169 = CARTESIAN_POINT ( 'NONE',  ( -0.4527559055118102749, -0.5400638737290845981, -0.3530559997133363437 ) ) ;
#70170 = EDGE_LOOP ( 'NONE', ( #36215, #74029, #72240, #41207 ) ) ;
#70171 = ORIENTED_EDGE ( 'NONE', *, *, #68721, .F. ) ;
#70172 = CARTESIAN_POINT ( 'NONE',  ( -9.787531504996566615E-17, 0.3996062992125985480, -1.809055118110236560 ) ) ;
#70174 = CIRCLE ( 'NONE', #12388, 2.637795275590551380 ) ;
#70173 = CARTESIAN_POINT ( 'NONE',  ( -0.5314960629921250401, 0.1660481256975885056, 0.3530559997133364547 ) ) ;
#70175 = CARTESIAN_POINT ( 'NONE',  ( 1.095800524934383846, -0.3162353388693405765, 0.4822834645669290543 ) ) ;
#70176 = CARTESIAN_POINT ( 'NONE',  ( -1.089238845144356427, -0.004921259842519576551, 0.3153832671262227771 ) ) ;
#70177 = CARTESIAN_POINT ( 'NONE',  ( -1.292650918635170010, -0.6692913385826771977, 0.1292274648535927661 ) ) ;
#70178 = CARTESIAN_POINT ( 'NONE',  ( 5.785732909357575061E-17, -0.4724409448818898682, -0.8661417322834645827 ) ) ;
#70179 = LINE ( 'NONE', #76919, #76120 ) ;
#70180 = CARTESIAN_POINT ( 'NONE',  ( -0.3392501089628017219, -0.1958661417322836718, -0.04461942257217842850 ) ) ;
#70181 = CARTESIAN_POINT ( 'NONE',  ( 1.587926509186352142, 0.05413385826771666132, 0.4176697321401328100 ) ) ;
#70182 = CARTESIAN_POINT ( 'NONE',  ( 0.2867679344610366554, 0.2867679344610366554, -1.954724409448818978 ) ) ;
#70183 = CARTESIAN_POINT ( 'NONE',  ( 0.02624671916010564918, -0.6046776061558809534, -0.2411417322834644161 ) ) ;
#70184 = CARTESIAN_POINT ( 'NONE',  ( -1.056430446194224881, -0.5511811023622046335, 0.09757992244046803654 ) ) ;
#70185 = CARTESIAN_POINT ( 'NONE',  ( -0.2887139107611542133, 0.2306618581243848609, 0.2411417322834645549 ) ) ;
#70186 = CARTESIAN_POINT ( 'NONE',  ( -0.3458507752293909498, 0.3458507752293907833, -2.773622047244094002 ) ) ;
#70187 = CARTESIAN_POINT ( 'NONE',  ( -0.6889763779527552368, -0.5400638737290845981, -0.3530559997133363437 ) ) ;
#70188 = CARTESIAN_POINT ( 'NONE',  ( -1.207349081364828880, 0.2306618581243847221, -0.2411417322834647770 ) ) ;
#70189 = CARTESIAN_POINT ( 'NONE',  ( 0.1058382717557500852, -0.3949938075777408852, -2.051837270341207109 ) ) ;
#70190 = CARTESIAN_POINT ( 'NONE',  ( 0.9448818897637802916, -0.1870078740157479769, 0.3641732283464567677 ) ) ;
#70191 = CARTESIAN_POINT ( 'NONE',  ( -0.6299212598425188991, -0.1870078740157479769, 0.3641732283464567677 ) ) ;
#70192 = CARTESIAN_POINT ( 'NONE',  ( 0.9251968503937015864, 0.07958543189024071263, -0.2665933059059888421 ) ) ;
#70193 = CARTESIAN_POINT ( 'NONE',  ( -1.568241469816272105, -0.05778040916215522460, 0.4822834645669289988 ) ) ;
#70194 = CARTESIAN_POINT ( 'NONE',  ( 1.286089238845145033, 0.2306618581243848609, 0.2411417322834645549 ) ) ;
#70195 = CARTESIAN_POINT ( 'NONE',  ( 0.3740157480314966754, -0.4536011799217367080, 0.2665933059059888421 ) ) ;
#70196 = CARTESIAN_POINT ( 'NONE',  ( -0.7414698162729651543, -0.6692913385826771977, 0.1292274648535927661 ) ) ;
#70197 = CARTESIAN_POINT ( 'NONE',  ( 1.272965879265092637, 0.05413385826771666132, 0.4176697321401328100 ) ) ;
#70198 = CARTESIAN_POINT ( 'NONE',  ( -0.2362204724409451284, 0.4091458600556402425, -0.08989501312335958227 ) ) ;
#70199 = CARTESIAN_POINT ( 'NONE',  ( -0.2230971128608915943, -0.004921259842519576551, 0.3153832671262227771 ) ) ;
#70200 = CARTESIAN_POINT ( 'NONE',  ( -0.1742125984251974291, -0.000000000000000000, -0.3937007874015748254 ) ) ;
#70201 = CARTESIAN_POINT ( 'NONE',  ( 0.4002624671916016896, -0.05778040916215522460, 0.4822834645669289988 ) ) ;
#70202 = CARTESIAN_POINT ( 'NONE',  ( 0.9776902887139113929, 0.1771653543307087630, 0.09757992244046791164 ) ) ;
#70203 = CARTESIAN_POINT ( 'NONE',  ( 0.03937007874015806264, 0.1771653543307087630, 0.000000000000000000 ) ) ;
#70205 = ADVANCED_FACE ( 'NONE', ( #16828 ), #9672, .T. ) ;
#70204 = CARTESIAN_POINT ( 'NONE',  ( -1.535433070866141225, 0.2952755905511811885, 0.000000000000000000 ) ) ;
#70206 = CARTESIAN_POINT ( 'NONE',  ( -0.8005249343832011588, -0.004921259842519870586, -0.3153832671262229437 ) ) ;
#70207 = DIRECTION ( 'NONE',  ( -0.000000000000000000, -1.000000000000000000, -0.000000000000000000 ) ) ;
#70208 = CARTESIAN_POINT ( 'NONE',  ( -1.187664041994750175, -0.05778040916215560624, -0.4822834645669293319 ) ) ;
#70209 = CARTESIAN_POINT ( 'NONE',  ( -0.6364829396325453192, -0.05778040916215560624, -0.4822834645669293319 ) ) ;
#70210 = CARTESIAN_POINT ( 'NONE',  ( -0.1998031496062991630, -0.3460692066303959202, -1.244750656167979086 ) ) ;
#70211 = CARTESIAN_POINT ( 'NONE',  ( 0.2867679344610365999, 0.2867679344610365999, -2.269685039370078705 ) ) ;
#70212 = CARTESIAN_POINT ( 'NONE',  ( 0.2165354330708668673, 0.07958543189024071263, -0.2665933059059888421 ) ) ;
#70213 = CARTESIAN_POINT ( 'NONE',  ( -0.4330708661417315697, -0.6692913385826771977, 8.415575281601705876E-17 ) ) ;
#70214 = CARTESIAN_POINT ( 'NONE',  ( -0.7808398950131222316, -0.3162353388693409650, -0.4822834645669289433 ) ) ;
#70215 = CARTESIAN_POINT ( 'NONE',  ( -0.6889763779527552368, 0.07958543189024085140, 0.2665933059059887866 ) ) ;
#70216 = DIRECTION ( 'NONE',  ( 0.000000000000000000, 0.000000000000000000, -1.000000000000000000 ) ) ;
#70217 = CARTESIAN_POINT ( 'NONE',  ( 0.01968503937007957949, -0.5400638737290845981, -0.3530559997133363437 ) ) ;
#70218 = EDGE_CURVE ( 'NONE', #41616, #22014, #10908, .T. ) ;
#70219 = CARTESIAN_POINT ( 'NONE',  ( -1.489501312335957062, -0.2845877964562161244, -0.3641732283464567121 ) ) ;
#70220 = CARTESIAN_POINT ( 'NONE',  ( 1.259842519685040019, -0.1870078740157479769, 0.4822834645669291653 ) ) ;
#70221 = CARTESIAN_POINT ( 'NONE',  ( -0.4485266855423988286, 1.695194674715583494, 1.028590675108155716 ) ) ;
#70222 = AXIS2_PLACEMENT_3D ( 'NONE', #83130, #82315, #44793 ) ;
#70223 = CARTESIAN_POINT ( 'NONE',  ( 0.2867679344610366554, -0.2867679344610365999, -2.299888082186038574 ) ) ;
#70224 = ORIENTED_EDGE ( 'NONE', *, *, #58316, .T. ) ;
#70225 = EDGE_CURVE ( 'NONE', #4976, #11614, #60594, .T. ) ;
#70226 = DIRECTION ( 'NONE',  ( -0.5144957554275264577, 0.8574929257125440962, 1.050125966765366037E-16 ) ) ;
#70227 = CARTESIAN_POINT ( 'NONE',  ( -1.476377952755905110, -0.5400638737290845981, -0.3530559997133363437 ) ) ;
#70228 = CARTESIAN_POINT ( 'NONE',  ( -0.8464566929133852113, -0.5400638737290845981, -0.3530559997133363437 ) ) ;
#70229 = CARTESIAN_POINT ( 'NONE',  ( -1.515748031496062076, -0.5400638737290844871, 0.3530559997133364547 ) ) ;
#70230 = CARTESIAN_POINT ( 'NONE',  ( -9.594673741351313045E-17, 0.3917322834645670104, -1.974409448818897683 ) ) ;
#70231 = DIRECTION ( 'NONE',  ( 0.000000000000000000, -1.000000000000000000, 0.000000000000000000 ) ) ;
#70232 = CARTESIAN_POINT ( 'NONE',  ( 0.8727034120734913358, -0.05778040916215522460, 0.4822834645669289988 ) ) ;
#70233 = CARTESIAN_POINT ( 'NONE',  ( 0.2034120734908144990, -0.6692913385826771977, 0.1292274648535927661 ) ) ;
#70234 = CARTESIAN_POINT ( 'NONE',  ( -0.3252997568826541674, -5.134928753749862370E-15, -0.4281989832122467532 ) ) ;
#70235 = CARTESIAN_POINT ( 'NONE',  ( 0.3460692066303958092, 0.1998031496062993018, -2.727690288713910949 ) ) ;
#70236 = CARTESIAN_POINT ( 'NONE',  ( 1.312335958005249825, 0.1283753931104746893, -0.1820866141732285504 ) ) ;
#70237 = CARTESIAN_POINT ( 'NONE',  ( 0.2925321140481932369, -0.2925321140481932369, -1.200787401574803015 ) ) ;
#70238 = VERTEX_POINT ( 'NONE', #82438 ) ;
#70239 = CARTESIAN_POINT ( 'NONE',  ( 0.1958661417322834775, 0.3392501089628018884, 0.01638488369322645480 ) ) ;
#70240 = ORIENTED_EDGE ( 'NONE', *, *, #45026, .T. ) ;
#70241 = CARTESIAN_POINT ( 'NONE',  ( -0.1312335958005241554, 0.2306618581243848609, 0.2411417322834645549 ) ) ;
#70242 = CARTESIAN_POINT ( 'NONE',  ( -0.7283464566929126471, 0.1660481256975883668, -0.3530559997133364547 ) ) ;
#70243 = CARTESIAN_POINT ( 'NONE',  ( -1.489501312335957062, -0.05778040916215522460, 0.4822834645669289988 ) ) ;
#70244 = CARTESIAN_POINT ( 'NONE',  ( 0.6167979002624679463, 0.05413385826771626580, -0.4176697321401330321 ) ) ;
#70245 = CARTESIAN_POINT ( 'NONE',  ( 1.489501312335958172, -0.3162353388693405765, 0.4822834645669290543 ) ) ;
#70246 = CARTESIAN_POINT ( 'NONE',  ( -1.313877454013331780, 0.2929341459200028863, 0.6999040823587868720 ) ) ;
#70247 = CARTESIAN_POINT ( 'NONE',  ( 0.006561679790026889343, -0.3162353388693409650, -0.4822834645669289433 ) ) ;
#70248 = CARTESIAN_POINT ( 'NONE',  ( -1.102362204724408601, -0.1870078740157480879, -0.4822834645669291653 ) ) ;
#70249 = CARTESIAN_POINT ( 'NONE',  ( 1.522309711286089939, -0.6046776061558809534, -0.2411417322834644161 ) ) ;
#70250 = ADVANCED_FACE ( 'NONE', ( #63483 ), #3525, .T. ) ;
#70251 = CARTESIAN_POINT ( 'NONE',  ( 1.502624671916010790, -0.05778040916215522460, 0.4822834645669289988 ) ) ;
#70252 = CARTESIAN_POINT ( 'NONE',  ( 0.006561679790026889343, -0.05778040916215522460, 0.4822834645669289988 ) ) ;
#70253 = CARTESIAN_POINT ( 'NONE',  ( -0.1958661417322834220, -0.3392501089628018884, -0.05774278215223092176 ) ) ;
#70254 = CARTESIAN_POINT ( 'NONE',  ( 0.3083989501312343062, -0.08942795157528024563, -0.3641732283464568787 ) ) ;
#70255 = ORIENTED_EDGE ( 'NONE', *, *, #14652, .F. ) ;
#70256 = CARTESIAN_POINT ( 'NONE',  ( -0.3949938075777409963, -7.255918531996591613E-17, -0.1968503937007874682 ) ) ;
#70257 = ORIENTED_EDGE ( 'NONE', *, *, #40280, .F. ) ;
#70258 = CARTESIAN_POINT ( 'NONE',  ( 0.08530183727034192087, -0.2845877964562161244, -0.3641732283464567121 ) ) ;
#70259 = CARTESIAN_POINT ( 'NONE',  ( 2.554262525012262586, 1.537401574803149984, -0.4744094488188970171 ) ) ;
#70260 = CARTESIAN_POINT ( 'NONE',  ( -0.006561679790025524116, -0.3162353388693405765, 0.4822834645669290543 ) ) ;
#70261 = CARTESIAN_POINT ( 'NONE',  ( -0.1115485564304456306, 0.2952755905511810774, -0.1292274648535930714 ) ) ;
#70262 = CARTESIAN_POINT ( 'NONE',  ( -0.4593175853018366950, 0.05413385826771666132, 0.4176697321401328100 ) ) ;
#70263 = ADVANCED_FACE ( 'NONE', ( #81629 ), #24756, .T. ) ;
#70264 = CARTESIAN_POINT ( 'NONE',  ( 0.3392501089628018329, 0.1958661417322835607, -1.860255536254279862 ) ) ;
#70265 = CARTESIAN_POINT ( 'NONE',  ( -1.010498687664041384, 0.05413385826771666132, 0.4176697321401328100 ) ) ;
#70266 = CARTESIAN_POINT ( 'NONE',  ( -0.3917322834645671215, 0.1049643490035301469, -2.479658792650918375 ) ) ;
#70267 = CARTESIAN_POINT ( 'NONE',  ( 1.141732283464567566, 0.1771653543307087630, 0.000000000000000000 ) ) ;
#70268 = CIRCLE ( 'NONE', #28652, 0.4724409448818898682 ) ;
#70269 = CARTESIAN_POINT ( 'NONE',  ( 0.9776902887139113929, -0.6692913385826773087, -0.1292274648535924053 ) ) ;
#70270 = CARTESIAN_POINT ( 'NONE',  ( 0.7217847769028878924, 0.05413385826771666132, 0.4176697321401328100 ) ) ;
#70271 = CARTESIAN_POINT ( 'NONE',  ( -0.3460692066303960868, 0.1998031496062990242, -0.8136482939632546652 ) ) ;
#70272 = CARTESIAN_POINT ( 'NONE',  ( -1.279527559055116948, -0.5400638737290844871, 0.3530559997133364547 ) ) ;
#70273 = CARTESIAN_POINT ( 'NONE',  ( 0.3460692066303958092, 0.1998031496062993018, -0.2080052493438320216 ) ) ;
#70274 = CARTESIAN_POINT ( 'NONE',  ( 0.1070741851644054776, -0.3996062992125984925, -0.1620734908136483299 ) ) ;
#70275 = CARTESIAN_POINT ( 'NONE',  ( 0.03937007874015806264, 0.2952755905511811885, 0.000000000000000000 ) ) ;
#70276 = CARTESIAN_POINT ( 'NONE',  ( 0.2925321140481932369, -0.2925321140481932369, -2.618110236220472675 ) ) ;
#70277 = EDGE_CURVE ( 'NONE', #37754, #66965, #43689, .T. ) ;
#70278 = CARTESIAN_POINT ( 'NONE',  ( -0.1958661417322836718, 0.3392501089628017219, -1.672572178477690352 ) ) ;
#70279 = CARTESIAN_POINT ( 'NONE',  ( 1.377952755905512472, -0.6692913385826771977, 8.415575281601705876E-17 ) ) ;
#70280 = CARTESIAN_POINT ( 'NONE',  ( 1.364829396325460076, 0.2306618581243848609, 0.2411417322834645549 ) ) ;
#70281 = CARTESIAN_POINT ( 'NONE',  ( 0.3674540682414705883, -0.5023911411419708095, 0.1820866141732285504 ) ) ;
#70282 = CARTESIAN_POINT ( 'NONE',  ( 1.049868766404200127, -0.6046776061558809534, -0.2411417322834644161 ) ) ;
#70283 = CARTESIAN_POINT ( 'NONE',  ( -0.4724409448818898682, -8.678599364036362592E-17, -1.533464566929133799 ) ) ;
#70284 = CARTESIAN_POINT ( 'NONE',  ( 0.5380577427821529035, -0.3690944881889763329, 0.3153832671262228327 ) ) ;
#70285 = CARTESIAN_POINT ( 'NONE',  ( 0.1837270341207354329, 0.2306618581243848609, 0.2411417322834645549 ) ) ;
#70286 = CIRCLE ( 'NONE', #55502, 0.2165354330708659791 ) ;
#70287 = CARTESIAN_POINT ( 'NONE',  ( -0.3949938075777408852, -0.1058382717557502933, -1.067585301837270739 ) ) ;
#70288 = CARTESIAN_POINT ( 'NONE',  ( -1.377952755905511140, 0.2952755905511811885, 0.000000000000000000 ) ) ;
#70289 = CARTESIAN_POINT ( 'NONE',  ( 1.076115485564305141, -0.5023911411419708095, 0.1820866141732285504 ) ) ;
#70290 = CARTESIAN_POINT ( 'NONE',  ( -2.594245572444953130, 1.668131542012049717, -0.4562955581495596324 ) ) ;
#70291 = CARTESIAN_POINT ( 'NONE',  ( -0.4199475065616791736, 0.2306618581243847221, -0.2411417322834647770 ) ) ;
#70292 = CARTESIAN_POINT ( 'NONE',  ( -0.1115485564304453947, -0.5511811023622046335, 0.09757992244046803654 ) ) ;
#70293 = CARTESIAN_POINT ( 'NONE',  ( 0.4556365106396694786, 1.773775493036639617, 0.5309055118110234117 ) ) ;
#70294 = CARTESIAN_POINT ( 'NONE',  ( -0.1640419947506555343, -0.3162353388693405765, 0.4822834645669290543 ) ) ;
#70295 = CARTESIAN_POINT ( 'NONE',  ( 0.1377952755905518800, -0.4536011799217367080, 0.2665933059059888421 ) ) ;
#70296 = CARTESIAN_POINT ( 'NONE',  ( -0.2925321140481930149, -0.2925321140481933480, -2.183070866141731958 ) ) ;
#70297 = CARTESIAN_POINT ( 'NONE',  ( -0.006561679790025524116, -0.05778040916215560624, -0.4822834645669293319 ) ) ;
#70298 =( BOUNDED_CURVE ( )  B_SPLINE_CURVE ( 2, ( #53046, #27808, #77494, #13945, #79178, #39602, #19830, #7630, #40850, #40028, #58962, #71176, #32868 ),
 .UNSPECIFIED., .F., .F. ) 
 B_SPLINE_CURVE_WITH_KNOTS ( ( 3, 2, 2, 2, 2, 2, 3 ),
 ( 0.7187856400893463116, 0.7196969696969697239, 0.7234848484848485084, 0.7272727272727272929, 0.7310606060606060774, 0.7348484848484848619, 0.7357598144561083853 ),
 .UNSPECIFIED. ) 
 CURVE ( )  GEOMETRIC_REPRESENTATION_ITEM ( )  RATIONAL_B_SPLINE_CURVE ( ( 0.9875488213027523443, 0.9918020599134680371, 1.000000000000000000, 0.9659258262890683122, 1.000000000000000000, 0.9659258262890683122, 1.000000000000000000, 0.9659258262890683122, 1.000000000000000000, 0.9659258262890683122, 1.000000000000000000, 0.9918020599134671489, 0.9875488213027514561 ) ) 
 REPRESENTATION_ITEM ( '' )  );
#70299 = CARTESIAN_POINT ( 'NONE',  ( 4.797336870675655290E-17, -0.3917322834645669549, -1.733576484743095669 ) ) ;
#70300 = CARTESIAN_POINT ( 'NONE',  ( 1.286089238845145033, -0.5023911411419708095, -0.1820866141732282451 ) ) ;
#70301 = CARTESIAN_POINT ( 'NONE',  ( -1.112371124080194340, -2.567464376874931580E-15, -0.4445507791589072832 ) ) ;
#70302 = CARTESIAN_POINT ( 'NONE',  ( -0.9448818897637790704, -0.1870078740157479769, 0.3641732283464567677 ) ) ;
#70303 = CARTESIAN_POINT ( 'NONE',  ( -0.6955380577427815458, -0.3690944881889765550, -0.3153832671262227771 ) ) ;
#70304 = CARTESIAN_POINT ( 'NONE',  ( -0.2296587926509179312, -0.05778040916215522460, 0.4822834645669289988 ) ) ;
#70305 = CARTESIAN_POINT ( 'NONE',  ( -0.2559055118110230564, 0.1660481256975883668, -0.3530559997133364547 ) ) ;
#70306 = CARTESIAN_POINT ( 'NONE',  ( 0.5839895013123367340, 0.1771653543307087630, 0.09757992244046791164 ) ) ;
#70307 = CARTESIAN_POINT ( 'NONE',  ( -3.900966923095589678, 2.677165354330708791, -0.5314960629921260393 ) ) ;
#70308 = CARTESIAN_POINT ( 'NONE',  ( 1.397637795275591177, -0.4536011799217367080, 0.2665933059059888421 ) ) ;
#70309 = CARTESIAN_POINT ( 'NONE',  ( 0.6955380577427828781, -0.4281496062992124485, 0.4176697321401328655 ) ) ;
#70310 = DIRECTION ( 'NONE',  ( 0.000000000000000000, 0.000000000000000000, 1.000000000000000000 ) ) ;
#70311 = CARTESIAN_POINT ( 'NONE',  ( -0.3412073490813641308, -0.6046776061558807314, 0.2411417322834647770 ) ) ;
#70312 = CARTESIAN_POINT ( 'NONE',  ( -0.3392501089628017219, -0.1958661417322836718, -0.9245406824146982228 ) ) ;
#70313 = CARTESIAN_POINT ( 'NONE',  ( -1.377952755905511140, 0.2952755905511811885, 0.000000000000000000 ) ) ;
#70314 = CARTESIAN_POINT ( 'NONE',  ( 0.9645669291338591078, -0.5400638737290845981, -0.3530559997133363437 ) ) ;
#70315 = CARTESIAN_POINT ( 'NONE',  ( 0.3871391076115493490, -0.3162353388693405765, 0.4822834645669290543 ) ) ;
#70316 = CARTESIAN_POINT ( 'NONE',  ( -0.2508553453239640851, 1.134444486973533062, -3.929028906623472928 ) ) ;
#70317 = CARTESIAN_POINT ( 'NONE',  ( 0.2099737532808405305, -0.5023911411419708095, 0.1820866141732285504 ) ) ;
#70318 = CARTESIAN_POINT ( 'NONE',  ( 1.318897637795276356, -0.5400638737290844871, 0.3530559997133364547 ) ) ;
#70319 = EDGE_CURVE ( 'NONE', #22642, #44890, #30674, .T. ) ;
#70320 = CARTESIAN_POINT ( 'NONE',  ( -0.5052493438320203589, -0.5511811023622046335, 0.09757992244046803654 ) ) ;
#70321 = CARTESIAN_POINT ( 'NONE',  ( -0.8267716535433065062, 0.2952755905511811885, 0.000000000000000000 ) ) ;
#70322 = CARTESIAN_POINT ( 'NONE',  ( 0.1181102362204724532, 0.04921259842519689481, -0.08523872084492506440 ) ) ;
#70323 = CARTESIAN_POINT ( 'NONE',  ( 0.3805774278215230400, 0.05413385826771626580, -0.4176697321401330321 ) ) ;
#70324 = CARTESIAN_POINT ( 'NONE',  ( -0.8792650918635160906, -0.4281496062992124485, 0.4176697321401328655 ) ) ;
#70325 = CARTESIAN_POINT ( 'NONE',  ( -0.7349081364829390672, 0.1283753931104746893, -0.1820866141732285504 ) ) ;
#70326 = CARTESIAN_POINT ( 'NONE',  ( 0.2165354330708668673, 0.1660481256975883668, -0.3530559997133364547 ) ) ;
#70327 = CARTESIAN_POINT ( 'NONE',  ( -1.240157480314959759, 0.1660481256975885056, 0.3530559997133364547 ) ) ;
#70328 = CARTESIAN_POINT ( 'NONE',  ( -0.1443569553805765515, -0.4281496062992127816, -0.4176697321401328100 ) ) ;
#70329 = CARTESIAN_POINT ( 'NONE',  ( 1.141732283464567788, 0.2066929133858268208, 0.000000000000000000 ) ) ;
#70331 = CARTESIAN_POINT ( 'NONE',  ( 1.167979002624672580, 0.05413385826771626580, -0.4176697321401330321 ) ) ;
#70330 = PLANE ( 'NONE',  #251 ) ;
#70332 = CARTESIAN_POINT ( 'NONE',  ( 1.148293963254593875, -0.6692913385826771977, 0.1292274648535927661 ) ) ;
#70333 = CARTESIAN_POINT ( 'NONE',  ( -0.3392501089628017219, -0.1958661417322836718, -2.091863517060367439 ) ) ;
#70334 = CARTESIAN_POINT ( 'NONE',  ( -1.220472440944878834, 2.362204724409448620, -0.5309055118110234117 ) ) ;
#70335 = CARTESIAN_POINT ( 'NONE',  ( -0.9645669291338575535, -0.5400638737290844871, 0.3530559997133364547 ) ) ;
#70336 = B_SPLINE_CURVE_WITH_KNOTS ( 'NONE', 3,
 ( #67143, #67971, #3577, #67555 ),
 .UNSPECIFIED., .F., .F.,
 ( 4, 4 ),
 ( 3.593986969192262371E-07, 0.001287825409103155903 ),
 .UNSPECIFIED. ) ;
#70337 = CARTESIAN_POINT ( 'NONE',  ( 0.1265901696524989462, 0.4724409448818897572, -0.4658792650918635592 ) ) ;
#70338 = CARTESIAN_POINT ( 'NONE',  ( 0.1070741851644054915, -0.3996062992125986035, 0.07217847769028869209 ) ) ;
#70339 = ORIENTED_EDGE ( 'NONE', *, *, #3924, .T. ) ;
#70340 = CARTESIAN_POINT ( 'NONE',  ( -0.006561679790025524116, -0.08942795157528024563, -0.3641732283464568787 ) ) ;
#70342 = CARTESIAN_POINT ( 'NONE',  ( 0.3917322834645670104, -0.1049643490035303411, -1.993438320209974135 ) ) ;
#70341 = AXIS2_PLACEMENT_3D ( 'NONE', #56794, #77002, #50477 ) ;
#70343 = CARTESIAN_POINT ( 'NONE',  ( 0.8005249343832027131, 0.05413385826771666132, 0.4176697321401328100 ) ) ;
#70344 = CARTESIAN_POINT ( 'NONE',  ( 0.4724409448818896462, 0.1265901696524990294, -2.801837270341207553 ) ) ;
#70345 = CARTESIAN_POINT ( 'NONE',  ( -1.968503937007874072, 0.000000000000000000, 5.701968306260621233 ) ) ;
#70346 = CARTESIAN_POINT ( 'NONE',  ( -0.5511811023622038563, -0.1870078740157479769, 0.3641732283464567677 ) ) ;
#70347 = CARTESIAN_POINT ( 'NONE',  ( 1.377952755905512472, 0.2952755905511811885, 0.000000000000000000 ) ) ;
#70348 = CARTESIAN_POINT ( 'NONE',  ( 0.8070866141732288002, 0.07958543189024085140, 0.2665933059059887866 ) ) ;
#70349 = CARTESIAN_POINT ( 'NONE',  ( -0.1509186351706028884, -0.3162353388693409650, -0.4822834645669289433 ) ) ;
#70350 = CARTESIAN_POINT ( 'NONE',  ( 0.1049643490035304522, -0.3917322834645668994, -0.6377759598087122672 ) ) ;
#70351 = CARTESIAN_POINT ( 'NONE',  ( -0.9908136482939626788, 0.2952755905511811885, 0.1292274648535926551 ) ) ;
#70352 = CARTESIAN_POINT ( 'NONE',  ( -1.246719160104986512, -0.004921259842519576551, 0.3153832671262227771 ) ) ;
#70353 = CARTESIAN_POINT ( 'NONE',  ( -0.3740157480314953431, -0.5400638737290845981, -0.3530559997133363437 ) ) ;
#70354 = CARTESIAN_POINT ( 'NONE',  ( -1.614173228346456712, 2.401574803149606474, -0.1372047244094478091 ) ) ;
#70355 = CARTESIAN_POINT ( 'NONE',  ( 0.6414174258557936437, -2.592014407703319119E-15, 0.3791475997938231202 ) ) ;
#70356 = ORIENTED_EDGE ( 'NONE', *, *, #59980, .F. ) ;
#70357 = CARTESIAN_POINT ( 'NONE',  ( 0.1958661417322834775, 0.3392501089628018884, -2.030859210794962344 ) ) ;
#70358 = CARTESIAN_POINT ( 'NONE',  ( 0.4986876640419954376, -0.6046776061558809534, -0.2411417322834644161 ) ) ;
#70359 = VERTEX_POINT ( 'NONE', #76946 ) ;
#70360 = CARTESIAN_POINT ( 'NONE',  ( -0.8464566929133852113, -0.5400638737290845981, -0.3530559997133363437 ) ) ;
#70361 = CARTESIAN_POINT ( 'NONE',  ( 1.463254593175853824, 0.2952755905511810774, -0.1292274648535930714 ) ) ;
#70362 = CARTESIAN_POINT ( 'NONE',  ( 0.8530183727034126306, 0.05413385826771626580, -0.4176697321401330321 ) ) ;
#70363 = CARTESIAN_POINT ( 'NONE',  ( 0.07217847769028949700, -0.3162353388693405765, 0.4822834645669290543 ) ) ;
#70364 = CARTESIAN_POINT ( 'NONE',  ( -0.3917322834645670104, -7.196005306013484475E-17, -1.226377952755905776 ) ) ;
#70365 = CARTESIAN_POINT ( 'NONE',  ( -0.7742782152230965886, 0.05413385826771666132, 0.4176697321401328100 ) ) ;
#70366 = CARTESIAN_POINT ( 'NONE',  ( -0.3280839895013117347, 0.05413385826771626580, -0.4176697321401330321 ) ) ;
#70367 = CARTESIAN_POINT ( 'NONE',  ( -0.8267716535433065062, 0.2952755905511811885, 0.000000000000000000 ) ) ;
#70368 = CARTESIAN_POINT ( 'NONE',  ( -0.1049868766404193215, -0.5023911411419708095, 0.1820866141732285504 ) ) ;
#70369 = CARTESIAN_POINT ( 'NONE',  ( -0.002674255378528274645, 0.3979867861068626111, 1.060393565908085801E-17 ) ) ;
#70370 = CARTESIAN_POINT ( 'NONE',  ( -0.2493438320209966919, 0.05413385826771626580, -0.4176697321401330321 ) ) ;
#70371 = FACE_OUTER_BOUND ( 'NONE', #57914, .T. ) ;
#70372 = CARTESIAN_POINT ( 'NONE',  ( 1.220472440944882386, -0.6692913385826771977, 8.415575281601705876E-17 ) ) ;
#70373 = CARTESIAN_POINT ( 'NONE',  ( 0.4848604877838280647, 0.000000000000000000, 0.3464511005275205946 ) ) ;
#70374 = EDGE_LOOP ( 'NONE', ( #8448, #40174, #7460, #9726, #75252, #46480, #39223, #32190, #80005, #3737, #64366, #8893, #41075, #9850 ) ) ;
#70375 = ORIENTED_EDGE ( 'NONE', *, *, #238, .T. ) ;
#70376 = CARTESIAN_POINT ( 'NONE',  ( 0.1312335958005257930, 0.2306618581243847221, -0.2411417322834647770 ) ) ;
#70377 = CARTESIAN_POINT ( 'NONE',  ( -0.4330708661417315697, 0.1771653543307087630, 0.000000000000000000 ) ) ;
#70379 = CARTESIAN_POINT ( 'NONE',  ( -0.3996062992125986035, -1.273259842764937629E-12, -1.929133858267794599 ) ) ;
#70378 = CARTESIAN_POINT ( 'NONE',  ( 1.305774278215223960, -0.5511811023622046335, 0.09757992244046803654 ) ) ;
#70380 = CARTESIAN_POINT ( 'NONE',  ( 0.3392501089628018329, 0.1958661417322835607, -1.318241469816273215 ) ) ;
#70381 = CARTESIAN_POINT ( 'NONE',  ( 0.2362204724409449064, 0.4091458600556404646, -0.06364829396325459576 ) ) ;
#70382 = CARTESIAN_POINT ( 'NONE',  ( 1.456692913385827515, -0.5511811023622047445, 6.969142054262312111E-17 ) ) ;
#70383 = CARTESIAN_POINT ( 'NONE',  ( 1.482939632545932307, 0.05413385826771626580, -0.4176697321401330321 ) ) ;
#70384 = CARTESIAN_POINT ( 'NONE',  ( 0.3460692066303958092, 0.1998031496062993018, -2.727690288713910949 ) ) ;
#70385 = CARTESIAN_POINT ( 'NONE',  ( -0.08530183727034056085, -0.05778040916215560624, -0.4822834645669293319 ) ) ;
#70386 = CARTESIAN_POINT ( 'NONE',  ( -1.266404199475064773, -0.05778040916215560624, -0.4822834645669293319 ) ) ;
#70387 = AXIS2_PLACEMENT_3D ( 'NONE', #79884, #34001, #73972 ) ;
#70388 = CARTESIAN_POINT ( 'NONE',  ( -1.122047244094487306, -0.5400638737290844871, 0.3530559997133364547 ) ) ;
#70389 = CARTESIAN_POINT ( 'NONE',  ( 0.1115485564304467270, -0.6692913385826773087, -0.1292274648535924053 ) ) ;
#70390 = CARTESIAN_POINT ( 'NONE',  ( 0.1974969037888706092, -0.3420746716998660508, -0.01115485564304462274 ) ) ;
#70391 = CARTESIAN_POINT ( 'NONE',  ( 1.673228346456693494, 0.1660481256975885056, 0.3530559997133364547 ) ) ;
#70392 = CARTESIAN_POINT ( 'NONE',  ( 0.8267716535433077274, 0.2952755905511811885, 0.000000000000000000 ) ) ;
#70393 = CARTESIAN_POINT ( 'NONE',  ( 1.266404199475066328, -0.2845877964562161244, -0.3641732283464567121 ) ) ;
#70394 = CARTESIAN_POINT ( 'NONE',  ( 0.4606732211678798428, 1.541615089183433485, -0.5309055118110237448 ) ) ;
#70395 = CARTESIAN_POINT ( 'NONE',  ( 0.7677165354330716118, 0.07958543189024071263, -0.2665933059059888421 ) ) ;
#70396 = CARTESIAN_POINT ( 'NONE',  ( -1.423884514435694859, -0.05778040916215560624, -0.4822834645669293319 ) ) ;
#70397 = CARTESIAN_POINT ( 'NONE',  ( 0.3996062992125984925, 0.1070741851644054637, -0.8313648293963252778 ) ) ;
#70398 = CARTESIAN_POINT ( 'NONE',  ( 1.089238845144357759, 0.05413385826771626580, -0.4176697321401330321 ) ) ;
#70399 = CARTESIAN_POINT ( 'NONE',  ( 0.1049643490035304938, -0.3917322834645669549, -0.07742782152230967552 ) ) ;
#70401 = DIRECTION ( 'NONE',  ( 2.956072690630991733E-16, -1.000000000000000000, -5.002896285981958034E-32 ) ) ;
#70400 = CARTESIAN_POINT ( 'NONE',  ( 0.6102362204724416372, 0.1660481256975883668, -0.3530559997133364547 ) ) ;
#70402 = CARTESIAN_POINT ( 'NONE',  ( -1.496062992125983815, -0.1870078740157480601, -0.3641732283464567677 ) ) ;
#70403 = CARTESIAN_POINT ( 'NONE',  ( -0.1181102362204717315, -0.6692913385826771977, 8.415575281601705876E-17 ) ) ;
#70404 = CARTESIAN_POINT ( 'NONE',  ( 0.8202099737532813073, 0.1771653543307087630, 0.09757992244046791164 ) ) ;
#70405 = AXIS2_PLACEMENT_3D ( 'NONE', #74097, #16859, #72846 ) ;
#70406 = CARTESIAN_POINT ( 'NONE',  ( 0.7874015748031503170, -0.1870078740157480879, -0.4822834645669291653 ) ) ;
#70407 = CARTESIAN_POINT ( 'NONE',  ( -0.5395952360118024815, 0.02791078216816064370, 0.4328096321851915285 ) ) ;
#70408 = CARTESIAN_POINT ( 'NONE',  ( -0.4593175853018366950, -0.004921259842519576551, 0.3153832671262227771 ) ) ;
#70409 = CARTESIAN_POINT ( 'NONE',  ( -0.4068241469816267775, 0.05413385826771626580, -0.4176697321401330321 ) ) ;
#70410 = CARTESIAN_POINT ( 'NONE',  ( 1.686351706036745890, 0.2952755905511811885, 0.1292274648535926551 ) ) ;
#70411 = CARTESIAN_POINT ( 'NONE',  ( -1.332020997375327642, -0.3162353388693409650, -0.4822834645669289433 ) ) ;
#70412 = CARTESIAN_POINT ( 'NONE',  ( 0.9711286089238851948, -0.6046776061558809534, -0.2411417322834644161 ) ) ;
#70413 = CARTESIAN_POINT ( 'NONE',  ( 0.3392501089628018884, -0.1958661417322833942, -0.7316466123697656920 ) ) ;
#70414 = CARTESIAN_POINT ( 'NONE',  ( -1.450131233595799651, 0.1771653543307087075, -0.09757992244046823083 ) ) ;
#70415 = EDGE_CURVE ( 'NONE', #67389, #42893, #14293, .T. ) ;
#70416 = FACE_OUTER_BOUND ( 'NONE', #42732, .T. ) ;
#70417 = CARTESIAN_POINT ( 'NONE',  ( 0.9645669291338588858, 0.1660481256975885056, 0.3530559997133364547 ) ) ;
#70418 = CARTESIAN_POINT ( 'NONE',  ( -0.4724409448818898682, -8.678599364036362592E-17, -2.635826771653543066 ) ) ;
#70419 = CARTESIAN_POINT ( 'NONE',  ( -1.541994750656167090, 0.2952755905511811885, 0.1292274648535926551 ) ) ;
#70420 = CARTESIAN_POINT ( 'NONE',  ( -1.430446194225720724, -0.004921259842519870586, -0.3153832671262229437 ) ) ;
#70421 = CARTESIAN_POINT ( 'NONE',  ( -1.036745406824146176, -0.004921259842519870586, -0.3153832671262229437 ) ) ;
#70422 = CARTESIAN_POINT ( 'NONE',  ( -0.2952755905511803003, -0.5400638737290845981, -0.3530559997133363437 ) ) ;
#70423 = CARTESIAN_POINT ( 'NONE',  ( -0.3018372703412066094, -0.3690944881889765550, -0.3153832671262227771 ) ) ;
#70424 = CARTESIAN_POINT ( 'NONE',  ( -1.673228346456691717, 0.07958543189024071263, -0.2665933059059888421 ) ) ;
#70425 = CARTESIAN_POINT ( 'NONE',  ( 0.9973753280839902091, 0.1283753931104746893, -0.1820866141732285504 ) ) ;
#70426 = CARTESIAN_POINT ( 'NONE',  ( 0.6102362204724416372, 0.1660481256975883668, -0.3530559997133364547 ) ) ;
#70427 = CARTESIAN_POINT ( 'NONE',  ( 1.377952755905512472, -0.6692913385826771977, 8.415575281601705876E-17 ) ) ;
#70428 = CARTESIAN_POINT ( 'NONE',  ( -0.1377952755905504645, -0.4536011799217368745, -0.2665933059059886201 ) ) ;
#70429 = CARTESIAN_POINT ( 'NONE',  ( 0.3805774278215230400, -0.4281496062992124485, 0.4176697321401328655 ) ) ;
#70430 = CARTESIAN_POINT ( 'NONE',  ( 0.4265091863517067039, -0.5511811023622048555, -0.09757992244046775898 ) ) ;
#70431 = CARTESIAN_POINT ( 'NONE',  ( -1.633858267716534529, 0.1660481256975885056, 0.3530559997133364547 ) ) ;
#70432 = CARTESIAN_POINT ( 'NONE',  ( -1.135170603674539924, 0.2952755905511810774, -0.1292274648535930714 ) ) ;
#70433 = CARTESIAN_POINT ( 'NONE',  ( -0.5446194225721777693, -0.3162353388693409650, -0.4822834645669289433 ) ) ;
#70434 = CARTESIAN_POINT ( 'NONE',  ( -0.3996062992125985480, -0.1070741851644057135, -0.5183727034120735322 ) ) ;
#70435 = CARTESIAN_POINT ( 'NONE',  ( 0.1998031496062994128, -0.3460692066303957537, -2.845800524934383624 ) ) ;
#70436 = CARTESIAN_POINT ( 'NONE',  ( 0.5708661417322841158, -0.5400638737290845981, -0.3530559997133363437 ) ) ;
#70437 = CARTESIAN_POINT ( 'NONE',  ( 1.128608923884514947, 0.1283753931104748280, 0.1820866141732283561 ) ) ;
#70438 = CARTESIAN_POINT ( 'NONE',  ( -0.5839895013123351797, -0.6692913385826771977, 0.1292274648535927661 ) ) ;
#70439 = CARTESIAN_POINT ( 'NONE',  ( 0.5577427821522314977, -0.3162353388693409650, -0.4822834645669289433 ) ) ;
#70440 = CARTESIAN_POINT ( 'NONE',  ( 0.1998031496062992740, 0.3460692066303959757, -2.191601049868766360 ) ) ;
#70441 = CARTESIAN_POINT ( 'NONE',  ( -0.1974969037888703871, -0.3420746716998661063, -1.640419947506561948 ) ) ;
#70442 = CARTESIAN_POINT ( 'NONE',  ( 4.893765752498283924E-17, -0.3996062992125986035, -2.755905511811023612 ) ) ;
#70443 = CARTESIAN_POINT ( 'NONE',  ( 0.2362204724409449064, 0.4091458600556404646, -2.506561679790026087 ) ) ;
#70444 = AXIS2_PLACEMENT_3D ( 'NONE', #69254, #82300, #49470 ) ;
#70445 = CARTESIAN_POINT ( 'NONE',  ( 0.3917322834645670104, 2.398668435337828261E-17, -0.8976377952755905110 ) ) ;
#70446 = CARTESIAN_POINT ( 'NONE',  ( -1.069553805774277722, 0.1771653543307087630, 0.09757992244046791164 ) ) ;
#70447 = CARTESIAN_POINT ( 'NONE',  ( -1.207349081364828880, 0.2306618581243847221, -0.2411417322834647770 ) ) ;
#70448 = CARTESIAN_POINT ( 'NONE',  ( -0.2891555358219909388, -0.2891555358219912164, -2.655511811023621771 ) ) ;
#70449 = CARTESIAN_POINT ( 'NONE',  ( 0.8661417322834653598, -0.1870078740157479769, 0.4822834645669291653 ) ) ;
#70450 = CARTESIAN_POINT ( 'NONE',  ( 1.332020997375328974, -0.05778040916215560624, -0.4822834645669293319 ) ) ;
#70451 = CARTESIAN_POINT ( 'NONE',  ( 0.6167979002624678353, -0.4281496062992124485, 0.4176697321401328655 ) ) ;
#70452 = CARTESIAN_POINT ( 'NONE',  ( -1.157146581871515012E-16, 0.4724409448818898682, -2.834645669291338432 ) ) ;
#70453 = CARTESIAN_POINT ( 'NONE',  ( 0.3996062992125986035, 0.1070741851644054776, -2.014435695538057569 ) ) ;
#70454 = CARTESIAN_POINT ( 'NONE',  ( -0.3917322834645671770, 0.1049643490035302024, -0.9744287646007369075 ) ) ;
#70455 = CARTESIAN_POINT ( 'NONE',  ( 0.000000000000000000, 1.724409448818897905, 0.000000000000000000 ) ) ;
#70456 = CARTESIAN_POINT ( 'NONE',  ( 0.6692913385826777528, 0.2952755905511811885, 0.000000000000000000 ) ) ;
#70457 = CARTESIAN_POINT ( 'NONE',  ( 0.4790026246719167324, -0.05778040916215522460, 0.4822834645669289988 ) ) ;
#70458 = AXIS2_PLACEMENT_3D ( 'NONE', #49223, #42902, #50454 ) ;
#70459 = CARTESIAN_POINT ( 'NONE',  ( 0.9317585301837276734, -0.3690944881889763329, 0.3153832671262228327 ) ) ;
#70460 = CARTESIAN_POINT ( 'NONE',  ( 1.220472440944882608, 0.2952755905511811885, 0.000000000000000000 ) ) ;
#70461 = CARTESIAN_POINT ( 'NONE',  ( -0.1049643490035307020, 0.3917322834645669549, -0.2486876640419948270 ) ) ;
#70462 = CARTESIAN_POINT ( 'NONE',  ( 0.4855643044619428750, 0.05413385826771666132, 0.4176697321401328100 ) ) ;
#70463 = CARTESIAN_POINT ( 'NONE',  ( 0.9776902887139113929, -0.6692913385826773087, -0.1292274648535924053 ) ) ;
#70464 = CARTESIAN_POINT ( 'NONE',  ( 0.4593175853018380828, 0.05413385826771626580, -0.4176697321401330321 ) ) ;
#70465 = CARTESIAN_POINT ( 'NONE',  ( 1.108923884514436686, -0.2845877964562161244, -0.3641732283464567121 ) ) ;
#70466 = CARTESIAN_POINT ( 'NONE',  ( -0.7414698162729651543, 0.2952755905511810774, -0.1292274648535930714 ) ) ;
#70467 = CARTESIAN_POINT ( 'NONE',  ( -0.8727034120734901146, -0.05778040916215560624, -0.4822834645669293319 ) ) ;
#70468 = CARTESIAN_POINT ( 'NONE',  ( 1.272965879265092637, 0.05413385826771666132, 0.4176697321401328100 ) ) ;
#70469 = CARTESIAN_POINT ( 'NONE',  ( -0.2867679344610365999, 0.2867679344610364889, -0.7342519685039372579 ) ) ;
#70470 = CARTESIAN_POINT ( 'NONE',  ( 0.1958661417322834775, 0.3392501089628018884, -1.553805774278215202 ) ) ;
#70471 = CARTESIAN_POINT ( 'NONE',  ( 0.2867679344610365999, -0.2867679344610365444, -2.610236220472441193 ) ) ;
#70472 = ORIENTED_EDGE ( 'NONE', *, *, #71659, .T. ) ;
#70473 = CARTESIAN_POINT ( 'NONE',  ( 0.2925321140481932369, 0.2925321140481932369, -0.1377952755905512139 ) ) ;
#70474 = VERTEX_POINT ( 'NONE', #49607 ) ;
#70475 = CARTESIAN_POINT ( 'NONE',  ( 1.476377952755906442, -0.5400638737290844871, 0.3530559997133364547 ) ) ;
#70476 = CARTESIAN_POINT ( 'NONE',  ( 1.358267716535433323, -0.4536011799217368745, -0.2665933059059886201 ) ) ;
#70477 = CARTESIAN_POINT ( 'NONE',  ( 0.3996062992125986590, -0.1070741851644053111, -1.528871391076114916 ) ) ;
#70478 = CARTESIAN_POINT ( 'NONE',  ( 1.364829396325460076, 0.1283753931104748280, 0.1820866141732283561 ) ) ;
#70479 = CARTESIAN_POINT ( 'NONE',  ( 0.6184250938292470412, 2.084810923686589862E-15, -0.3791475997938226761 ) ) ;
#70480 = CARTESIAN_POINT ( 'NONE',  ( -0.4672469119858430053, 1.453788974454129912, 2.571228699324735079 ) ) ;
#70481 = CARTESIAN_POINT ( 'NONE',  ( 0.3937527723457950324, -0.009287274676460888917, -1.929133858267718660 ) ) ;
#70482 = CARTESIAN_POINT ( 'NONE',  ( 0.3917322834645670104, -0.1049643490035303411, -0.9835958005249345604 ) ) ;
#70483 = CARTESIAN_POINT ( 'NONE',  ( -0.5971128608923877978, -0.5511811023622048555, -0.09757992244046775898 ) ) ;
#70484 = CARTESIAN_POINT ( 'NONE',  ( -1.443569553805773564, -0.5023911411419708095, 0.1820866141732285504 ) ) ;
#70485 = CARTESIAN_POINT ( 'NONE',  ( -1.469816272965878357, 0.2306618581243848609, 0.2411417322834645549 ) ) ;
#70486 = CARTESIAN_POINT ( 'NONE',  ( 0.08530183727034192087, -0.3162353388693409650, -0.4822834645669289433 ) ) ;
#70487 = CARTESIAN_POINT ( 'NONE',  ( -1.594488188976377119, 0.1660481256975883668, -0.3530559997133364547 ) ) ;
#70488 = EDGE_LOOP ( 'NONE', ( #38388, #50460, #14793, #53306 ) ) ;
#70489 = CARTESIAN_POINT ( 'NONE',  ( -1.193521905106661674, 2.660739321503277841E-15, -0.3464511005275191513 ) ) ;
#70490 = DIRECTION ( 'NONE',  ( 1.000000000000000000, -6.123233995736767268E-17, 0.000000000000000000 ) ) ;
#70491 = CARTESIAN_POINT ( 'NONE',  ( -0.4724409448818899238, 0.1265901696524986686, -1.922572178477689908 ) ) ;
#70492 = CARTESIAN_POINT ( 'NONE',  ( -1.586052503253847057, 1.574803149606300412, 0.1653254495020574921 ) ) ;
#70493 = CARTESIAN_POINT ( 'NONE',  ( -0.6758530183727028406, 0.1771653543307087630, 0.09757992244046791164 ) ) ;
#70494 = CARTESIAN_POINT ( 'NONE',  ( -1.017060367454067249, -0.05778040916215522460, 0.4822834645669289988 ) ) ;
#70495 = CARTESIAN_POINT ( 'NONE',  ( 1.076115485564305141, 0.2306618581243847221, -0.2411417322834647770 ) ) ;
#70496 = ORIENTED_EDGE ( 'NONE', *, *, #24528, .T. ) ;
#70498 = DIRECTION ( 'NONE',  ( 0.000000000000000000, 0.000000000000000000, 1.000000000000000000 ) ) ;
#70497 = DIRECTION ( 'NONE',  ( 0.000000000000000000, 0.000000000000000000, -1.000000000000000000 ) ) ;
#70499 = CARTESIAN_POINT ( 'NONE',  ( 1.036745406824147731, 0.05413385826771666132, 0.4176697321401328100 ) ) ;
#70500 = CARTESIAN_POINT ( 'NONE',  ( -1.141732283464566011, -0.6692913385826771977, 8.415575281601705876E-17 ) ) ;
#70501 = CARTESIAN_POINT ( 'NONE',  ( -0.3392501089628019439, 0.1958661417322832554, -0.7362011566591059042 ) ) ;
#70502 = CARTESIAN_POINT ( 'NONE',  ( -0.3805774278215216522, -0.3690944881889765550, -0.3153832671262227771 ) ) ;
#70503 = CARTESIAN_POINT ( 'NONE',  ( 0.3917322834645670104, -0.1049643490035303273, -0.8261154855643044748 ) ) ;
#70504 = CIRCLE ( 'NONE', #10025, 3.937007874015748143 ) ;
#70505 = CARTESIAN_POINT ( 'NONE',  ( -0.6036745406824141069, -0.5023911411419708095, -0.1820866141732282451 ) ) ;
#70506 = CARTESIAN_POINT ( 'NONE',  ( 0.1771653543307093182, 0.07958543189024085140, 0.2665933059059887866 ) ) ;
#70507 = CARTESIAN_POINT ( 'NONE',  ( 0.1706036745406830368, 0.05413385826771666132, 0.4176697321401328100 ) ) ;
#70508 = CARTESIAN_POINT ( 'NONE',  ( -1.332020997375327642, -0.08942795157527998196, 0.3641732283464567121 ) ) ;
#70509 = CARTESIAN_POINT ( 'NONE',  ( -0.1958661417322836718, 0.3392501089628017219, -2.682414698162729483 ) ) ;
#70510 = CARTESIAN_POINT ( 'NONE',  ( 1.056430446194226436, -0.6692913385826773087, -0.1292274648535924053 ) ) ;
#70511 = ADVANCED_FACE ( 'NONE', ( #56335 ), #76537, .T. ) ;
#70512 = CARTESIAN_POINT ( 'NONE',  ( -1.332020997375327642, -0.05778040916215522460, 0.4822834645669289988 ) ) ;
#70513 = CARTESIAN_POINT ( 'NONE',  ( -0.4724409448818899238, 0.1265901696524986686, -1.211942257217847541 ) ) ;
#70514 = CARTESIAN_POINT ( 'NONE',  ( -0.2493438320209966919, 0.05413385826771626580, -0.4176697321401330321 ) ) ;
#70515 = CARTESIAN_POINT ( 'NONE',  ( -0.9514435695538050464, -0.05778040916215560624, -0.4822834645669293319 ) ) ;
#70516 = CARTESIAN_POINT ( 'NONE',  ( 0.8858267716535438430, 0.07958543189024085140, 0.2665933059059887866 ) ) ;
#70517 = AXIS2_PLACEMENT_3D ( 'NONE', #24211, #17105, #56199 ) ;
#70518 = CARTESIAN_POINT ( 'NONE',  ( -0.4790026246719154557, -0.2845877964562159024, 0.3641732283464567677 ) ) ;
#70519 = CARTESIAN_POINT ( 'NONE',  ( -0.6167979002624665030, 0.05413385826771666132, 0.4176697321401328100 ) ) ;
#70520 = CARTESIAN_POINT ( 'NONE',  ( -1.332020997375327642, -0.05778040916215522460, 0.4822834645669289988 ) ) ;
#70521 = DIRECTION ( 'NONE',  ( 0.000000000000000000, 0.000000000000000000, 1.000000000000000000 ) ) ;
#70522 = CARTESIAN_POINT ( 'NONE',  ( 1.259842519685040019, -0.1870078740157480601, -0.3641732283464567677 ) ) ;
#70523 = CARTESIAN_POINT ( 'NONE',  ( -0.1902887139107604098, 0.2952755905511810774, -0.1292274648535930714 ) ) ;
#70524 = CARTESIAN_POINT ( 'NONE',  ( -1.450131233595799651, -0.6692913385826771977, 0.1292274648535927661 ) ) ;
#70525 = ORIENTED_EDGE ( 'NONE', *, *, #36983, .F. ) ;
#70526 = CARTESIAN_POINT ( 'NONE',  ( -0.3996062992125985480, -7.340648628747423112E-17, -2.478346456692913868 ) ) ;
#70527 =( BOUNDED_CURVE ( )  B_SPLINE_CURVE ( 1, ( #54480, #41853 ),
 .UNSPECIFIED., .F., .F. ) 
 B_SPLINE_CURVE_WITH_KNOTS ( ( 2, 2 ),
 ( 0.0007457734483630566735, 0.002000000000000005246 ),
 .UNSPECIFIED. ) 
 CURVE ( )  GEOMETRIC_REPRESENTATION_ITEM ( )  RATIONAL_B_SPLINE_CURVE ( ( 0.9875488213027530104, 0.9875488213027530104 ) ) 
 REPRESENTATION_ITEM ( '' )  );
#70528 = CARTESIAN_POINT ( 'NONE',  ( -0.7283464566929126471, -0.4536011799217367080, 0.2665933059059888421 ) ) ;
#70529 = CARTESIAN_POINT ( 'NONE',  ( 0.5314960629921264834, 0.1660481256975883668, -0.3530559997133364547 ) ) ;
#70530 = CARTESIAN_POINT ( 'NONE',  ( -1.076115485564303809, 0.1283753931104748280, 0.1820866141732283561 ) ) ;
#70531 = CARTESIAN_POINT ( 'NONE',  ( -0.2925321140481930149, -0.2925321140481933480, -1.238188976377952999 ) ) ;
#70532 = CARTESIAN_POINT ( 'NONE',  ( -1.161417322834644716, -0.5400638737290845981, -0.3530559997133363437 ) ) ;
#70533 = CARTESIAN_POINT ( 'NONE',  ( 0.7414698162729663755, 0.2952755905511811885, 0.1292274648535926551 ) ) ;
#70534 = CARTESIAN_POINT ( 'NONE',  ( 0.2887139107611556010, 0.2306618581243847221, -0.2411417322834647770 ) ) ;
#70535 = CARTESIAN_POINT ( 'NONE',  ( -0.2362204724409447953, -0.4091458600556404646, -0.06561679790026246628 ) ) ;
#70536 = CARTESIAN_POINT ( 'NONE',  ( -1.633858267716534529, -0.4536011799217368745, -0.2665933059059886201 ) ) ;
#70537 = CARTESIAN_POINT ( 'NONE',  ( 0.3460692066303958092, 0.1998031496062993018, -0.5229658792650918597 ) ) ;
#70538 = CARTESIAN_POINT ( 'NONE',  ( -0.1070741851644051862, -0.3996062992125987146, -1.017060367454067915 ) ) ;
#70539 = CARTESIAN_POINT ( 'NONE',  ( 0.2891555358219910499, -0.2891555358219909944, -0.09842519685039378963 ) ) ;
#70540 = CARTESIAN_POINT ( 'NONE',  ( 0.4744094488188886349, 1.546132656481029599, 2.554262525012303886 ) ) ;
#70541 = CARTESIAN_POINT ( 'NONE',  ( 1.089238845144357759, -0.004921259842519870586, -0.3153832671262229437 ) ) ;
#70542 = ADVANCED_FACE ( 'NONE', ( #18466 ), #17646, .T. ) ;
#70543 = CARTESIAN_POINT ( 'NONE',  ( 0.1443569553805781891, -0.3690944881889763329, 0.3153832671262228327 ) ) ;
#70544 = CARTESIAN_POINT ( 'NONE',  ( 0.1771653543307093182, 0.1660481256975885056, 0.3530559997133364547 ) ) ;
#70545 = CARTESIAN_POINT ( 'NONE',  ( -0.2362204724409447953, -0.4091458600556404646, -2.347112860892388575 ) ) ;
#70546 = CARTESIAN_POINT ( 'NONE',  ( 0.3949938075777409963, 2.418639510665530743E-17, -1.139763779527559251 ) ) ;
#70547 = CARTESIAN_POINT ( 'NONE',  ( 0.2296587926509192634, -0.2845877964562159024, 0.3641732283464567677 ) ) ;
#70548 = CARTESIAN_POINT ( 'NONE',  ( -0.6233595800524928121, -0.3162353388693409650, -0.4822834645669289433 ) ) ;
#70549 = CARTESIAN_POINT ( 'NONE',  ( -1.292650918635170010, 0.2952755905511810774, -0.1292274648535930714 ) ) ;
#70550 = CARTESIAN_POINT ( 'NONE',  ( 0.6824146981627303710, -0.6046776061558807314, 0.2411417322834647770 ) ) ;
#70551 = CARTESIAN_POINT ( 'NONE',  ( 0.2362204724409449064, 0.4091458600556404646, -1.404199475065616820 ) ) ;
#70552 = DIRECTION ( 'NONE',  ( 1.000000000000000000, -0.000000000000000000, -0.000000000000000000 ) ) ;
#70553 = B_SPLINE_CURVE_WITH_KNOTS ( 'NONE', 3,
 ( #49573, #73310, #9332, #8915 ),
 .UNSPECIFIED., .F., .F.,
 ( 4, 4 ),
 ( 0.05883702829161106124, 0.06031386722719112026 ),
 .UNSPECIFIED. ) ;
#70554 = ORIENTED_EDGE ( 'NONE', *, *, #27043, .F. ) ;
#70555 = ORIENTED_EDGE ( 'NONE', *, *, #30143, .F. ) ;
#70556 = CARTESIAN_POINT ( 'NONE',  ( -1.482939632545930975, -0.4281496062992127816, -0.4176697321401328100 ) ) ;
#70557 = CARTESIAN_POINT ( 'NONE',  ( -0.5774278215223089816, -0.6046776061558807314, 0.2411417322834647770 ) ) ;
#70559 = CARTESIAN_POINT ( 'NONE',  ( -0.7480314960629914633, -0.6692913385826771977, 8.415575281601705876E-17 ) ) ;
#70558 = CARTESIAN_POINT ( 'NONE',  ( -0.5774278215223089816, -0.5023911411419708095, 0.1820866141732285504 ) ) ;
#70560 = CARTESIAN_POINT ( 'NONE',  ( -0.3917322834645668994, -0.1049643490035306742, -2.015728715714224517 ) ) ;
#70561 = CARTESIAN_POINT ( 'NONE',  ( 0.1377952755905518800, -0.4536011799217367080, 0.2665933059059888421 ) ) ;
#70562 = LINE ( 'NONE', #71405, #12739 ) ;
#70563 = CARTESIAN_POINT ( 'NONE',  ( -1.640419947506561060, -0.004921259842519576551, 0.3153832671262227771 ) ) ;
#70564 = CARTESIAN_POINT ( 'NONE',  ( -1.194225721784776262, 0.05413385826771626580, -0.4176697321401330321 ) ) ;
#70565 = CARTESIAN_POINT ( 'NONE',  ( 0.3018372703412079971, -0.4281496062992124485, 0.4176697321401328655 ) ) ;
#70566 = CARTESIAN_POINT ( 'NONE',  ( -0.8661417322834640276, -0.1870078740157479769, 0.4822834645669291653 ) ) ;
#70567 = EDGE_CURVE ( 'NONE', #16379, #47374, #69440, .T. ) ;
#70568 = CARTESIAN_POINT ( 'NONE',  ( -0.2867679344610364334, -0.2867679344610367109, -1.625984251968503491 ) ) ;
#70569 = CARTESIAN_POINT ( 'NONE',  ( -0.9186351706036736120, -0.5023911411419708095, -0.1820866141732282451 ) ) ;
#70570 = VERTEX_POINT ( 'NONE', #11325 ) ;
#70571 = CARTESIAN_POINT ( 'NONE',  ( -0.2891555358219908833, -0.2891555358219912164, -1.791338582677165725 ) ) ;
#70572 = VERTEX_POINT ( 'NONE', #51244 ) ;
#70573 = CARTESIAN_POINT ( 'NONE',  ( -1.594488188976377563, -0.4536011799217367080, 0.2665933059059888421 ) ) ;
#70574 = CARTESIAN_POINT ( 'NONE',  ( -1.213910761154854745, -0.6692913385826771977, 0.1292274648535927661 ) ) ;
#70575 = CARTESIAN_POINT ( 'NONE',  ( -0.7480314960629914633, -0.6692913385826771977, 8.415575281601705876E-17 ) ) ;
#70576 = CARTESIAN_POINT ( 'NONE',  ( -0.3460692066303958092, -0.1998031496062994683, -0.05249343832020997996 ) ) ;
#70577 = CARTESIAN_POINT ( 'NONE',  ( -1.240157480314959759, 0.1660481256975885056, 0.3530559997133364547 ) ) ;
#70578 = CARTESIAN_POINT ( 'NONE',  ( -1.325459317585300889, -0.4281496062992127816, -0.4176697321401328100 ) ) ;
#70579 = DIRECTION ( 'NONE',  ( -3.096699300667737957E-16, 1.000000000000000000, -0.000000000000000000 ) ) ;
#70580 = CARTESIAN_POINT ( 'NONE',  ( 0.4724409448818898682, 0.000000000000000000, -2.755905511811024056 ) ) ;
#70581 = AXIS2_PLACEMENT_3D ( 'NONE', #74322, #41081, #78988 ) ;
#70582 = CARTESIAN_POINT ( 'NONE',  ( 0.3149606299212606708, -0.1870078740157480601, -0.3641732283464567677 ) ) ;
#70583 = CARTESIAN_POINT ( 'NONE',  ( -0.4831401376419939830, -3.153061149046662969E-15, -0.4118477457933005237 ) ) ;
#70584 = CARTESIAN_POINT ( 'NONE',  ( 0.3917322834645670104, 2.398668435337828261E-17, -0.3602362204724410266 ) ) ;
#70585 = CARTESIAN_POINT ( 'NONE',  ( -0.2362204724409442680, -0.1870078740157480601, -0.3641732283464567677 ) ) ;
#70586 = CARTESIAN_POINT ( 'NONE',  ( -0.6627296587926501115, 0.2952755905511810774, -0.1292274648535930714 ) ) ;
#70587 = CARTESIAN_POINT ( 'NONE',  ( 1.325459317585302665, 0.05413385826771626580, -0.4176697321401330321 ) ) ;
#70588 = CARTESIAN_POINT ( 'NONE',  ( -0.5839895013123351797, -0.6692913385826771977, 0.1292274648535927661 ) ) ;
#70589 = CARTESIAN_POINT ( 'NONE',  ( 0.000000000000000000, 0.04921259842519689481, 0.08523872084492503665 ) ) ;
#70590 = ORIENTED_EDGE ( 'NONE', *, *, #34333, .T. ) ;
#70591 = CARTESIAN_POINT ( 'NONE',  ( 0.1070741851644053388, 0.3996062992125986035, -1.959973753280839892 ) ) ;
#70592 = CARTESIAN_POINT ( 'NONE',  ( -0.9186351706036736120, -0.6046776061558809534, -0.2411417322834644161 ) ) ;
#70593 = CARTESIAN_POINT ( 'NONE',  ( 1.482939632545932307, 0.05413385826771626580, -0.4176697321401330321 ) ) ;
#70594 = CARTESIAN_POINT ( 'NONE',  ( -1.200787401574802349, 0.07958543189024071263, -0.2665933059059888421 ) ) ;
#70595 = CARTESIAN_POINT ( 'NONE',  ( -1.502624671916009680, -0.05778040916215560624, -0.4822834645669293319 ) ) ;
#70596 = CARTESIAN_POINT ( 'NONE',  ( -0.1265901696524986964, -0.4724409448818899238, -0.7020997375328084100 ) ) ;
#70597 = CARTESIAN_POINT ( 'NONE',  ( -3.900966923095589678, 2.677165354330708791, 0.5314960629921260393 ) ) ;
#70598 = CARTESIAN_POINT ( 'NONE',  ( 0.1958661417322836440, -0.3392501089628017219, -0.3989501312335957950 ) ) ;
#70599 = CARTESIAN_POINT ( 'NONE',  ( 0.1049643490035304799, -0.3917322834645669549, -2.217191601049868677 ) ) ;
#70600 = CARTESIAN_POINT ( 'NONE',  ( 0.1049868766404206816, 0.2306618581243848609, 0.2411417322834645549 ) ) ;
#70601 = CARTESIAN_POINT ( 'NONE',  ( -1.069553805774277722, -0.5511811023622048555, -0.09757992244046775898 ) ) ;
#70602 = CARTESIAN_POINT ( 'NONE',  ( -0.7414698162729651543, 0.2952755905511810774, -0.1292274648535930714 ) ) ;
#70603 = CARTESIAN_POINT ( 'NONE',  ( -0.2362204724409451284, 0.4091458600556402425, -2.767060367454068359 ) ) ;
#70604 = CARTESIAN_POINT ( 'NONE',  ( -1.345144356955379816, -0.05778040916215560624, -0.4822834645669293319 ) ) ;
#70605 = CARTESIAN_POINT ( 'NONE',  ( -1.023622047244094002, -0.1870078740157480879, -0.4822834645669291653 ) ) ;
#70606 = CARTESIAN_POINT ( 'NONE',  ( -0.1574803149606292529, -0.1870078740157479769, 0.4822834645669291653 ) ) ;
#70607 = CARTESIAN_POINT ( 'NONE',  ( 0.1058382717557500852, -0.3949938075777408852, -2.524278215223097366 ) ) ;
#70608 = CARTESIAN_POINT ( 'NONE',  ( 0.9908136482939640111, 0.1771653543307087075, -0.09757992244046823083 ) ) ;
#70609 = CARTESIAN_POINT ( 'NONE',  ( -0.6167979002624665030, -0.004921259842519576551, 0.3153832671262227771 ) ) ;
#70610 = CARTESIAN_POINT ( 'NONE',  ( -0.04000121214432307559, 1.064648596787614032, -1.441347525760512838 ) ) ;
#70611 = CARTESIAN_POINT ( 'NONE',  ( 0.8202099737532814183, -0.5511811023622048555, -0.09757992244046775898 ) ) ;
#70612 = CARTESIAN_POINT ( 'NONE',  ( 1.194225721784777594, -0.3690944881889765550, -0.3153832671262227771 ) ) ;
#70613 = CARTESIAN_POINT ( 'NONE',  ( 1.246719160104987623, -0.4281496062992124485, 0.4176697321401328655 ) ) ;
#70614 = CARTESIAN_POINT ( 'NONE',  ( 0.5052493438320218022, -0.5511811023622048555, -0.09757992244046775898 ) ) ;
#70615 = CARTESIAN_POINT ( 'NONE',  ( 0.1049643490035304938, -0.3917322834645669549, -1.652230971128608505 ) ) ;
#70616 = CARTESIAN_POINT ( 'NONE',  ( -0.8333333333333323711, 0.2952755905511811885, 0.1292274648535926551 ) ) ;
#70617 = CARTESIAN_POINT ( 'NONE',  ( 1.345144356955381593, -0.3162353388693409650, -0.4822834645669289433 ) ) ;
#70618 = CARTESIAN_POINT ( 'NONE',  ( -0.3458507752293909498, 0.3458507752293907833, 0.06102362204724409017 ) ) ;
#70619 = CARTESIAN_POINT ( 'NONE',  ( -0.5052493438320203589, 0.1771653543307087075, -0.09757992244046823083 ) ) ;
#70620 = CARTESIAN_POINT ( 'NONE',  ( 0.03937007874015806264, 0.2952755905511811885, 0.000000000000000000 ) ) ;
#70621 = CARTESIAN_POINT ( 'NONE',  ( 0.4265091863517067594, 0.2952755905511811885, 0.1292274648535926551 ) ) ;
#70622 = DIRECTION ( 'NONE',  ( 0.000000000000000000, 0.000000000000000000, 1.000000000000000000 ) ) ;
#70623 = CARTESIAN_POINT ( 'NONE',  ( 0.8530183727034126306, -0.004921259842519870586, -0.3153832671262229437 ) ) ;
#70624 = CARTESIAN_POINT ( 'NONE',  ( 0.04593175853018440641, 0.1771653543307087075, -0.09757992244046823083 ) ) ;
#70625 = CARTESIAN_POINT ( 'NONE',  ( 0.06561679790026316017, -0.4281496062992124485, 0.4176697321401328655 ) ) ;
#70626 = CARTESIAN_POINT ( 'NONE',  ( -1.450131233595799651, -0.6692913385826771977, 0.1292274648535927661 ) ) ;
#70627 = CARTESIAN_POINT ( 'NONE',  ( -0.5708661417322825615, -0.4536011799217367080, 0.2665933059059888421 ) ) ;
#70628 = CARTESIAN_POINT ( 'NONE',  ( -0.3503937007874015630, -0.5120078740157480990, -0.01968503937007903132 ) ) ;
#70629 = CARTESIAN_POINT ( 'NONE',  ( -0.3018372703412066094, -0.4281496062992127816, -0.4176697321401328100 ) ) ;
#70630 = CARTESIAN_POINT ( 'NONE',  ( -0.2925321140481930149, -0.2925321140481933480, -1.238188976377952999 ) ) ;
#70631 = CARTESIAN_POINT ( 'NONE',  ( 0.3917322834645670104, -0.1049643490035303411, -2.558398950131233196 ) ) ;
#70632 = CARTESIAN_POINT ( 'NONE',  ( 0.2296587926509192634, -0.08942795157528024563, -0.3641732283464568787 ) ) ;
#70633 = CARTESIAN_POINT ( 'NONE',  ( -0.7480314960629914633, -0.6692913385826771977, 8.415575281601705876E-17 ) ) ;
#70634 = AXIS2_PLACEMENT_3D ( 'NONE', #30357, #30775, #56436 ) ;
#70635 = CARTESIAN_POINT ( 'NONE',  ( -0.9448818897637790704, -0.1870078740157480879, -0.4822834645669291653 ) ) ;
#70636 = CARTESIAN_POINT ( 'NONE',  ( -1.318897637795274802, 0.07958543189024085140, 0.2665933059059887866 ) ) ;
#70637 = CARTESIAN_POINT ( 'NONE',  ( -3.908778449111570463, 1.475589138410839052, -0.4706212595521235831 ) ) ;
#70638 = CARTESIAN_POINT ( 'NONE',  ( -0.3412073490813641308, 0.2306618581243847221, -0.2411417322834647770 ) ) ;
#70639 = CARTESIAN_POINT ( 'NONE',  ( -0.8923884514435688198, -0.5023911411419708095, 0.1820866141732285504 ) ) ;
#70640 = CARTESIAN_POINT ( 'NONE',  ( -1.679790026246718693, 0.1283753931104746893, -0.1820866141732285504 ) ) ;
#70641 = CARTESIAN_POINT ( 'NONE',  ( 1.272965879265092637, 0.05413385826771666132, 0.4176697321401328100 ) ) ;
#70642 = CARTESIAN_POINT ( 'NONE',  ( 5.785732909357575061E-17, -0.4724409448818898682, -0.7086614173228346081 ) ) ;
#70643 = CARTESIAN_POINT ( 'NONE',  ( -0.2867679344610365444, -0.2867679344610367664, -1.945557373524620992 ) ) ;
#70644 = ORIENTED_EDGE ( 'NONE', *, *, #5930, .T. ) ;
#70645 = DIRECTION ( 'NONE',  ( -0.000000000000000000, -1.000000000000000000, -0.000000000000000000 ) ) ;
#70646 = EDGE_CURVE ( 'NONE', #76146, #25432, #37402, .T. ) ;
#70647 = CARTESIAN_POINT ( 'NONE',  ( -1.259842519685038686, -0.1870078740157479769, 0.4822834645669291653 ) ) ;
#70648 = CARTESIAN_POINT ( 'NONE',  ( -0.8202099737532801971, -0.6692913385826771977, 0.1292274648535927661 ) ) ;
#70649 = CARTESIAN_POINT ( 'NONE',  ( -1.476377952755905110, 0.1660481256975885056, 0.3530559997133364547 ) ) ;
#70650 = CARTESIAN_POINT ( 'NONE',  ( -0.1958661417322836718, 0.3392501089628017219, -2.145013123359580387 ) ) ;
#70651 = CARTESIAN_POINT ( 'NONE',  ( 1.463254593175853824, -0.5511811023622046335, 0.09757992244046803654 ) ) ;
#70652 = CARTESIAN_POINT ( 'NONE',  ( 0.4265091863517067594, 0.2952755905511811885, 0.1292274648535926551 ) ) ;
#70653 = CARTESIAN_POINT ( 'NONE',  ( 0.1509186351706045259, -0.05778040916215560624, -0.4822834645669293319 ) ) ;
#70654 = CARTESIAN_POINT ( 'NONE',  ( -0.3249695492770445782, -2.567464376874931580E-15, -0.4445507791589072832 ) ) ;
#70655 = DIRECTION ( 'NONE',  ( -3.096699300667737957E-16, 1.000000000000000000, -0.000000000000000000 ) ) ;
#70656 = CARTESIAN_POINT ( 'NONE',  ( 0.9514435695538062676, -0.08942795157527998196, 0.3641732283464567121 ) ) ;
#70657 = B_SPLINE_CURVE_WITH_KNOTS ( 'NONE', 3,
 ( #55085, #66086, #2108, #9667, #54679, #60590, #79558, #22290, #35336, #48361, #53437, #47536, #73654, #9256 ),
 .UNSPECIFIED., .F., .F.,
 ( 4, 2, 2, 2, 2, 2, 4 ),
 ( 0.000000000000000000, 0.0003923887041693363098, 0.0007847774083386726196, 0.001177166112508008875, 0.001569554816677345239, 0.002354332225016047241, 0.003139109633354749025 ),
 .UNSPECIFIED. ) ;
#70658 = CARTESIAN_POINT ( 'NONE',  ( 4.893765752498283924E-17, -0.3996062992125986035, -1.338582677165354173 ) ) ;
#70659 = ORIENTED_EDGE ( 'NONE', *, *, #1862, .F. ) ;
#70660 = CARTESIAN_POINT ( 'NONE',  ( -0.3917322834645670104, -7.196005306013484475E-17, -2.866141732283464361 ) ) ;
#70661 = VERTEX_POINT ( 'NONE', #38634 ) ;
#70662 = CARTESIAN_POINT ( 'NONE',  ( -0.2099737532808391705, -0.6046776061558809534, -0.2411417322834644161 ) ) ;
#70663 = CARTESIAN_POINT ( 'NONE',  ( -0.8923884514435688198, 0.2306618581243847221, -0.2411417322834647770 ) ) ;
#70664 = CARTESIAN_POINT ( 'NONE',  ( -1.528871391076114250, -0.6692913385826771977, 0.1292274648535927661 ) ) ;
#70665 = CARTESIAN_POINT ( 'NONE',  ( 0.5971128608923891301, 0.2952755905511810774, -0.1292274648535930714 ) ) ;
#70666 = CARTESIAN_POINT ( 'NONE',  ( -1.587926509186350810, -0.004921259842519870586, -0.3153832671262229437 ) ) ;
#70667 = CARTESIAN_POINT ( 'NONE',  ( 1.437007874015748810, 0.1660481256975885056, 0.3530559997133364547 ) ) ;
#70668 = CARTESIAN_POINT ( 'NONE',  ( -0.3937007874015740483, -0.1870078740157479769, 0.4822834645669291653 ) ) ;
#70669 = CARTESIAN_POINT ( 'NONE',  ( 0.5708661417322841158, -0.5400638737290845981, -0.3530559997133363437 ) ) ;
#70670 = CARTESIAN_POINT ( 'NONE',  ( -1.614173228346455824, 0.2952755905511811885, 0.000000000000000000 ) ) ;
#70671 = CARTESIAN_POINT ( 'NONE',  ( 1.299212598425197429, 0.2952755905511811885, 0.000000000000000000 ) ) ;
#70672 = CARTESIAN_POINT ( 'NONE',  ( 1.679790026246720025, 0.2306618581243848609, 0.2411417322834645549 ) ) ;
#70673 = CARTESIAN_POINT ( 'NONE',  ( -0.2427821522309703550, -0.05778040916215560624, -0.4822834645669293319 ) ) ;
#70674 = ADVANCED_FACE ( 'NONE', ( #4581 ), #30252, .F. ) ;
#70675 = CARTESIAN_POINT ( 'NONE',  ( -0.3917322834645671215, 0.1049643490035301469, -0.3398950131233596239 ) ) ;
#70676 = CARTESIAN_POINT ( 'NONE',  ( 0.4265091863517067594, 0.1771653543307087630, 0.09757992244046791164 ) ) ;
#70677 = ORIENTED_EDGE ( 'NONE', *, *, #2876, .F. ) ;
#70678 = CARTESIAN_POINT ( 'NONE',  ( 0.1974969037888704704, 0.3420746716998660508, -0.4593175853018373056 ) ) ;
#70679 = ORIENTED_EDGE ( 'NONE', *, *, #18297, .T. ) ;
#70680 = CARTESIAN_POINT ( 'NONE',  ( -0.3805774278215216522, -0.3690944881889765550, -0.3153832671262227771 ) ) ;
#70681 = AXIS2_PLACEMENT_3D ( 'NONE', #20541, #40312, #64312 ) ;
#70682 = CIRCLE ( 'NONE', #39806, 0.5118110236220471121 ) ;
#70683 = CARTESIAN_POINT ( 'NONE',  ( -0.3503937007874015630, -0.3242060844882008741, 0.000000000000000000 ) ) ;
#70684 = CARTESIAN_POINT ( 'NONE',  ( 0.2165354330708668673, 0.1660481256975883668, -0.3530559997133364547 ) ) ;
#70685 = CARTESIAN_POINT ( 'NONE',  ( -0.02624671916010428221, -0.6046776061558807314, 0.2411417322834647770 ) ) ;
#70686 = ADVANCED_FACE ( 'NONE', ( #39473 ), #766, .F. ) ;
#70687 = CARTESIAN_POINT ( 'NONE',  ( -0.8858267716535425107, 0.1660481256975883668, -0.3530559997133364547 ) ) ;
#70688 = CARTESIAN_POINT ( 'NONE',  ( -0.3392501089628017219, -0.1958661417322836995, -1.781515378773965042 ) ) ;
#70689 = CARTESIAN_POINT ( 'NONE',  ( -1.095800524934382292, -0.3162353388693409650, -0.4822834645669289433 ) ) ;
#70690 = LINE ( 'NONE', #38696, #78725 ) ;
#70691 = CARTESIAN_POINT ( 'NONE',  ( 0.8661417322834652488, -0.1870078740157480601, -0.3641732283464567677 ) ) ;
#70692 = CARTESIAN_POINT ( 'NONE',  ( 0.4133858267716541968, 0.1660481256975885056, 0.3530559997133364547 ) ) ;
#70693 = CARTESIAN_POINT ( 'NONE',  ( 0.9580052493438327987, -0.4281496062992127816, -0.4176697321401328100 ) ) ;
#70694 = CARTESIAN_POINT ( 'NONE',  ( 4.893765752498283924E-17, -0.3996062992125986035, -1.338582677165354173 ) ) ;
#70695 = CARTESIAN_POINT ( 'NONE',  ( 0.3268936723430476143, 1.795490347638496118E-16, 0.3627985898453511271 ) ) ;
#70696 = CARTESIAN_POINT ( 'NONE',  ( -0.2925321140481932369, 0.2925321140481931259, -0.8838582677165351953 ) ) ;
#70697 = CARTESIAN_POINT ( 'NONE',  ( -0.3996062992125985480, -7.340648628747423112E-17, -0.2736220472440945017 ) ) ;
#70698 = CARTESIAN_POINT ( 'NONE',  ( -0.02624671916010428221, -0.6046776061558807314, 0.2411417322834647770 ) ) ;
#70699 = CARTESIAN_POINT ( 'NONE',  ( 0.1070741851644053527, 0.3996062992125986590, -2.513123359580052174 ) ) ;
#70700 = CARTESIAN_POINT ( 'NONE',  ( -0.3917322834645669549, -0.1049643490035306603, -1.547900262467191590 ) ) ;
#70701 = CARTESIAN_POINT ( 'NONE',  ( -1.272965879265091305, -0.004921259842519870586, -0.3153832671262229437 ) ) ;
#70702 = CARTESIAN_POINT ( 'NONE',  ( 1.338582677165355062, -0.1870078740157480879, -0.4822834645669291653 ) ) ;
#70703 = CONICAL_SURFACE ( 'NONE', #76058, 2.362204724409449508, 0.8726646259971734265 ) ;
#70704 = CARTESIAN_POINT ( 'NONE',  ( 1.181102362204725198, -0.1870078740157479769, 0.4822834645669291653 ) ) ;
#70705 = CARTESIAN_POINT ( 'NONE',  ( 8.195543980992789655E-16, -0.1870078740157480601, -0.3641732283464567677 ) ) ;
#70706 = CARTESIAN_POINT ( 'NONE',  ( 0.4724409448818904789, -0.1870078740157479769, 0.4822834645669291653 ) ) ;
#70707 = CARTESIAN_POINT ( 'NONE',  ( -0.2362204724409447953, -0.4091458600556404646, -1.402230971128609172 ) ) ;
#70708 = CARTESIAN_POINT ( 'NONE',  ( 0.5052493438320218022, -0.5511811023622048555, -0.09757992244046775898 ) ) ;
#70709 = CARTESIAN_POINT ( 'NONE',  ( 0.1968503937007881344, 0.2952755905511811885, 0.000000000000000000 ) ) ;
#70710 = CARTESIAN_POINT ( 'NONE',  ( 0.1974969037888704704, 0.3420746716998660508, -0.8510498687664042050 ) ) ;
#70711 = CARTESIAN_POINT ( 'NONE',  ( -1.200787401574802349, 0.1660481256975883668, -0.3530559997133364547 ) ) ;
#70712 = CARTESIAN_POINT ( 'NONE',  ( 0.6627296587926515548, 0.1771653543307087630, 0.09757992244046791164 ) ) ;
#70713 = EDGE_CURVE ( 'NONE', #63415, #43601, #22191, .T. ) ;
#70714 = CARTESIAN_POINT ( 'NONE',  ( -2.586063147568568699, 1.653225543546882781, -0.4603267246303533455 ) ) ;
#70715 = CARTESIAN_POINT ( 'NONE',  ( -0.1377952755905504645, 0.1660481256975885056, 0.3530559997133364547 ) ) ;
#70716 = CARTESIAN_POINT ( 'NONE',  ( -0.4265091863517051496, -0.5511811023622046335, 0.09757992244046803654 ) ) ;
#70717 = DIRECTION ( 'NONE',  ( 0.000000000000000000, 0.000000000000000000, 1.000000000000000000 ) ) ;
#70718 = CARTESIAN_POINT ( 'NONE',  ( -0.3412073490813641308, -0.6046776061558807314, 0.2411417322834647770 ) ) ;
#70719 = CARTESIAN_POINT ( 'NONE',  ( 0.1181102362204730916, -0.5511811023622047445, 6.969142054262312111E-17 ) ) ;
#70720 = CARTESIAN_POINT ( 'NONE',  ( -9.787531504996566615E-17, 0.3996062992125985480, -2.124015748031496287 ) ) ;
#70721 = CARTESIAN_POINT ( 'NONE',  ( -0.07217847769028787330, -0.05778040916215522460, 0.4822834645669289988 ) ) ;
#70722 =( BOUNDED_CURVE ( )  B_SPLINE_CURVE ( 2, ( #38096, #11622, #31366, #74776, #82726, #30956, #76007, #49902, #29724, #56623, #69277, #70083, #25045 ),
 .UNSPECIFIED., .F., .F. ) 
 B_SPLINE_CURVE_WITH_KNOTS ( ( 3, 2, 2, 2, 2, 2, 3 ),
 ( 0.7625000000000000666, 0.7666666666666668295, 0.7708333333333334814, 0.7750000000000001332, 0.7791666666666667851, 0.7833333333333334370, 0.7875000000000000888 ),
 .UNSPECIFIED. ) 
 CURVE ( )  GEOMETRIC_REPRESENTATION_ITEM ( )  RATIONAL_B_SPLINE_CURVE ( ( 0.9999999999999991118, 0.9659258262890692004, 1.000000000000000000, 0.9659258262890683122, 1.000000000000000000, 0.9659258262890683122, 1.000000000000000000, 0.9659258262890683122, 1.000000000000000000, 0.9659258262890683122, 1.000000000000000000, 0.9659258262890674240, 1.000000000000000888 ) ) 
 REPRESENTATION_ITEM ( '' )  );
#70723 = CARTESIAN_POINT ( 'NONE',  ( 0.3392501089628018329, -0.1958661417322834497, -1.759823203903200017 ) ) ;
#70724 = CARTESIAN_POINT ( 'NONE',  ( 1.351706036745407680, -0.004921259842519576551, 0.3153832671262227771 ) ) ;
#70725 = CARTESIAN_POINT ( 'NONE',  ( 0.4835386291766070044, 2.606013654608237919E-15, 0.3954974714151456849 ) ) ;
#70726 = CARTESIAN_POINT ( 'NONE',  ( -0.9973753280839886548, -0.5023911411419708095, -0.1820866141732282451 ) ) ;
#70727 = CARTESIAN_POINT ( 'NONE',  ( -0.7808398950131225646, -0.08942795157527998196, 0.3641732283464567121 ) ) ;
#70728 = CARTESIAN_POINT ( 'NONE',  ( -0.6036745406824141069, -0.6046776061558809534, -0.2411417322834644161 ) ) ;
#70729 = CARTESIAN_POINT ( 'NONE',  ( 0.05905511811023681640, 0.1660481256975883668, -0.3530559997133364547 ) ) ;
#70730 = CARTESIAN_POINT ( 'NONE',  ( 0.6758530183727039509, -0.5511811023622046335, 0.09757992244046803654 ) ) ;
#70731 = LINE ( 'NONE', #64415, #63600 ) ;
#70732 = CARTESIAN_POINT ( 'NONE',  ( 0.8989501312335963501, -0.5511811023622048555, -0.09757992244046775898 ) ) ;
#70733 = ADVANCED_FACE ( 'NONE', ( #39047 ), #65160, .F. ) ;
#70734 = CARTESIAN_POINT ( 'NONE',  ( 0.7677165354330716118, 0.1660481256975883668, -0.3530559997133364547 ) ) ;
#70735 = CARTESIAN_POINT ( 'NONE',  ( -1.646051170424378096, -0.1870078740157480046, 1.254653134982923898E-17 ) ) ;
#70736 = CARTESIAN_POINT ( 'NONE',  ( -0.05905511811023545637, -0.5400638737290845981, -0.3530559997133363437 ) ) ;
#70737 = AXIS2_PLACEMENT_3D ( 'NONE', #4469, #81505, #23827 ) ;
#70738 = CARTESIAN_POINT ( 'NONE',  ( 0.1958661417322836440, -0.3392501089628017219, -1.121391076115485719 ) ) ;
#70739 = CARTESIAN_POINT ( 'NONE',  ( 1.423884514435696191, -0.08942795157527998196, 0.3641732283464567121 ) ) ;
#70740 = CARTESIAN_POINT ( 'NONE',  ( 0.7545931758530189937, 0.2952755905511810774, -0.1292274648535930714 ) ) ;
#70741 = VECTOR ( 'NONE', #17079, 39.37007874015748143 ) ;
#70742 = CARTESIAN_POINT ( 'NONE',  ( -0.03280839895013062252, 0.2952755905511810774, -0.1292274648535930714 ) ) ;
#70743 = CARTESIAN_POINT ( 'NONE',  ( -0.2893689214265932619, 1.160196156542221413, -3.926443535894562409 ) ) ;
#70744 = CARTESIAN_POINT ( 'NONE',  ( 0.5446194225721792126, -0.2845877964562159024, 0.3641732283464567677 ) ) ;
#70745 = CARTESIAN_POINT ( 'NONE',  ( 0.7414698162729663755, 0.2952755905511811885, 0.1292274648535926551 ) ) ;
#70746 = CARTESIAN_POINT ( 'NONE',  ( -0.4199475065616791736, 0.1283753931104746893, -0.1820866141732285504 ) ) ;
#70747 = CARTESIAN_POINT ( 'NONE',  ( -0.7414698162729651543, -0.6692913385826771977, 0.1292274648535927661 ) ) ;
#70748 = CARTESIAN_POINT ( 'NONE',  ( -0.03443470937339728616, 0.2929341459200028863, -1.537015892239756099 ) ) ;
#70749 = CARTESIAN_POINT ( 'NONE',  ( 0.1706036745406830368, 0.05413385826771666132, 0.4176697321401328100 ) ) ;
#70750 = CARTESIAN_POINT ( 'NONE',  ( -1.384514435695537005, -0.6692913385826773087, -0.1292274648535924053 ) ) ;
#70751 = CARTESIAN_POINT ( 'NONE',  ( -0.8398950131233589023, -0.5023911411419708095, -0.1820866141732282451 ) ) ;
#70752 = CARTESIAN_POINT ( 'NONE',  ( 0.2427821522309716595, -0.3162353388693409650, -0.4822834645669289433 ) ) ;
#70753 = CARTESIAN_POINT ( 'NONE',  ( -1.312335958005248715, -0.6046776061558809534, -0.2411417322834644161 ) ) ;
#70754 = CARTESIAN_POINT ( 'NONE',  ( -0.4986876640419939388, 0.2306618581243847221, -0.2411417322834647770 ) ) ;
#70755 = EDGE_CURVE ( 'NONE', #30707, #820, #14655, .T. ) ;
#70757 = CARTESIAN_POINT ( 'NONE',  ( 1.535433070866142335, -0.6692913385826771977, 8.415575281601705876E-17 ) ) ;
#70756 = DIRECTION ( 'NONE',  ( 0.000000000000000000, -1.000000000000000000, 0.000000000000000000 ) ) ;
#70758 = CARTESIAN_POINT ( 'NONE',  ( 1.351706036745407680, 0.05413385826771666132, 0.4176697321401328100 ) ) ;
#70759 = CARTESIAN_POINT ( 'NONE',  ( -0.3917322834645670104, -7.196005306013484475E-17, -2.551181102362204633 ) ) ;
#70760 = B_SPLINE_CURVE_WITH_KNOTS ( 'NONE', 3,
 ( #14843, #66599, #27872, #41336, #47634, #73328, #16505, #35847, #54361, #80073, #61096, #22390, #15258, #15675, #10182, #28699, #67426, #35020, #55182, #40503, #61516, #80484, #22797, #3861, #59852, #60275, #67016, #79240 ),
 .UNSPECIFIED., .F., .F.,
 ( 4, 2, 2, 2, 2, 2, 2, 2, 2, 2, 2, 2, 2, 4 ),
 ( 0.01906920098334001501, 0.02026021391800203117, 0.02145122685266404733, 0.02264223978732606696, 0.02383325272198808312, 0.02621527859131211544, 0.02740629152597413160, 0.02859730446063614429, 0.03097933032996016273, 0.03217034326462216154, 0.03336135619928416729, 0.03574338206860819267, 0.03693439500327019842, 0.03812540793793221111 ),
 .UNSPECIFIED. ) ;
#70762 = CIRCLE ( 'NONE', #72097, 1.122047244094488194 ) ;
#70761 = CARTESIAN_POINT ( 'NONE',  ( -1.601049868766403650, 0.2306618581243847221, -0.2411417322834647770 ) ) ;
#70763 = CARTESIAN_POINT ( 'NONE',  ( -0.9055118110236215490, 0.2952755905511811885, 0.000000000000000000 ) ) ;
#70764 = CARTESIAN_POINT ( 'NONE',  ( 0.1265901696524989462, 0.4724409448818897572, -0.9383202099737533164 ) ) ;
#70765 = CARTESIAN_POINT ( 'NONE',  ( 0.3996062992125986035, 0.1070741851644054776, -0.1246719160104987068 ) ) ;
#70766 = ORIENTED_EDGE ( 'NONE', *, *, #49461, .T. ) ;
#70767 = CARTESIAN_POINT ( 'NONE',  ( 0.1049868766404206816, 0.1283753931104748280, 0.1820866141732283561 ) ) ;
#70768 = CARTESIAN_POINT ( 'NONE',  ( -0.3917322834645669549, -0.1049643490035306603, -1.770341207349081181 ) ) ;
#70769 = ORIENTED_EDGE ( 'NONE', *, *, #41785, .T. ) ;
#70770 = CARTESIAN_POINT ( 'NONE',  ( 0.1640419947506569498, -0.05778040916215522460, 0.4822834645669289988 ) ) ;
#70771 = CARTESIAN_POINT ( 'NONE',  ( 0.4658792650918640033, -0.3162353388693405765, 0.4822834645669290543 ) ) ;
#70772 = CARTESIAN_POINT ( 'NONE',  ( 0.4091458600556403535, 0.2362204724409449896, -2.808398950131233640 ) ) ;
#70773 = DIRECTION ( 'NONE',  ( -1.000000000000000000, -3.469446951953613696E-16, 0.000000000000000000 ) ) ;
#70774 = CARTESIAN_POINT ( 'NONE',  ( -0.5314960629921250401, 0.07958543189024085140, 0.2665933059059887866 ) ) ;
#70775 = CARTESIAN_POINT ( 'NONE',  ( -0.2319625946588664833, -0.1829408352246090774, 0.1465682319128800981 ) ) ;
#70776 = CARTESIAN_POINT ( 'NONE',  ( 0.7939632545931766261, -0.3162353388693409650, -0.4822834645669289433 ) ) ;
#70777 = CARTESIAN_POINT ( 'NONE',  ( 0.9251968503937015864, -0.4536011799217367080, 0.2665933059059888421 ) ) ;
#70778 = CARTESIAN_POINT ( 'NONE',  ( -0.5839895013123351797, -0.6692913385826771977, 0.1292274648535927661 ) ) ;
#70779 = CARTESIAN_POINT ( 'NONE',  ( 0.3392501089628018329, -0.1958661417322834497, -1.129901944060680563 ) ) ;
#70780 = CARTESIAN_POINT ( 'NONE',  ( -0.8070866141732276899, 0.1660481256975883668, -0.3530559997133364547 ) ) ;
#70781 = CARTESIAN_POINT ( 'NONE',  ( -1.391076115485563758, 0.1283753931104748280, 0.1820866141732283561 ) ) ;
#70782 = CARTESIAN_POINT ( 'NONE',  ( -0.7939632545931754048, -0.3162353388693405765, 0.4822834645669290543 ) ) ;
#70783 = CARTESIAN_POINT ( 'NONE',  ( 1.686351706036745890, 0.2952755905511811885, 0.1292274648535926551 ) ) ;
#70784 = CARTESIAN_POINT ( 'NONE',  ( -0.4567483893478792578, 1.408297760469687798, -2.131068205843717145 ) ) ;
#70785 = EDGE_LOOP ( 'NONE', ( #7424, #14590, #25903, #13864 ) ) ;
#70786 = CARTESIAN_POINT ( 'NONE',  ( -0.3392501089628019995, 0.1958661417322831999, -2.542670234417010011 ) ) ;
#70787 = CARTESIAN_POINT ( 'NONE',  ( 0.1443569553805781891, 0.05413385826771626580, -0.4176697321401330321 ) ) ;
#70788 = ORIENTED_EDGE ( 'NONE', *, *, #68011, .F. ) ;
#70789 = CARTESIAN_POINT ( 'NONE',  ( -0.7283464566929126471, 0.1660481256975883668, -0.3530559997133364547 ) ) ;
#70790 = CARTESIAN_POINT ( 'NONE',  ( 1.266404199475066328, -0.05778040916215522460, 0.4822834645669289988 ) ) ;
#70791 = CARTESIAN_POINT ( 'NONE',  ( 1.266404199475066328, -0.05778040916215522460, 0.4822834645669289988 ) ) ;
#70792 = CARTESIAN_POINT ( 'NONE',  ( 0.6430446194225728496, 0.05413385826771666132, 0.4176697321401328100 ) ) ;
#70793 = CARTESIAN_POINT ( 'NONE',  ( 0.2427821522309719648, -0.05778040916215522460, 0.4822834645669289988 ) ) ;
#70794 = CARTESIAN_POINT ( 'NONE',  ( 0.1049643490035303689, 0.3917322834645670104, -1.495406824146981117 ) ) ;
#70795 = CARTESIAN_POINT ( 'NONE',  ( -1.115485564304461219, -0.4281496062992124485, 0.4176697321401328655 ) ) ;
#70796 = CARTESIAN_POINT ( 'NONE',  ( -0.2165354330708654795, 0.1660481256975885056, 0.3530559997133364547 ) ) ;
#70797 = CARTESIAN_POINT ( 'NONE',  ( -0.1574803149606292529, -0.1870078740157480601, -0.3641732283464567677 ) ) ;
#70798 = CARTESIAN_POINT ( 'NONE',  ( -0.2945512653497797673, -0.02373080790438483051, 5.526002588227517442 ) ) ;
#70799 = CARTESIAN_POINT ( 'NONE',  ( 0.03280839895013198948, 0.2952755905511811885, 0.1292274648535926551 ) ) ;
#70800 = CARTESIAN_POINT ( 'NONE',  ( -0.5314960629921396951, 2.697992270790283698, 3.898836503597931991 ) ) ;
#70801 = CARTESIAN_POINT ( 'NONE',  ( 0.9711286089238851948, 0.2306618581243848609, 0.2411417322834645549 ) ) ;
#70802 = DIRECTION ( 'NONE',  ( 0.000000000000000000, -0.000000000000000000, -1.000000000000000000 ) ) ;
#70803 = ORIENTED_EDGE ( 'NONE', *, *, #24986, .F. ) ;
#70804 = VERTEX_POINT ( 'NONE', #39897 ) ;
#70805 = AXIS2_PLACEMENT_3D ( 'NONE', #36352, #41833, #42660 ) ;
#70806 = CARTESIAN_POINT ( 'NONE',  ( 0.4593175853018380828, 0.05413385826771626580, -0.4176697321401330321 ) ) ;
#70807 = CARTESIAN_POINT ( 'NONE',  ( -0.1968503937007867743, -0.5511811023622047445, 6.969142054262312111E-17 ) ) ;
#70808 = VECTOR ( 'NONE', #54740, 39.37007874015748854 ) ;
#70809 = AXIS2_PLACEMENT_3D ( 'NONE', #50676, #51080, #31740 ) ;
#70811 = CARTESIAN_POINT ( 'NONE',  ( -0.06632061457837669372, -2.294479370626195693E-15, 0.3464511005275217603 ) ) ;
#70810 = CARTESIAN_POINT ( 'NONE',  ( 1.522309711286089939, 0.1283753931104748280, 0.1820866141732283561 ) ) ;
#70812 = CARTESIAN_POINT ( 'NONE',  ( 0.4724409448818898682, 2.892866454678787531E-17, -0.03740157480314962313 ) ) ;
#70813 = CARTESIAN_POINT ( 'NONE',  ( 1.601049868766404982, -0.5023911411419708095, -0.1820866141732282451 ) ) ;
#70814 = EDGE_CURVE ( 'NONE', #48318, #77301, #82826, .T. ) ;
#70815 = CARTESIAN_POINT ( 'NONE',  ( -1.496062992125983815, -0.1870078740157479769, 0.4822834645669291653 ) ) ;
#70816 = CARTESIAN_POINT ( 'NONE',  ( 0.3460692066303959202, -0.1998031496062991630, -2.701443569553806157 ) ) ;
#70817 = PRODUCT ( 'Chuck Key Tool', 'Chuck Key Tool', '', ( #46889 ) ) ;
#70818 = CARTESIAN_POINT ( 'NONE',  ( -0.09186351706036689768, 0.05413385826771626580, -0.4176697321401330321 ) ) ;
#70819 = CARTESIAN_POINT ( 'NONE',  ( -1.069553805774277722, -0.6692913385826773087, -0.1292274648535924053 ) ) ;
#70820 = CARTESIAN_POINT ( 'NONE',  ( -1.541994750656167090, 0.2952755905511811885, 0.1292274648535926551 ) ) ;
#70821 = CARTESIAN_POINT ( 'NONE',  ( 0.2755905511811031494, -0.6692913385826771977, 8.415575281601705876E-17 ) ) ;
#70822 = EDGE_CURVE ( 'NONE', #79813, #65941, #45768, .T. ) ;
#70823 = CARTESIAN_POINT ( 'NONE',  ( -0.3949938075777411073, 0.1058382717557497660, -0.2670603674540682482 ) ) ;
#70824 = CARTESIAN_POINT ( 'NONE',  ( 1.568241469816273659, -0.05778040916215560624, -0.4822834645669293319 ) ) ;
#70825 = CARTESIAN_POINT ( 'NONE',  ( 0.9514435695538062676, -0.05778040916215522460, 0.4822834645669289988 ) ) ;
#70826 = CARTESIAN_POINT ( 'NONE',  ( 1.141732283464567788, -0.5511811023622047445, 6.969142054262312111E-17 ) ) ;
#70827 = CARTESIAN_POINT ( 'NONE',  ( 0.2941356937468260768, 1.187227223647445484, 0.1081275479939705769 ) ) ;
#70828 = CARTESIAN_POINT ( 'NONE',  ( 0.8792650918635177559, -0.004921259842519576551, 0.3153832671262227771 ) ) ;
#70829 = CARTESIAN_POINT ( 'NONE',  ( -1.345144356955379816, -0.3162353388693405765, 0.4822834645669290543 ) ) ;
#70830 = CARTESIAN_POINT ( 'NONE',  ( 0.2925321140481932369, -0.2925321140481931814, -0.8051181102362205966 ) ) ;
#70831 = CARTESIAN_POINT ( 'NONE',  ( 1.010498687664042716, -0.4281496062992124485, 0.4176697321401328655 ) ) ;
#70832 = CARTESIAN_POINT ( 'NONE',  ( 0.2867679344610365999, -0.2867679344610365444, -0.5629921259842519676 ) ) ;
#70834 = CARTESIAN_POINT ( 'NONE',  ( -0.4122368018044647031, 1.300920202588027541, 2.057881464606095889 ) ) ;
#70833 = CARTESIAN_POINT ( 'NONE',  ( 0.5249343832021005074, -0.6046776061558807314, 0.2411417322834647770 ) ) ;
#70835 = CARTESIAN_POINT ( 'NONE',  ( -1.692913385826770645, 0.1771653543307087630, 0.000000000000000000 ) ) ;
#70836 = CARTESIAN_POINT ( 'NONE',  ( 0.5643044619422579178, -0.3690944881889765550, -0.3153832671262227771 ) ) ;
#70837 = CARTESIAN_POINT ( 'NONE',  ( 0.6167979002624679463, 0.05413385826771626580, -0.4176697321401330321 ) ) ;
#70838 = CARTESIAN_POINT ( 'NONE',  ( 1.614173228346457378, -0.5511811023622047445, 6.969142054262312111E-17 ) ) ;
#70839 = CARTESIAN_POINT ( 'NONE',  ( -0.7283464566929126471, 0.07958543189024071263, -0.2665933059059888421 ) ) ;
#70840 = CARTESIAN_POINT ( 'NONE',  ( -0.4265091863517051496, 0.2952755905511810774, -0.1292274648535930714 ) ) ;
#70841 = CARTESIAN_POINT ( 'NONE',  ( -1.633858267716534529, 0.07958543189024085140, 0.2665933059059887866 ) ) ;
#70842 = CARTESIAN_POINT ( 'NONE',  ( -0.9973753280839886548, -0.6046776061558809534, -0.2411417322834644161 ) ) ;
#70843 = CARTESIAN_POINT ( 'NONE',  ( 0.8530183727034128527, -0.4281496062992124485, 0.4176697321401328655 ) ) ;
#70844 = CARTESIAN_POINT ( 'NONE',  ( -1.423884514435694859, -0.08942795157528024563, -0.3641732283464568787 ) ) ;
#70845 = DIRECTION ( 'NONE',  ( 1.000000000000000000, -0.000000000000000000, -0.000000000000000000 ) ) ;
#70846 = CARTESIAN_POINT ( 'NONE',  ( 0.9580052493438326877, 0.05413385826771666132, 0.4176697321401328100 ) ) ;
#70847 = CARTESIAN_POINT ( 'NONE',  ( -0.4724409448818895907, -0.1265901696524993070, -2.642388451443570041 ) ) ;
#70848 = CARTESIAN_POINT ( 'NONE',  ( -1.692913385826770645, 0.2952755905511811885, 0.000000000000000000 ) ) ;
#70849 = CARTESIAN_POINT ( 'NONE',  ( 1.240157480314961314, 0.1660481256975883668, -0.3530559997133364547 ) ) ;
#70850 = CARTESIAN_POINT ( 'NONE',  ( -1.082677165354329896, 0.07958543189024085140, 0.2665933059059887866 ) ) ;
#70851 = DIRECTION ( 'NONE',  ( 1.000000000000000000, 0.000000000000000000, 0.000000000000000000 ) ) ;
#70852 = CARTESIAN_POINT ( 'NONE',  ( -0.2755905511811015396, -0.6692913385826771977, 8.415575281601705876E-17 ) ) ;
#70853 = CARTESIAN_POINT ( 'NONE',  ( -0.4068241469816264999, -0.3690944881889763329, 0.3153832671262228327 ) ) ;
#70854 = CARTESIAN_POINT ( 'NONE',  ( -1.653543307086613234, -0.1870078740157480601, -0.3641732283464567677 ) ) ;
#70855 = CARTESIAN_POINT ( 'NONE',  ( 0.8858267716535438430, -0.4536011799217368745, -0.2665933059059886201 ) ) ;
#70856 = CARTESIAN_POINT ( 'NONE',  ( 0.6233595800524942554, -0.05778040916215560624, -0.4822834645669293319 ) ) ;
#70857 = CARTESIAN_POINT ( 'NONE',  ( 1.430446194225722500, 0.05413385826771666132, 0.4176697321401328100 ) ) ;
#70858 = CARTESIAN_POINT ( 'NONE',  ( 0.3215223097112867578, -0.3162353388693409650, -0.4822834645669289433 ) ) ;
#70859 = CARTESIAN_POINT ( 'NONE',  ( 0.3740157480314966754, 0.07958543189024071263, -0.2665933059059888421 ) ) ;
#70861 = CARTESIAN_POINT ( 'NONE',  ( -1.555118110236219930, -0.5400638737290845981, -0.3530559997133363437 ) ) ;
#70860 = AXIS2_PLACEMENT_3D ( 'NONE', #70345, #65307, #26575 ) ;
#70862 = CARTESIAN_POINT ( 'NONE',  ( -1.371391076115484609, -0.6692913385826771977, 0.1292274648535927661 ) ) ;
#70863 = CARTESIAN_POINT ( 'NONE',  ( -0.6430446194225716283, -0.4281496062992124485, 0.4176697321401328655 ) ) ;
#70864 = VECTOR ( 'NONE', #82027, 39.37007874015748143 ) ;
#70865 = CARTESIAN_POINT ( 'NONE',  ( 0.2925321140481932369, -0.2925321140481931814, -0.4133858267716534196 ) ) ;
#70866 = CARTESIAN_POINT ( 'NONE',  ( 0.3996062992125985480, 2.446882876249141654E-17, -2.872047244094488416 ) ) ;
#70867 = CARTESIAN_POINT ( 'NONE',  ( -0.07217847769028813698, -0.3162353388693409650, -0.4822834645669289433 ) ) ;
#70868 = CARTESIAN_POINT ( 'NONE',  ( 1.279527559055118724, 0.07958543189024085140, 0.2665933059059887866 ) ) ;
#70869 = VECTOR ( 'NONE', #59831, 39.37007874015748143 ) ;
#70870 = CARTESIAN_POINT ( 'NONE',  ( -0.6036745406824141069, -0.6046776061558809534, -0.2411417322834644161 ) ) ;
#70871 = CARTESIAN_POINT ( 'NONE',  ( 0.4855643044619428750, 0.05413385826771666132, 0.4176697321401328100 ) ) ;
#70872 = CARTESIAN_POINT ( 'NONE',  ( -0.2925321140481932924, 0.2925321140481931814, -2.381889763779527325 ) ) ;
#70873 = CARTESIAN_POINT ( 'NONE',  ( -0.2891555358219911054, 0.2891555358219909388, -1.909448818897637956 ) ) ;
#70874 = CARTESIAN_POINT ( 'NONE',  ( -0.2867679344610364334, -0.2867679344610367109, -0.3661417322834645827 ) ) ;
#70875 = CARTESIAN_POINT ( 'NONE',  ( -3.924389226575468737, 2.755905511811024056, 0.3149606299212597271 ) ) ;
#70876 = CARTESIAN_POINT ( 'NONE',  ( 0.3917322834645670104, -0.1049643490035303273, -1.048556430446194287 ) ) ;
#70877 = CARTESIAN_POINT ( 'NONE',  ( -0.9251968503937002541, 0.07958543189024085140, 0.2665933059059887866 ) ) ;
#70878 = CARTESIAN_POINT ( 'NONE',  ( -1.043307086614172707, 0.1660481256975883668, -0.3530559997133364547 ) ) ;
#70879 = CARTESIAN_POINT ( 'NONE',  ( -0.1049643490035306742, 0.3917322834645668994, 0.2283657724747524265 ) ) ;
#70880 = CARTESIAN_POINT ( 'NONE',  ( 0.2559055118110243332, 0.1660481256975885056, 0.3530559997133364547 ) ) ;
#70881 = CARTESIAN_POINT ( 'NONE',  ( 1.253280839895013710, -0.3162353388693405765, 0.4822834645669290543 ) ) ;
#70882 = CARTESIAN_POINT ( 'NONE',  ( 0.9251968503937015864, -0.5400638737290844871, 0.3530559997133364547 ) ) ;
#70883 = CARTESIAN_POINT ( 'NONE',  ( -0.2362204724409447953, -0.4091458600556404646, -2.742782152230971437 ) ) ;
#70884 = CARTESIAN_POINT ( 'NONE',  ( 0.3996062992125986035, 0.1070741851644054776, -2.644356955380577912 ) ) ;
#70885 = CARTESIAN_POINT ( 'NONE',  ( -0.1049643490035302301, -0.3917322834645671770, -1.328759473262154378 ) ) ;
#70886 = CARTESIAN_POINT ( 'NONE',  ( 1.640419947506562393, -0.4281496062992124485, 0.4176697321401328655 ) ) ;
#70887 = CARTESIAN_POINT ( 'NONE',  ( 0.4658792650918640033, -0.3162353388693405765, 0.4822834645669290543 ) ) ;
#70888 = CARTESIAN_POINT ( 'NONE',  ( 0.3674540682414705883, 0.2306618581243847221, -0.2411417322834647770 ) ) ;
#70889 = CARTESIAN_POINT ( 'NONE',  ( 0.6496062992125991586, 0.07958543189024085140, 0.2665933059059887866 ) ) ;
#70890 = CARTESIAN_POINT ( 'NONE',  ( 1.430446194225722500, -0.4281496062992127816, -0.4176697321401328100 ) ) ;
#70891 = CARTESIAN_POINT ( 'NONE',  ( -9.594673741351313045E-17, 0.3917322834645670104, 0.07283464566929125084 ) ) ;
#70892 = CARTESIAN_POINT ( 'NONE',  ( 0.4265091863517067039, -0.6692913385826773087, -0.1292274648535924053 ) ) ;
#70893 = CARTESIAN_POINT ( 'NONE',  ( 1.036745406824147731, 0.05413385826771666132, 0.4176697321401328100 ) ) ;
#70894 = CARTESIAN_POINT ( 'NONE',  ( 0.4330708661417329575, 0.2952755905511811885, 0.000000000000000000 ) ) ;
#70895 = CARTESIAN_POINT ( 'NONE',  ( 1.148293963254593875, -0.5511811023622046335, 0.09757992244046803654 ) ) ;
#70896 = CARTESIAN_POINT ( 'NONE',  ( -1.049868766404198794, 0.2306618581243847221, -0.2411417322834647770 ) ) ;
#70897 = CARTESIAN_POINT ( 'NONE',  ( -1.056430446194224881, 0.2952755905511810774, -0.1292274648535930714 ) ) ;
#70898 = CARTESIAN_POINT ( 'NONE',  ( 1.286089238845145033, 0.2306618581243848609, 0.2411417322834645549 ) ) ;
#70899 = CARTESIAN_POINT ( 'NONE',  ( -0.1958661417322834220, -0.3392501089628018884, -0.7801837270341208663 ) ) ;
#70900 = CARTESIAN_POINT ( 'NONE',  ( -0.3917322834645670104, -7.196005306013484475E-17, -2.078740157480314821 ) ) ;
#70901 = CARTESIAN_POINT ( 'NONE',  ( 0.3392501089628018884, -0.1958661417322834220, -2.616797900262466836 ) ) ;
#70902 = ORIENTED_EDGE ( 'NONE', *, *, #9160, .T. ) ;
#70903 = CARTESIAN_POINT ( 'NONE',  ( 0.2925321140481932369, -0.2925321140481932369, 0.05905511811023619884 ) ) ;
#70904 = ORIENTED_EDGE ( 'NONE', *, *, #4484, .F. ) ;
#70905 = CARTESIAN_POINT ( 'NONE',  ( 0.8595800524934390507, -0.08942795157528024563, -0.3641732283464568787 ) ) ;
#70906 = CARTESIAN_POINT ( 'NONE',  ( 0.2925321140481932369, -0.2925321140481932369, -1.515748031496062742 ) ) ;
#70907 = CARTESIAN_POINT ( 'NONE',  ( 1.181102362204725198, -0.1870078740157479769, 0.3641732283464567677 ) ) ;
#70908 = CARTESIAN_POINT ( 'NONE',  ( 0.4531182788721080934, 1.535433070866141447, -0.5309055118110237448 ) ) ;
#70909 = CARTESIAN_POINT ( 'NONE',  ( 0.000000000000000000, 0.000000000000000000, -0.4921259842519685179 ) ) ;
#70910 = DIRECTION ( 'NONE',  ( -1.000000000000000000, -0.000000000000000000, -0.000000000000000000 ) ) ;
#70911 = CARTESIAN_POINT ( 'NONE',  ( 0.3917322834645670104, 2.398668435337828261E-17, -0.6751968503937009203 ) ) ;
#70912 = EDGE_CURVE ( 'NONE', #53271, #29384, #72716, .T. ) ;
#70913 = CARTESIAN_POINT ( 'NONE',  ( -1.194225721784776262, -0.3690944881889763329, 0.3153832671262228327 ) ) ;
#70914 = CARTESIAN_POINT ( 'NONE',  ( -1.699475065616797398, 0.1771653543307087630, 0.09757992244046791164 ) ) ;
#70915 = CARTESIAN_POINT ( 'NONE',  ( -1.233595800524933894, -0.6046776061558809534, -0.2411417322834644161 ) ) ;
#70916 = CARTESIAN_POINT ( 'NONE',  ( 0.2755905511811031494, -0.6692913385826771977, 8.415575281601705876E-17 ) ) ;
#70917 = CARTESIAN_POINT ( 'NONE',  ( 1.364829396325459854, -0.6046776061558809534, -0.2411417322834644161 ) ) ;
#70918 = ORIENTED_EDGE ( 'NONE', *, *, #1240, .T. ) ;
#70919 = CARTESIAN_POINT ( 'NONE',  ( -1.044296345234789758, 1.299058944788251901, -0.4104848940941682733 ) ) ;
#70920 = DIRECTION ( 'NONE',  ( -0.04893523608364114263, 0.000000000000000000, -0.9988019536772235751 ) ) ;
#70921 = CARTESIAN_POINT ( 'NONE',  ( 0.4724409448818897572, -0.1265901696524988906, -2.001312335958005395 ) ) ;
#70922 = CARTESIAN_POINT ( 'NONE',  ( 0.000000000000000000, 0.000000000000000000, -0.3937007874015748254 ) ) ;
#70923 = CARTESIAN_POINT ( 'NONE',  ( -1.614173228346456712, 2.401574803149606474, -0.1372047244094478091 ) ) ;
#70924 = CARTESIAN_POINT ( 'NONE',  ( -0.8989501312335946848, -0.5511811023622046335, 0.09757992244046803654 ) ) ;
#70925 = CARTESIAN_POINT ( 'NONE',  ( 0.4724409448818898682, 0.000000000000000000, -2.755905511811024056 ) ) ;
#70926 = CARTESIAN_POINT ( 'NONE',  ( 0.7677165354330716118, 0.1660481256975883668, -0.3530559997133364547 ) ) ;
#70927 = CIRCLE ( 'NONE', #49409, 1.122047244094488194 ) ;
#70928 = VERTEX_POINT ( 'NONE', #14238 ) ;
#70930 = CARTESIAN_POINT ( 'NONE',  ( 0.000000000000000000, 2.165354330708661568, 0.000000000000000000 ) ) ;
#70929 = CARTESIAN_POINT ( 'NONE',  ( -0.1265901696524986964, -0.4724409448818899238, -2.511154855643044748 ) ) ;
#70931 = CARTESIAN_POINT ( 'NONE',  ( 1.049868766404200349, 0.2306618581243848609, 0.2411417322834645549 ) ) ;
#70932 = CARTESIAN_POINT ( 'NONE',  ( 1.535433070866142335, -0.5511811023622047445, 6.969142054262312111E-17 ) ) ;
#70933 = CARTESIAN_POINT ( 'NONE',  ( 0.3917322834645669549, 2.398668435337827645E-17, -0.8280646737194732321 ) ) ;
#70934 = CARTESIAN_POINT ( 'NONE',  ( -0.5446194225721777693, -0.2845877964562161244, -0.3641732283464567121 ) ) ;
#70935 = CARTESIAN_POINT ( 'NONE',  ( -1.286089238845143479, 0.1283753931104746893, -0.1820866141732285504 ) ) ;
#70936 = CARTESIAN_POINT ( 'NONE',  ( -0.4359958488159647039, 1.724409448818897905, -2.094141031014960408 ) ) ;
#70937 = CARTESIAN_POINT ( 'NONE',  ( -0.3543307086614165824, 0.1771653543307087630, 0.000000000000000000 ) ) ;
#70938 = CARTESIAN_POINT ( 'NONE',  ( 0.2821522309711292364, -0.5511811023622046335, 0.09757992244046803654 ) ) ;
#70939 = CARTESIAN_POINT ( 'NONE',  ( -0.03937007874015669567, -0.6692913385826771977, 8.415575281601705876E-17 ) ) ;
#70940 = CARTESIAN_POINT ( 'NONE',  ( -1.115485564304461219, -0.004921259842519870586, -0.3153832671262229437 ) ) ;
#70941 = CARTESIAN_POINT ( 'NONE',  ( 0.2867679344610365999, -0.2867679344610365444, -2.610236220472441193 ) ) ;
#70942 = CARTESIAN_POINT ( 'NONE',  ( 1.010498687664042716, 0.05413385826771626580, -0.4176697321401330321 ) ) ;
#70943 = CARTESIAN_POINT ( 'NONE',  ( -1.601049868766403650, 0.2306618581243847221, -0.2411417322834647770 ) ) ;
#70944 = CARTESIAN_POINT ( 'NONE',  ( 0.4724409448818898682, 2.892866454678787531E-17, -1.297244094488188670 ) ) ;
#70945 = CARTESIAN_POINT ( 'NONE',  ( -0.4396325459317579898, 0.2952755905511811885, 0.1292274648535926551 ) ) ;
#70946 = CARTESIAN_POINT ( 'NONE',  ( -1.030183727034119867, -0.3162353388693405765, 0.4822834645669290543 ) ) ;
#70947 = CARTESIAN_POINT ( 'NONE',  ( 0.9186351706036752773, 0.1283753931104746893, -0.1820866141732285504 ) ) ;
#70948 = CARTESIAN_POINT ( 'NONE',  ( -0.2887139107611542133, 0.1283753931104748280, 0.1820866141732283561 ) ) ;
#70949 = CARTESIAN_POINT ( 'NONE',  ( -0.7742782152230965886, 0.05413385826771666132, 0.4176697321401328100 ) ) ;
#70950 = CARTESIAN_POINT ( 'NONE',  ( -1.417322834645668772, -0.1870078740157480879, -0.4822834645669291653 ) ) ;
#70951 = FACE_OUTER_BOUND ( 'NONE', #60463, .T. ) ;
#70952 = CARTESIAN_POINT ( 'NONE',  ( 1.246719160104987623, -0.004921259842519870586, -0.3153832671262229437 ) ) ;
#70953 = CARTESIAN_POINT ( 'NONE',  ( -1.450131233595799651, 0.2952755905511810774, -0.1292274648535930714 ) ) ;
#70954 = CARTESIAN_POINT ( 'NONE',  ( -1.377952755905511140, 0.2952755905511811885, 0.000000000000000000 ) ) ;
#70955 = ORIENTED_EDGE ( 'NONE', *, *, #43993, .F. ) ;
#70956 = CARTESIAN_POINT ( 'NONE',  ( 0.1070741851644053388, 0.3996062992125986035, -2.432414698162729039 ) ) ;
#70957 = CARTESIAN_POINT ( 'NONE',  ( -0.7349081364829387342, -0.5023911411419708095, 0.1820866141732285504 ) ) ;
#70958 = CARTESIAN_POINT ( 'NONE',  ( 0.6364829396325465405, -0.05778040916215522460, 0.4822834645669289988 ) ) ;
#70959 = CARTESIAN_POINT ( 'NONE',  ( -1.148293963254592542, -0.5511811023622048555, -0.09757992244046775898 ) ) ;
#70960 = CARTESIAN_POINT ( 'NONE',  ( -0.3460692066303957537, -0.1998031496062994405, -1.389107611548556553 ) ) ;
#70961 = CARTESIAN_POINT ( 'NONE',  ( -1.122047244094487306, -0.5400638737290844871, 0.3530559997133364547 ) ) ;
#70962 = CARTESIAN_POINT ( 'NONE',  ( 0.6758530183727039509, -0.6692913385826771977, 0.1292274648535927661 ) ) ;
#70963 = CARTESIAN_POINT ( 'NONE',  ( 0.4921259842519691285, -0.5400638737290845981, -0.3530559997133363437 ) ) ;
#70964 = CARTESIAN_POINT ( 'NONE',  ( 0.000000000000000000, 0.000000000000000000, 0.1968503937007874405 ) ) ;
#70965 = CARTESIAN_POINT ( 'NONE',  ( -1.318897637795274802, -0.4536011799217368745, -0.2665933059059886201 ) ) ;
#70966 = CARTESIAN_POINT ( 'NONE',  ( 4.893765752498283308E-17, -0.3996062992125985480, -0.4704724409448819422 ) ) ;
#70967 = CARTESIAN_POINT ( 'NONE',  ( -9.787531504996567848E-17, 0.3996062992125986035, -0.9448818897637796255 ) ) ;
#70968 = CARTESIAN_POINT ( 'NONE',  ( 0.3949938075777409963, 2.418639510665530435E-17, -0.7480314960629920185 ) ) ;
#70969 = CARTESIAN_POINT ( 'NONE',  ( 2.795275590551181466, 2.793565526369266916, 0.000000000000000000 ) ) ;
#70970 = CARTESIAN_POINT ( 'NONE',  ( 1.377952755905512472, 0.1771653543307087630, 0.000000000000000000 ) ) ;
#70971 = CARTESIAN_POINT ( 'NONE',  ( 0.2624671916010504757, -0.5023911411419708095, -0.1820866141732282451 ) ) ;
#70972 = CARTESIAN_POINT ( 'NONE',  ( 0.2821522309711292364, -0.6692913385826771977, 0.1292274648535927661 ) ) ;
#70973 = CARTESIAN_POINT ( 'NONE',  ( 1.410761154855643795, -0.3162353388693405765, 0.4822834645669290543 ) ) ;
#70974 = CARTESIAN_POINT ( 'NONE',  ( -9.674558042662122972E-17, 0.3949938075777409963, -1.336614173228346081 ) ) ;
#70975 = CARTESIAN_POINT ( 'NONE',  ( 0.5511811023622055217, -0.1870078740157479769, 0.3641732283464567677 ) ) ;
#70976 = CARTESIAN_POINT ( 'NONE',  ( -0.6364829396325453192, -0.05778040916215560624, -0.4822834645669293319 ) ) ;
#70977 = CARTESIAN_POINT ( 'NONE',  ( -1.233595800524933894, -0.6046776061558809534, -0.2411417322834644161 ) ) ;
#70978 = CARTESIAN_POINT ( 'NONE',  ( 0.8530183727034128527, -0.4281496062992124485, 0.4176697321401328655 ) ) ;
#70979 = CARTESIAN_POINT ( 'NONE',  ( -0.4724409448818899238, 0.1265901696524986686, -1.450131233595800317 ) ) ;
#70980 = VECTOR ( 'NONE', #2127, 39.37007874015748143 ) ;
#70981 = CARTESIAN_POINT ( 'NONE',  ( -0.7217847769028863381, 0.05413385826771626580, -0.4176697321401330321 ) ) ;
#70982 = ORIENTED_EDGE ( 'NONE', *, *, #32702, .T. ) ;
#70983 = ORIENTED_EDGE ( 'NONE', *, *, #51624, .F. ) ;
#70984 = CARTESIAN_POINT ( 'NONE',  ( -1.141732283464566011, -0.6692913385826771977, 8.415575281601705876E-17 ) ) ;
#70985 = CARTESIAN_POINT ( 'NONE',  ( -0.5446194225721777693, -0.05778040916215522460, 0.4822834645669289988 ) ) ;
#70987 = CARTESIAN_POINT ( 'NONE',  ( -0.9055118110236215490, -0.6692913385826771977, 8.415575281601705876E-17 ) ) ;
#70986 = CARTESIAN_POINT ( 'NONE',  ( -0.7217847769028863381, -0.3690944881889763329, 0.3153832671262228327 ) ) ;
#70988 = CARTESIAN_POINT ( 'NONE',  ( 0.1958661417322834497, 0.3392501089628018329, -1.799193282643357428 ) ) ;
#70989 = CARTESIAN_POINT ( 'NONE',  ( -0.4617417521217842546, -1.429000049448402363E-15, 0.4118477457933010233 ) ) ;
#70990 = CARTESIAN_POINT ( 'NONE',  ( -1.528871391076114250, -0.5511811023622046335, 0.09757992244046803654 ) ) ;
#70991 = CARTESIAN_POINT ( 'NONE',  ( -1.292650918635170010, -0.6692913385826771977, 0.1292274648535927661 ) ) ;
#70992 = CARTESIAN_POINT ( 'NONE',  ( 0.1902887139107617975, 0.2952755905511811885, 0.1292274648535926551 ) ) ;
#70993 = CARTESIAN_POINT ( 'NONE',  ( -0.7020997375328074108, -0.05778040916215522460, 0.4822834645669289988 ) ) ;
#70994 = EDGE_CURVE ( 'NONE', #51375, #73460, #30360, .T. ) ;
#70995 = CARTESIAN_POINT ( 'NONE',  ( -0.2867679344610365999, 0.2867679344610364889, -1.271653543307086798 ) ) ;
#70996 = CARTESIAN_POINT ( 'NONE',  ( -1.017060367454067249, -0.08942795157527998196, 0.3641732283464567121 ) ) ;
#70997 = ORIENTED_EDGE ( 'NONE', *, *, #28086, .F. ) ;
#70998 = CARTESIAN_POINT ( 'NONE',  ( -0.3949938075777411628, 0.1058382717557497937, -2.080052493438320216 ) ) ;
#70999 = EDGE_LOOP ( 'NONE', ( #29272, #52102, #76811, #57831 ) ) ;
#71000 = DIRECTION ( 'NONE',  ( -1.000000000000000000, -0.000000000000000000, -0.000000000000000000 ) ) ;
#71001 = CARTESIAN_POINT ( 'NONE',  ( -1.286089238845143479, -0.6046776061558807314, 0.2411417322834647770 ) ) ;
#71002 = CARTESIAN_POINT ( 'NONE',  ( -1.266404199475064773, -0.05778040916215560624, -0.4822834645669293319 ) ) ;
#71003 = CARTESIAN_POINT ( 'NONE',  ( -0.2925321140481932924, 0.2925321140481931814, -0.3346456692913385988 ) ) ;
#71004 = CARTESIAN_POINT ( 'NONE',  ( -1.122047244094487306, -0.5400638737290844871, 0.3530559997133364547 ) ) ;
#71005 = CARTESIAN_POINT ( 'NONE',  ( -1.102362204724408601, -0.1870078740157479769, 0.4822834645669291653 ) ) ;
#71006 = CARTESIAN_POINT ( 'NONE',  ( -0.3822046412494086165, -4.992347309556208597E-15, 0.3791483426435189319 ) ) ;
#71007 = CARTESIAN_POINT ( 'NONE',  ( -0.1049643490035307020, 0.3917322834645669549, 0.2237532808398949025 ) ) ;
#71008 = CARTESIAN_POINT ( 'NONE',  ( -0.09842519685039295696, -0.4536011799217367080, 0.2665933059059888421 ) ) ;
#71009 = CARTESIAN_POINT ( 'NONE',  ( 0.4603267246303430760, 1.653225543546893439, 2.138346301250358739 ) ) ;
#71010 = CARTESIAN_POINT ( 'NONE',  ( -0.3917322834645671215, 0.1049643490035301469, -0.2749343832020998413 ) ) ;
#71011 = CARTESIAN_POINT ( 'NONE',  ( -0.1837270341207343505, -0.5023911411419708095, 0.1820866141732285504 ) ) ;
#71012 = CARTESIAN_POINT ( 'NONE',  ( -0.7677165354330699465, -0.5400638737290845981, -0.3530559997133363437 ) ) ;
#71013 = CARTESIAN_POINT ( 'NONE',  ( 1.246719160104987623, -0.4281496062992124485, 0.4176697321401328655 ) ) ;
#71014 = CARTESIAN_POINT ( 'NONE',  ( -0.6889763779527552368, 0.1660481256975885056, 0.3530559997133364547 ) ) ;
#71015 = ORIENTED_EDGE ( 'NONE', *, *, #17807, .F. ) ;
#71016 = ORIENTED_EDGE ( 'NONE', *, *, #14771, .T. ) ;
#71017 = CARTESIAN_POINT ( 'NONE',  ( 0.1998031496062992463, 0.3460692066303959202, -2.110892388451443225 ) ) ;
#71018 = CARTESIAN_POINT ( 'NONE',  ( -0.8005249343832011588, 0.05413385826771626580, -0.4176697321401330321 ) ) ;
#71019 = CARTESIAN_POINT ( 'NONE',  ( 1.233595800524935227, -0.6046776061558807314, 0.2411417322834647770 ) ) ;
#71020 = CARTESIAN_POINT ( 'NONE',  ( -1.279527559055116948, -0.4536011799217367080, 0.2665933059059888421 ) ) ;
#71021 = CARTESIAN_POINT ( 'NONE',  ( -1.469816272965878357, -0.6046776061558809534, -0.2411417322834644161 ) ) ;
#71022 = CARTESIAN_POINT ( 'NONE',  ( -0.1265901696524986964, -0.4724409448818899238, -1.017060367454067915 ) ) ;
#71023 = CARTESIAN_POINT ( 'NONE',  ( -2.103512204792533868, 1.710976477253047801, 0.4417575354491484751 ) ) ;
#71024 = CARTESIAN_POINT ( 'NONE',  ( -0.1958661417322834220, -0.3392501089628018884, -0.2152230971128608339 ) ) ;
#71025 = CARTESIAN_POINT ( 'NONE',  ( 0.3917322834645670104, -0.04642319063763879206, -1.932137297949608978 ) ) ;
#71026 = CARTESIAN_POINT ( 'NONE',  ( 0.2296587926509192634, -0.3162353388693405765, 0.4822834645669290543 ) ) ;
#71027 = CARTESIAN_POINT ( 'NONE',  ( -1.443569553805773564, 0.1283753931104746893, -0.1820866141732285504 ) ) ;
#71028 = CARTESIAN_POINT ( 'NONE',  ( -0.5905511811023615998, 0.2952755905511811885, 0.000000000000000000 ) ) ;
#71029 = CARTESIAN_POINT ( 'NONE',  ( -1.157146581871515012E-16, 0.4724409448818898682, -2.753937007874015741 ) ) ;
#71031 = CARTESIAN_POINT ( 'NONE',  ( -0.5314960629921147151, 2.716535433070866645, -3.224202737261816942 ) ) ;
#71030 = CARTESIAN_POINT ( 'NONE',  ( -1.128608923884513837, -0.6046776061558807314, 0.2411417322834647770 ) ) ;
#71032 = CARTESIAN_POINT ( 'NONE',  ( -0.8202099737532801971, -0.6692913385826771977, 0.1292274648535927661 ) ) ;
#71033 = CARTESIAN_POINT ( 'NONE',  ( 0.1246719160104994284, -0.6692913385826771977, 0.1292274648535927661 ) ) ;
#71034 = CARTESIAN_POINT ( 'NONE',  ( -9.674558042662122972E-17, 0.3949938075777409963, -2.753937007874016185 ) ) ;
#71035 = CARTESIAN_POINT ( 'NONE',  ( 0.7020997375328090762, -0.08942795157528024563, -0.3641732283464568787 ) ) ;
#71036 = CARTESIAN_POINT ( 'NONE',  ( -0.7545931758530177724, 0.1771653543307087630, 0.09757992244046791164 ) ) ;
#71037 = CARTESIAN_POINT ( 'NONE',  ( -0.03443470937339819515, 1.064243487142144673, -1.633358474390059989 ) ) ;
#71038 = CARTESIAN_POINT ( 'NONE',  ( 0.7349081364829403995, 0.1283753931104748280, 0.1820866141732283561 ) ) ;
#71039 = CARTESIAN_POINT ( 'NONE',  ( 1.463254593175853824, 0.1771653543307087075, -0.09757992244046823083 ) ) ;
#71040 = CARTESIAN_POINT ( 'NONE',  ( 1.200787401574803681, -0.5400638737290845981, -0.3530559997133363437 ) ) ;
#71041 = CARTESIAN_POINT ( 'NONE',  ( 0.3083989501312343062, -0.08942795157528024563, -0.3641732283464568787 ) ) ;
#71042 = CARTESIAN_POINT ( 'NONE',  ( 4.797336870675656522E-17, -0.3917322834645670104, -1.488188976377952777 ) ) ;
#71043 = CARTESIAN_POINT ( 'NONE',  ( -0.7677165354330699465, -0.5400638737290845981, -0.3530559997133363437 ) ) ;
#71044 = CARTESIAN_POINT ( 'NONE',  ( 1.279527559055118724, 0.1660481256975885056, 0.3530559997133364547 ) ) ;
#71045 =( BOUNDED_CURVE ( )  B_SPLINE_CURVE ( 2, ( #11125, #67545, #54898, #22914, #42264, #48581, #4387, #16622, #30471, #30055, #81840, #67961, #68379 ),
 .UNSPECIFIED., .F., .F. ) 
 B_SPLINE_CURVE_WITH_KNOTS ( ( 3, 2, 2, 2, 2, 2, 3 ),
 ( 0.6285787205705962721, 0.6287878787878787845, 0.6325757575757575690, 0.6363636363636363535, 0.6401515151515151381, 0.6439393939393939226, 0.6441485521566764350 ),
 .UNSPECIFIED. ) 
 CURVE ( )  GEOMETRIC_REPRESENTATION_ITEM ( )  RATIONAL_B_SPLINE_CURVE ( ( 0.9964447847208419695, 0.9981185001348091834, 1.000000000000000000, 0.9659258262890683122, 1.000000000000000000, 0.9659258262890683122, 1.000000000000000000, 0.9659258262890683122, 1.000000000000000000, 0.9659258262890683122, 1.000000000000000000, 0.9981185001348091834, 0.9964447847208420805 ) ) 
 REPRESENTATION_ITEM ( '' )  );
#71046 = CARTESIAN_POINT ( 'NONE',  ( 0.2362204724409451007, -0.4091458600556402980, -0.01115485564304462100 ) ) ;
#71047 = CARTESIAN_POINT ( 'NONE',  ( -0.4921259842519677963, 0.07958543189024071263, -0.2665933059059888421 ) ) ;
#71048 = CARTESIAN_POINT ( 'NONE',  ( -0.4199475065616791736, 0.2306618581243847221, -0.2411417322834647770 ) ) ;
#71049 = CARTESIAN_POINT ( 'NONE',  ( 0.2690288713910767848, 0.2952755905511811885, 0.1292274648535926551 ) ) ;
#71050 = CARTESIAN_POINT ( 'NONE',  ( -3.937007874015748143, 2.165354330708662012, -0.6299212598425202314 ) ) ;
#71051 = CARTESIAN_POINT ( 'NONE',  ( 0.9645669291338588858, 0.07958543189024085140, 0.2665933059059887866 ) ) ;
#71052 = CARTESIAN_POINT ( 'NONE',  ( 0.1574803149606306130, -0.1870078740157479769, 0.3641732283464567677 ) ) ;
#71053 = CARTESIAN_POINT ( 'NONE',  ( -0.1509186351706028884, -0.3162353388693409650, -0.4822834645669289433 ) ) ;
#71054 = CARTESIAN_POINT ( 'NONE',  ( -1.469816272965878357, -0.6046776061558809534, -0.2411417322834644161 ) ) ;
#71055 = CARTESIAN_POINT ( 'NONE',  ( -0.8202099737532799750, 0.1771653543307087075, -0.09757992244046823083 ) ) ;
#71056 = CARTESIAN_POINT ( 'NONE',  ( -1.646051170424378096, -0.1870078740157480046, 1.254653134982923898E-17 ) ) ;
#71057 = CARTESIAN_POINT ( 'NONE',  ( -0.7545931758530176614, -0.6692913385826773087, -0.1292274648535924053 ) ) ;
#71058 = CARTESIAN_POINT ( 'NONE',  ( 0.3460692066303959202, -0.1998031496062991630, -1.126640419947506633 ) ) ;
#71059 = CARTESIAN_POINT ( 'NONE',  ( 0.1049643490035304938, -0.3917322834645669549, -2.689632545931758489 ) ) ;
#71060 = CARTESIAN_POINT ( 'NONE',  ( 0.09186351706036799403, -0.3690944881889765550, -0.3153832671262227771 ) ) ;
#71061 = CARTESIAN_POINT ( 'NONE',  ( -0.8398950131233585692, 0.2306618581243848609, 0.2411417322834645549 ) ) ;
#71062 = CARTESIAN_POINT ( 'NONE',  ( -1.069553805774277722, -0.6692913385826773087, -0.1292274648535924053 ) ) ;
#71063 = CARTESIAN_POINT ( 'NONE',  ( -1.279527559055116948, 0.07958543189024071263, -0.2665933059059888421 ) ) ;
#71064 = CARTESIAN_POINT ( 'NONE',  ( -3.918945891830401429, 1.247862022481391886, -0.3770874914321828419 ) ) ;
#71065 = CARTESIAN_POINT ( 'NONE',  ( -0.8136482939632537770, 0.1283753931104746893, -0.1820866141732285504 ) ) ;
#71066 = CARTESIAN_POINT ( 'NONE',  ( 0.4330708661417321248, 2.793565526369266028, 0.000000000000000000 ) ) ;
#71067 = CARTESIAN_POINT ( 'NONE',  ( 1.233595800524935227, -0.6046776061558807314, 0.2411417322834647770 ) ) ;
#71068 = LINE ( 'NONE', #26447, #68977 ) ;
#71069 = B_SPLINE_CURVE_WITH_KNOTS ( 'NONE', 3,
 ( #49477, #49059, #30536, #31347 ),
 .UNSPECIFIED., .F., .F.,
 ( 4, 4 ),
 ( 0.08422315286269926871, 0.08567085022608394995 ),
 .UNSPECIFIED. ) ;
#71070 = CARTESIAN_POINT ( 'NONE',  ( -0.1958661417322836995, 0.3392501089628017219, -2.057105929955067580 ) ) ;
#71071 = EDGE_CURVE ( 'NONE', #65199, #71941, #12956, .T. ) ;
#71072 = VERTEX_POINT ( 'NONE', #7497 ) ;
#71073 = CARTESIAN_POINT ( 'NONE',  ( -1.291027602697912169, 0.2755905511811023723, 0.5830028338522510456 ) ) ;
#71074 = CARTESIAN_POINT ( 'NONE',  ( 1.391076115485564868, -0.5023911411419708095, 0.1820866141732285504 ) ) ;
#71075 = CARTESIAN_POINT ( 'NONE',  ( -1.463254593175852492, -0.6692913385826773087, -0.1292274648535924053 ) ) ;
#71076 = CARTESIAN_POINT ( 'NONE',  ( 1.233595800524935227, -0.6046776061558807314, 0.2411417322834647770 ) ) ;
#71077 = CARTESIAN_POINT ( 'NONE',  ( -0.1958661417322836718, 0.3392501089628017219, -1.830052493438320216 ) ) ;
#71078 = CARTESIAN_POINT ( 'NONE',  ( 1.469816272965879911, -0.5023911411419708095, 0.1820866141732285504 ) ) ;
#71079 = CARTESIAN_POINT ( 'NONE',  ( 0.5511811023622055217, -0.1870078740157479769, 0.4822834645669291653 ) ) ;
#71080 = CARTESIAN_POINT ( 'NONE',  ( -0.006561679790025524116, -0.05778040916215560624, -0.4822834645669293319 ) ) ;
#71081 = CARTESIAN_POINT ( 'NONE',  ( -0.3495983942378629306, -0.3045330818767438275, -0.01888973282054034336 ) ) ;
#71082 = CARTESIAN_POINT ( 'NONE',  ( -0.7137454485294953965, 2.165354330708661124, -0.4917280318828585184 ) ) ;
#71083 = CARTESIAN_POINT ( 'NONE',  ( 0.8398950131233602345, 0.1283753931104746893, -0.1820866141732285504 ) ) ;
#71084 = CARTESIAN_POINT ( 'NONE',  ( -0.2925321140481932924, 0.2925321140481931814, -1.279527559055118058 ) ) ;
#71085 = ORIENTED_EDGE ( 'NONE', *, *, #21721, .F. ) ;
#71086 = CARTESIAN_POINT ( 'NONE',  ( 0.2867679344610366554, -0.2867679344610365999, -0.09516367273721974829 ) ) ;
#71087 = ORIENTED_EDGE ( 'NONE', *, *, #71221, .T. ) ;
#71088 = CARTESIAN_POINT ( 'NONE',  ( -0.1706036745406816491, -0.4281496062992124485, 0.4176697321401328655 ) ) ;
#71089 = CARTESIAN_POINT ( 'NONE',  ( -1.614173228346455824, 0.2952755905511811885, 0.000000000000000000 ) ) ;
#71090 = CARTESIAN_POINT ( 'NONE',  ( 0.4790026246719168435, -0.3162353388693409650, -0.4822834645669289433 ) ) ;
#71091 = CARTESIAN_POINT ( 'NONE',  ( 1.338582677165355062, -0.1870078740157479769, 0.4822834645669291653 ) ) ;
#71092 = CARTESIAN_POINT ( 'NONE',  ( 1.233595800524935227, -0.6046776061558807314, 0.2411417322834647770 ) ) ;
#71093 = CARTESIAN_POINT ( 'NONE',  ( -0.5708661417322825615, -0.5400638737290844871, 0.3530559997133364547 ) ) ;
#71094 = CARTESIAN_POINT ( 'NONE',  ( 0.1574803149606306130, -0.1870078740157479769, 0.4822834645669291653 ) ) ;
#71095 = CARTESIAN_POINT ( 'NONE',  ( 1.417322834645670104, -0.1870078740157479769, 0.4822834645669291653 ) ) ;
#71096 = CARTESIAN_POINT ( 'NONE',  ( 1.476377952755906220, 0.1660481256975883668, -0.3530559997133364547 ) ) ;
#71097 = CARTESIAN_POINT ( 'NONE',  ( 1.148293963254593875, -0.6692913385826771977, 0.1292274648535927661 ) ) ;
#71098 = CARTESIAN_POINT ( 'NONE',  ( -0.2755905511811018171, 0.2952755905511811885, 0.000000000000000000 ) ) ;
#71099 = CARTESIAN_POINT ( 'NONE',  ( -0.3392501089628017219, -0.1958661417322836718, -0.2020997375328083545 ) ) ;
#71100 = CARTESIAN_POINT ( 'NONE',  ( 0.2821522309711292364, 0.1771653543307087075, -0.09757992244046823083 ) ) ;
#71101 = ORIENTED_EDGE ( 'NONE', *, *, #77172, .F. ) ;
#71102 = CARTESIAN_POINT ( 'NONE',  ( 0.3420746716998660508, -0.1974969037888703871, -0.7349081364829396223 ) ) ;
#71103 = ORIENTED_EDGE ( 'NONE', *, *, #23392, .F. ) ;
#71104 = CARTESIAN_POINT ( 'NONE',  ( -0.6102362204724400829, 0.07958543189024085140, 0.2665933059059887866 ) ) ;
#71105 = DIRECTION ( 'NONE',  ( 1.000000000000000000, 0.000000000000000000, 0.000000000000000000 ) ) ;
#71106 = CARTESIAN_POINT ( 'NONE',  ( 0.2887139107611556010, -0.6046776061558807314, 0.2411417322834647770 ) ) ;
#71107 = CARTESIAN_POINT ( 'NONE',  ( -0.1968503937007867743, -0.6692913385826771977, 8.415575281601705876E-17 ) ) ;
#71108 = CARTESIAN_POINT ( 'NONE',  ( -1.069553805774277722, 0.2952755905511811885, 0.1292274648535926551 ) ) ;
#71109 = CARTESIAN_POINT ( 'NONE',  ( 0.1958661417322836718, -0.3392501089628017219, -1.820885457514122452 ) ) ;
#71110 = CARTESIAN_POINT ( 'NONE',  ( -1.509186351706035767, -0.4281496062992124485, 0.4176697321401328655 ) ) ;
#71111 = CARTESIAN_POINT ( 'NONE',  ( -0.2952755905511810774, 0.000000000000000000, 6.062992125984251857 ) ) ;
#71112 = CARTESIAN_POINT ( 'NONE',  ( 0.9711286089238851948, 0.1283753931104748280, 0.1820866141732283561 ) ) ;
#71113 = CARTESIAN_POINT ( 'NONE',  ( 0.6758530183727039509, -0.6692913385826771977, 0.1292274648535927661 ) ) ;
#71114 = CARTESIAN_POINT ( 'NONE',  ( 0.9055118110236227702, 0.2952755905511811885, 0.000000000000000000 ) ) ;
#71115 = CARTESIAN_POINT ( 'NONE',  ( 0.3996062992125986035, 2.446882876249141962E-17, -1.377952755905511806 ) ) ;
#71116 = CARTESIAN_POINT ( 'NONE',  ( 0.3252997568826557773, 2.459406111854941508E-15, 0.4281989832122450323 ) ) ;
#71117 = CARTESIAN_POINT ( 'NONE',  ( -9.787531504996566615E-17, 0.3996062992125985480, -0.8641732283464567121 ) ) ;
#71118 = CARTESIAN_POINT ( 'NONE',  ( -0.3996062992125984925, -0.1070741851644056858, 0.03477690288713908284 ) ) ;
#71119 = CARTESIAN_POINT ( 'NONE',  ( -0.1706036745406816491, -0.4281496062992124485, 0.4176697321401328655 ) ) ;
#71120 = CARTESIAN_POINT ( 'NONE',  ( -0.3996062992125986035, -7.340648628747425578E-17, -2.559055118110236560 ) ) ;
#71121 = CARTESIAN_POINT ( 'NONE',  ( 0.1049643490035303689, 0.3917322834645670104, -1.967847769028871374 ) ) ;
#71122 = CARTESIAN_POINT ( 'NONE',  ( -1.181102362204723644, -0.1870078740157479769, 0.3641732283464567677 ) ) ;
#71123 = CARTESIAN_POINT ( 'NONE',  ( 1.240157480314961314, -0.5400638737290844871, 0.3530559997133364547 ) ) ;
#71124 = CARTESIAN_POINT ( 'NONE',  ( 1.384514435695538559, 0.2952755905511810774, -0.1292274648535930714 ) ) ;
#71125 = CARTESIAN_POINT ( 'NONE',  ( 0.2296587926509192634, -0.2845877964562159024, 0.3641732283464567677 ) ) ;
#71126 = CARTESIAN_POINT ( 'NONE',  ( 0.4461942257217855201, -0.6046776061558807314, 0.2411417322834647770 ) ) ;
#71127 = CARTESIAN_POINT ( 'NONE',  ( -0.4091458600556402980, -0.2362204724409451284, -1.389107611548556553 ) ) ;
#71128 = CARTESIAN_POINT ( 'NONE',  ( 0.3280839895013130669, -0.3690944881889765550, -0.3153832671262227771 ) ) ;
#71129 = CARTESIAN_POINT ( 'NONE',  ( -0.1049868766404193215, 0.2306618581243847221, -0.2411417322834647770 ) ) ;
#71130 = CARTESIAN_POINT ( 'NONE',  ( -0.1974969037888704149, -0.3420746716998661063, -1.244750656167979086 ) ) ;
#71131 = CARTESIAN_POINT ( 'NONE',  ( -1.404199475065615932, 0.05413385826771666132, 0.4176697321401328100 ) ) ;
#71132 = CARTESIAN_POINT ( 'NONE',  ( 0.4986876640419954376, 0.1283753931104748280, 0.1820866141732283561 ) ) ;
#71133 = DIRECTION ( 'NONE',  ( 0.000000000000000000, 0.000000000000000000, -1.000000000000000000 ) ) ;
#71135 = EDGE_CURVE ( 'NONE', #80330, #17178, #33166, .T. ) ;
#71134 = CARTESIAN_POINT ( 'NONE',  ( -0.5380577427821514602, -0.4281496062992127816, -0.4176697321401328100 ) ) ;
#71136 = CARTESIAN_POINT ( 'NONE',  ( -0.3477690288713902178, 0.1771653543307087075, -0.09757992244046823083 ) ) ;
#71137 = CARTESIAN_POINT ( 'NONE',  ( -0.3129921259842520787, 1.496062992125984259, 2.300774849103979725E-17 ) ) ;
#71138 = CARTESIAN_POINT ( 'NONE',  ( -0.9186351706036736120, 0.2306618581243848609, 0.2411417322834645549 ) ) ;
#71139 = CARTESIAN_POINT ( 'NONE',  ( -0.09186351706036663400, -0.4281496062992124485, 0.4176697321401328655 ) ) ;
#71140 = CARTESIAN_POINT ( 'NONE',  ( 0.1837270341207354329, 0.1283753931104748280, 0.1820866141732283561 ) ) ;
#71141 = CARTESIAN_POINT ( 'NONE',  ( 0.1070741851644054776, -0.3996062992125984925, -2.051837270341207109 ) ) ;
#71142 = CARTESIAN_POINT ( 'NONE',  ( -0.07874015748031421014, -0.1870078740157479769, 0.4822834645669291653 ) ) ;
#71143 = EDGE_CURVE ( 'NONE', #82700, #13953, #77805, .T. ) ;
#71144 = CARTESIAN_POINT ( 'NONE',  ( 0.2867679344610365999, 0.2867679344610365999, -1.950111917813961426 ) ) ;
#71145 = CARTESIAN_POINT ( 'NONE',  ( 0.8530183727034128527, -0.3690944881889763329, 0.3153832671262228327 ) ) ;
#71146 = CARTESIAN_POINT ( 'NONE',  ( 1.213910761154856299, -0.6692913385826773087, -0.1292274648535924053 ) ) ;
#71147 = VECTOR ( 'NONE', #81168, 39.37007874015748143 ) ;
#71148 = CARTESIAN_POINT ( 'NONE',  ( -1.023622047244094002, -0.1870078740157480601, -0.3641732283464567677 ) ) ;
#71149 = CARTESIAN_POINT ( 'NONE',  ( -1.246719160104986512, -0.004921259842519576551, 0.3153832671262227771 ) ) ;
#71150 = CARTESIAN_POINT ( 'NONE',  ( -0.5839895013123351797, -0.6692913385826771977, 0.1292274648535927661 ) ) ;
#71151 = CARTESIAN_POINT ( 'NONE',  ( 0.09842519685039434474, -0.5400638737290845981, -0.3530559997133363437 ) ) ;
#71152 = CARTESIAN_POINT ( 'NONE',  ( 0.3805774278215230400, -0.3690944881889763329, 0.3153832671262228327 ) ) ;
#71153 = CARTESIAN_POINT ( 'NONE',  ( -0.4091458600556405756, 0.2362204724409446288, -2.388451443569553856 ) ) ;
#71154 = CARTESIAN_POINT ( 'NONE',  ( 1.023622047244095112, -0.1870078740157480601, -0.3641732283464567677 ) ) ;
#71155 = CARTESIAN_POINT ( 'NONE',  ( 0.1771653543307093182, -0.5400638737290845981, -0.3530559997133363437 ) ) ;
#71156 = ADVANCED_FACE ( 'NONE', ( #65585 ), #54580, .F. ) ;
#71157 = CARTESIAN_POINT ( 'NONE',  ( -1.614173228346456712, 2.362204724409448620, 0.1372047244094477536 ) ) ;
#71158 = CARTESIAN_POINT ( 'NONE',  ( -0.07874015748031421014, -0.1870078740157480879, -0.4822834645669291653 ) ) ;
#71159 = CARTESIAN_POINT ( 'NONE',  ( -0.1049643490035302024, -0.3917322834645671215, -1.416666666666666519 ) ) ;
#71160 = CARTESIAN_POINT ( 'NONE',  ( 1.515748031496063186, -0.4536011799217368745, -0.2665933059059886201 ) ) ;
#71161 = CARTESIAN_POINT ( 'NONE',  ( 0.2624671916010504757, 0.2306618581243848609, 0.2411417322834645549 ) ) ;
#71162 = CARTESIAN_POINT ( 'NONE',  ( 0.2952755905511819101, 0.1660481256975883668, -0.3530559997133364547 ) ) ;
#71163 = CARTESIAN_POINT ( 'NONE',  ( 0.5708661417322841158, 0.1012011053420777407, 0.2882089793578256898 ) ) ;
#71164 = CARTESIAN_POINT ( 'NONE',  ( 0.01968503937007957949, -0.4536011799217368745, -0.2665933059059886201 ) ) ;
#71165 = CARTESIAN_POINT ( 'NONE',  ( 0.8923884514435703741, 0.2306618581243848609, 0.2411417322834645549 ) ) ;
#71166 = CARTESIAN_POINT ( 'NONE',  ( -0.3215223097112853146, -0.2845877964562159024, 0.3641732283464567677 ) ) ;
#71167 = CARTESIAN_POINT ( 'NONE',  ( -0.7611548556430438595, -0.6046776061558809534, -0.2411417322834644161 ) ) ;
#71168 = CARTESIAN_POINT ( 'NONE',  ( 0.000000000000000000, 0.000000000000000000, -2.755905511811024056 ) ) ;
#71169 = CARTESIAN_POINT ( 'NONE',  ( -0.2690288713910754526, 0.2952755905511810774, -0.1292274648535930714 ) ) ;
#71170 = CARTESIAN_POINT ( 'NONE',  ( -1.246719160104985846, -0.4281496062992127816, -0.4176697321401328100 ) ) ;
#71171 = CARTESIAN_POINT ( 'NONE',  ( -0.4855643044619415427, -0.3690944881889763329, 0.3153832671262228327 ) ) ;
#71172 = CARTESIAN_POINT ( 'NONE',  ( 0.1574803149606306130, -0.1870078740157479769, 0.4822834645669291653 ) ) ;
#71173 = CARTESIAN_POINT ( 'NONE',  ( -1.430446194225721390, -0.4281496062992124485, 0.4176697321401328655 ) ) ;
#71174 = CARTESIAN_POINT ( 'NONE',  ( -0.1968503937007867743, 0.2952755905511811885, 0.000000000000000000 ) ) ;
#71175 = CARTESIAN_POINT ( 'NONE',  ( 0.4724973665168182846, 1.580780302271975080, -2.165475543433776462 ) ) ;
#71177 = CARTESIAN_POINT ( 'NONE',  ( 1.148293963254593653, 0.2952755905511810774, -0.1292274648535930714 ) ) ;
#71176 = CARTESIAN_POINT ( 'NONE',  ( -0.9332960234133773625, 0.02791078216816064370, 0.4328096321851915285 ) ) ;
#71178 = CARTESIAN_POINT ( 'NONE',  ( 1.213910761154856299, 0.2952755905511811885, 0.1292274648535926551 ) ) ;
#71179 = CARTESIAN_POINT ( 'NONE',  ( 0.3392501089628018329, 0.1958661417322835607, -2.643044619422571628 ) ) ;
#71180 = DIRECTION ( 'NONE',  ( -1.000000000000000000, -0.000000000000000000, -0.000000000000000000 ) ) ;
#71181 = CARTESIAN_POINT ( 'NONE',  ( -1.371391076115484831, 0.2952755905511810774, -0.1292274648535930714 ) ) ;
#71182 = CARTESIAN_POINT ( 'NONE',  ( -1.157146581871515012E-16, 0.4724409448818898682, -0.7874015748031496509 ) ) ;
#71183 = CARTESIAN_POINT ( 'NONE',  ( 0.1070741851644053527, 0.3996062992125986590, -0.1509186351706036655 ) ) ;
#71184 = ORIENTED_EDGE ( 'NONE', *, *, #23107, .F. ) ;
#71185 = CARTESIAN_POINT ( 'NONE',  ( 0.01312335958005323398, -0.3690944881889765550, -0.3153832671262227771 ) ) ;
#71186 = CARTESIAN_POINT ( 'NONE',  ( -0.3917322834645671215, 0.1049643490035301469, -1.914698162729658648 ) ) ;
#71187 = EDGE_LOOP ( 'NONE', ( #6180, #66437, #65087, #16245 ) ) ;
#71188 = CARTESIAN_POINT ( 'NONE',  ( 0.3608923884514443348, 0.2952755905511810774, -0.1292274648535930714 ) ) ;
#71189 = CARTESIAN_POINT ( 'NONE',  ( 0.4265091863517067039, -0.6692913385826773087, -0.1292274648535924053 ) ) ;
#71190 = CARTESIAN_POINT ( 'NONE',  ( 0.4724409448818897572, -0.1265901696524988906, -2.788713910761154047 ) ) ;
#71191 = CARTESIAN_POINT ( 'NONE',  ( -1.586052503253849499, 0.4724409448818907564, 0.1653254495020552439 ) ) ;
#71192 = CARTESIAN_POINT ( 'NONE',  ( -0.8661417322834640276, -0.1870078740157479769, 0.3641732283464567677 ) ) ;
#71193 = CARTESIAN_POINT ( 'NONE',  ( -0.2726377952755906220, -0.1133856558944467546, 0.1574803149606299191 ) ) ;
#71194 = CARTESIAN_POINT ( 'NONE',  ( 0.8530183727034128527, -0.4281496062992124485, 0.4176697321401328655 ) ) ;
#71195 = CARTESIAN_POINT ( 'NONE',  ( 0.8595800524934390507, -0.08942795157528024563, -0.3641732283464568787 ) ) ;
#71196 = CARTESIAN_POINT ( 'NONE',  ( -0.2099737532808391705, 0.2306618581243848609, 0.2411417322834645549 ) ) ;
#71197 = CARTESIAN_POINT ( 'NONE',  ( 0.3392501089628018329, -0.1958661417322834497, -1.287382259021310427 ) ) ;
#71198 = CARTESIAN_POINT ( 'NONE',  ( -0.8727034120734901146, -0.3162353388693405765, 0.4822834645669290543 ) ) ;
#71199 = CARTESIAN_POINT ( 'NONE',  ( -1.725721784776902190, -0.08942795157527998196, 0.3641732283464567121 ) ) ;
#71200 = CARTESIAN_POINT ( 'NONE',  ( -0.8398950131233589023, -0.6046776061558809534, -0.2411417322834644161 ) ) ;
#71201 = CARTESIAN_POINT ( 'NONE',  ( 1.391076115485564868, 0.2306618581243847221, -0.2411417322834647770 ) ) ;
#71202 = CARTESIAN_POINT ( 'NONE',  ( 1.614173228346457378, -0.5511811023622047445, 6.969142054262312111E-17 ) ) ;
#71203 = ORIENTED_EDGE ( 'NONE', *, *, #40191, .T. ) ;
#71204 = CARTESIAN_POINT ( 'NONE',  ( -0.3917322834645670104, -0.1049643490035307020, -2.562355273787088716 ) ) ;
#71205 = CARTESIAN_POINT ( 'NONE',  ( -0.1837270341207340729, 0.2306618581243847221, -0.2411417322834647770 ) ) ;
#71206 = VERTEX_POINT ( 'NONE', #20955 ) ;
#71207 = CARTESIAN_POINT ( 'NONE',  ( -0.6496062992125976043, -0.5400638737290844871, 0.3530559997133364547 ) ) ;
#71208 = CARTESIAN_POINT ( 'NONE',  ( 1.535433070866142335, -0.6692913385826771977, 8.415575281601705876E-17 ) ) ;
#71209 = CARTESIAN_POINT ( 'NONE',  ( 1.364829396325459854, -0.6046776061558809534, -0.2411417322834644161 ) ) ;
#71210 = CARTESIAN_POINT ( 'NONE',  ( 0.1837270341207354329, 0.2306618581243848609, 0.2411417322834645549 ) ) ;
#71211 = CARTESIAN_POINT ( 'NONE',  ( -0.03280839895013062252, 0.2952755905511810774, -0.1292274648535930714 ) ) ;
#71212 = CARTESIAN_POINT ( 'NONE',  ( 0.3392501089628018329, 0.1958661417322835607, -1.948162729658792891 ) ) ;
#71213 = CARTESIAN_POINT ( 'NONE',  ( -1.043307086614172707, 0.1660481256975883668, -0.3530559997133364547 ) ) ;
#71214 = CARTESIAN_POINT ( 'NONE',  ( -0.3871391076115476282, -0.05778040916215522460, 0.4822834645669289988 ) ) ;
#71215 = CARTESIAN_POINT ( 'NONE',  ( -0.1968503937007867743, 0.1771653543307087630, 0.000000000000000000 ) ) ;
#71216 = CARTESIAN_POINT ( 'NONE',  ( -0.08106202739150959735, 0.3841287887292361702, -8.192289201020256726E-18 ) ) ;
#71217 = CARTESIAN_POINT ( 'NONE',  ( 1.286089238845145033, -0.6046776061558809534, -0.2411417322834644161 ) ) ;
#71219 = B_SPLINE_CURVE_WITH_KNOTS ( 'NONE', 3,
 ( #77876, #20630, #45857, #65251 ),
 .UNSPECIFIED., .F., .F.,
 ( 4, 4 ),
 ( 3.210432057730626195E-07, 0.001287787053611958712 ),
 .UNSPECIFIED. ) ;
#71218 = CARTESIAN_POINT ( 'NONE',  ( -0.5905511811023615998, 0.2952755905511811885, 0.000000000000000000 ) ) ;
#71220 = CARTESIAN_POINT ( 'NONE',  ( -1.194225721784776262, 0.05413385826771626580, -0.4176697321401330321 ) ) ;
#71221 = EDGE_CURVE ( 'NONE', #47373, #39419, #1187, .T. ) ;
#71222 = CARTESIAN_POINT ( 'NONE',  ( 0.9842519685039375910, 0.2952755905511811885, 0.000000000000000000 ) ) ;
#71223 = FACE_OUTER_BOUND ( 'NONE', #63504, .T. ) ;
#71224 = VERTEX_POINT ( 'NONE', #48684 ) ;
#71225 = ORIENTED_EDGE ( 'NONE', *, *, #37212, .F. ) ;
#71226 = CARTESIAN_POINT ( 'NONE',  ( 0.3543307086614181922, -0.6692913385826771977, 8.415575281601705876E-17 ) ) ;
#71227 = CARTESIAN_POINT ( 'NONE',  ( -0.1049868766404193215, 0.1283753931104746893, -0.1820866141732285504 ) ) ;
#71229 = DIRECTION ( 'NONE',  ( 0.000000000000000000, 0.000000000000000000, -1.000000000000000000 ) ) ;
#71228 = CARTESIAN_POINT ( 'NONE',  ( 1.397637795275591177, 0.07958543189024071263, -0.2665933059059888421 ) ) ;
#71230 = CARTESIAN_POINT ( 'NONE',  ( -0.4724409448818899238, 0.1265901696524986686, -0.4245406824146981672 ) ) ;
#71231 = CARTESIAN_POINT ( 'NONE',  ( 1.607611548556431069, -0.5511811023622048555, -0.09757992244046775898 ) ) ;
#71232 = CARTESIAN_POINT ( 'NONE',  ( 1.358267716535433323, -0.5400638737290845981, -0.3530559997133363437 ) ) ;
#71233 = CARTESIAN_POINT ( 'NONE',  ( 0.3949938075777409408, -0.1058382717557499186, -0.3458005249343832910 ) ) ;
#71234 = CARTESIAN_POINT ( 'NONE',  ( 0.04593175853018440641, 0.2952755905511810774, -0.1292274648535930714 ) ) ;
#71235 = DIRECTION ( 'NONE',  ( 0.000000000000000000, 0.000000000000000000, -1.000000000000000000 ) ) ;
#71236 = CARTESIAN_POINT ( 'NONE',  ( -1.666666666666665853, 0.05413385826771626580, -0.4176697321401330321 ) ) ;
#71237 = CARTESIAN_POINT ( 'NONE',  ( -0.3346456692913377662, -0.5400638737290844871, 0.3530559997133364547 ) ) ;
#71238 = CARTESIAN_POINT ( 'NONE',  ( -0.3949938075777408852, -0.1058382717557502933, -0.1227034120734908501 ) ) ;
#71239 = CARTESIAN_POINT ( 'NONE',  ( -1.489501312335957062, -0.08942795157527998196, 0.3641732283464567121 ) ) ;
#71240 = CARTESIAN_POINT ( 'NONE',  ( 0.3280839895013130669, 0.05413385826771666132, 0.4176697321401328100 ) ) ;
#71241 = CARTESIAN_POINT ( 'NONE',  ( 1.023622047244095334, -0.1870078740157479769, 0.3641732283464567677 ) ) ;
#71242 = CARTESIAN_POINT ( 'NONE',  ( 0.2699421371814171300, 1.133868921557234843, 0.1587517418123144675 ) ) ;
#71243 = CARTESIAN_POINT ( 'NONE',  ( 0.9186351706036752773, 0.1283753931104746893, -0.1820866141732285504 ) ) ;
#71244 = CARTESIAN_POINT ( 'NONE',  ( -1.089238845144356427, -0.4281496062992127816, -0.4176697321401328100 ) ) ;
#71245 = CARTESIAN_POINT ( 'NONE',  ( -0.3996062992125984925, -0.1070741851644056858, -0.9101049868766404316 ) ) ;
#71246 = CARTESIAN_POINT ( 'NONE',  ( 1.115485564304462551, -0.4281496062992127816, -0.4176697321401328100 ) ) ;
#71247 = CARTESIAN_POINT ( 'NONE',  ( 0.3917322834645669549, 0.1049643490035304660, -0.7467191601049868455 ) ) ;
#71249 = CARTESIAN_POINT ( 'NONE',  ( 0.9317585301837276734, 0.05413385826771626580, -0.4176697321401330321 ) ) ;
#71248 = CARTESIAN_POINT ( 'NONE',  ( 0.7020997375328090762, -0.3162353388693405765, 0.4822834645669290543 ) ) ;
#71250 = LINE ( 'NONE', #77990, #26798 ) ;
#71251 = CARTESIAN_POINT ( 'NONE',  ( 0.2821522309711292364, -0.5511811023622046335, 0.09757992244046803654 ) ) ;
#71252 = CARTESIAN_POINT ( 'NONE',  ( 0.4265091863517067594, 0.2952755905511811885, 0.1292274648535926551 ) ) ;
#71253 = CARTESIAN_POINT ( 'NONE',  ( -0.4732185887570871108, 1.572090529166659811, 2.167227123902327079 ) ) ;
#71254 = CARTESIAN_POINT ( 'NONE',  ( -1.115485564304461219, -0.3690944881889763329, 0.3153832671262228327 ) ) ;
#71255 = CARTESIAN_POINT ( 'NONE',  ( -0.9908136482939626788, -0.6692913385826773087, -0.1292274648535924053 ) ) ;
#71256 = CARTESIAN_POINT ( 'NONE',  ( 1.017060367454068803, -0.3162353388693405765, 0.4822834645669290543 ) ) ;
#71257 = CARTESIAN_POINT ( 'NONE',  ( -1.023622047244094002, -0.1870078740157480879, -0.4822834645669291653 ) ) ;
#71258 = CARTESIAN_POINT ( 'NONE',  ( 0.7742782152230979209, 0.05413385826771626580, -0.4176697321401330321 ) ) ;
#71259 = CARTESIAN_POINT ( 'NONE',  ( -1.489501312335957062, -0.08942795157527998196, 0.3641732283464567121 ) ) ;
#71260 = DIRECTION ( 'NONE',  ( -1.000000000000000000, -0.000000000000000000, -0.000000000000000000 ) ) ;
#71261 = CARTESIAN_POINT ( 'NONE',  ( 1.167979002624672580, 0.05413385826771626580, -0.4176697321401330321 ) ) ;
#71262 = CARTESIAN_POINT ( 'NONE',  ( 0.3458507752293908943, 0.3458507752293908943, -2.576771653543307394 ) ) ;
#71263 = CARTESIAN_POINT ( 'NONE',  ( 1.358267716535433323, 0.1660481256975885056, 0.3530559997133364547 ) ) ;
#71264 = CARTESIAN_POINT ( 'NONE',  ( -1.522309711286088607, 0.1283753931104746893, -0.1820866141732285504 ) ) ;
#71265 = CARTESIAN_POINT ( 'NONE',  ( 1.561679790026247350, -0.004921259842519870586, -0.3153832671262229437 ) ) ;
#71266 = CARTESIAN_POINT ( 'NONE',  ( -1.489501312335957062, -0.08942795157527998196, 0.3641732283464567121 ) ) ;
#71267 = CARTESIAN_POINT ( 'NONE',  ( -0.4265091863517051496, -0.5511811023622046335, 0.09757992244046803654 ) ) ;
#71268 = DIRECTION ( 'NONE',  ( 1.408710688920637755E-15, -1.000000000000000000, 4.918487082195260922E-30 ) ) ;
#71269 = CARTESIAN_POINT ( 'NONE',  ( 0.9383202099737536495, -0.2845877964562159024, 0.3641732283464567677 ) ) ;
#71270 = CARTESIAN_POINT ( 'NONE',  ( 0.5905511811023629321, 0.2952755905511811885, 0.000000000000000000 ) ) ;
#71271 = CARTESIAN_POINT ( 'NONE',  ( 1.187664041994751285, -0.3162353388693409650, -0.4822834645669289433 ) ) ;
#71272 = CARTESIAN_POINT ( 'NONE',  ( -0.02624671916010428221, 0.2306618581243847221, -0.2411417322834647770 ) ) ;
#71273 = CARTESIAN_POINT ( 'NONE',  ( 0.7611548556430451917, -0.5023911411419708095, 0.1820866141732285504 ) ) ;
#71274 = CARTESIAN_POINT ( 'NONE',  ( -1.482939632545930975, 0.05413385826771666132, 0.4176697321401328100 ) ) ;
#71275 = CARTESIAN_POINT ( 'NONE',  ( -1.614173228346455824, 0.2952755905511811885, 0.000000000000000000 ) ) ;
#71276 = CARTESIAN_POINT ( 'NONE',  ( -0.4068241469816267775, 0.05413385826771626580, -0.4176697321401330321 ) ) ;
#71277 = CARTESIAN_POINT ( 'NONE',  ( 4.893765752498283924E-17, -0.3996062992125986035, -0.5511811023622047445 ) ) ;
#71278 = LINE ( 'NONE', #46001, #1874 ) ;
#71279 = CARTESIAN_POINT ( 'NONE',  ( 0.1771653543307093182, 0.1660481256975885056, 0.3530559997133364547 ) ) ;
#71280 = CARTESIAN_POINT ( 'NONE',  ( -0.5446194225721777693, -0.05778040916215522460, 0.4822834645669289988 ) ) ;
#71281 = CARTESIAN_POINT ( 'NONE',  ( -0.006561679790025524116, -0.3162353388693405765, 0.4822834645669290543 ) ) ;
#71282 = ADVANCED_FACE ( 'NONE', ( #79459, #41956 ), #66829, .F. ) ;
#71283 = CARTESIAN_POINT ( 'NONE',  ( 0.3996062992125986035, 2.446882876249141962E-17, -2.637795275590551380 ) ) ;
#71284 = CARTESIAN_POINT ( 'NONE',  ( 4.837279021331060870E-17, -0.3949938075777409963, -1.811023622047243986 ) ) ;
#71285 = CARTESIAN_POINT ( 'NONE',  ( 0.1049643490035303689, 0.3917322834645670104, -0.4580052493438320216 ) ) ;
#71286 = DIRECTION ( 'NONE',  ( 0.000000000000000000, 1.000000000000000000, -0.000000000000000000 ) ) ;
#71287 = CARTESIAN_POINT ( 'NONE',  ( -0.1049643490035307020, 0.3917322834645669549, -1.101049868766404094 ) ) ;
#71288 = EDGE_CURVE ( 'NONE', #25114, #70359, #9233, .T. ) ;
#71289 = CARTESIAN_POINT ( 'NONE',  ( -1.108923884514435132, -0.2845877964562159024, 0.3641732283464567677 ) ) ;
#71290 = CARTESIAN_POINT ( 'NONE',  ( -0.3917322834645669549, -0.1049643490035306603, -0.9829396325459317518 ) ) ;
#71291 = CARTESIAN_POINT ( 'NONE',  ( -1.030183727034119867, -0.05778040916215560624, -0.4822834645669293319 ) ) ;
#71292 = CARTESIAN_POINT ( 'NONE',  ( -0.1058382717557497660, -0.3949938075777411073, -2.826115485564304475 ) ) ;
#71293 = CARTESIAN_POINT ( 'NONE',  ( 0.2493438320209980519, 0.05413385826771666132, 0.4176697321401328100 ) ) ;
#71294 = CARTESIAN_POINT ( 'NONE',  ( -0.1640419947506555343, -0.2845877964562159024, 0.3641732283464567677 ) ) ;
#71295 = CARTESIAN_POINT ( 'NONE',  ( 1.272965879265092637, 0.05413385826771666132, 0.4176697321401328100 ) ) ;
#71296 = CARTESIAN_POINT ( 'NONE',  ( 0.2624671916010504757, -0.6046776061558809534, -0.2411417322834644161 ) ) ;
#71297 = CARTESIAN_POINT ( 'NONE',  ( -0.4741627488320071526, 1.554989095716458269, -2.169534490215677902 ) ) ;
#71298 = CARTESIAN_POINT ( 'NONE',  ( -0.2925321140481932924, 0.2925321140481931814, -2.696850393700787052 ) ) ;
#71299 = CARTESIAN_POINT ( 'NONE',  ( 0.1958661417322836718, -0.3392501089628017219, -1.033483882710973134 ) ) ;
#71300 = CARTESIAN_POINT ( 'NONE',  ( 1.305774278215223960, -0.6692913385826771977, 0.1292274648535927661 ) ) ;
#71301 = CARTESIAN_POINT ( 'NONE',  ( 0.4133858267716541968, -0.5400638737290845981, -0.3530559997133363437 ) ) ;
#71302 = CARTESIAN_POINT ( 'NONE',  ( 0.2362204724409456558, -0.1870078740157480879, -0.4822834645669291653 ) ) ;
#71303 = CARTESIAN_POINT ( 'NONE',  ( 1.345144356955381593, -0.05778040916215522460, 0.4822834645669289988 ) ) ;
#71304 =( REPRESENTATION_RELATIONSHIP ('NONE','NONE', #79348, #61632 ) REPRESENTATION_RELATIONSHIP_WITH_TRANSFORMATION ( #49382 )SHAPE_REPRESENTATION_RELATIONSHIP( ) );
#71305 = CARTESIAN_POINT ( 'NONE',  ( -0.2867679344610365999, 0.2867679344610364889, -0.7342519685039372579 ) ) ;
#71306 = CARTESIAN_POINT ( 'NONE',  ( 0.03280839895013198948, 0.2952755905511811885, 0.1292274648535926551 ) ) ;
#71307 = CARTESIAN_POINT ( 'NONE',  ( 1.017060367454068803, -0.3162353388693405765, 0.4822834645669290543 ) ) ;
#71308 = CARTESIAN_POINT ( 'NONE',  ( 0.3543307086614181922, -0.6692913385826771977, 8.415575281601705876E-17 ) ) ;
#71309 = CARTESIAN_POINT ( 'NONE',  ( 1.003937007874016407, -0.4536011799217367080, 0.2665933059059888421 ) ) ;
#71310 = CARTESIAN_POINT ( 'NONE',  ( -1.023622047244094002, -0.1870078740157480879, -0.4822834645669291653 ) ) ;
#71311 = CARTESIAN_POINT ( 'NONE',  ( -1.312335958005248715, -0.6046776061558809534, -0.2411417322834644161 ) ) ;
#71312 = CARTESIAN_POINT ( 'NONE',  ( 0.8398950131233602345, 0.2306618581243847221, -0.2411417322834647770 ) ) ;
#71313 = CARTESIAN_POINT ( 'NONE',  ( 0.03611438844186872638, -0.3902087894126607392, -1.929133858267717105 ) ) ;
#71314 = CARTESIAN_POINT ( 'NONE',  ( 0.3392501089628018884, -0.1958661417322834220, -1.986876640419947604 ) ) ;
#71315 = CARTESIAN_POINT ( 'NONE',  ( 1.509186351706037543, 0.05413385826771666132, 0.4176697321401328100 ) ) ;
#71316 = ORIENTED_EDGE ( 'NONE', *, *, #83256, .F. ) ;
#71317 = CARTESIAN_POINT ( 'NONE',  ( 0.1998031496062994405, -0.3460692066303958092, 0.06561679790026245240 ) ) ;
#71318 = ORIENTED_EDGE ( 'NONE', *, *, #82137, .F. ) ;
#71319 = CARTESIAN_POINT ( 'NONE',  ( 1.653543307086614789, -0.1870078740157479769, 0.4822834645669291653 ) ) ;
#71320 = CARTESIAN_POINT ( 'NONE',  ( 0.9251968503937015864, -0.4536011799217367080, 0.2665933059059888421 ) ) ;
#71321 = CARTESIAN_POINT ( 'NONE',  ( -1.157146581871515012E-16, 0.4724409448818898682, -2.438976377952756014 ) ) ;
#71322 = CARTESIAN_POINT ( 'NONE',  ( -0.1443569553805768291, 0.05413385826771666132, 0.4176697321401328100 ) ) ;
#71323 = CARTESIAN_POINT ( 'NONE',  ( -0.4091458600556402980, -0.2362204724409451284, -1.154855643044619518 ) ) ;
#71324 = CARTESIAN_POINT ( 'NONE',  ( -0.3392501089628019995, 0.1958661417322832277, -0.8982939632545933195 ) ) ;
#71325 = EDGE_CURVE ( 'NONE', #36386, #18415, #54164, .T. ) ;
#71326 = CARTESIAN_POINT ( 'NONE',  ( -1.292650918635170010, 0.1771653543307087075, -0.09757992244046823083 ) ) ;
#71327 = CARTESIAN_POINT ( 'NONE',  ( 1.587926509186352142, 0.05413385826771666132, 0.4176697321401328100 ) ) ;
#71328 = CARTESIAN_POINT ( 'NONE',  ( -1.640419947506561060, 0.05413385826771666132, 0.4176697321401328100 ) ) ;
#71329 = CARTESIAN_POINT ( 'NONE',  ( -0.1312335958005241554, 0.2306618581243848609, 0.2411417322834645549 ) ) ;
#71330 = CARTESIAN_POINT ( 'NONE',  ( 1.430446194225722500, 0.05413385826771666132, 0.4176697321401328100 ) ) ;
#71331 = ORIENTED_EDGE ( 'NONE', *, *, #30606, .T. ) ;
#71332 = AXIS2_PLACEMENT_3D ( 'NONE', #18227, #29193, #3527 ) ;
#71333 = CARTESIAN_POINT ( 'NONE',  ( -0.7210809602247715278, -2.613618158232546091E-15, -0.3464511005275220379 ) ) ;
#71334 = CARTESIAN_POINT ( 'NONE',  ( -0.2362204724409451284, 0.4091458600556402425, -2.690288713910760965 ) ) ;
#71335 = LINE ( 'NONE', #7357, #73471 ) ;
#71336 = CARTESIAN_POINT ( 'NONE',  ( -0.7283464566929126471, -0.4536011799217367080, 0.2665933059059888421 ) ) ;
#71337 = CARTESIAN_POINT ( 'NONE',  ( -1.489501312335957062, -0.05778040916215522460, 0.4822834645669289988 ) ) ;
#71338 = CARTESIAN_POINT ( 'NONE',  ( 0.7020997375328090762, -0.3162353388693405765, 0.4822834645669290543 ) ) ;
#71339 = VERTEX_POINT ( 'NONE', #35653 ) ;
#71341 = DIRECTION ( 'NONE',  ( -0.000000000000000000, 1.000000000000000000, 0.000000000000000000 ) ) ;
#71340 = CARTESIAN_POINT ( 'NONE',  ( 0.2362204724409451007, -0.4091458600556402980, -2.530839895013123453 ) ) ;
#71342 = CARTESIAN_POINT ( 'NONE',  ( 1.167979002624672580, -0.4281496062992124485, 0.4176697321401328655 ) ) ;
#71343 = CARTESIAN_POINT ( 'NONE',  ( -1.574803149606298636, -0.1870078740157479769, 0.4822834645669291653 ) ) ;
#71344 = CARTESIAN_POINT ( 'NONE',  ( -0.3917322834645670659, 0.1049643490035301607, -0.9002431514097621879 ) ) ;
#71345 = CARTESIAN_POINT ( 'NONE',  ( -0.2952755905511804668, 0.07958543189024085140, 0.2665933059059887866 ) ) ;
#71346 = CARTESIAN_POINT ( 'NONE',  ( -1.587926509186350810, -0.004921259842519870586, -0.3153832671262229437 ) ) ;
#71347 = DIRECTION ( 'NONE',  ( -0.000000000000000000, -1.000000000000000000, -0.000000000000000000 ) ) ;
#71348 = CARTESIAN_POINT ( 'NONE',  ( 0.4396325459317590445, -0.6692913385826771977, 0.1292274648535927661 ) ) ;
#71349 = CARTESIAN_POINT ( 'NONE',  ( -0.4461942257217840213, -0.5023911411419708095, -0.1820866141732282451 ) ) ;
#71350 = CARTESIAN_POINT ( 'NONE',  ( 0.04593175853018440641, 0.1771653543307087075, -0.09757992244046823083 ) ) ;
#71351 = AXIS2_PLACEMENT_3D ( 'NONE', #21082, #2139, #27807 ) ;
#71352 = CARTESIAN_POINT ( 'NONE',  ( 0.1115485564304467270, -0.6692913385826773087, -0.1292274648535924053 ) ) ;
#71353 = CARTESIAN_POINT ( 'NONE',  ( -1.043307086614172041, -0.4536011799217367080, 0.2665933059059888421 ) ) ;
#71354 = CARTESIAN_POINT ( 'NONE',  ( -0.3917322834645671770, 0.1049643490035302024, -0.02954687483695727160 ) ) ;
#71355 = CARTESIAN_POINT ( 'NONE',  ( 0.8398950131233602345, 0.2306618581243847221, -0.2411417322834647770 ) ) ;
#71356 = CARTESIAN_POINT ( 'NONE',  ( -1.581364829396324945, -0.05778040916215560624, -0.4822834645669293319 ) ) ;
#71357 = CARTESIAN_POINT ( 'NONE',  ( 0.2362204724409451007, -0.4091458600556402980, -1.270997375328083878 ) ) ;
#71358 = CARTESIAN_POINT ( 'NONE',  ( -0.4658792650918627265, -0.05778040916215522460, 0.4822834645669289988 ) ) ;
#71359 = CARTESIAN_POINT ( 'NONE',  ( 0.2624671916010504757, -0.5023911411419708095, -0.1820866141732282451 ) ) ;
#71360 = CARTESIAN_POINT ( 'NONE',  ( -0.8595800524934373854, -0.05778040916215522460, 0.4822834645669289988 ) ) ;
#71361 = CARTESIAN_POINT ( 'NONE',  ( 0.7152230971128616943, -0.08942795157527998196, 0.3641732283464567121 ) ) ;
#71362 = CARTESIAN_POINT ( 'NONE',  ( -0.3018372703412066094, -0.004921259842519576551, 0.3153832671262227771 ) ) ;
#71363 = CARTESIAN_POINT ( 'NONE',  ( -0.8398950131233589023, -0.6046776061558809534, -0.2411417322834644161 ) ) ;
#71364 = CARTESIAN_POINT ( 'NONE',  ( -1.502624671916009680, -0.3162353388693405765, 0.4822834645669290543 ) ) ;
#71365 = FACE_OUTER_BOUND ( 'NONE', #55634, .T. ) ;
#71366 = CARTESIAN_POINT ( 'NONE',  ( 1.377952755905512472, 0.1771653543307087630, 0.000000000000000000 ) ) ;
#71367 = CARTESIAN_POINT ( 'NONE',  ( 0.5380577427821529035, -0.4281496062992124485, 0.4176697321401328655 ) ) ;
#71368 = CARTESIAN_POINT ( 'NONE',  ( -1.410761154855641575, -0.3162353388693409650, -0.4822834645669289433 ) ) ;
#71369 = CARTESIAN_POINT ( 'NONE',  ( -1.541994750656167090, 0.2952755905511811885, 0.1292274648535926551 ) ) ;
#71370 = ORIENTED_EDGE ( 'NONE', *, *, #35215, .T. ) ;
#71371 = CARTESIAN_POINT ( 'NONE',  ( -0.1070741851644056997, 0.3996062992125984925, -2.603018372703412631 ) ) ;
#71372 = CARTESIAN_POINT ( 'NONE',  ( -1.043307086614172041, -0.4536011799217367080, 0.2665933059059888421 ) ) ;
#71373 = CARTESIAN_POINT ( 'NONE',  ( 0.8727034120734912248, -0.3162353388693409650, -0.4822834645669289433 ) ) ;
#71374 = CARTESIAN_POINT ( 'NONE',  ( -1.167979002624671470, -0.3690944881889765550, -0.3153832671262227771 ) ) ;
#71375 = CARTESIAN_POINT ( 'NONE',  ( 0.1998031496062992463, 0.3460692066303959202, -1.638451443569554078 ) ) ;
#71376 = CARTESIAN_POINT ( 'NONE',  ( -1.102362204724408601, -0.1870078740157479769, 0.4822834645669291653 ) ) ;
#71377 = CARTESIAN_POINT ( 'NONE',  ( 0.9448818897637802916, -0.1870078740157480879, -0.4822834645669291653 ) ) ;
#71378 = CARTESIAN_POINT ( 'NONE',  ( 0.4265091863517067594, 0.2952755905511811885, 0.1292274648535926551 ) ) ;
#71379 = CARTESIAN_POINT ( 'NONE',  ( 1.614173228346457378, 0.2753471884572478157, 0.1372047244094478646 ) ) ;
#71380 = CARTESIAN_POINT ( 'NONE',  ( -1.699475065616797398, 0.1771653543307087630, 0.09757992244046791164 ) ) ;
#71382 = ADVANCED_FACE ( 'NONE', ( #81111 ), #3671, .T. ) ;
#71381 = CARTESIAN_POINT ( 'NONE',  ( 0.2925321140481931814, -0.2925321140481931259, -0.9625984251968502381 ) ) ;
#71383 = CARTESIAN_POINT ( 'NONE',  ( -0.1998031496062991907, -0.3460692066303959757, -1.167979002624671914 ) ) ;
#71384 = CARTESIAN_POINT ( 'NONE',  ( -9.674558042662121740E-17, 0.3949938075777409963, -0.6299212598425196763 ) ) ;
#71385 = CARTESIAN_POINT ( 'NONE',  ( 1.018747574612958173, 1.602034772339061330, 0.4702623840880322259 ) ) ;
#71386 = CARTESIAN_POINT ( 'NONE',  ( 0.7414698162729663755, 0.1771653543307087630, 0.09757992244046791164 ) ) ;
#71387 = CARTESIAN_POINT ( 'NONE',  ( 0.3149606299212603933, -0.1870078740157479769, 0.3641732283464567677 ) ) ;
#71388 = CARTESIAN_POINT ( 'NONE',  ( 0.1640419947506569498, -0.05778040916215522460, 0.4822834645669289988 ) ) ;
#71389 = CARTESIAN_POINT ( 'NONE',  ( 1.141732283464567566, 0.2952755905511811885, 0.000000000000000000 ) ) ;
#71390 = CARTESIAN_POINT ( 'NONE',  ( 0.1974969037888704704, 0.3420746716998660508, -1.795931758530183942 ) ) ;
#71391 = CARTESIAN_POINT ( 'NONE',  ( 0.2427821522309719648, -0.08942795157527998196, 0.3641732283464567121 ) ) ;
#71392 = CARTESIAN_POINT ( 'NONE',  ( -0.8333333333333323711, 0.2952755905511811885, 0.1292274648535926551 ) ) ;
#71393 = CARTESIAN_POINT ( 'NONE',  ( -1.646981627296586703, -0.05778040916215522460, 0.4822834645669289988 ) ) ;
#71394 = CARTESIAN_POINT ( 'NONE',  ( 0.6561679790026253567, -0.6046776061558809534, -0.2411417322834644161 ) ) ;
#71395 = CARTESIAN_POINT ( 'NONE',  ( -0.4724409448818899238, 0.1265901696524986686, -1.765091863517059823 ) ) ;
#71396 = CARTESIAN_POINT ( 'NONE',  ( 0.09156050430091122738, 0.3808816823641256732, -2.755905511811024056 ) ) ;
#71397 =( BOUNDED_CURVE ( )  B_SPLINE_CURVE ( 2, ( #35614, #73930, #35202, #9124, #15023, #54125, #41514, #15866, #61277, #79839, #3630, #28050, #60453 ),
 .UNSPECIFIED., .F., .F. ) 
 B_SPLINE_CURVE_WITH_KNOTS ( ( 3, 2, 2, 2, 2, 2, 3 ),
 ( 0.7642401855438917258, 0.7651515151515151381, 0.7689393939393939226, 0.7727272727272727071, 0.7765151515151514916, 0.7803030303030302761, 0.7812143599106537994 ),
 .UNSPECIFIED. ) 
 CURVE ( )  GEOMETRIC_REPRESENTATION_ITEM ( )  RATIONAL_B_SPLINE_CURVE ( ( 0.9875488213027523443, 0.9918020599134680371, 1.000000000000000000, 0.9659258262890683122, 1.000000000000000000, 0.9659258262890683122, 1.000000000000000000, 0.9659258262890683122, 1.000000000000000000, 0.9659258262890683122, 1.000000000000000000, 0.9918020599134671489, 0.9875488213027514561 ) ) 
 REPRESENTATION_ITEM ( '' )  );
#71398 = VERTEX_POINT ( 'NONE', #60493 ) ;
#71399 = ORIENTED_EDGE ( 'NONE', *, *, #27431, .F. ) ;
#71400 = CARTESIAN_POINT ( 'NONE',  ( -1.338582677165353729, -0.1870078740157480879, -0.4822834645669291653 ) ) ;
#71401 = CARTESIAN_POINT ( 'NONE',  ( -0.9973753280839886548, 0.2306618581243848609, 0.2411417322834645549 ) ) ;
#71403 = CARTESIAN_POINT ( 'NONE',  ( -0.8464566929133852113, 0.1660481256975885056, 0.3530559997133364547 ) ) ;
#71402 = CARTESIAN_POINT ( 'NONE',  ( -0.7677165354330699465, -0.4536011799217368745, -0.2665933059059886201 ) ) ;
#71404 = CARTESIAN_POINT ( 'NONE',  ( -0.3392501089628019439, 0.1958661417322832554, -2.153523991304775009 ) ) ;
#71405 = CARTESIAN_POINT ( 'NONE',  ( 1.348312163386739426, 0.2755905511811023723, 0.6195921248415929838 ) ) ;
#71406 = CARTESIAN_POINT ( 'NONE',  ( -1.574803149606298192, -0.1870078740157480601, -0.3641732283464567677 ) ) ;
#71407 = AXIS2_PLACEMENT_3D ( 'NONE', #35013, #66591, #81294 ) ;
#71408 = CARTESIAN_POINT ( 'NONE',  ( -1.423884514435694859, -0.3162353388693405765, 0.4822834645669290543 ) ) ;
#71409 = CARTESIAN_POINT ( 'NONE',  ( 0.1443569553805781891, -0.4281496062992124485, 0.4176697321401328655 ) ) ;
#71410 = CARTESIAN_POINT ( 'NONE',  ( -0.9514435695538050464, -0.05778040916215560624, -0.4822834645669293319 ) ) ;
#71411 = CARTESIAN_POINT ( 'NONE',  ( -0.1958661417322836718, 0.3392501089628017219, 0.05971128608923875758 ) ) ;
#71412 = CARTESIAN_POINT ( 'NONE',  ( 0.7677165354330716118, -0.5400638737290844871, 0.3530559997133364547 ) ) ;
#71413 = CARTESIAN_POINT ( 'NONE',  ( -0.3917322834645670104, -7.196005306013484475E-17, -1.606299212598425452 ) ) ;
#71414 = CARTESIAN_POINT ( 'NONE',  ( -0.6430446194225712953, -0.004921259842519870586, -0.3153832671262229437 ) ) ;
#71415 = ORIENTED_EDGE ( 'NONE', *, *, #69731, .F. ) ;
#71416 = CARTESIAN_POINT ( 'NONE',  ( -0.3949938075777409408, -0.1058382717557502933, -1.778215223097113107 ) ) ;
#71417 = ORIENTED_EDGE ( 'NONE', *, *, #64831, .T. ) ;
#71418 = CARTESIAN_POINT ( 'NONE',  ( -1.712598425196849572, 0.07958543189024085140, 0.2665933059059887866 ) ) ;
#71419 = CARTESIAN_POINT ( 'NONE',  ( -1.128608923884513837, -0.6046776061558807314, 0.2411417322834647770 ) ) ;
#71420 = CARTESIAN_POINT ( 'NONE',  ( -1.174540682414697335, -0.05778040916215522460, 0.4822834645669289988 ) ) ;
#71421 = CARTESIAN_POINT ( 'NONE',  ( 0.2925321140481932369, 0.2925321140481932369, -0.4527559055118109965 ) ) ;
#71422 = CARTESIAN_POINT ( 'NONE',  ( -0.9514435695538050464, -0.3162353388693405765, 0.4822834645669290543 ) ) ;
#71423 = CARTESIAN_POINT ( 'NONE',  ( -1.207349081364828880, 0.2306618581243847221, -0.2411417322834647770 ) ) ;
#71424 = CARTESIAN_POINT ( 'NONE',  ( -1.515748031496062076, -0.5400638737290844871, 0.3530559997133364547 ) ) ;
#71425 = CARTESIAN_POINT ( 'NONE',  ( -3.937007874015748143, 1.537401574803149984, -2.901595197523589142E-16 ) ) ;
#71426 = CARTESIAN_POINT ( 'NONE',  ( 0.2755905511811031494, 0.1771653543307087630, 0.000000000000000000 ) ) ;
#71427 = CARTESIAN_POINT ( 'NONE',  ( -0.01115035570243675701, 1.063087231634078922, -1.441367282966121488 ) ) ;
#71428 = CARTESIAN_POINT ( 'NONE',  ( 0.2867679344610365999, -0.2867679344610365444, -0.1830708661417323746 ) ) ;
#71429 = CARTESIAN_POINT ( 'NONE',  ( -0.1640419947506555343, -0.2845877964562159024, 0.3641732283464567677 ) ) ;
#71430 = CARTESIAN_POINT ( 'NONE',  ( -0.9842519685039360366, 0.2952755905511811885, 0.000000000000000000 ) ) ;
#71431 = CARTESIAN_POINT ( 'NONE',  ( 0.8267716535433077274, 0.2952755905511811885, 0.000000000000000000 ) ) ;
#71432 = CARTESIAN_POINT ( 'NONE',  ( -0.4199475065616791736, -0.6046776061558807314, 0.2411417322834647770 ) ) ;
#71433 = VERTEX_POINT ( 'NONE', #42365 ) ;
#71434 = ORIENTED_EDGE ( 'NONE', *, *, #78534, .T. ) ;
#71435 = CARTESIAN_POINT ( 'NONE',  ( -0.1070741851644056997, 0.3996062992125984925, -1.973097112860892510 ) ) ;
#71436 = CARTESIAN_POINT ( 'NONE',  ( -0.8595800524934373854, -0.05778040916215522460, 0.4822834645669289988 ) ) ;
#71437 = CARTESIAN_POINT ( 'NONE',  ( 1.259842519685040019, -0.1870078740157479769, 0.4822834645669291653 ) ) ;
#71438 = CARTESIAN_POINT ( 'NONE',  ( -1.397637795275589623, 0.07958543189024085140, 0.2665933059059887866 ) ) ;
#71439 = CARTESIAN_POINT ( 'NONE',  ( 0.3458507752293908943, 0.3458507752293908943, -0.7677165354330709457 ) ) ;
#71440 = DIRECTION ( 'NONE',  ( 0.000000000000000000, 1.000000000000000000, -0.000000000000000000 ) ) ;
#71441 = CARTESIAN_POINT ( 'NONE',  ( -0.1049643490035307020, 0.3917322834645669549, -0.4711286089238844177 ) ) ;
#71442 = CARTESIAN_POINT ( 'NONE',  ( 0.3917322834645670104, 2.398668435337828261E-17, -1.935039370078740273 ) ) ;
#71443 = CARTESIAN_POINT ( 'NONE',  ( -0.4265091863517051496, -0.6692913385826771977, 0.1292274648535927661 ) ) ;
#71444 = CARTESIAN_POINT ( 'NONE',  ( -1.627296587926508442, 0.1283753931104748280, 0.1820866141732283561 ) ) ;
#71445 = CARTESIAN_POINT ( 'NONE',  ( -0.7939632545931754048, -0.3162353388693405765, 0.4822834645669290543 ) ) ;
#71446 = CARTESIAN_POINT ( 'NONE',  ( -0.3996062992125984925, -0.1070741851644056858, 0.1922572178477689464 ) ) ;
#71448 = CARTESIAN_POINT ( 'NONE',  ( -0.3503937007874015630, -0.5120078740157480990, -0.01968503937007903132 ) ) ;
#71447 = CARTESIAN_POINT ( 'NONE',  ( -1.482939632545930975, -0.4281496062992127816, -0.4176697321401328100 ) ) ;
#71449 = CARTESIAN_POINT ( 'NONE',  ( -0.9317585301837263412, 0.05413385826771666132, 0.4176697321401328100 ) ) ;
#71450 = CARTESIAN_POINT ( 'NONE',  ( -0.4658792650918627265, -0.05778040916215522460, 0.4822834645669289988 ) ) ;
#71451 = CARTESIAN_POINT ( 'NONE',  ( -0.3420746716998660508, -0.1974969037888706924, -2.491469816272965598 ) ) ;
#71452 = CARTESIAN_POINT ( 'NONE',  ( 0.9120734908136489683, -0.5511811023622046335, 0.09757992244046803654 ) ) ;
#71453 = CARTESIAN_POINT ( 'NONE',  ( 0.2867679344610366554, 0.2867679344610366554, -0.06496062992125993529 ) ) ;
#71454 = CARTESIAN_POINT ( 'NONE',  ( 0.5643044619422579178, -0.004921259842519576551, 0.3153832671262227771 ) ) ;
#71455 = CARTESIAN_POINT ( 'NONE',  ( 1.240157480314961314, -0.4536011799217367080, 0.2665933059059888421 ) ) ;
#71456 = PRESENTATION_LAYER_ASSIGNMENT (  '', '', ( #56467 ) ) ;
#71457 = CARTESIAN_POINT ( 'NONE',  ( 1.574803149606299746, -0.1870078740157479769, 0.4822834645669291653 ) ) ;
#71458 = UNCERTAINTY_MEASURE_WITH_UNIT (LENGTH_MEASURE( 1.000000000000000082E-05 ), #23816, 'distance_accuracy_value', 'NONE');
#71459 = CARTESIAN_POINT ( 'NONE',  ( 0.1706036745406830368, -0.3690944881889765550, -0.3153832671262227771 ) ) ;
#71460 = CARTESIAN_POINT ( 'NONE',  ( -0.1958661417322834220, -0.3392501089628018884, -1.632545931758530244 ) ) ;
#71461 = CARTESIAN_POINT ( 'NONE',  ( -1.325459317585300889, 0.05413385826771666132, 0.4176697321401328100 ) ) ;
#71462 = CARTESIAN_POINT ( 'NONE',  ( 1.253280839895013710, -0.3162353388693405765, 0.4822834645669290543 ) ) ;
#71463 = CARTESIAN_POINT ( 'NONE',  ( 0.1265901696524990294, -0.4724409448818896462, 0.1528871391076115360 ) ) ;
#71464 = CARTESIAN_POINT ( 'NONE',  ( -0.5971128608923877978, -0.5511811023622048555, -0.09757992244046775898 ) ) ;
#71465 = CARTESIAN_POINT ( 'NONE',  ( -0.4133858267716528090, 0.1660481256975883391, -0.3530559997133364547 ) ) ;
#71466 = CARTESIAN_POINT ( 'NONE',  ( 0.3543307086614181922, -0.6692913385826771977, 8.415575281601705876E-17 ) ) ;
#71467 = DIRECTION ( 'NONE',  ( 0.000000000000000000, 1.000000000000000000, 0.000000000000000000 ) ) ;
#71468 = CARTESIAN_POINT ( 'NONE',  ( 0.9317585301837276734, -0.3690944881889763329, 0.3153832671262228327 ) ) ;
#71469 = CARTESIAN_POINT ( 'NONE',  ( 0.1443569553805781891, -0.3690944881889763329, 0.3153832671262228327 ) ) ;
#71470 = CARTESIAN_POINT ( 'NONE',  ( -0.2624671916010490880, -0.6046776061558807314, 0.2411417322834647770 ) ) ;
#71471 = CARTESIAN_POINT ( 'NONE',  ( -1.443569553805773564, -0.6046776061558807314, 0.2411417322834647770 ) ) ;
#71472 = CARTESIAN_POINT ( 'NONE',  ( -0.7217847769028863381, -0.3690944881889763329, 0.3153832671262228327 ) ) ;
#71473 = CARTESIAN_POINT ( 'NONE',  ( -2.556891446142596447, 2.729656600850901782, -0.5314960629921260393 ) ) ;
#71474 = CARTESIAN_POINT ( 'NONE',  ( 0.4724409448818904789, -0.1870078740157480879, -0.4822834645669291653 ) ) ;
#71475 = CARTESIAN_POINT ( 'NONE',  ( -0.9842519685039360366, 0.2952755905511811885, 0.000000000000000000 ) ) ;
#71476 = CARTESIAN_POINT ( 'NONE',  ( 0.3996062992125986035, -0.1070741851644052972, -1.290682414698162583 ) ) ;
#71477 = ADVANCED_FACE ( 'NONE', ( #68064 ), #16418, .F. ) ;
#71478 = CARTESIAN_POINT ( 'NONE',  ( 0.2867679344610365999, -0.2867679344610365444, -2.860236220472440749 ) ) ;
#71479 = CARTESIAN_POINT ( 'NONE',  ( 0.3674540682414705883, 0.1283753931104746893, -0.1820866141732285504 ) ) ;
#71480 = CARTESIAN_POINT ( 'NONE',  ( -0.9251968503937002541, -0.5400638737290845981, -0.3530559997133363437 ) ) ;
#71481 = CARTESIAN_POINT ( 'NONE',  ( -1.240157480314959759, -0.5400638737290845981, -0.3530559997133363437 ) ) ;
#71482 = CARTESIAN_POINT ( 'NONE',  ( -1.272965879265091305, -0.004921259842519870586, -0.3153832671262229437 ) ) ;
#71483 = CARTESIAN_POINT ( 'NONE',  ( 1.607611548556431069, -0.6692913385826773087, -0.1292274648535924053 ) ) ;
#71484 = CARTESIAN_POINT ( 'NONE',  ( -0.6824146981627288167, 0.1283753931104748280, 0.1820866141732283561 ) ) ;
#71485 = CARTESIAN_POINT ( 'NONE',  ( -0.7545931758530176614, 0.2066929133858267931, 0.1054918080437490802 ) ) ;
#71486 = CARTESIAN_POINT ( 'NONE',  ( 1.502624671916010790, -0.3162353388693409650, -0.4822834645669289433 ) ) ;
#71487 = CARTESIAN_POINT ( 'NONE',  ( 4.893765752498283924E-17, -0.3996062992125986035, 0.07874015748031494566 ) ) ;
#71488 = CARTESIAN_POINT ( 'NONE',  ( -0.1049643490035307158, 0.3917322834645670104, -2.522985195046931306 ) ) ;
#71489 = ORIENTED_EDGE ( 'NONE', *, *, #13980, .F. ) ;
#71490 = CARTESIAN_POINT ( 'NONE',  ( -3.861135848600278475, 2.745602313593968447, -0.5314960629921260393 ) ) ;
#71491 = CARTESIAN_POINT ( 'NONE',  ( 1.371391076115485719, -0.5511811023622048555, -0.09757992244046775898 ) ) ;
#71492 = CARTESIAN_POINT ( 'NONE',  ( -1.496062992125983815, -0.1870078740157480879, -0.4822834645669291653 ) ) ;
#71493 = CARTESIAN_POINT ( 'NONE',  ( 1.135170603674541256, 0.2952755905511811885, 0.1292274648535926551 ) ) ;
#71494 = CARTESIAN_POINT ( 'NONE',  ( 0.3392501089628018884, -0.1958661417322834220, -2.236876640419947826 ) ) ;
#71495 = FACE_OUTER_BOUND ( 'NONE', #39510, .T. ) ;
#71496 = CARTESIAN_POINT ( 'NONE',  ( 0.6036745406824154392, 0.2306618581243847221, -0.2411417322834647770 ) ) ;
#71497 = CARTESIAN_POINT ( 'NONE',  ( 0.1968503937007881344, -0.6692913385826771977, 8.415575281601705876E-17 ) ) ;
#71498 = CARTESIAN_POINT ( 'NONE',  ( 0.3134705033195891999, 1.179969644333642709, -3.924569983224646563 ) ) ;
#71499 = CARTESIAN_POINT ( 'NONE',  ( -0.3149606299212633909, 2.559055118110236560, 1.076935383196056417 ) ) ;
#71500 = CARTESIAN_POINT ( 'NONE',  ( 0.6364829396325465405, -0.08942795157527998196, 0.3641732283464567121 ) ) ;
#71501 = CARTESIAN_POINT ( 'NONE',  ( -0.3460692066303958092, -0.1998031496062994683, -1.312335958005249381 ) ) ;
#71502 = ORIENTED_EDGE ( 'NONE', *, *, #39374, .F. ) ;
#71503 = CARTESIAN_POINT ( 'NONE',  ( -0.1049643490035302301, -0.3917322834645671770, 0.08856336138351518505 ) ) ;
#71504 = EDGE_LOOP ( 'NONE', ( #17667, #79322, #62958, #1551 ) ) ;
#71505 = CARTESIAN_POINT ( 'NONE',  ( 0.05905511811023681640, 0.1660481256975883668, -0.3530559997133364547 ) ) ;
#71506 = PRODUCT_DEFINITION_SHAPE ( 'NONE', 'NONE',  #12068 ) ;
#71507 = CARTESIAN_POINT ( 'NONE',  ( 1.128608923884514947, 0.2306618581243848609, 0.2411417322834645549 ) ) ;
#71508 = CARTESIAN_POINT ( 'NONE',  ( 0.5380577427821529035, -0.4281496062992124485, 0.4176697321401328655 ) ) ;
#71509 = CARTESIAN_POINT ( 'NONE',  ( 1.266404199475066328, -0.3162353388693409650, -0.4822834645669289433 ) ) ;
#71510 = CARTESIAN_POINT ( 'NONE',  ( -0.4396325459317577122, -0.6692913385826773087, -0.1292274648535924053 ) ) ;
#71511 = CARTESIAN_POINT ( 'NONE',  ( 0.2230971128608929543, 0.05413385826771626580, -0.4176697321401330321 ) ) ;
#71512 = CARTESIAN_POINT ( 'NONE',  ( -1.607611548556429737, 0.2952755905511810774, -0.1292274648535930714 ) ) ;
#71513 = CIRCLE ( 'NONE', #76913, 0.09842519685039351207 ) ;
#71514 = CARTESIAN_POINT ( 'NONE',  ( 1.207349081364829990, -0.6046776061558809534, -0.2411417322834644161 ) ) ;
#71515 = CARTESIAN_POINT ( 'NONE',  ( 1.115485564304462551, -0.4281496062992127816, -0.4176697321401328100 ) ) ;
#71516 = CARTESIAN_POINT ( 'NONE',  ( 0.1958661417322836440, -0.3392501089628017219, -0.3989501312335957950 ) ) ;
#71517 = CARTESIAN_POINT ( 'NONE',  ( 0.2887139107611556010, 0.1283753931104746893, -0.1820866141732285504 ) ) ;
#71518 = ORIENTED_EDGE ( 'NONE', *, *, #69234, .F. ) ;
#71519 = CARTESIAN_POINT ( 'NONE',  ( -0.3949938075777409408, -0.1058382717557502933, -0.5183727034120736432 ) ) ;
#71520 = ORIENTED_EDGE ( 'NONE', *, *, #44498, .F. ) ;
#71521 = CARTESIAN_POINT ( 'NONE',  ( -0.4461942257217840213, 0.1283753931104748280, 0.1820866141732283561 ) ) ;
#71522 = CARTESIAN_POINT ( 'NONE',  ( -0.08530183727034056085, -0.3162353388693405765, 0.4822834645669290543 ) ) ;
#71523 = CARTESIAN_POINT ( 'NONE',  ( 2.822444539845176958, 1.119136672863569881, -0.2244172274865228744 ) ) ;
#71524 = CARTESIAN_POINT ( 'NONE',  ( 0.1837270341207354329, 0.2306618581243848609, 0.2411417322834645549 ) ) ;
#71525 = CARTESIAN_POINT ( 'NONE',  ( 0.1443569553805781891, -0.4281496062992124485, 0.4176697321401328655 ) ) ;
#71526 = CARTESIAN_POINT ( 'NONE',  ( -0.8333333333333323711, -0.6692913385826773087, -0.1292274648535924053 ) ) ;
#71527 = CARTESIAN_POINT ( 'NONE',  ( 1.522309711286089939, 0.1283753931104748280, 0.1820866141732283561 ) ) ;
#71528 = CARTESIAN_POINT ( 'NONE',  ( 0.000000000000000000, 0.000000000000000000, -2.755905511811024056 ) ) ;
#71529 = CARTESIAN_POINT ( 'NONE',  ( 0.000000000000000000, 2.145669291338582418, -0.3129921259842520787 ) ) ;
#71530 = CARTESIAN_POINT ( 'NONE',  ( 0.9120734908136489683, -0.5511811023622046335, 0.09757992244046803654 ) ) ;
#71531 = CARTESIAN_POINT ( 'NONE',  ( 0.3740157480314966754, -0.5400638737290844871, 0.3530559997133364547 ) ) ;
#71532 = CARTESIAN_POINT ( 'NONE',  ( 0.9514435695538062676, -0.3162353388693409650, -0.4822834645669289433 ) ) ;
#71533 = CARTESIAN_POINT ( 'NONE',  ( -0.3996062992125987146, 0.1070741851644051862, -1.450131233595800317 ) ) ;
#71534 = DIRECTION ( 'NONE',  ( 0.000000000000000000, 0.000000000000000000, -1.000000000000000000 ) ) ;
#71535 = CARTESIAN_POINT ( 'NONE',  ( 0.3996062992125985480, 2.446882876249141654E-17, -0.6673228346456693272 ) ) ;
#71536 = CARTESIAN_POINT ( 'NONE',  ( -0.3460692066303957537, -0.1998031496062994405, 0.02821522309711283621 ) ) ;
#71537 = CARTESIAN_POINT ( 'NONE',  ( -0.6561679790026240244, -0.6046776061558807314, 0.2411417322834647770 ) ) ;
#71538 = CARTESIAN_POINT ( 'NONE',  ( -0.3996062992125986035, -0.1070741851644056997, -2.723097112860892288 ) ) ;
#71539 =( BOUNDED_CURVE ( )  B_SPLINE_CURVE ( 1, ( #63481, #82845 ),
 .UNSPECIFIED., .F., .F. ) 
 B_SPLINE_CURVE_WITH_KNOTS ( ( 2, 2 ),
 ( 0.000000000000000000, 0.002000000000000001776 ),
 .UNSPECIFIED. ) 
 CURVE ( )  GEOMETRIC_REPRESENTATION_ITEM ( )  RATIONAL_B_SPLINE_CURVE ( ( 0.9875488213027530104, 0.9875488213027530104 ) ) 
 REPRESENTATION_ITEM ( '' )  );
#71540 = CARTESIAN_POINT ( 'NONE',  ( -0.3917322834645670104, -7.196005306013484475E-17, -2.171259842519685179 ) ) ;
#71541 = CARTESIAN_POINT ( 'NONE',  ( -1.174540682414697335, -0.08942795157527998196, 0.3641732283464567121 ) ) ;
#71542 = CARTESIAN_POINT ( 'NONE',  ( 1.115485564304462551, 0.05413385826771666132, 0.4176697321401328100 ) ) ;
#71543 = CARTESIAN_POINT ( 'NONE',  ( 0.9120734908136490793, 0.2952755905511810774, -0.1292274648535930714 ) ) ;
#71544 = CARTESIAN_POINT ( 'NONE',  ( -0.4396325459317577122, -0.5511811023622048555, -0.09757992244046775898 ) ) ;
#71545 = CARTESIAN_POINT ( 'NONE',  ( 0.2952755905511816326, -0.5400638737290844871, 0.3530559997133364547 ) ) ;
#71546 = CARTESIAN_POINT ( 'NONE',  ( -0.1265901696524986964, -0.4724409448818899238, -1.408792650918635259 ) ) ;
#71547 = CARTESIAN_POINT ( 'NONE',  ( 0.2230971128608932319, -0.3690944881889763329, 0.3153832671262228327 ) ) ;
#71548 = CARTESIAN_POINT ( 'NONE',  ( 0.03937007874015806264, 0.2952755905511811885, 0.000000000000000000 ) ) ;
#71549 = CARTESIAN_POINT ( 'NONE',  ( 0.3949938075777409408, -0.1058382717557499186, -1.448162729658792669 ) ) ;
#71550 = CARTESIAN_POINT ( 'NONE',  ( -1.174540682414697335, -0.3162353388693409650, -0.4822834645669289433 ) ) ;
#71551 = CARTESIAN_POINT ( 'NONE',  ( 0.4396325459317590445, -0.5511811023622046335, 0.09757992244046803654 ) ) ;
#71552 = CARTESIAN_POINT ( 'NONE',  ( 3.886287458032462006, 1.724409448818897905, -0.6299212598425196763 ) ) ;
#71553 = CARTESIAN_POINT ( 'NONE',  ( -0.6430446194225716283, -0.4281496062992124485, 0.4176697321401328655 ) ) ;
#71554 = CARTESIAN_POINT ( 'NONE',  ( -0.5052493438320203589, 0.1771653543307087075, -0.09757992244046823083 ) ) ;
#71555 = LINE ( 'NONE', #25671, #18417 ) ;
#71556 = CARTESIAN_POINT ( 'NONE',  ( -0.5380577427821514602, -0.4281496062992127816, -0.4176697321401328100 ) ) ;
#71557 = CARTESIAN_POINT ( 'NONE',  ( -0.5446194225721777693, -0.05778040916215522460, 0.4822834645669289988 ) ) ;
#71558 = CARTESIAN_POINT ( 'NONE',  ( 0.4724409448818904789, -0.1870078740157479769, 0.3641732283464567677 ) ) ;
#71559 = CARTESIAN_POINT ( 'NONE',  ( -0.1070741851644056997, 0.3996062992125984925, -2.288057742782152459 ) ) ;
#71560 = CARTESIAN_POINT ( 'NONE',  ( -0.1509186351706028884, -0.3162353388693409650, -0.4822834645669289433 ) ) ;
#71561 = CARTESIAN_POINT ( 'NONE',  ( -0.3392501089628019439, 0.1958661417322832554, -1.996043676344145146 ) ) ;
#71562 = CARTESIAN_POINT ( 'NONE',  ( 1.348312163386739426, 1.062992125984252079, 0.6402614161801758463 ) ) ;
#71563 = CARTESIAN_POINT ( 'NONE',  ( 0.9580052493438327987, -0.3690944881889765550, -0.3153832671262227771 ) ) ;
#71564 = CARTESIAN_POINT ( 'NONE',  ( 1.594488188976378673, 0.1660481256975885056, 0.3530559997133364547 ) ) ;
#71565 = CARTESIAN_POINT ( 'NONE',  ( -1.017060367454067249, -0.2845877964562161244, -0.3641732283464567121 ) ) ;
#71566 = CARTESIAN_POINT ( 'NONE',  ( -1.253280839895012377, -0.08942795157527998196, 0.3641732283464567121 ) ) ;
#71567 = CARTESIAN_POINT ( 'NONE',  ( -0.7939632545931750718, -0.05778040916215560624, -0.4822834645669293319 ) ) ;
#71568 = CARTESIAN_POINT ( 'NONE',  ( 0.03280839895013198948, 0.2952755905511811885, 0.1292274648535926551 ) ) ;
#71569 = CARTESIAN_POINT ( 'NONE',  ( 0.3674540682414705883, -0.5023911411419708095, 0.1820866141732285504 ) ) ;
#71570 = CARTESIAN_POINT ( 'NONE',  ( -0.2845351084527214525, 0.07967650482972132853, 5.860631297047876664 ) ) ;
#71571 = CARTESIAN_POINT ( 'NONE',  ( 0.8792650918635177559, -0.3690944881889765550, -0.3153832671262227771 ) ) ;
#71572 = CARTESIAN_POINT ( 'NONE',  ( 0.1706036745406830368, -0.4281496062992127816, -0.4176697321401328100 ) ) ;
#71573 = CARTESIAN_POINT ( 'NONE',  ( -0.1070741851644056997, 0.3996062992125984925, -0.08333333333333335646 ) ) ;
#71574 = CARTESIAN_POINT ( 'NONE',  ( -0.5183727034120726440, -0.6692913385826773087, -0.1292274648535924053 ) ) ;
#71575 = CARTESIAN_POINT ( 'NONE',  ( -0.3917322834645671215, 0.1049643490035301469, -1.219816272965879023 ) ) ;
#71576 = CARTESIAN_POINT ( 'NONE',  ( 1.338582677165355062, -0.1870078740157480601, -0.3641732283464567677 ) ) ;
#71577 = CARTESIAN_POINT ( 'NONE',  ( 0.3871391076115493490, -0.3162353388693405765, 0.4822834645669290543 ) ) ;
#71578 = CARTESIAN_POINT ( 'NONE',  ( 0.1115485564304470323, 0.2952755905511811885, 0.1292274648535926551 ) ) ;
#71579 = DIRECTION ( 'NONE',  ( -0.000000000000000000, 1.000000000000000000, -0.000000000000000000 ) ) ;
#71580 = CARTESIAN_POINT ( 'NONE',  ( 0.04593175853018440641, -0.5511811023622046335, 0.09757992244046803654 ) ) ;
#71581 = CARTESIAN_POINT ( 'NONE',  ( 0.9251968503937015864, 0.1660481256975883668, -0.3530559997133364547 ) ) ;
#71582 = CARTESIAN_POINT ( 'NONE',  ( -0.2230971128608915943, -0.3690944881889765550, -0.3153832671262227771 ) ) ;
#71583 = CARTESIAN_POINT ( 'NONE',  ( -0.8530183727034112984, 0.05413385826771666132, 0.4176697321401328100 ) ) ;
#71584 = LINE ( 'NONE', #51359, #15227 ) ;
#71585 = CARTESIAN_POINT ( 'NONE',  ( -0.3412073490813641308, -0.6046776061558807314, 0.2411417322834647770 ) ) ;
#71586 = ORIENTED_EDGE ( 'NONE', *, *, #44453, .F. ) ;
#71587 = CARTESIAN_POINT ( 'NONE',  ( -1.049868766404198794, -0.6046776061558807314, 0.2411417322834647770 ) ) ;
#71588 = CARTESIAN_POINT ( 'NONE',  ( -0.6102362204724400829, 0.07958543189024085140, 0.2665933059059887866 ) ) ;
#71589 = CARTESIAN_POINT ( 'NONE',  ( -0.03280839895013062252, -0.6692913385826771977, 0.1292274648535927661 ) ) ;
#71590 = CARTESIAN_POINT ( 'NONE',  ( -1.286089238845143479, -0.6046776061558807314, 0.2411417322834647770 ) ) ;
#71591 = CARTESIAN_POINT ( 'NONE',  ( -0.5643044619422565855, -0.4281496062992124485, 0.4176697321401328655 ) ) ;
#71592 = CARTESIAN_POINT ( 'NONE',  ( 2.795275590551181910, 1.535433070866142335, 0.000000000000000000 ) ) ;
#71594 = CARTESIAN_POINT ( 'NONE',  ( 0.8595800524934390507, -0.05778040916215560624, -0.4822834645669293319 ) ) ;
#71593 = CARTESIAN_POINT ( 'NONE',  ( 1.646981627296588035, -0.3162353388693405765, 0.4822834645669290543 ) ) ;
#71595 = CARTESIAN_POINT ( 'NONE',  ( 1.082677165354331228, 0.1660481256975883668, -0.3530559997133364547 ) ) ;
#71596 = CARTESIAN_POINT ( 'NONE',  ( -0.1049643490035307020, 0.3917322834645669549, -2.360892388451443669 ) ) ;
#71597 = DIRECTION ( 'NONE',  ( 0.000000000000000000, 8.673617379884024625E-16, 1.000000000000000000 ) ) ;
#71598 = CARTESIAN_POINT ( 'NONE',  ( -1.253280839895012377, -0.05778040916215522460, 0.4822834645669289988 ) ) ;
#71599 = CARTESIAN_POINT ( 'NONE',  ( -0.1265901696524986964, -0.4724409448818899238, -0.8595800524934383846 ) ) ;
#71600 = CARTESIAN_POINT ( 'NONE',  ( -0.1998031496062991907, -0.3460692066303959757, 0.09186351706036742504 ) ) ;
#71601 = ORIENTED_EDGE ( 'NONE', *, *, #72820, .T. ) ;
#71602 = CARTESIAN_POINT ( 'NONE',  ( 0.07874015748031558404, -0.1870078740157479769, 0.3641732283464567677 ) ) ;
#71603 = CARTESIAN_POINT ( 'NONE',  ( -0.1958661417322834220, -0.3392501089628018884, -1.947506561679789971 ) ) ;
#71604 = ORIENTED_EDGE ( 'NONE', *, *, #632, .T. ) ;
#71605 = CARTESIAN_POINT ( 'NONE',  ( 0.4199475065616803948, -0.6046776061558809534, -0.2411417322834644161 ) ) ;
#71606 = CARTESIAN_POINT ( 'NONE',  ( -0.09842519685039295696, 0.1660481256975883668, -0.3530559997133364547 ) ) ;
#71607 = CARTESIAN_POINT ( 'NONE',  ( -0.7349081364829387342, -0.6046776061558807314, 0.2411417322834647770 ) ) ;
#71608 = DIRECTION ( 'NONE',  ( 1.000000000000000000, 0.000000000000000000, -0.000000000000000000 ) ) ;
#71609 = CARTESIAN_POINT ( 'NONE',  ( -0.7217847769028863381, -0.3690944881889763329, 0.3153832671262228327 ) ) ;
#71610 = CARTESIAN_POINT ( 'NONE',  ( 0.3608923884514443348, 0.2952755905511810219, -0.1292274648535930437 ) ) ;
#71611 = CARTESIAN_POINT ( 'NONE',  ( 0.7414698162729663755, 0.2952755905511811885, 0.1292274648535926551 ) ) ;
#71612 = EDGE_CURVE ( 'NONE', #72444, #39742, #42379, .T. ) ;
#71613 = CARTESIAN_POINT ( 'NONE',  ( 0.8267716535433077274, 0.1771653543307087630, 0.000000000000000000 ) ) ;
#71614 = CARTESIAN_POINT ( 'NONE',  ( -0.4461942257217840213, -0.6046776061558809534, -0.2411417322834644161 ) ) ;
#71615 = CARTESIAN_POINT ( 'NONE',  ( 0.1958661417322836162, -0.3392501089628018329, -1.116778584480628389 ) ) ;
#71616 = CARTESIAN_POINT ( 'NONE',  ( -0.9317585301837263412, -0.4281496062992127816, -0.4176697321401328100 ) ) ;
#71617 = DIRECTION ( 'NONE',  ( 0.000000000000000000, -1.000000000000000000, 0.000000000000000000 ) ) ;
#71618 = CARTESIAN_POINT ( 'NONE',  ( 1.528871391076116026, 0.2952755905511811885, 0.1292274648535926551 ) ) ;
#71619 = FACE_OUTER_BOUND ( 'NONE', #30529, .T. ) ;
#71620 = ORIENTED_EDGE ( 'NONE', *, *, #21343, .F. ) ;
#71621 = CARTESIAN_POINT ( 'NONE',  ( -0.2867679344610367109, 0.2867679344610365444, -2.378628239666354283 ) ) ;
#71622 = CARTESIAN_POINT ( 'NONE',  ( 0.06561679790026316017, -0.4281496062992124485, 0.4176697321401328655 ) ) ;
#71623 = ORIENTED_EDGE ( 'NONE', *, *, #46286, .T. ) ;
#71624 = CARTESIAN_POINT ( 'NONE',  ( -0.6758530183727028406, -0.6692913385826773087, -0.1292274648535924053 ) ) ;
#71625 = CARTESIAN_POINT ( 'NONE',  ( 1.194225721784777594, -0.4281496062992127816, -0.4176697321401328100 ) ) ;
#71626 = CARTESIAN_POINT ( 'NONE',  ( 1.443569553805774897, 0.2306618581243848609, 0.2411417322834645549 ) ) ;
#71627 = CARTESIAN_POINT ( 'NONE',  ( 0.1706036745406830368, 0.05413385826771666132, 0.4176697321401328100 ) ) ;
#71628 = AXIS2_PLACEMENT_3D ( 'NONE', #81257, #36611, #62290 ) ;
#71629 = CARTESIAN_POINT ( 'NONE',  ( -0.4068241469816264999, -0.4281496062992124485, 0.4176697321401328655 ) ) ;
#71630 = CARTESIAN_POINT ( 'NONE',  ( -0.3917322834645670104, -7.196005306013484475E-17, -1.856299212598425230 ) ) ;
#71631 = CARTESIAN_POINT ( 'NONE',  ( -1.056430446194224881, 0.2952755905511810774, -0.1292274648535930714 ) ) ;
#71632 = CARTESIAN_POINT ( 'NONE',  ( -0.1706036745406816491, 0.05413385826771626580, -0.4176697321401330321 ) ) ;
#71633 = CARTESIAN_POINT ( 'NONE',  ( -0.03937007874015669567, 0.1771653543307087630, 0.000000000000000000 ) ) ;
#71634 = CARTESIAN_POINT ( 'NONE',  ( 1.561679790026247350, 0.05413385826771626580, -0.4176697321401330321 ) ) ;
#71635 = CARTESIAN_POINT ( 'NONE',  ( 1.456692913385827515, -0.6692913385826771977, 8.415575281601705876E-17 ) ) ;
#71636 = CARTESIAN_POINT ( 'NONE',  ( -0.6561679790026240244, -0.6046776061558807314, 0.2411417322834647770 ) ) ;
#71637 = CARTESIAN_POINT ( 'NONE',  ( -0.5314960629921395840, 2.748002881374839834, 3.856579543051779524 ) ) ;
#71638 = CARTESIAN_POINT ( 'NONE',  ( 1.023622047244095112, -0.1870078740157480879, -0.4822834645669291653 ) ) ;
#71639 = FACE_OUTER_BOUND ( 'NONE', #44663, .T. ) ;
#71640 = ADVANCED_FACE ( 'NONE', ( #74813 ), #10825, .F. ) ;
#71641 = VERTEX_POINT ( 'NONE', #62160 ) ;
#71642 = CARTESIAN_POINT ( 'NONE',  ( 0.3674540682414705883, -0.6046776061558807314, 0.2411417322834647770 ) ) ;
#71643 = CARTESIAN_POINT ( 'NONE',  ( -0.1706036745406816491, -0.3690944881889763329, 0.3153832671262228327 ) ) ;
#71645 = CARTESIAN_POINT ( 'NONE',  ( -0.8989501312335947958, 0.2066929133858267098, -0.1054918080437494132 ) ) ;
#71644 = CARTESIAN_POINT ( 'NONE',  ( 0.9055118110236227702, 0.1771653543307087630, 0.000000000000000000 ) ) ;
#71646 = CARTESIAN_POINT ( 'NONE',  ( 0.2362204724409449064, 0.4091458600556404646, -0.2211286089238845010 ) ) ;
#71647 = CARTESIAN_POINT ( 'NONE',  ( 0.9881811337016640495, 2.755905511811024056, -0.5314960629921260393 ) ) ;
#71648 = CARTESIAN_POINT ( 'NONE',  ( 1.351706036745407458, -0.4281496062992127816, -0.4176697321401328100 ) ) ;
#71649 = CARTESIAN_POINT ( 'NONE',  ( 0.1058382717557499880, 0.3949938075777409408, -0.07020997375328083545 ) ) ;
#71650 = CARTESIAN_POINT ( 'NONE',  ( 0.03937007874015806264, 0.2952755905511811885, 0.000000000000000000 ) ) ;
#71651 = CARTESIAN_POINT ( 'NONE',  ( -1.653543307086613234, -0.1870078740157479769, 0.4822834645669291653 ) ) ;
#71652 = CARTESIAN_POINT ( 'NONE',  ( -1.633858267716534529, -0.5400638737290845981, -0.3530559997133363437 ) ) ;
#71653 = CARTESIAN_POINT ( 'NONE',  ( -0.2559055118110230564, 0.1660481256975883668, -0.3530559997133364547 ) ) ;
#71654 = CARTESIAN_POINT ( 'NONE',  ( 0.1974969037888706092, -0.3420746716998660508, -0.1686351706036745279 ) ) ;
#71655 = CARTESIAN_POINT ( 'NONE',  ( -1.614173228346455824, 0.1771653543307087630, 0.000000000000000000 ) ) ;
#71656 = CARTESIAN_POINT ( 'NONE',  ( 0.4330708661417329575, -0.6692913385826771977, 8.415575281601705876E-17 ) ) ;
#71657 = CARTESIAN_POINT ( 'NONE',  ( 0.9776902887139113929, -0.5511811023622048555, -0.09757992244046775898 ) ) ;
#71658 = CARTESIAN_POINT ( 'NONE',  ( -0.01158586635040114929, 0.02791078216816508459, -0.4328096321851889194 ) ) ;
#71659 = EDGE_CURVE ( 'NONE', #25547, #40163, #41971, .T. ) ;
#71660 = CARTESIAN_POINT ( 'NONE',  ( 0.3412073490813655186, -0.5023911411419708095, -0.1820866141732282451 ) ) ;
#71661 = CARTESIAN_POINT ( 'NONE',  ( -1.305774278215222184, 0.2952755905511811885, 0.1292274648535926551 ) ) ;
#71662 = CARTESIAN_POINT ( 'NONE',  ( 0.1070741851644054776, -0.3996062992125984925, -0.7919947506561679784 ) ) ;
#71663 = CARTESIAN_POINT ( 'NONE',  ( 1.351706036745407680, 0.05413385826771666132, 0.4176697321401328100 ) ) ;
#71664 = CARTESIAN_POINT ( 'NONE',  ( -0.3392501089628019995, 0.1958661417322832277, -0.6482939632545930975 ) ) ;
#71666 = CARTESIAN_POINT ( 'NONE',  ( 1.392101432702376629, 0.2755905511811023723, 0.9507481457704560768 ) ) ;
#71665 = CARTESIAN_POINT ( 'NONE',  ( 0.8858267716535438430, 0.1660481256975885056, 0.3530559997133364547 ) ) ;
#71667 = CARTESIAN_POINT ( 'NONE',  ( -0.3495983942378627640, 0.3045330818767438275, -0.01888973282054017683 ) ) ;
#71668 = CARTESIAN_POINT ( 'NONE',  ( 0.6036745406824153282, -0.5023911411419708095, 0.1820866141732285504 ) ) ;
#71669 = CARTESIAN_POINT ( 'NONE',  ( 0.6496062992125991586, -0.5400638737290845981, -0.3530559997133363437 ) ) ;
#71670 = DIRECTION ( 'NONE',  ( 0.000000000000000000, 0.000000000000000000, -1.000000000000000000 ) ) ;
#71671 = CARTESIAN_POINT ( 'NONE',  ( -0.7545931758530177724, 0.1771653543307087630, 0.09757992244046791164 ) ) ;
#71672 = CARTESIAN_POINT ( 'NONE',  ( -0.8661417322834640276, -0.1870078740157480879, -0.4822834645669291653 ) ) ;
#71673 = AXIS2_PLACEMENT_3D ( 'NONE', #76440, #24663, #70521 ) ;
#71674 = CARTESIAN_POINT ( 'NONE',  ( -1.541994750656167090, 0.2952755905511811885, 0.1292274648535926551 ) ) ;
#71675 = CARTESIAN_POINT ( 'NONE',  ( 0.8858267716535438430, 0.1660481256975885056, 0.3530559997133364547 ) ) ;
#71676 = CARTESIAN_POINT ( 'NONE',  ( 1.496062992125985147, -0.1870078740157479769, 0.4822834645669291653 ) ) ;
#71677 = CARTESIAN_POINT ( 'NONE',  ( 1.038339513766209476, 1.326687365142510178, -0.4253272082265546761 ) ) ;
#71678 = CARTESIAN_POINT ( 'NONE',  ( 0.9842519685039375910, 0.2952755905511811885, 0.000000000000000000 ) ) ;
#71679 = CARTESIAN_POINT ( 'NONE',  ( 0.3996062992125984925, 0.1070741851644054637, 0.1135170603674540285 ) ) ;
#71680 = CARTESIAN_POINT ( 'NONE',  ( 1.679790026246720025, 0.2306618581243848609, 0.2411417322834645549 ) ) ;
#71681 = CARTESIAN_POINT ( 'NONE',  ( 1.450131233595801428, -0.6692913385826773087, -0.1292274648535924053 ) ) ;
#71682 = CARTESIAN_POINT ( 'NONE',  ( -1.489501312335957062, -0.2845877964562161244, -0.3641732283464567121 ) ) ;
#71683 = CARTESIAN_POINT ( 'NONE',  ( 1.345144356955381593, -0.08942795157527998196, 0.3641732283464567121 ) ) ;
#71684 = CARTESIAN_POINT ( 'NONE',  ( -1.240157480314959759, -0.4536011799217368745, -0.2665933059059886201 ) ) ;
#71685 = CARTESIAN_POINT ( 'NONE',  ( -0.6233595800524928121, -0.2845877964562161244, -0.3641732283464567121 ) ) ;
#71686 = DIRECTION ( 'NONE',  ( -0.000000000000000000, 0.000000000000000000, -1.000000000000000000 ) ) ;
#71687 = CARTESIAN_POINT ( 'NONE',  ( 0.7349081364829402885, -0.5023911411419708095, -0.1820866141732282451 ) ) ;
#71688 = AXIS2_PLACEMENT_3D ( 'NONE', #41863, #54069, #16632 ) ;
#71689 = CARTESIAN_POINT ( 'NONE',  ( 0.7283464566929143125, 0.1660481256975885056, 0.3530559997133364547 ) ) ;
#71690 = CARTESIAN_POINT ( 'NONE',  ( 0.9711286089238851948, 0.2306618581243848609, 0.2411417322834645549 ) ) ;
#71691 = CARTESIAN_POINT ( 'NONE',  ( -0.1312335958005241554, -0.6046776061558809534, -0.2411417322834644161 ) ) ;
#71692 = CARTESIAN_POINT ( 'NONE',  ( 0.7545931758530188826, -0.5511811023622046335, 0.09757992244046803654 ) ) ;
#71693 = CARTESIAN_POINT ( 'NONE',  ( 1.194225721784777594, -0.4281496062992127816, -0.4176697321401328100 ) ) ;
#71694 = CARTESIAN_POINT ( 'NONE',  ( -0.2234477481026881651, 0.004960608223778821026, 0.3437734562760189072 ) ) ;
#71695 = CARTESIAN_POINT ( 'NONE',  ( -0.5380577427821514602, -0.4281496062992127816, -0.4176697321401328100 ) ) ;
#71696 = CARTESIAN_POINT ( 'NONE',  ( 0.3460692066303959202, 0.1998031496062993295, -0.9186351706036745002 ) ) ;
#71697 = CYLINDRICAL_SURFACE ( 'NONE', #552, 1.181102362204724310 ) ;
#71698 = CARTESIAN_POINT ( 'NONE',  ( 0.2034120734908142214, 0.2952755905511810774, -0.1292274648535930714 ) ) ;
#71699 = CARTESIAN_POINT ( 'NONE',  ( -0.4002624671916004129, -0.3162353388693405765, 0.4822834645669290543 ) ) ;
#71700 = CARTESIAN_POINT ( 'NONE',  ( -0.1968503937007867743, -0.6692913385826771977, 8.415575281601705876E-17 ) ) ;
#71701 = CARTESIAN_POINT ( 'NONE',  ( -0.3996062992125986035, -7.340648628747425578E-17, -2.559055118110236560 ) ) ;
#71702 = CARTESIAN_POINT ( 'NONE',  ( 4.837279021331060870E-17, -0.3949938075777409963, -2.125984251968503713 ) ) ;
#71703 = CARTESIAN_POINT ( 'NONE',  ( 0.2867679344610365999, 0.2867679344610365999, -0.4448818897637794589 ) ) ;
#71704 = CARTESIAN_POINT ( 'NONE',  ( 0.2362235781738431795, -0.1771612133531280942, 5.714029142339813738 ) ) ;
#71705 = CARTESIAN_POINT ( 'NONE',  ( -0.1958661417322834220, -0.3392501089628018884, -1.002624671916010568 ) ) ;
#71706 = CARTESIAN_POINT ( 'NONE',  ( -0.9055118110236215490, 0.1771653543307087630, 0.000000000000000000 ) ) ;
#71707 = CARTESIAN_POINT ( 'NONE',  ( 0.3392501089628018329, 0.1958661417322835607, -1.225721784776902634 ) ) ;
#71708 = CARTESIAN_POINT ( 'NONE',  ( -0.9973753280839886548, -0.6046776061558809534, -0.2411417322834644161 ) ) ;
#71709 = CARTESIAN_POINT ( 'NONE',  ( -0.3917322834645669549, -7.196005306013483243E-17, 0.03807705856399132283 ) ) ;
#71710 = CARTESIAN_POINT ( 'NONE',  ( 0.3346456692913393205, -0.5400638737290845981, -0.3530559997133363437 ) ) ;
#71711 = CARTESIAN_POINT ( 'NONE',  ( -0.6233595800524928121, -0.08942795157527998196, 0.3641732283464567121 ) ) ;
#71712 = CARTESIAN_POINT ( 'NONE',  ( 1.089238845144357537, -0.4281496062992124485, 0.4176697321401328655 ) ) ;
#71713 = CARTESIAN_POINT ( 'NONE',  ( 0.2034120734908142214, 0.2952755905511810774, -0.1292274648535930714 ) ) ;
#71714 = CARTESIAN_POINT ( 'NONE',  ( -0.3458507752293909498, 0.3458507752293908388, -0.09645669291338582196 ) ) ;
#71715 = CARTESIAN_POINT ( 'NONE',  ( -0.2925321140481930704, -0.2925321140481933480, -2.736220472440944018 ) ) ;
#71716 = CARTESIAN_POINT ( 'NONE',  ( 0.3392501089628018329, 0.1958661417322835607, -1.230334276411760186 ) ) ;
#71717 = CARTESIAN_POINT ( 'NONE',  ( 1.391076115485564868, 0.2306618581243847221, -0.2411417322834647770 ) ) ;
#71718 = CARTESIAN_POINT ( 'NONE',  ( 0.5052493438320215802, 0.2952755905511811885, 0.1292274648535926551 ) ) ;
#71719 = CARTESIAN_POINT ( 'NONE',  ( 0.03280839895013198948, 0.2952755905511811885, 0.1292274648535926551 ) ) ;
#71720 = CARTESIAN_POINT ( 'NONE',  ( 1.463254593175853824, 0.2952755905511810774, -0.1292274648535930714 ) ) ;
#71721 = CARTESIAN_POINT ( 'NONE',  ( 0.7545931758530189937, 0.2952755905511810774, -0.1292274648535930714 ) ) ;
#71722 = CARTESIAN_POINT ( 'NONE',  ( 0.2867679344610365999, -0.2867679344610365444, -0.4980314960629922405 ) ) ;
#71723 = CARTESIAN_POINT ( 'NONE',  ( 0.2034120734908142214, 0.2952755905511810774, -0.1292274648535930714 ) ) ;
#71724 = CARTESIAN_POINT ( 'NONE',  ( 1.076115485564305141, 0.2306618581243847221, -0.2411417322834647770 ) ) ;
#71725 = CARTESIAN_POINT ( 'NONE',  ( 0.3412073490813655186, -0.6046776061558809534, -0.2411417322834644161 ) ) ;
#71726 = CIRCLE ( 'NONE', #34058, 1.220472440944881942 ) ;
#71727 = CARTESIAN_POINT ( 'NONE',  ( 0.9514435695538062676, -0.2845877964562161244, -0.3641732283464567121 ) ) ;
#71728 = CARTESIAN_POINT ( 'NONE',  ( -0.8070866141732276899, -0.5400638737290844871, 0.3530559997133364547 ) ) ;
#71729 = CARTESIAN_POINT ( 'NONE',  ( -1.240157480314959759, 0.1660481256975885056, 0.3530559997133364547 ) ) ;
#71730 = CARTESIAN_POINT ( 'NONE',  ( 0.6430446194225728496, 0.05413385826771666132, 0.4176697321401328100 ) ) ;
#71731 = CARTESIAN_POINT ( 'NONE',  ( 0.3692639355350713637, -0.1324727617106734590, -1.929133858267717549 ) ) ;
#71732 = CARTESIAN_POINT ( 'NONE',  ( 0.3917322834645670104, 2.398668435337828261E-17, -1.842519685039370136 ) ) ;
#71733 = EDGE_LOOP ( 'NONE', ( #67807, #78668, #18900, #50590 ) ) ;
#71734 = CARTESIAN_POINT ( 'NONE',  ( -0.3996062992125987146, 0.1070741851644051862, 0.1246719160104986790 ) ) ;
#71735 = ORIENTED_EDGE ( 'NONE', *, *, #58451, .T. ) ;
#71736 = CARTESIAN_POINT ( 'NONE',  ( 1.607611548556431069, -0.6692913385826773087, -0.1292274648535924053 ) ) ;
#71737 = CARTESIAN_POINT ( 'NONE',  ( 0.8136482939632553313, 0.1283753931104748280, 0.1820866141732283561 ) ) ;
#71738 = CARTESIAN_POINT ( 'NONE',  ( 1.080276388343102000E-18, 0.000000000000000000, 0.000000000000000000 ) ) ;
#71739 = DIRECTION ( 'NONE',  ( -0.000000000000000000, -0.000000000000000000, 1.000000000000000000 ) ) ;
#71740 = CARTESIAN_POINT ( 'NONE',  ( -0.4498537592782897998, 0.000000000000000000, 2.118110236220472675 ) ) ;
#71741 = CARTESIAN_POINT ( 'NONE',  ( 0.3392501089628018884, -0.1958661417322834220, -0.9770341207349081403 ) ) ;
#71742 = AXIS2_PLACEMENT_3D ( 'NONE', #15732, #68316, #55650 ) ;
#71743 = CARTESIAN_POINT ( 'NONE',  ( -1.227034120734907141, -0.5511811023622048555, -0.09757992244046775898 ) ) ;
#71744 = CARTESIAN_POINT ( 'NONE',  ( 1.535433070866142335, -0.6692913385826771977, 8.415575281601705876E-17 ) ) ;
#71745 = CARTESIAN_POINT ( 'NONE',  ( 0.4744094488189112835, 1.537401574803149984, -3.908320185825791881 ) ) ;
#71746 = CARTESIAN_POINT ( 'NONE',  ( -0.1509186351706028884, -0.05778040916215522460, 0.4822834645669289988 ) ) ;
#71747 = CARTESIAN_POINT ( 'NONE',  ( 1.108923884514436242, -0.05778040916215522460, 0.4822834645669289988 ) ) ;
#71748 = ORIENTED_EDGE ( 'NONE', *, *, #47017, .F. ) ;
#71749 = CARTESIAN_POINT ( 'NONE',  ( -1.653543307086613234, -0.1870078740157480879, -0.4822834645669291653 ) ) ;
#71750 = CARTESIAN_POINT ( 'NONE',  ( 0.5157744752565104340, 1.509207849855103811, 0.5177606540819029712 ) ) ;
#71751 = LINE ( 'NONE', #18742, #17019 ) ;
#71752 = CARTESIAN_POINT ( 'NONE',  ( -0.03443470937339728616, 0.000000000000000000, -1.753551325310622078 ) ) ;
#71753 = CARTESIAN_POINT ( 'NONE',  ( -0.9055118110236215490, -0.5511811023622047445, 6.969142054262312111E-17 ) ) ;
#71754 = CARTESIAN_POINT ( 'NONE',  ( -1.502624671916009680, -0.3162353388693405765, 0.4822834645669290543 ) ) ;
#71755 = CARTESIAN_POINT ( 'NONE',  ( 0.4461942257217856311, 0.2306618581243847221, -0.2411417322834647770 ) ) ;
#71756 = EDGE_LOOP ( 'NONE', ( #81795, #15604, #68096, #31853, #30403, #50285, #53718, #45063, #18403, #83165, #60237, #38586, #69110, #6405 ) ) ;
#71758 = LINE ( 'NONE', #62436, #27787 ) ;
#71757 = DIRECTION ( 'NONE',  ( 1.000000000000000000, -0.000000000000000000, -0.000000000000000000 ) ) ;
#71759 = ADVANCED_FACE ( 'NONE', ( #4501 ), #5330, .F. ) ;
#71760 = CARTESIAN_POINT ( 'NONE',  ( 0.7283464566929143125, 0.1660481256975885056, 0.3530559997133364547 ) ) ;
#71761 = CARTESIAN_POINT ( 'NONE',  ( -1.541994750656167090, 0.2952755905511811885, 0.1292274648535926551 ) ) ;
#71762 = CARTESIAN_POINT ( 'NONE',  ( 0.1049643490035304522, -0.3917322834645668994, -0.9527365897299718833 ) ) ;
#71763 = CARTESIAN_POINT ( 'NONE',  ( -1.010498687664041384, -0.3690944881889765550, -0.3153832671262227771 ) ) ;
#71764 = CARTESIAN_POINT ( 'NONE',  ( 1.679790026246720025, 0.2306618581243848609, 0.2411417322834645549 ) ) ;
#71765 = CARTESIAN_POINT ( 'NONE',  ( 0.4849061582275019378, 2.793565526369266028, -0.4921425059946357705 ) ) ;
#71767 = EDGE_CURVE ( 'NONE', #25114, #54726, #33073, .T. ) ;
#71766 = CARTESIAN_POINT ( 'NONE',  ( 0.5249343832021003964, 0.2306618581243847221, -0.2411417322834647770 ) ) ;
#71768 = CARTESIAN_POINT ( 'NONE',  ( -1.043307086614172041, -0.4536011799217367080, 0.2665933059059888421 ) ) ;
#71769 = CARTESIAN_POINT ( 'NONE',  ( 0.006561679790026889343, -0.08942795157527998196, 0.3641732283464567121 ) ) ;
#71770 = CARTESIAN_POINT ( 'NONE',  ( -0.4461942257217840213, 0.2306618581243848609, 0.2411417322834645549 ) ) ;
#71771 = CARTESIAN_POINT ( 'NONE',  ( -1.174540682414697335, -0.08942795157527998196, 0.3641732283464567121 ) ) ;
#71772 = CARTESIAN_POINT ( 'NONE',  ( -0.3917322834645670659, -7.196005306013484475E-17, -0.1935888695876134269 ) ) ;
#71773 = CARTESIAN_POINT ( 'NONE',  ( 0.8661417322834652488, -0.1870078740157480879, -0.4822834645669291653 ) ) ;
#71774 = CARTESIAN_POINT ( 'NONE',  ( -1.358267716535432434, -0.5400638737290844871, 0.3530559997133364547 ) ) ;
#71775 = CARTESIAN_POINT ( 'NONE',  ( -0.4091458600556405756, 0.2362204724409446288, -1.362860892388451539 ) ) ;
#71776 = CARTESIAN_POINT ( 'NONE',  ( -0.9120734908136475250, 0.2952755905511811885, 0.1292274648535926551 ) ) ;
#71777 = CARTESIAN_POINT ( 'NONE',  ( -0.2624671916010490880, 0.1283753931104746893, -0.1820866141732285504 ) ) ;
#71778 = CARTESIAN_POINT ( 'NONE',  ( -1.305774278215222184, 0.2952755905511811885, 0.1292274648535926551 ) ) ;
#71779 = CARTESIAN_POINT ( 'NONE',  ( 0.7611548556430454138, 0.1283753931104746893, -0.1820866141732285504 ) ) ;
#71780 = CARTESIAN_POINT ( 'NONE',  ( -0.3543307086614165824, -0.5511811023622047445, 6.969142054262312111E-17 ) ) ;
#71781 = CARTESIAN_POINT ( 'NONE',  ( -1.062992125984250968, 0.2952755905511811885, 0.000000000000000000 ) ) ;
#71782 = CARTESIAN_POINT ( 'NONE',  ( -0.9973753280839886548, -0.6046776061558809534, -0.2411417322834644161 ) ) ;
#71783 = CARTESIAN_POINT ( 'NONE',  ( -1.476377952755905110, 0.1660481256975885056, 0.3530559997133364547 ) ) ;
#71784 = CYLINDRICAL_SURFACE ( 'NONE', #46112, 0.2165354330708660069 ) ;
#71785 = CARTESIAN_POINT ( 'NONE',  ( 1.161417322834646493, -0.4536011799217367080, 0.2665933059059888421 ) ) ;
#71786 = AXIS2_PLACEMENT_3D ( 'NONE', #47572, #39607, #2563 ) ;
#71787 = CARTESIAN_POINT ( 'NONE',  ( 0.5314960629921267055, -0.5400638737290844871, 0.3530559997133364547 ) ) ;
#71788 = CARTESIAN_POINT ( 'NONE',  ( -1.548556430446193399, -0.6046776061558809534, -0.2411417322834644161 ) ) ;
#71789 = CARTESIAN_POINT ( 'NONE',  ( -1.515748031496062076, 0.1660481256975883668, -0.3530559997133364547 ) ) ;
#71790 = ORIENTED_EDGE ( 'NONE', *, *, #44272, .F. ) ;
#71791 = EDGE_CURVE ( 'NONE', #82812, #80676, #24255, .T. ) ;
#71792 = CARTESIAN_POINT ( 'NONE',  ( -0.1070741851644051862, -0.3996062992125986590, -2.353674540682414218 ) ) ;
#71793 = CARTESIAN_POINT ( 'NONE',  ( -1.049868766404198794, -0.5023911411419708095, 0.1820866141732285504 ) ) ;
#71794 = CARTESIAN_POINT ( 'NONE',  ( 0.9251968503937015864, -0.5400638737290844871, 0.3530559997133364547 ) ) ;
#71795 = CARTESIAN_POINT ( 'NONE',  ( -1.240157480314959759, 0.07958543189024085140, 0.2665933059059887866 ) ) ;
#71796 = CARTESIAN_POINT ( 'NONE',  ( 0.1070741851644053388, 0.3996062992125986035, -1.802493438320210029 ) ) ;
#71797 = CARTESIAN_POINT ( 'NONE',  ( -1.548556430446193399, 0.2306618581243848609, 0.2411417322834645549 ) ) ;
#71798 = CARTESIAN_POINT ( 'NONE',  ( 0.9776902887139113929, -0.6692913385826773087, -0.1292274648535924053 ) ) ;
#71799 = CARTESIAN_POINT ( 'NONE',  ( 0.5052493438320218022, -0.6692913385826773087, -0.1292274648535924053 ) ) ;
#71800 = CARTESIAN_POINT ( 'NONE',  ( 1.141732283464567566, 0.2952755905511811885, 0.000000000000000000 ) ) ;
#71801 = CARTESIAN_POINT ( 'NONE',  ( -1.332020997375327642, -0.2845877964562161244, -0.3641732283464567121 ) ) ;
#71802 = CARTESIAN_POINT ( 'NONE',  ( -0.1998031496062994405, 0.3460692066303957537, -1.192257217847769057 ) ) ;
#71804 = ADVANCED_FACE ( 'NONE', ( #49935 ), #81520, .F. ) ;
#71803 = CARTESIAN_POINT ( 'NONE',  ( -0.3996062992125986035, -7.340648628747425578E-17, -1.456692913385826849 ) ) ;
#71805 = VECTOR ( 'NONE', #17677, 39.37007874015748143 ) ;
#71806 = CARTESIAN_POINT ( 'NONE',  ( -0.3420746716998659953, -0.1974969037888706647, -0.8398950131233596794 ) ) ;
#71807 = DIRECTION ( 'NONE',  ( -1.000000000000000000, -3.083952846180990774E-16, 0.000000000000000000 ) ) ;
#71808 = CARTESIAN_POINT ( 'NONE',  ( 0.6627296587926517768, -0.5511811023622048555, -0.09757992244046775898 ) ) ;
#71809 = CARTESIAN_POINT ( 'NONE',  ( 0.2690288713910767848, -0.5511811023622048555, -0.09757992244046775898 ) ) ;
#71810 = CARTESIAN_POINT ( 'NONE',  ( 0.1837270341207354329, 0.2306618581243848609, 0.2411417322834645549 ) ) ;
#71811 = CARTESIAN_POINT ( 'NONE',  ( 1.463254593175853824, 0.2952755905511810774, -0.1292274648535930714 ) ) ;
#71812 = CARTESIAN_POINT ( 'NONE',  ( -0.3949938075777411073, 0.1058382717557497660, -1.684383202099737575 ) ) ;
#71813 = CARTESIAN_POINT ( 'NONE',  ( 0.5905511811023629321, 0.1771653543307087630, 0.000000000000000000 ) ) ;
#71814 = EDGE_CURVE ( 'NONE', #35562, #70572, #21801, .T. ) ;
#71815 = CARTESIAN_POINT ( 'NONE',  ( -0.8595800524934373854, -0.05778040916215522460, 0.4822834645669289988 ) ) ;
#71816 = CARTESIAN_POINT ( 'NONE',  ( -1.515748031496062076, -0.5400638737290844871, 0.3530559997133364547 ) ) ;
#71817 = CARTESIAN_POINT ( 'NONE',  ( 0.9580052493438327987, -0.4281496062992127816, -0.4176697321401328100 ) ) ;
#71818 = CARTESIAN_POINT ( 'NONE',  ( -0.4091458600556402980, -0.2362204724409451284, -2.099737532808398921 ) ) ;
#71819 = CARTESIAN_POINT ( 'NONE',  ( 0.3622863298689343314, -0.1504864506494317244, -2.755905511811024056 ) ) ;
#71820 = ORIENTED_EDGE ( 'NONE', *, *, #78000, .F. ) ;
#71821 = EDGE_LOOP ( 'NONE', ( #25733, #52372, #3826, #74654 ) ) ;
#71822 = CARTESIAN_POINT ( 'NONE',  ( -1.292650918635170010, -0.6692913385826771977, 0.1292274648535927661 ) ) ;
#71824 = CARTESIAN_POINT ( 'NONE',  ( -1.292650918635170010, 0.2952755905511810774, -0.1292274648535930714 ) ) ;
#71823 = CARTESIAN_POINT ( 'NONE',  ( -0.9186351706036736120, -0.5023911411419708095, -0.1820866141732282451 ) ) ;
#71825 = CARTESIAN_POINT ( 'NONE',  ( 0.3917322834645668994, -0.1049643490035303134, -2.396306143535746447 ) ) ;
#71826 = DIRECTION ( 'NONE',  ( 0.000000000000000000, 0.000000000000000000, 1.000000000000000000 ) ) ;
#71827 = CARTESIAN_POINT ( 'NONE',  ( 1.469816272965879911, -0.6046776061558807314, 0.2411417322834647770 ) ) ;
#71828 = CARTESIAN_POINT ( 'NONE',  ( -1.043307086614172707, 0.1660481256975883668, -0.3530559997133364547 ) ) ;
#71829 = CARTESIAN_POINT ( 'NONE',  ( 0.1968503937007881344, 0.2952755905511811885, 0.000000000000000000 ) ) ;
#71830 = CARTESIAN_POINT ( 'NONE',  ( -1.259842519685038686, -0.1870078740157480879, -0.4822834645669291653 ) ) ;
#71832 = CARTESIAN_POINT ( 'NONE',  ( 0.3917322834645668994, 0.1049643490035304522, -2.724390133037059236 ) ) ;
#71831 = B_SPLINE_CURVE_WITH_KNOTS ( 'NONE', 3,
 ( #60207, #2137, #47149, #65288, #7626, #47566, #72840, #15189, #40846, #9285, #2969, #28215, #53874, #34956, #60619, #24681, #63400, #44431 ),
 .UNSPECIFIED., .F., .F.,
 ( 4, 2, 2, 2, 2, 2, 2, 2, 4 ),
 ( 0.000000000000000000, 2.503579457910189637E-05, 5.007158915820379274E-05, 0.0001001431783164055797, 0.0002002863566328091536, 0.0004005727132656153257, 0.0008011454265312270735, 0.001602290853062450461, 0.003204581706124896151 ),
 .UNSPECIFIED. ) ;
#71833 = CARTESIAN_POINT ( 'NONE',  ( 0.6167979002624678353, -0.4281496062992124485, 0.4176697321401328655 ) ) ;
#71834 = CARTESIAN_POINT ( 'NONE',  ( 0.3392501089628018329, 0.1958661417322835607, -2.013123359580052618 ) ) ;
#71835 = CARTESIAN_POINT ( 'NONE',  ( -0.7545931758530176614, -0.5511811023622048555, -0.09757992244046775898 ) ) ;
#71836 = ORIENTED_EDGE ( 'NONE', *, *, #38498, .T. ) ;
#71837 = CARTESIAN_POINT ( 'NONE',  ( 0.1058382717557499880, 0.3949938075777411073, -2.040682414698163250 ) ) ;
#71838 = ORIENTED_EDGE ( 'NONE', *, *, #51676, .T. ) ;
#71839 = CARTESIAN_POINT ( 'NONE',  ( -0.6414174258557919783, -3.721645946415733147E-15, -0.3791475997938235643 ) ) ;
#71840 = CARTESIAN_POINT ( 'NONE',  ( -1.154855643044618851, -0.6046776061558809534, -0.2411417322834644161 ) ) ;
#71841 = CARTESIAN_POINT ( 'NONE',  ( -1.476377952755905110, 0.1660481256975885056, 0.3530559997133364547 ) ) ;
#71842 = CARTESIAN_POINT ( 'NONE',  ( -0.2925321140481932924, 0.2925321140481931814, -0.4921259842519684624 ) ) ;
#71843 = CARTESIAN_POINT ( 'NONE',  ( -1.666666666666665853, 0.05413385826771626580, -0.4176697321401330321 ) ) ;
#71844 = CARTESIAN_POINT ( 'NONE',  ( -1.161417322834644716, -0.5400638737290845981, -0.3530559997133363437 ) ) ;
#71845 = CARTESIAN_POINT ( 'NONE',  ( -1.607611548556429737, 0.2952755905511810774, -0.1292274648535930714 ) ) ;
#71846 = DIRECTION ( 'NONE',  ( 0.000000000000000000, 0.000000000000000000, -1.000000000000000000 ) ) ;
#71847 = FACE_OUTER_BOUND ( 'NONE', #56480, .T. ) ;
#71848 = CARTESIAN_POINT ( 'NONE',  ( 0.1246719160104994284, 0.1771653543307087075, -0.09757992244046823083 ) ) ;
#71849 = DIRECTION ( 'NONE',  ( 0.000000000000000000, 0.000000000000000000, 1.000000000000000000 ) ) ;
#71850 = CARTESIAN_POINT ( 'NONE',  ( 0.2867679344610365999, 0.2867679344610365999, -0.3799212598425197318 ) ) ;
#71851 = CARTESIAN_POINT ( 'NONE',  ( -0.4396325459317579898, 0.1771653543307087630, 0.09757992244046791164 ) ) ;
#71852 = CIRCLE ( 'NONE', #73171, 0.2165354330708660069 ) ;
#71853 = CARTESIAN_POINT ( 'NONE',  ( -0.7545931758530176614, -0.6692913385826773087, -0.1292274648535924053 ) ) ;
#71854 = CARTESIAN_POINT ( 'NONE',  ( 1.102362204724410155, -0.1870078740157479769, 0.4822834645669291653 ) ) ;
#71855 = CARTESIAN_POINT ( 'NONE',  ( -0.7545931758530176614, -0.6692913385826773087, -0.1292274648535924053 ) ) ;
#71856 = VERTEX_POINT ( 'NONE', #71379 ) ;
#71857 = ORIENTED_EDGE ( 'NONE', *, *, #62070, .F. ) ;
#71858 = CARTESIAN_POINT ( 'NONE',  ( -1.082677165354329896, -0.5400638737290845981, -0.3530559997133363437 ) ) ;
#71859 = CARTESIAN_POINT ( 'NONE',  ( 0.9776902887139113929, 0.2952755905511811885, 0.1292274648535926551 ) ) ;
#71860 = CARTESIAN_POINT ( 'NONE',  ( -1.443569553805773564, -0.5023911411419708095, 0.1820866141732285504 ) ) ;
#71861 = CARTESIAN_POINT ( 'NONE',  ( -0.2362204724409447953, -0.4091458600556404646, -1.167979002624671914 ) ) ;
#71862 = CARTESIAN_POINT ( 'NONE',  ( 2.159196716653021930, 1.469708627452553928, 0.4698506773045486029 ) ) ;
#71863 = CARTESIAN_POINT ( 'NONE',  ( 0.2867679344610365999, 0.2867679344610365999, -0.1299212598425196485 ) ) ;
#71864 = CARTESIAN_POINT ( 'NONE',  ( 0.3917322834645670104, -0.1049643490035303273, -2.243438320209973913 ) ) ;
#71865 = CARTESIAN_POINT ( 'NONE',  ( -0.1968503937007867743, 0.2952755905511811885, 0.000000000000000000 ) ) ;
#71866 = CARTESIAN_POINT ( 'NONE',  ( 1.673228346456693494, 0.1660481256975885056, 0.3530559997133364547 ) ) ;
#71867 = CARTESIAN_POINT ( 'NONE',  ( -0.7480314960629914633, 0.2952755905511811885, 0.000000000000000000 ) ) ;
#71868 = CARTESIAN_POINT ( 'NONE',  ( 0.1070741851644054776, -0.3996062992125984925, -0.004593175853018396058 ) ) ;
#71869 = CARTESIAN_POINT ( 'NONE',  ( -1.456692913385826182, -0.6692913385826771977, 8.415575281601705876E-17 ) ) ;
#71870 = EDGE_CURVE ( 'NONE', #21240, #37037, #37721, .T. ) ;
#71871 = CARTESIAN_POINT ( 'NONE',  ( -0.9973753280839886548, -0.6046776061558809534, -0.2411417322834644161 ) ) ;
#71872 = CARTESIAN_POINT ( 'NONE',  ( -0.1902887139107604098, -0.6692913385826771977, 0.1292274648535927661 ) ) ;
#71873 = VECTOR ( 'NONE', #81074, 39.37007874015748143 ) ;
#71874 = CARTESIAN_POINT ( 'NONE',  ( -0.3420746716998662729, 0.1974969037888702206, -2.465223097112861250 ) ) ;
#71875 = CARTESIAN_POINT ( 'NONE',  ( 0.4921259842519691285, 0.07958543189024085140, 0.2665933059059887866 ) ) ;
#71876 = DIRECTION ( 'NONE',  ( 0.000000000000000000, 0.000000000000000000, 1.000000000000000000 ) ) ;
#71877 = CARTESIAN_POINT ( 'NONE',  ( 0.2755905511811031494, 0.1771653543307087630, 0.000000000000000000 ) ) ;
#71878 = CARTESIAN_POINT ( 'NONE',  ( 1.325459317585302665, -0.004921259842519870586, -0.3153832671262229437 ) ) ;
#71879 = CARTESIAN_POINT ( 'NONE',  ( 1.292650918635171564, 0.2952755905511811885, 0.1292274648535926551 ) ) ;
#71880 = CARTESIAN_POINT ( 'NONE',  ( 0.01312335958005323398, -0.3690944881889765550, -0.3153832671262227771 ) ) ;
#71881 = CARTESIAN_POINT ( 'NONE',  ( 0.2867679344610365999, -0.2867679344610365444, -1.980314960629921073 ) ) ;
#71882 = CARTESIAN_POINT ( 'NONE',  ( -1.443569553805773564, 0.2306618581243847221, -0.2411417322834647770 ) ) ;
#71883 = CARTESIAN_POINT ( 'NONE',  ( 1.338582677165355062, -0.1870078740157480879, -0.4822834645669291653 ) ) ;
#71884 = CARTESIAN_POINT ( 'NONE',  ( 0.4091458600556403535, 0.2362204724409449896, -0.05052493438320210251 ) ) ;
#71885 = CARTESIAN_POINT ( 'NONE',  ( -0.6561679790026240244, 0.1283753931104746893, -0.1820866141732285504 ) ) ;
#71886 = CARTESIAN_POINT ( 'NONE',  ( 0.01158586635040232717, 0.02791078216816225699, 0.4328096321851905293 ) ) ;
#71887 = CARTESIAN_POINT ( 'NONE',  ( 0.1837270341207357105, -0.6046776061558809534, -0.2411417322834644161 ) ) ;
#71888 = CARTESIAN_POINT ( 'NONE',  ( -0.4724409448818899238, 0.1265901696524986964, -0.7395013123359578389 ) ) ;
#71889 = CARTESIAN_POINT ( 'NONE',  ( 1.108923884514436242, -0.08942795157527998196, 0.3641732283464567121 ) ) ;
#71890 = CARTESIAN_POINT ( 'NONE',  ( 0.2952755905511816326, -0.4536011799217367080, 0.2665933059059888421 ) ) ;
#71891 = CARTESIAN_POINT ( 'NONE',  ( -0.09842519685039295696, -0.5400638737290844871, 0.3530559997133364547 ) ) ;
#71892 = PLANE ( 'NONE',  #19672 ) ;
#71893 = CARTESIAN_POINT ( 'NONE',  ( -0.6758530183727028406, 0.1771653543307087630, 0.09757992244046791164 ) ) ;
#71894 = CARTESIAN_POINT ( 'NONE',  ( 1.348312163386739426, 0.2755905511811023723, 0.6195921248415929838 ) ) ;
#71895 = CARTESIAN_POINT ( 'NONE',  ( 0.3871391076115493490, -0.3162353388693405765, 0.4822834645669290543 ) ) ;
#71896 = CARTESIAN_POINT ( 'NONE',  ( -0.9055118110236215490, -0.6692913385826771977, 8.415575281601705876E-17 ) ) ;
#71897 = CARTESIAN_POINT ( 'NONE',  ( 0.3460692066303958092, 0.1998031496062993018, -1.310367454068241511 ) ) ;
#71898 = CARTESIAN_POINT ( 'NONE',  ( -0.2867679344610364334, -0.2867679344610367109, -2.663385826771653253 ) ) ;
#71899 = CARTESIAN_POINT ( 'NONE',  ( 0.1377952755905518800, -0.4536011799217367080, 0.2665933059059888421 ) ) ;
#71900 = CARTESIAN_POINT ( 'NONE',  ( -0.8202099737532799750, 0.2952755905511810774, -0.1292274648535930714 ) ) ;
#71901 = CARTESIAN_POINT ( 'NONE',  ( -1.095800524934382292, -0.3162353388693409650, -0.4822834645669289433 ) ) ;
#71902 = CARTESIAN_POINT ( 'NONE',  ( -1.128608923884513837, 0.1283753931104746893, -0.1820866141732285504 ) ) ;
#71903 = CARTESIAN_POINT ( 'NONE',  ( 0.000000000000000000, 0.000000000000000000, -0.4921259842519685179 ) ) ;
#71904 =( BOUNDED_CURVE ( )  B_SPLINE_CURVE ( 2, ( #68494, #41979, #23039, #55016, #67261, #35674, #48705, #10834, #67673, #10009, #9594, #28116, #3277 ),
 .UNSPECIFIED., .F., .F. ) 
 B_SPLINE_CURVE_WITH_KNOTS ( ( 3, 2, 2, 2, 2, 2, 3 ),
 ( 0.3558514478433236206, 0.3560606060606060774, 0.3598484848484848619, 0.3636363636363636465, 0.3674242424242424310, 0.3712121212121212155, 0.3714212794294036724 ),
 .UNSPECIFIED. ) 
 CURVE ( )  GEOMETRIC_REPRESENTATION_ITEM ( )  RATIONAL_B_SPLINE_CURVE ( ( 0.9964447847208428577, 0.9981185001348096275, 1.000000000000000000, 0.9659258262890683122, 1.000000000000000000, 0.9659258262890683122, 1.000000000000000000, 0.9659258262890683122, 1.000000000000000000, 0.9659258262890683122, 1.000000000000000000, 0.9981185001348097385, 0.9964447847208430797 ) ) 
 REPRESENTATION_ITEM ( '' )  );
#71905 = CARTESIAN_POINT ( 'NONE',  ( -1.023622047244093558, -0.1870078740157479769, 0.3641732283464567677 ) ) ;
#71906 = FACE_OUTER_BOUND ( 'NONE', #22231, .T. ) ;
#71907 = CARTESIAN_POINT ( 'NONE',  ( 0.6889763779527563470, 0.1660481256975883668, -0.3530559997133364547 ) ) ;
#71908 = CARTESIAN_POINT ( 'NONE',  ( 0.2925321140481932369, -0.2925321140481932369, -0.09842519685039373412 ) ) ;
#71909 = CARTESIAN_POINT ( 'NONE',  ( 4.797336870675656522E-17, -0.3917322834645670659, -2.437683357776589510 ) ) ;
#71910 = ORIENTED_EDGE ( 'NONE', *, *, #26715, .T. ) ;
#71911 = AXIS2_PLACEMENT_3D ( 'NONE', #1469, #65020, #20820 ) ;
#71912 = CARTESIAN_POINT ( 'NONE',  ( -0.9348729704079935532, -2.191421614605370878E-15, 0.4445507791589071167 ) ) ;
#71913 = CARTESIAN_POINT ( 'NONE',  ( 1.450131233595801428, 0.1771653543307087630, 0.09757992244046791164 ) ) ;
#71914 = CARTESIAN_POINT ( 'NONE',  ( -1.404199475065615932, 0.05413385826771666132, 0.4176697321401328100 ) ) ;
#71915 = CARTESIAN_POINT ( 'NONE',  ( 1.056430446194226436, -0.6692913385826773087, -0.1292274648535924053 ) ) ;
#71916 = CARTESIAN_POINT ( 'NONE',  ( -0.3392501089628019995, 0.1958661417322832277, -2.315616797900262647 ) ) ;
#71917 = CARTESIAN_POINT ( 'NONE',  ( 1.528871391076116026, 0.1771653543307087630, 0.09757992244046791164 ) ) ;
#71918 = CARTESIAN_POINT ( 'NONE',  ( 0.4658792650918641698, -0.05778040916215560624, -0.4822834645669293319 ) ) ;
#71919 = CARTESIAN_POINT ( 'NONE',  ( -0.2230971128608915943, 0.05413385826771666132, 0.4176697321401328100 ) ) ;
#71920 = CARTESIAN_POINT ( 'NONE',  ( 0.4744094488189115055, 1.506021921081838633, -3.908320185825790993 ) ) ;
#71921 = CARTESIAN_POINT ( 'NONE',  ( 0.2925321140481932369, 0.2925321140481932369, -2.027559055118109743 ) ) ;
#71922 = CARTESIAN_POINT ( 'NONE',  ( 0.6955380577427828781, -0.004921259842519870586, -0.3153832671262229437 ) ) ;
#71923 = CARTESIAN_POINT ( 'NONE',  ( -0.3996062992125986035, -7.340648628747425578E-17, -1.456692913385826849 ) ) ;
#71924 = ORIENTED_EDGE ( 'NONE', *, *, #76134, .T. ) ;
#71926 = CARTESIAN_POINT ( 'NONE',  ( 0.3392501089628018884, -0.1958661417322833942, 0.05575496243338393110 ) ) ;
#71925 = VECTOR ( 'NONE', #55369, 39.37007874015748143 ) ;
#71927 = ORIENTED_EDGE ( 'NONE', *, *, #44019, .F. ) ;
#71928 = CARTESIAN_POINT ( 'NONE',  ( -0.09842519685039295696, 0.1660481256975883668, -0.3530559997133364547 ) ) ;
#71929 = CARTESIAN_POINT ( 'NONE',  ( 1.345144356955381593, -0.3162353388693409650, -0.4822834645669289433 ) ) ;
#71930 = CARTESIAN_POINT ( 'NONE',  ( 0.3280839895013130669, -0.4281496062992127816, -0.4176697321401328100 ) ) ;
#71931 = CARTESIAN_POINT ( 'NONE',  ( 1.423884514435696413, -0.3162353388693409650, -0.4822834645669289433 ) ) ;
#71932 = CARTESIAN_POINT ( 'NONE',  ( -0.5774278215223089816, -0.6046776061558807314, 0.2411417322834647770 ) ) ;
#71933 = CARTESIAN_POINT ( 'NONE',  ( 0.01968503937007930540, 0.1660481256975885056, 0.3530559997133364547 ) ) ;
#71934 = CARTESIAN_POINT ( 'NONE',  ( 1.437007874015748810, 0.1660481256975885056, 0.3530559997133364547 ) ) ;
#71935 = CARTESIAN_POINT ( 'NONE',  ( 1.213910761154856299, -0.6692913385826773087, -0.1292274648535924053 ) ) ;
#71936 = CARTESIAN_POINT ( 'NONE',  ( 0.9776902887139113929, -0.6692913385826773087, -0.1292274648535924053 ) ) ;
#71937 = CARTESIAN_POINT ( 'NONE',  ( -0.3392501089628019995, 0.1958661417322832277, -0.4908136482939632339 ) ) ;
#71938 = CARTESIAN_POINT ( 'NONE',  ( 0.3346456692913393205, -0.4536011799217368745, -0.2665933059059886201 ) ) ;
#71939 = ORIENTED_EDGE ( 'NONE', *, *, #76134, .F. ) ;
#71940 = CARTESIAN_POINT ( 'NONE',  ( -9.674558042662121740E-17, 0.3949938075777409963, -0.7874015748031496509 ) ) ;
#71941 = VERTEX_POINT ( 'NONE', #12471 ) ;
#71942 = CARTESIAN_POINT ( 'NONE',  ( -0.5905511811023615998, 0.1771653543307087630, 0.000000000000000000 ) ) ;
#71943 = CARTESIAN_POINT ( 'NONE',  ( -0.1706036745406816491, 0.05413385826771626580, -0.4176697321401330321 ) ) ;
#71944 = CARTESIAN_POINT ( 'NONE',  ( -1.545038802164343306, 1.128537896298102305, 0.2406134192599649335 ) ) ;
#71945 = CARTESIAN_POINT ( 'NONE',  ( -0.3937007874015740483, -0.1870078740157480879, -0.4822834645669291653 ) ) ;
#71946 = CARTESIAN_POINT ( 'NONE',  ( 0.03937007874015806264, 0.2952755905511811885, 0.000000000000000000 ) ) ;
#71947 = CARTESIAN_POINT ( 'NONE',  ( -0.8530183727034112984, 0.05413385826771666132, 0.4176697321401328100 ) ) ;
#71948 = CARTESIAN_POINT ( 'NONE',  ( -1.187664041994750175, -0.05778040916215560624, -0.4822834645669293319 ) ) ;
#71949 = CARTESIAN_POINT ( 'NONE',  ( 1.174540682414699111, -0.2845877964562159024, 0.3641732283464567677 ) ) ;
#71950 = CARTESIAN_POINT ( 'NONE',  ( -1.620734908136482577, 0.2952755905511811885, 0.1292274648535926551 ) ) ;
#71951 = CARTESIAN_POINT ( 'NONE',  ( -0.9881811337016640495, 2.755905511811024056, -0.5314960629921260393 ) ) ;
#71952 = CARTESIAN_POINT ( 'NONE',  ( 1.076115485564305141, -0.5023911411419708095, 0.1820866141732285504 ) ) ;
#71953 = CARTESIAN_POINT ( 'NONE',  ( 0.4724409448818904789, -0.1870078740157480879, -0.4822834645669291653 ) ) ;
#71954 = CARTESIAN_POINT ( 'NONE',  ( 0.6233595800524942554, -0.05778040916215560624, -0.4822834645669293319 ) ) ;
#71955 = CARTESIAN_POINT ( 'NONE',  ( -0.2925321140481932924, 0.2925321140481931814, -1.437007874015747921 ) ) ;
#71956 = DIRECTION ( 'NONE',  ( 0.000000000000000000, -1.000000000000000000, 0.000000000000000000 ) ) ;
#71957 = CARTESIAN_POINT ( 'NONE',  ( 0.1998031496062992463, 0.3460692066303959202, -0.8510498687664042050 ) ) ;
#71958 = CARTESIAN_POINT ( 'NONE',  ( -0.1998031496062994405, 0.3460692066303957537, -0.4048556430446194621 ) ) ;
#71959 = CARTESIAN_POINT ( 'NONE',  ( -0.7086614173228339419, -0.1870078740157480879, -0.4822834645669291653 ) ) ;
#71960 = CARTESIAN_POINT ( 'NONE',  ( -0.3458507752293906723, -0.3458507752293910609, -0.2165354330708661734 ) ) ;
#71961 = CARTESIAN_POINT ( 'NONE',  ( 4.797336870675656522E-17, -0.3917322834645670104, -2.053149606299212948 ) ) ;
#71962 = CARTESIAN_POINT ( 'NONE',  ( -1.102362204724408601, -0.1870078740157480601, -0.3641732283464567677 ) ) ;
#71963 = CARTESIAN_POINT ( 'NONE',  ( 1.003937007874016185, 0.1660481256975883668, -0.3530559997133364547 ) ) ;
#71964 = CARTESIAN_POINT ( 'NONE',  ( 1.128608923884515169, -0.6046776061558809534, -0.2411417322834644161 ) ) ;
#71965 = CARTESIAN_POINT ( 'NONE',  ( -0.03937007874015669567, 0.1771653543307087630, 0.000000000000000000 ) ) ;
#71966 = CARTESIAN_POINT ( 'NONE',  ( 0.5643044619422579178, -0.4281496062992127816, -0.4176697321401328100 ) ) ;
#71967 = CARTESIAN_POINT ( 'NONE',  ( 0.4724409448818898682, 2.892866454678787531E-17, -1.927165354330708569 ) ) ;
#71968 = CARTESIAN_POINT ( 'NONE',  ( -0.09842519685039295696, -0.4536011799217367080, 0.2665933059059888421 ) ) ;
#71969 = CARTESIAN_POINT ( 'NONE',  ( 0.04593175853018440641, 0.2952755905511810774, -0.1292274648535930714 ) ) ;
#71970 = EDGE_CURVE ( 'NONE', #32372, #81967, #19606, .T. ) ;
#71971 = CARTESIAN_POINT ( 'NONE',  ( 0.2891555358219910499, -0.2891555358219909944, -1.277559055118109965 ) ) ;
#71972 = CARTESIAN_POINT ( 'NONE',  ( -1.272965879265091305, -0.4281496062992124485, 0.4176697321401328655 ) ) ;
#71973 = CARTESIAN_POINT ( 'NONE',  ( 0.5249343832021003964, 0.1283753931104746893, -0.1820866141732285504 ) ) ;
#71974 = CARTESIAN_POINT ( 'NONE',  ( -0.7233796917120549619, 1.992010844874188447, -0.5048038503170217961 ) ) ;
#71975 = CARTESIAN_POINT ( 'NONE',  ( -0.5971128608923877978, 0.2952755905511811885, 0.1292274648535926551 ) ) ;
#71976 = CARTESIAN_POINT ( 'NONE',  ( -0.1771653543307080136, 0.07958543189024071263, -0.2665933059059888421 ) ) ;
#71977 = CARTESIAN_POINT ( 'NONE',  ( -2.557132292622109837, 1.503024749832831519, -0.4732391302016651369 ) ) ;
#71978 = CARTESIAN_POINT ( 'NONE',  ( -0.5446194225721777693, -0.3162353388693409650, -0.4822834645669289433 ) ) ;
#71979 = CARTESIAN_POINT ( 'NONE',  ( -0.5249343832020990641, 0.2306618581243848609, 0.2411417322834645549 ) ) ;
#71980 = CARTESIAN_POINT ( 'NONE',  ( -0.02624671916010428221, 0.2306618581243847221, -0.2411417322834647770 ) ) ;
#71981 = CARTESIAN_POINT ( 'NONE',  ( 0.1998031496062994128, -0.3460692066303957537, -2.215879265091863726 ) ) ;
#71982 = CARTESIAN_POINT ( 'NONE',  ( 0.3917322834645668994, -0.1049643490035303134, -1.923865198653856634 ) ) ;
#71983 = VECTOR ( 'NONE', #13606, 39.37007874015748143 ) ;
#71984 = CARTESIAN_POINT ( 'NONE',  ( -1.646981627296586703, -0.2845877964562161244, -0.3641732283464567121 ) ) ;
#71985 = CARTESIAN_POINT ( 'NONE',  ( 0.5774278215223104249, 0.1283753931104748280, 0.1820866141732283561 ) ) ;
#71986 = CARTESIAN_POINT ( 'NONE',  ( 1.233595800524935227, -0.6046776061558807314, 0.2411417322834647770 ) ) ;
#71987 = CARTESIAN_POINT ( 'NONE',  ( -0.7742782152230965886, -0.004921259842519576551, 0.3153832671262227771 ) ) ;
#71988 = CARTESIAN_POINT ( 'NONE',  ( -1.076115485564303809, 0.1283753931104748280, 0.1820866141732283561 ) ) ;
#71989 = CARTESIAN_POINT ( 'NONE',  ( -0.5971128608923877978, -0.6692913385826773087, -0.1292274648535924053 ) ) ;
#71990 = CARTESIAN_POINT ( 'NONE',  ( -0.6299212598425188991, -0.1870078740157479769, 0.4822834645669291653 ) ) ;
#71991 = CARTESIAN_POINT ( 'NONE',  ( 0.6627296587926517768, -0.5511811023622048555, -0.09757992244046775898 ) ) ;
#71992 = CARTESIAN_POINT ( 'NONE',  ( -0.2896989933648237980, 0.05817964957694448519, 5.534220241493016168 ) ) ;
#71993 = CARTESIAN_POINT ( 'NONE',  ( 1.181102362204724976, -0.1870078740157480601, -0.3641732283464567677 ) ) ;
#71994 = CARTESIAN_POINT ( 'NONE',  ( 0.3280839895013130669, -0.4281496062992127816, -0.4176697321401328100 ) ) ;
#71995 = CARTESIAN_POINT ( 'NONE',  ( 0.3996062992125984925, 0.1070741851644054637, 0.1135170603674540563 ) ) ;
#71996 = CARTESIAN_POINT ( 'NONE',  ( -0.5708661417322828946, 0.1660481256975883668, -0.3530559997133364547 ) ) ;
#71997 = CARTESIAN_POINT ( 'NONE',  ( 0.1958661417322836440, -0.3392501089628017219, -1.593832020997375531 ) ) ;
#71998 = CARTESIAN_POINT ( 'NONE',  ( 1.253280839895013710, -0.2845877964562159024, 0.3641732283464567677 ) ) ;
#71999 = CARTESIAN_POINT ( 'NONE',  ( 0.5118110236220480003, -0.6692913385826771977, 8.415575281601705876E-17 ) ) ;
#72000 = CARTESIAN_POINT ( 'NONE',  ( 0.2099737532808405305, -0.6046776061558807314, 0.2411417322834647770 ) ) ;
#72001 = CARTESIAN_POINT ( 'NONE',  ( -0.1181102362204717315, -0.5511811023622047445, 6.969142054262312111E-17 ) ) ;
#72002 = CARTESIAN_POINT ( 'NONE',  ( -0.2087913723976026203, -0.2087913723976025926, 0.1248231986745540339 ) ) ;
#72003 = CARTESIAN_POINT ( 'NONE',  ( -0.1837270341207340729, 0.1283753931104746893, -0.1820866141732285504 ) ) ;
#72004 = CARTESIAN_POINT ( 'NONE',  ( 0.5971128608923891301, 0.2952755905511810774, -0.1292274648535930714 ) ) ;
#72005 = CARTESIAN_POINT ( 'NONE',  ( -0.5446194225721777693, -0.2845877964562161244, -0.3641732283464567121 ) ) ;
#72006 = CARTESIAN_POINT ( 'NONE',  ( -0.8858267716535425107, -0.5400638737290844871, 0.3530559997133364547 ) ) ;
#72007 = CARTESIAN_POINT ( 'NONE',  ( -1.220472440944878834, 0.000000000000000000, -0.5309055118110234117 ) ) ;
#72008 = ORIENTED_EDGE ( 'NONE', *, *, #38239, .T. ) ;
#72009 = CARTESIAN_POINT ( 'NONE',  ( -1.253280839895012377, -0.3162353388693409650, -0.4822834645669289433 ) ) ;
#72010 = CARTESIAN_POINT ( 'NONE',  ( -0.9383202099737524282, -0.08942795157527998196, 0.3641732283464567121 ) ) ;
#72011 = CARTESIAN_POINT ( 'NONE',  ( -0.1771653543307080136, -0.5400638737290844871, 0.3530559997133364547 ) ) ;
#72012 = CARTESIAN_POINT ( 'NONE',  ( -1.633858267716534529, -0.5400638737290845981, -0.3530559997133363437 ) ) ;
#72013 = CARTESIAN_POINT ( 'NONE',  ( -0.7217847769028863381, -0.4281496062992124485, 0.4176697321401328655 ) ) ;
#72014 = CARTESIAN_POINT ( 'NONE',  ( 0.4732141852945755400, 1.572163861244850303, -2.167216380768100858 ) ) ;
#72016 = CARTESIAN_POINT ( 'NONE',  ( 0.8923884514435701520, -0.6046776061558809534, -0.2411417322834644161 ) ) ;
#72015 = DIRECTION ( 'NONE',  ( 0.000000000000000000, 0.000000000000000000, -1.000000000000000000 ) ) ;
#72017 = CARTESIAN_POINT ( 'NONE',  ( 0.8136482939632553313, -0.6046776061558809534, -0.2411417322834644161 ) ) ;
#72018 = CARTESIAN_POINT ( 'NONE',  ( -0.2867679344610364334, -0.2867679344610367109, -2.413385826771653253 ) ) ;
#72019 = CARTESIAN_POINT ( 'NONE',  ( 1.607611548556431069, 0.2952755905511811885, 0.1292274648535926551 ) ) ;
#72020 = CARTESIAN_POINT ( 'NONE',  ( -1.450131233595799651, -0.6692913385826771977, 0.1292274648535927661 ) ) ;
#72021 = CARTESIAN_POINT ( 'NONE',  ( 0.3460692066303959757, -0.1998031496062991907, -0.1049868766404199599 ) ) ;
#72022 = EDGE_LOOP ( 'NONE', ( #25221, #47056 ) ) ;
#72023 = CARTESIAN_POINT ( 'NONE',  ( -0.3871391076115476282, -0.08942795157527998196, 0.3641732283464567121 ) ) ;
#72024 = CARTESIAN_POINT ( 'NONE',  ( -0.3392501089628017219, -0.1958661417322836718, -1.934383202099737575 ) ) ;
#72025 = ORIENTED_EDGE ( 'NONE', *, *, #28086, .T. ) ;
#72026 = CARTESIAN_POINT ( 'NONE',  ( 0.05905511811023681640, 0.1660481256975883668, -0.3530559997133364547 ) ) ;
#72027 = CARTESIAN_POINT ( 'NONE',  ( 0.05905511811023681640, 0.1660481256975883668, -0.3530559997133364547 ) ) ;
#72028 = CARTESIAN_POINT ( 'NONE',  ( -0.7545931758530176614, -0.6692913385826773087, -0.1292274648535924053 ) ) ;
#72029 = CARTESIAN_POINT ( 'NONE',  ( 1.581364829396326277, -0.3162353388693409650, -0.4822834645669289433 ) ) ;
#72030 = CARTESIAN_POINT ( 'NONE',  ( -0.9383202099737524282, -0.2845877964562161244, -0.3641732283464567121 ) ) ;
#72031 = CARTESIAN_POINT ( 'NONE',  ( 5.333846858410640380E-15, 1.062992125984252079, -1.444810848096780953 ) ) ;
#72032 = CARTESIAN_POINT ( 'NONE',  ( 0.9645669291338591078, -0.5400638737290845981, -0.3530559997133363437 ) ) ;
#72033 = CARTESIAN_POINT ( 'NONE',  ( 0.6692913385826777528, 0.1771653543307087630, 0.000000000000000000 ) ) ;
#72034 = CARTESIAN_POINT ( 'NONE',  ( -0.3018372703412066094, -0.4281496062992127816, -0.4176697321401328100 ) ) ;
#72035 = CARTESIAN_POINT ( 'NONE',  ( -0.1958661417322834497, -0.3392501089628018884, -1.090531865320523153 ) ) ;
#72036 = CARTESIAN_POINT ( 'NONE',  ( -0.7939632545931750718, -0.05778040916215560624, -0.4822834645669293319 ) ) ;
#72037 = CARTESIAN_POINT ( 'NONE',  ( -1.555118110236219930, 0.07958543189024085140, 0.2665933059059887866 ) ) ;
#72038 =( BOUNDED_CURVE ( )  B_SPLINE_CURVE ( 2, ( #76944, #31485, #39045, #14236, #13812, #77362, #70620, #57146, #12976, #77786, #6644, #71886, #65158 ),
 .UNSPECIFIED., .F., .F. ) 
 B_SPLINE_CURVE_WITH_KNOTS ( ( 3, 2, 2, 2, 2, 2, 3 ),
 ( 0.4460583673620736045, 0.4469696969696969613, 0.4507575757575757458, 0.4545454545454545303, 0.4583333333333333148, 0.4621212121212120993, 0.4630325417288355672 ),
 .UNSPECIFIED. ) 
 CURVE ( )  GEOMETRIC_REPRESENTATION_ITEM ( )  RATIONAL_B_SPLINE_CURVE ( ( 0.9875488213027530104, 0.9918020599134685922, 1.000000000000000000, 0.9659258262890683122, 1.000000000000000000, 0.9659258262890683122, 1.000000000000000000, 0.9659258262890683122, 1.000000000000000000, 0.9659258262890683122, 1.000000000000000000, 0.9918020599134675930, 0.9875488213027519002 ) ) 
 REPRESENTATION_ITEM ( '' )  );
#72039 = CARTESIAN_POINT ( 'NONE',  ( 1.502624671916010790, -0.05778040916215522460, 0.4822834645669289988 ) ) ;
#72040 = CARTESIAN_POINT ( 'NONE',  ( 1.528871391076116026, 0.1771653543307087630, 0.09757992244046791164 ) ) ;
#72041 = EDGE_LOOP ( 'NONE', ( #16775, #54307, #25338, #7224 ) ) ;
#72042 = CARTESIAN_POINT ( 'NONE',  ( 0.3392501089628018329, 0.1958661417322835607, -2.647657111057429624 ) ) ;
#72043 = CARTESIAN_POINT ( 'NONE',  ( 0.1246719160104994284, 0.2952755905511810774, -0.1292274648535930714 ) ) ;
#72044 = EDGE_LOOP ( 'NONE', ( #7622, #81985, #70356, #4940, #26391 ) ) ;
#72045 = CONICAL_SURFACE ( 'NONE', #46479, 1.181102362204724310, 0.7853981633974621568 ) ;
#72046 = CARTESIAN_POINT ( 'NONE',  ( -1.345144356955379816, -0.05778040916215560624, -0.4822834645669293319 ) ) ;
#72047 = CARTESIAN_POINT ( 'NONE',  ( 1.391076115485564868, -0.6046776061558807314, 0.2411417322834647770 ) ) ;
#72048 = CARTESIAN_POINT ( 'NONE',  ( 1.358267716535433323, -0.5400638737290845981, -0.3530559997133363437 ) ) ;
#72049 = CARTESIAN_POINT ( 'NONE',  ( 0.3018372703412079971, -0.4281496062992124485, 0.4176697321401328655 ) ) ;
#72050 = CARTESIAN_POINT ( 'NONE',  ( -0.4461942257217840213, -0.6046776061558809534, -0.2411417322834644161 ) ) ;
#72051 = CARTESIAN_POINT ( 'NONE',  ( 4.797336870675656522E-17, -0.3917322834645670104, -1.895669291338582640 ) ) ;
#72052 = CARTESIAN_POINT ( 'NONE',  ( -1.141732283464566011, -0.6692913385826771977, 8.415575281601705876E-17 ) ) ;
#72053 = CARTESIAN_POINT ( 'NONE',  ( -0.7611548556430438595, -0.6046776061558809534, -0.2411417322834644161 ) ) ;
#72054 = CARTESIAN_POINT ( 'NONE',  ( -0.5314960629921250401, 0.07958543189024085140, 0.2665933059059887866 ) ) ;
#72055 = CARTESIAN_POINT ( 'NONE',  ( 1.522309711286089939, 0.2306618581243848609, 0.2411417322834645549 ) ) ;
#72056 = CARTESIAN_POINT ( 'NONE',  ( -0.3871391076115479057, -0.3162353388693409650, -0.4822834645669289433 ) ) ;
#72057 = CARTESIAN_POINT ( 'NONE',  ( 0.1181102362204724254, 8.537024980200824098E-18, 0.000000000000000000 ) ) ;
#72058 = CARTESIAN_POINT ( 'NONE',  ( 0.6167979002624678353, -0.4281496062992124485, 0.4176697321401328655 ) ) ;
#72059 = CARTESIAN_POINT ( 'NONE',  ( 0.5384083780239495853, 0.004960608223778644084, -0.3437734562760191293 ) ) ;
#72060 = EDGE_CURVE ( 'NONE', #43230, #8650, #39383, .T. ) ;
#72061 = CARTESIAN_POINT ( 'NONE',  ( -0.2362204724409440182, -0.1870078740157479769, 0.4822834645669291653 ) ) ;
#72062 = CARTESIAN_POINT ( 'NONE',  ( -0.2887139107611542133, 0.1283753931104748280, 0.1820866141732283561 ) ) ;
#72064 = CARTESIAN_POINT ( 'NONE',  ( 0.6971652711706697314, -4.135162568743707313E-16, -0.3791483426435169335 ) ) ;
#72063 = CARTESIAN_POINT ( 'NONE',  ( 0.8727034120734913358, -0.08942795157527998196, 0.3641732283464567121 ) ) ;
#72065 = CARTESIAN_POINT ( 'NONE',  ( -0.4724409448818895907, -0.1265901696524993070, -0.2801837270341207553 ) ) ;
#72066 = LINE ( 'NONE', #33351, #39169 ) ;
#72067 = CARTESIAN_POINT ( 'NONE',  ( 1.187664041994751285, -0.3162353388693409650, -0.4822834645669289433 ) ) ;
#72068 = CARTESIAN_POINT ( 'NONE',  ( -0.2891555358219911054, 0.2891555358219909388, -0.09645669291338582196 ) ) ;
#72069 = CARTESIAN_POINT ( 'NONE',  ( 0.1771653543307093182, 0.1660481256975885056, 0.3530559997133364547 ) ) ;
#72070 = LINE ( 'NONE', #27441, #24354 ) ;
#72071 = CARTESIAN_POINT ( 'NONE',  ( 1.574803149606299746, -0.1870078740157479769, 0.3641732283464567677 ) ) ;
#72072 = CARTESIAN_POINT ( 'NONE',  ( -0.3608923884514428360, -0.6692913385826773087, -0.1292274648535924053 ) ) ;
#72073 = CARTESIAN_POINT ( 'NONE',  ( 0.2891555358219910499, -0.2891555358219909944, -0.1751968503937007815 ) ) ;
#72074 = CARTESIAN_POINT ( 'NONE',  ( -1.594488188976377119, 0.07958543189024071263, -0.2665933059059888421 ) ) ;
#72075 = CARTESIAN_POINT ( 'NONE',  ( 0.6364829396325465405, -0.05778040916215522460, 0.4822834645669289988 ) ) ;
#72076 = CARTESIAN_POINT ( 'NONE',  ( 0.8727034120734913358, -0.08942795157527998196, 0.3641732283464567121 ) ) ;
#72077 = CYLINDRICAL_SURFACE ( 'NONE', #33139, 1.181102362204724310 ) ;
#72078 = CARTESIAN_POINT ( 'NONE',  ( 0.3018372703412079971, -0.004921259842519870586, -0.3153832671262229437 ) ) ;
#72079 = CARTESIAN_POINT ( 'NONE',  ( -1.082677165354329896, -0.5400638737290845981, -0.3530559997133363437 ) ) ;
#72080 = CARTESIAN_POINT ( 'NONE',  ( -0.1998031496062991630, -0.3460692066303959202, -0.9297900262467192478 ) ) ;
#72081 = CARTESIAN_POINT ( 'NONE',  ( 1.345144356955381593, -0.05778040916215522460, 0.4822834645669289988 ) ) ;
#72082 = AXIS2_PLACEMENT_3D ( 'NONE', #78082, #79752, #20828 ) ;
#72083 = CARTESIAN_POINT ( 'NONE',  ( -0.2867679344610365999, 0.2867679344610364889, -0.4842519685039369248 ) ) ;
#72084 = AXIS2_PLACEMENT_3D ( 'NONE', #68975, #82034, #70622 ) ;
#72086 = CARTESIAN_POINT ( 'NONE',  ( 0.4724409448818902568, -0.1265901696524981135, -0.5032808398950130435 ) ) ;
#72085 = CARTESIAN_POINT ( 'NONE',  ( 0.3608923884514443348, -0.6692913385826771977, 0.1292274648535927661 ) ) ;
#72087 = CARTESIAN_POINT ( 'NONE',  ( 0.3346456692913390985, 0.07958543189024085140, 0.2665933059059887866 ) ) ;
#72088 = CARTESIAN_POINT ( 'NONE',  ( 0.4658792650918641698, -0.05778040916215560624, -0.4822834645669293319 ) ) ;
#72089 = CARTESIAN_POINT ( 'NONE',  ( -0.8661417322834640276, -0.1870078740157480601, -0.3641732283464567677 ) ) ;
#72090 = CARTESIAN_POINT ( 'NONE',  ( -0.9645669291338575535, -0.5400638737290844871, 0.3530559997133364547 ) ) ;
#72091 = CARTESIAN_POINT ( 'NONE',  ( -1.712598425196849572, 0.1660481256975885056, 0.3530559997133364547 ) ) ;
#72092 = CARTESIAN_POINT ( 'NONE',  ( 1.036745406824147731, 0.05413385826771666132, 0.4176697321401328100 ) ) ;
#72093 = CARTESIAN_POINT ( 'NONE',  ( 1.489501312335958172, -0.3162353388693405765, 0.4822834645669290543 ) ) ;
#72094 = CARTESIAN_POINT ( 'NONE',  ( -0.3965571307776180610, -0.02707642104390632631, -1.220472440944881942 ) ) ;
#72095 = CARTESIAN_POINT ( 'NONE',  ( 0.7152230971128614723, -0.3162353388693409650, -0.4822834645669289433 ) ) ;
#72096 = CARTESIAN_POINT ( 'NONE',  ( -0.1998031496062994405, 0.3460692066303957537, 0.2250656167979002420 ) ) ;
#72097 = AXIS2_PLACEMENT_3D ( 'NONE', #13788, #20514, #20928 ) ;
#72098 = CARTESIAN_POINT ( 'NONE',  ( 1.601049868766404982, -0.6046776061558809534, -0.2411417322834644161 ) ) ;
#72099 = CARTESIAN_POINT ( 'NONE',  ( 1.286089238845145033, -0.6046776061558809534, -0.2411417322834644161 ) ) ;
#72100 = CARTESIAN_POINT ( 'NONE',  ( -1.646981627296586703, -0.2845877964562161244, -0.3641732283464567121 ) ) ;
#72101 = CARTESIAN_POINT ( 'NONE',  ( 1.181102362204725198, -0.1870078740157479769, 0.3641732283464567677 ) ) ;
#72102 = CARTESIAN_POINT ( 'NONE',  ( -1.299212598425196097, 0.1771653543307087630, 0.000000000000000000 ) ) ;
#72103 = CARTESIAN_POINT ( 'NONE',  ( -0.4461942257217840213, -0.5023911411419708095, -0.1820866141732282451 ) ) ;
#72104 = CARTESIAN_POINT ( 'NONE',  ( -1.559171609364246924, 0.3937007874015747699, 0.6156134192599649335 ) ) ;
#72105 = CARTESIAN_POINT ( 'NONE',  ( 0.3280839895013130669, -0.004921259842519576551, 0.3153832671262227771 ) ) ;
#72106 = CARTESIAN_POINT ( 'NONE',  ( 0.5774278215223104249, 0.2306618581243848609, 0.2411417322834645549 ) ) ;
#72107 = CARTESIAN_POINT ( 'NONE',  ( 0.9120734908136489683, -0.6692913385826771977, 0.1292274648535927661 ) ) ;
#72108 = CARTESIAN_POINT ( 'NONE',  ( 0.03937007874015833325, -0.6692913385826771977, 8.415575281601705876E-17 ) ) ;
#72109 = CARTESIAN_POINT ( 'NONE',  ( -0.03937007874015669567, -0.5511811023622047445, 6.969142054262312111E-17 ) ) ;
#72110 = CARTESIAN_POINT ( 'NONE',  ( 1.213910761154856299, -0.6692913385826773087, -0.1292274648535924053 ) ) ;
#72111 = DIRECTION ( 'NONE',  ( 0.000000000000000000, 0.4999999999999998890, -0.8660254037844385966 ) ) ;
#72112 = CARTESIAN_POINT ( 'NONE',  ( -1.141732283464566011, -0.6692913385826771977, 8.415575281601705876E-17 ) ) ;
#72113 = CARTESIAN_POINT ( 'NONE',  ( 0.1998031496062994405, -0.3460692066303958092, -0.8792650918635170898 ) ) ;
#72114 = CARTESIAN_POINT ( 'NONE',  ( 0.01312335958005323398, 0.009842519685039463617, 0.3409548833797002576 ) ) ;
#72115 = CARTESIAN_POINT ( 'NONE',  ( 0.06561679790026316017, 0.05413385826771626580, -0.4176697321401330321 ) ) ;
#72116 = CARTESIAN_POINT ( 'NONE',  ( -0.8727034120734901146, -0.3162353388693405765, 0.4822834645669290543 ) ) ;
#72117 = CARTESIAN_POINT ( 'NONE',  ( -0.2624671916010490880, 0.2306618581243847221, -0.2411417322834647770 ) ) ;
#72118 = CARTESIAN_POINT ( 'NONE',  ( 0.2925321140481932369, 0.2925321140481932369, -2.500000000000000444 ) ) ;
#72119 = CARTESIAN_POINT ( 'NONE',  ( -0.3949938075777409408, -0.1058382717557502933, -1.778215223097113107 ) ) ;
#72120 = B_SPLINE_CURVE_WITH_KNOTS ( 'NONE', 3,
 ( #43457, #17824, #74661, #49783, #81387, #68342, #42645 ),
 .UNSPECIFIED., .F., .F.,
 ( 4, 3, 4 ),
 ( 1.734723475976807094E-18, 0.001246230184515569571, 0.002492489877932635954 ),
 .UNSPECIFIED. ) ;
#72121 = CARTESIAN_POINT ( 'NONE',  ( 0.3917322834645670104, -0.1049643490035303411, -0.4186351706036745557 ) ) ;
#72122 = CARTESIAN_POINT ( 'NONE',  ( -9.594673741351313045E-17, 0.3917322834645670104, -0.9370078740157480324 ) ) ;
#72123 = CARTESIAN_POINT ( 'NONE',  ( -0.8333333333333323711, -0.5511811023622048555, -0.09757992244046775898 ) ) ;
#72124 = CARTESIAN_POINT ( 'NONE',  ( 0.3392501089628018329, 0.1958661417322835607, -0.9107611548556429071 ) ) ;
#72125 = CARTESIAN_POINT ( 'NONE',  ( -1.732283464566928277, -0.1870078740157479769, 0.4822834645669291653 ) ) ;
#72126 = CARTESIAN_POINT ( 'NONE',  ( 0.3392501089628018329, 0.1958661417322835052, -0.05378645849637612303 ) ) ;
#72127 = CARTESIAN_POINT ( 'NONE',  ( 0.2624671916010504757, 0.2306618581243848609, 0.2411417322834645549 ) ) ;
#72128 = CARTESIAN_POINT ( 'NONE',  ( -0.6102362204724400829, 0.07958543189024085140, 0.2665933059059887866 ) ) ;
#72129 = CARTESIAN_POINT ( 'NONE',  ( 0.7611548556430451917, -0.6046776061558807314, 0.2411417322834647770 ) ) ;
#72130 = CARTESIAN_POINT ( 'NONE',  ( 0.3740157480314966754, 0.1660481256975883668, -0.3530559997133364547 ) ) ;
#72131 = DIRECTION ( 'NONE',  ( 0.000000000000000000, 1.000000000000000000, -0.000000000000000000 ) ) ;
#72132 = VECTOR ( 'NONE', #30551, 39.37007874015748143 ) ;
#72133 = CARTESIAN_POINT ( 'NONE',  ( 0.3996062992125986590, -0.1070741851644053111, -2.473753280839894764 ) ) ;
#72134 = CARTESIAN_POINT ( 'NONE',  ( 0.1049643490035304799, -0.3917322834645670104, -1.026922202920946825 ) ) ;
#72135 = CARTESIAN_POINT ( 'NONE',  ( 1.253280839895013710, -0.05778040916215560624, -0.4822834645669293319 ) ) ;
#72136 = VECTOR ( 'NONE', #38961, 39.37007874015748854 ) ;
#72137 = CIRCLE ( 'NONE', #65420, 0.01968503937007875723 ) ;
#72138 = CARTESIAN_POINT ( 'NONE',  ( 0.4724409448818904789, -0.1870078740157479769, 0.4822834645669291653 ) ) ;
#72139 = CARTESIAN_POINT ( 'NONE',  ( 0.2099737532808405305, 0.2306618581243847221, -0.2411417322834647770 ) ) ;
#72140 = CARTESIAN_POINT ( 'NONE',  ( 1.325459317585302665, 0.05413385826771626580, -0.4176697321401330321 ) ) ;
#72141 = CARTESIAN_POINT ( 'NONE',  ( 0.7152230971128616943, -0.05778040916215522460, 0.4822834645669289988 ) ) ;
#72142 = CARTESIAN_POINT ( 'NONE',  ( -0.1958661417322834220, -0.3392501089628018884, -0.4652230971128609727 ) ) ;
#72143 = CARTESIAN_POINT ( 'NONE',  ( 0.05249343832021075018, 0.2306618581243847221, -0.2411417322834647770 ) ) ;
#72144 = CARTESIAN_POINT ( 'NONE',  ( 0.6430446194225729606, -0.4281496062992127816, -0.4176697321401328100 ) ) ;
#72145 = CARTESIAN_POINT ( 'NONE',  ( -0.06561679790026180015, 0.05413385826771666132, 0.4176697321401328100 ) ) ;
#72146 = CARTESIAN_POINT ( 'NONE',  ( 1.220472440944882608, 0.1771653543307087630, 0.000000000000000000 ) ) ;
#72147 = CARTESIAN_POINT ( 'NONE',  ( -1.502624671916009680, -0.05778040916215560624, -0.4822834645669293319 ) ) ;
#72148 = CARTESIAN_POINT ( 'NONE',  ( -1.325459317585300889, -0.4281496062992127816, -0.4176697321401328100 ) ) ;
#72149 = CARTESIAN_POINT ( 'NONE',  ( 0.6102362204724416372, -0.5400638737290844871, 0.3530559997133364547 ) ) ;
#72150 = CARTESIAN_POINT ( 'NONE',  ( -0.02733964191563385132, -0.3913445824880820156, -1.929133858267717994 ) ) ;
#72151 = B_SPLINE_CURVE_WITH_KNOTS ( 'NONE', 3,
 ( #67659, #2445, #79469, #61324 ),
 .UNSPECIFIED., .F., .F.,
 ( 4, 4 ),
 ( 3.593986969204291827E-07, 0.001287825409103209679 ),
 .UNSPECIFIED. ) ;
#72152 = CARTESIAN_POINT ( 'NONE',  ( 0.3917322834645670104, 2.398668435337828261E-17, -2.000000000000000000 ) ) ;
#72153 = VERTEX_POINT ( 'NONE', #19188 ) ;
#72154 = CARTESIAN_POINT ( 'NONE',  ( 0.3996062992125986590, -0.1070741851644053111, -0.5839895013123358458 ) ) ;
#72155 = ORIENTED_EDGE ( 'NONE', *, *, #4418, .T. ) ;
#72156 = CARTESIAN_POINT ( 'NONE',  ( 1.049868766404200349, 0.2306618581243848609, 0.2411417322834645549 ) ) ;
#72157 = CARTESIAN_POINT ( 'NONE',  ( 1.148293963254593653, 0.1771653543307087075, -0.09757992244046823083 ) ) ;
#72158 = CARTESIAN_POINT ( 'NONE',  ( 0.6036745406824154392, 0.2306618581243847221, -0.2411417322834647770 ) ) ;
#72159 = CARTESIAN_POINT ( 'NONE',  ( -0.4477177017962782335, 1.379801381128185511, 2.610383882218336282 ) ) ;
#72160 = CARTESIAN_POINT ( 'NONE',  ( 0.4724409448818898127, -0.1265901696524988629, -1.213910761154855411 ) ) ;
#72161 = CARTESIAN_POINT ( 'NONE',  ( -0.3917322834645669549, -0.1049643490035306603, -1.390419947506561504 ) ) ;
#72162 = CARTESIAN_POINT ( 'NONE',  ( 1.128608923884514947, 0.2306618581243848609, 0.2411417322834645549 ) ) ;
#72163 = CARTESIAN_POINT ( 'NONE',  ( -1.594488188976377119, 0.1660481256975883668, -0.3530559997133364547 ) ) ;
#72164 = CARTESIAN_POINT ( 'NONE',  ( -0.2624671916010490880, 0.2306618581243847221, -0.2411417322834647770 ) ) ;
#72165 = CARTESIAN_POINT ( 'NONE',  ( 0.9383202099737536495, -0.3162353388693405765, 0.4822834645669290543 ) ) ;
#72166 = VERTEX_POINT ( 'NONE', #57480 ) ;
#72167 = CARTESIAN_POINT ( 'NONE',  ( -1.581364829396324945, -0.3162353388693405765, 0.4822834645669290543 ) ) ;
#72168 = CARTESIAN_POINT ( 'NONE',  ( 0.4824498642376759960, 1.223219560026271499E-15, 0.4445507791589056734 ) ) ;
#72169 = APPLICATION_PROTOCOL_DEFINITION ( 'draft international standard', 'automotive_design', 1998, #13801 ) ;
#72170 = CARTESIAN_POINT ( 'NONE',  ( 1.555118110236221041, 0.07958543189024071263, -0.2665933059059888421 ) ) ;
#72171 = DIRECTION ( 'NONE',  ( 0.000000000000000000, 0.000000000000000000, 1.000000000000000000 ) ) ;
#72172 = CARTESIAN_POINT ( 'NONE',  ( -1.062992125984250968, -0.5511811023622047445, 6.969142054262312111E-17 ) ) ;
#72173 = CARTESIAN_POINT ( 'NONE',  ( -1.614173228346455824, 0.2952755905511811885, 0.000000000000000000 ) ) ;
#72174 = CARTESIAN_POINT ( 'NONE',  ( 0.4790026246719168435, -0.3162353388693409650, -0.4822834645669289433 ) ) ;
#72175 = EDGE_LOOP ( 'NONE', ( #76557, #55971, #11199, #9524, #30799, #6136 ) ) ;
#72177 = FACE_OUTER_BOUND ( 'NONE', #54198, .T. ) ;
#72176 = CARTESIAN_POINT ( 'NONE',  ( -0.7426113562969628434, 2.209901789876557832, 0.5309055118110236338 ) ) ;
#72178 = CARTESIAN_POINT ( 'NONE',  ( 0.7217847769028878924, 0.05413385826771666132, 0.4176697321401328100 ) ) ;
#72179 = CARTESIAN_POINT ( 'NONE',  ( -1.548556430446193399, 0.2306618581243848609, 0.2411417322834645549 ) ) ;
#72180 = CARTESIAN_POINT ( 'NONE',  ( 0.3917322834645668994, 0.1049643490035304522, -0.9921066684701294047 ) ) ;
#72181 = CARTESIAN_POINT ( 'NONE',  ( -0.8464566929133852113, -0.4536011799217368745, -0.2665933059059886201 ) ) ;
#72182 = CARTESIAN_POINT ( 'NONE',  ( 1.627296587926509996, -0.6046776061558807314, 0.2411417322834647770 ) ) ;
#72183 = CARTESIAN_POINT ( 'NONE',  ( 0.1958661417322836440, -0.3392501089628017219, -1.121391076115485719 ) ) ;
#72184 = CARTESIAN_POINT ( 'NONE',  ( 0.5052493438320215802, 0.2952755905511811885, 0.1292274648535926551 ) ) ;
#72185 = CARTESIAN_POINT ( 'NONE',  ( -0.9055118110236215490, -0.5511811023622047445, 6.969142054262312111E-17 ) ) ;
#72186 = CARTESIAN_POINT ( 'NONE',  ( -0.03937007874015669567, -0.5511811023622047445, 6.969142054262312111E-17 ) ) ;
#72187 = EDGE_CURVE ( 'NONE', #59983, #15514, #50594, .T. ) ;
#72188 = CARTESIAN_POINT ( 'NONE',  ( -0.4986876640419942164, -0.6046776061558807314, 0.2411417322834647770 ) ) ;
#72189 = CARTESIAN_POINT ( 'NONE',  ( -1.200787401574802349, -0.4536011799217367080, 0.2665933059059888421 ) ) ;
#72190 = CARTESIAN_POINT ( 'NONE',  ( 0.2867679344610366554, 0.2867679344610366554, 0.02294656348325270490 ) ) ;
#72191 = CARTESIAN_POINT ( 'NONE',  ( 0.8333333333333340365, 0.2952755905511810774, -0.1292274648535930714 ) ) ;
#72192 = VECTOR ( 'NONE', #39390, 39.37007874015748143 ) ;
#72193 = ADVANCED_FACE ( 'NONE', ( #6982 ), #79854, .F. ) ;
#72194 = AXIS2_PLACEMENT_3D ( 'NONE', #24754, #50015, #23938 ) ;
#72195 = CARTESIAN_POINT ( 'NONE',  ( 2.516666458167341691, 2.742784437388869012, 0.5314960629921260393 ) ) ;
#72196 = STYLED_ITEM ( 'NONE', ( #29187 ), #59541 ) ;
#72197 = CARTESIAN_POINT ( 'NONE',  ( -0.4724409448818898682, -8.678599364036362592E-17, -1.690944881889763884 ) ) ;
#72198 = CIRCLE ( 'NONE', #58720, 0.3149606299212598381 ) ;
#72199 = CARTESIAN_POINT ( 'NONE',  ( -0.6496062992125976043, -0.5400638737290844871, 0.3530559997133364547 ) ) ;
#72200 = CARTESIAN_POINT ( 'NONE',  ( -0.3608923884514428360, -0.5511811023622048555, -0.09757992244046775898 ) ) ;
#72201 = CARTESIAN_POINT ( 'NONE',  ( -1.351706036745406347, -0.4281496062992124485, 0.4176697321401328655 ) ) ;
#72202 = CARTESIAN_POINT ( 'NONE',  ( 0.7020997375328090762, -0.2845877964562159024, 0.3641732283464567677 ) ) ;
#72203 = CARTESIAN_POINT ( 'NONE',  ( -0.6758530183727028406, -0.5511811023622048555, -0.09757992244046775898 ) ) ;
#72204 = CARTESIAN_POINT ( 'NONE',  ( -1.102362204724408601, -0.1870078740157479769, 0.4822834645669291653 ) ) ;
#72205 = CARTESIAN_POINT ( 'NONE',  ( -1.082677165354329896, 0.1660481256975885056, 0.3530559997133364547 ) ) ;
#72206 = CARTESIAN_POINT ( 'NONE',  ( 1.627296587926509996, -0.6046776061558807314, 0.2411417322834647770 ) ) ;
#72207 = CARTESIAN_POINT ( 'NONE',  ( -1.313877454013331780, 0.2755905511811023723, 0.7983292792091805090 ) ) ;
#72208 = CARTESIAN_POINT ( 'NONE',  ( 1.062992125984252745, 0.1771653543307087630, 0.000000000000000000 ) ) ;
#72209 = PRODUCT ( 'Independent Actuating Lead Screws', 'Independent Actuating Lead Screws', '', ( #29207 ) ) ;
#72210 = CARTESIAN_POINT ( 'NONE',  ( 0.3674540682414705883, -0.6046776061558807314, 0.2411417322834647770 ) ) ;
#72211 = CARTESIAN_POINT ( 'NONE',  ( -1.646981627296586703, -0.05778040916215522460, 0.4822834645669289988 ) ) ;
#72212 = CARTESIAN_POINT ( 'NONE',  ( -1.719160104986876103, 0.05413385826771666132, 0.4176697321401328100 ) ) ;
#72213 = ORIENTED_EDGE ( 'NONE', *, *, #45608, .T. ) ;
#72214 = CARTESIAN_POINT ( 'NONE',  ( -0.1058382717557503072, 0.3949938075777408852, 0.2316272965879264401 ) ) ;
#72215 = EDGE_CURVE ( 'NONE', #8202, #36894, #66141, .T. ) ;
#72216 = CARTESIAN_POINT ( 'NONE',  ( -1.220472440944881054, -0.5511811023622047445, 6.969142054262312111E-17 ) ) ;
#72217 = CARTESIAN_POINT ( 'NONE',  ( -0.6627296587926501115, 0.2952755905511810774, -0.1292274648535930714 ) ) ;
#72218 = CARTESIAN_POINT ( 'NONE',  ( 0.8333333333333340365, 0.2952755905511810774, -0.1292274648535930714 ) ) ;
#72219 = CARTESIAN_POINT ( 'NONE',  ( -1.535433070866141225, 0.1771653543307087630, 0.000000000000000000 ) ) ;
#72220 = CARTESIAN_POINT ( 'NONE',  ( 0.1998031496062994128, -0.3460692066303957537, -1.743438320209973913 ) ) ;
#72221 = CARTESIAN_POINT ( 'NONE',  ( -1.601049868766403650, -0.6046776061558807314, 0.2411417322834647770 ) ) ;
#72222 = CARTESIAN_POINT ( 'NONE',  ( 0.6430446194225729606, -0.4281496062992127816, -0.4176697321401328100 ) ) ;
#72223 = CARTESIAN_POINT ( 'NONE',  ( 0.6430446194225729606, -0.4281496062992127816, -0.4176697321401328100 ) ) ;
#72224 = EDGE_CURVE ( 'NONE', #16885, #48718, #60233, .T. ) ;
#72225 = CARTESIAN_POINT ( 'NONE',  ( 1.207349081364829990, -0.6046776061558809534, -0.2411417322834644161 ) ) ;
#72226 = DIRECTION ( 'NONE',  ( -0.4999999999999987788, -0.7071067811865503483, 0.4999999999999972244 ) ) ;
#72227 = CARTESIAN_POINT ( 'NONE',  ( -9.787531504996567848E-17, 0.3996062992125986035, -1.259842519685039353 ) ) ;
#72228 = CARTESIAN_POINT ( 'NONE',  ( -0.1974969037888703871, -0.3420746716998661063, -0.8530183727034120755 ) ) ;
#72229 = CARTESIAN_POINT ( 'NONE',  ( 0.4417590601942769646, 1.710972922415834097, 2.620894764083904871 ) ) ;
#72230 = CARTESIAN_POINT ( 'NONE',  ( 0.2165354330708668673, 0.07958543189024071263, -0.2665933059059888421 ) ) ;
#72231 = CARTESIAN_POINT ( 'NONE',  ( 0.05249343832021075018, 0.2306618581243847221, -0.2411417322834647770 ) ) ;
#72232 = CARTESIAN_POINT ( 'NONE',  ( 1.450131233595801428, 0.2952755905511811885, 0.1292274648535926551 ) ) ;
#72233 = CARTESIAN_POINT ( 'NONE',  ( -0.3420746716998660508, -0.1974969037888706924, -1.861548556430446588 ) ) ;
#72234 = CARTESIAN_POINT ( 'NONE',  ( 0.4133858267716541968, 0.07958543189024085140, 0.2665933059059887866 ) ) ;
#72235 = CARTESIAN_POINT ( 'NONE',  ( -0.6299212598425188991, -0.1870078740157480879, -0.4822834645669291653 ) ) ;
#72236 = CARTESIAN_POINT ( 'NONE',  ( 1.469816272965879911, 0.2306618581243847221, -0.2411417322834647770 ) ) ;
#72237 = CARTESIAN_POINT ( 'NONE',  ( 0.3215223097112867578, -0.3162353388693409650, -0.4822834645669289433 ) ) ;
#72238 = CARTESIAN_POINT ( 'NONE',  ( -0.4724409448818899238, 0.1265901696524986686, -2.080052493438320216 ) ) ;
#72239 = DIRECTION ( 'NONE',  ( 0.7071067811865462405, 2.189697074797793648E-16, 0.7071067811865486830 ) ) ;
#72240 = ORIENTED_EDGE ( 'NONE', *, *, #38275, .T. ) ;
#72241 = ORIENTED_EDGE ( 'NONE', *, *, #63554, .T. ) ;
#72242 = CARTESIAN_POINT ( 'NONE',  ( 1.463254593175853824, 0.1771653543307087075, -0.09757992244046823083 ) ) ;
#72244 = CARTESIAN_POINT ( 'NONE',  ( -1.115485564304461219, 0.05413385826771626580, -0.4176697321401330321 ) ) ;
#72243 = CARTESIAN_POINT ( 'NONE',  ( -1.194225721784776262, -0.3690944881889763329, 0.3153832671262228327 ) ) ;
#72245 = CARTESIAN_POINT ( 'NONE',  ( -0.3917322834645669549, -7.196005306013483243E-17, -2.324127665845457713 ) ) ;
#72246 = DIRECTION ( 'NONE',  ( 0.000000000000000000, 0.000000000000000000, -1.000000000000000000 ) ) ;
#72247 = CARTESIAN_POINT ( 'NONE',  ( -1.522309711286088607, -0.5023911411419708095, 0.1820866141732285504 ) ) ;
#72248 = CARTESIAN_POINT ( 'NONE',  ( -1.371391076115484831, 0.2952755905511810774, -0.1292274648535930714 ) ) ;
#72249 = CARTESIAN_POINT ( 'NONE',  ( 0.05905511811023681640, 0.1660481256975883668, -0.3530559997133364547 ) ) ;
#72250 = CARTESIAN_POINT ( 'NONE',  ( -1.364829396325458521, -0.6046776061558807314, 0.2411417322834647770 ) ) ;
#72251 = CARTESIAN_POINT ( 'NONE',  ( -0.3392501089628019439, 0.1958661417322832554, -2.783445251147295352 ) ) ;
#72252 = CARTESIAN_POINT ( 'NONE',  ( 0.6824146981627303710, 0.2306618581243847221, -0.2411417322834647770 ) ) ;
#72253 = CARTESIAN_POINT ( 'NONE',  ( -0.3917322834645669549, -0.1049643490035306603, -1.770341207349081181 ) ) ;
#72254 = CARTESIAN_POINT ( 'NONE',  ( -1.122047244094487306, 0.07958543189024071263, -0.2665933059059888421 ) ) ;
#72255 = ORIENTED_EDGE ( 'NONE', *, *, #79291, .T. ) ;
#72256 = CARTESIAN_POINT ( 'NONE',  ( 0.1058382717557499880, 0.3949938075777411073, -2.198162729658792891 ) ) ;
#72257 = ORIENTED_EDGE ( 'NONE', *, *, #18704, .T. ) ;
#72258 = CARTESIAN_POINT ( 'NONE',  ( -1.653543307086613234, -0.1870078740157480601, -0.3641732283464567677 ) ) ;
#72259 = AXIS2_PLACEMENT_3D ( 'NONE', #49239, #18099, #75757 ) ;
#72260 = CARTESIAN_POINT ( 'NONE',  ( -1.003937007874015297, -0.5400638737290845981, -0.3530559997133363437 ) ) ;
#72261 = CARTESIAN_POINT ( 'NONE',  ( -1.423884514435694859, -0.05778040916215560624, -0.4822834645669293319 ) ) ;
#72262 = CARTESIAN_POINT ( 'NONE',  ( -0.3996062992125986035, -7.340648628747425578E-17, -0.6692913385826770867 ) ) ;
#72263 = CARTESIAN_POINT ( 'NONE',  ( 0.4177787735907000366, 0.3937007874015748254, -1.559171609364239375 ) ) ;
#72264 = CARTESIAN_POINT ( 'NONE',  ( -1.660104986876639543, -0.05778040916215560624, -0.4822834645669293319 ) ) ;
#72265 = CARTESIAN_POINT ( 'NONE',  ( -1.292650918635170010, 0.2952755905511810774, -0.1292274648535930714 ) ) ;
#72266 = CARTESIAN_POINT ( 'NONE',  ( 0.03178304480586199854, -0.3983403474834772418, -9.560572922657961637E-16 ) ) ;
#72267 = CARTESIAN_POINT ( 'NONE',  ( -1.614173228346456712, 0.7166040191147899918, -0.1372047244094478091 ) ) ;
#72268 = CARTESIAN_POINT ( 'NONE',  ( 0.05905511811023709395, -0.4536011799217367080, 0.2665933059059888421 ) ) ;
#72269 = CARTESIAN_POINT ( 'NONE',  ( -0.3917322834645670104, -7.196005306013484475E-17, -0.4389763779527560139 ) ) ;
#72270 = CARTESIAN_POINT ( 'NONE',  ( -0.7020997375328076329, -0.2845877964562161244, -0.3641732283464567121 ) ) ;
#72271 = CARTESIAN_POINT ( 'NONE',  ( -0.7283464566929126471, -0.5400638737290844871, 0.3530559997133364547 ) ) ;
#72272 = CARTESIAN_POINT ( 'NONE',  ( 0.7414698162729663755, -0.6692913385826773087, -0.1292274648535924053 ) ) ;
#72273 = CARTESIAN_POINT ( 'NONE',  ( -1.108923884514435132, -0.05778040916215560624, -0.4822834645669293319 ) ) ;
#72274 = EDGE_LOOP ( 'NONE', ( #21111, #67686, #55968, #32341, #67558, #73418, #49467, #22565, #41419, #64483, #45925, #62699 ) ) ;
#72275 = ORIENTED_EDGE ( 'NONE', *, *, #62163, .T. ) ;
#72276 = B_SPLINE_CURVE_WITH_KNOTS ( 'NONE', 3,
 ( #21456, #47114, #72803, #15990, #67328, #15152, #66918 ),
 .UNSPECIFIED., .F., .F.,
 ( 4, 3, 4 ),
 ( 1.232595164407830946E-32, 0.001246232571205310594, 0.002492492258783241162 ),
 .UNSPECIFIED. ) ;
#72277 = CARTESIAN_POINT ( 'NONE',  ( -0.9055118110236215490, -0.6692913385826771977, 8.415575281601705876E-17 ) ) ;
#72278 = CARTESIAN_POINT ( 'NONE',  ( 0.9317585301837276734, -0.4281496062992124485, 0.4176697321401328655 ) ) ;
#72279 = CARTESIAN_POINT ( 'NONE',  ( -1.640419947506561060, -0.3690944881889765550, -0.3153832671262227771 ) ) ;
#72280 = CARTESIAN_POINT ( 'NONE',  ( -1.719160104986876103, 0.05413385826771666132, 0.4176697321401328100 ) ) ;
#72281 = CARTESIAN_POINT ( 'NONE',  ( -0.1265901696524986964, -0.4724409448818899238, -1.332020997375328086 ) ) ;
#72282 = EDGE_CURVE ( 'NONE', #52658, #76474, #12196, .T. ) ;
#72283 = CARTESIAN_POINT ( 'NONE',  ( 2.165607527688952594, 1.494646310179101656, -0.4725519687354808873 ) ) ;
#72284 = CARTESIAN_POINT ( 'NONE',  ( 0.1958661417322834775, 0.3392501089628018884, -0.4514435695538057125 ) ) ;
#72285 = CARTESIAN_POINT ( 'NONE',  ( 0.3392501089628018884, -0.1958661417322834220, -2.394356955380577467 ) ) ;
#72286 = CARTESIAN_POINT ( 'NONE',  ( -0.4855643044619415427, 0.05413385826771626580, -0.4176697321401330321 ) ) ;
#72287 = CARTESIAN_POINT ( 'NONE',  ( -1.391076115485563314, -0.5023911411419708095, -0.1820866141732282451 ) ) ;
#72288 = CARTESIAN_POINT ( 'NONE',  ( -0.2925321140481930149, -0.2925321140481933480, 0.02165354330708658959 ) ) ;
#72290 = CARTESIAN_POINT ( 'NONE',  ( 2.795275590551181466, 1.023622047244095556, -2.156651478620225655E-16 ) ) ;
#72289 = CARTESIAN_POINT ( 'NONE',  ( -1.207349081364828880, 0.2306618581243847221, -0.2411417322834647770 ) ) ;
#72291 = CARTESIAN_POINT ( 'NONE',  ( -1.345144356955379816, -0.05778040916215560624, -0.4822834645669293319 ) ) ;
#72292 = CARTESIAN_POINT ( 'NONE',  ( -0.2362204724409442680, -0.1870078740157480879, -0.4822834645669291653 ) ) ;
#72293 = CARTESIAN_POINT ( 'NONE',  ( -0.1974969037888704149, -0.3420746716998661063, -2.819553805774278388 ) ) ;
#72294 = CARTESIAN_POINT ( 'NONE',  ( 0.5118110236220478892, 0.1771653543307087630, 0.000000000000000000 ) ) ;
#72295 = CARTESIAN_POINT ( 'NONE',  ( -9.594673741351313045E-17, 0.3917322834645670104, -0.08464566929133868212 ) ) ;
#72296 = CARTESIAN_POINT ( 'NONE',  ( 0.4133858267716541968, 0.07958543189024085140, 0.2665933059059887866 ) ) ;
#72297 = CARTESIAN_POINT ( 'NONE',  ( 1.548556430446194954, -0.5023911411419708095, 0.1820866141732285504 ) ) ;
#72298 = CARTESIAN_POINT ( 'NONE',  ( 0.7742782152230978099, -0.4281496062992124485, 0.4176697321401328655 ) ) ;
#72299 = CARTESIAN_POINT ( 'NONE',  ( -0.01968503937007793844, 0.07958543189024071263, -0.2665933059059888421 ) ) ;
#72300 = CARTESIAN_POINT ( 'NONE',  ( 0.2867679344610365999, 0.2867679344610365999, -1.862204724409449064 ) ) ;
#72301 = CARTESIAN_POINT ( 'NONE',  ( -1.482939632545930975, 0.05413385826771666132, 0.4176697321401328100 ) ) ;
#72302 = CARTESIAN_POINT ( 'NONE',  ( -0.07874015748031421014, -0.1870078740157480601, -0.3641732283464567677 ) ) ;
#72303 = CARTESIAN_POINT ( 'NONE',  ( -1.476377952755905110, 0.07958543189024085140, 0.2665933059059887866 ) ) ;
#72304 = CARTESIAN_POINT ( 'NONE',  ( -0.1265901696524993347, 0.4724409448818895907, -0.2408136482939632061 ) ) ;
#72305 = CARTESIAN_POINT ( 'NONE',  ( -0.5905511811023613777, -0.5511811023622047445, 6.969142054262312111E-17 ) ) ;
#72306 = CARTESIAN_POINT ( 'NONE',  ( 0.4411264095795432993, 1.362677836172179635, -1.627053844800393501 ) ) ;
#72307 = CARTESIAN_POINT ( 'NONE',  ( -0.09842519685039295696, -0.5400638737290844871, 0.3530559997133364547 ) ) ;
#72308 = CARTESIAN_POINT ( 'NONE',  ( -1.017203447268042016, 1.569595554511555857, -0.4735931522784879721 ) ) ;
#72309 = CARTESIAN_POINT ( 'NONE',  ( 0.4396325459317590445, -0.5511811023622046335, 0.09757992244046803654 ) ) ;
#72310 = CARTESIAN_POINT ( 'NONE',  ( -0.1771653543307080136, -0.4536011799217367080, 0.2665933059059888421 ) ) ;
#72311 = CARTESIAN_POINT ( 'NONE',  ( -0.3937007874015740483, -0.1870078740157479769, 0.4822834645669291653 ) ) ;
#72312 = FACE_OUTER_BOUND ( 'NONE', #56711, .T. ) ;
#72313 = CARTESIAN_POINT ( 'NONE',  ( -0.9186351706036736120, -0.5023911411419708095, -0.1820866141732282451 ) ) ;
#72314 = CARTESIAN_POINT ( 'NONE',  ( 0.1265901696524989184, 0.4724409448818898127, -1.959973753280839892 ) ) ;
#72315 = CARTESIAN_POINT ( 'NONE',  ( 0.7677165354330716118, 0.1660481256975883668, -0.3530559997133364547 ) ) ;
#72316 = CARTESIAN_POINT ( 'NONE',  ( -0.8136482939632537770, 0.2306618581243847221, -0.2411417322834647770 ) ) ;
#72317 = CARTESIAN_POINT ( 'NONE',  ( 0.3460692066303959202, -0.1998031496062991630, -1.599081364829396223 ) ) ;
#72318 = ADVANCED_FACE ( 'NONE', ( #66557 ), #58560, .T. ) ;
#72319 = CARTESIAN_POINT ( 'NONE',  ( -0.3917322834645669549, -0.1049643490035306603, -2.807742782152229832 ) ) ;
#72320 = CARTESIAN_POINT ( 'NONE',  ( -0.3412073490813641308, -0.5023911411419708095, 0.1820866141732285504 ) ) ;
#72321 = CARTESIAN_POINT ( 'NONE',  ( -1.417322834645668772, -0.1870078740157480879, -0.4822834645669291653 ) ) ;
#72322 = CARTESIAN_POINT ( 'NONE',  ( -1.036745406824146176, -0.3690944881889763329, 0.3153832671262228327 ) ) ;
#72323 = FACE_OUTER_BOUND ( 'NONE', #67719, .T. ) ;
#72324 = CARTESIAN_POINT ( 'NONE',  ( -0.9842519685039360366, 0.1771653543307087630, 0.000000000000000000 ) ) ;
#72325 = FACE_OUTER_BOUND ( 'NONE', #77330, .T. ) ;
#72326 = CARTESIAN_POINT ( 'NONE',  ( 0.9580052493438326877, 0.05413385826771666132, 0.4176697321401328100 ) ) ;
#72327 = CARTESIAN_POINT ( 'NONE',  ( 0.1998031496062992740, 0.3460692066303959757, 0.01312335958005248458 ) ) ;
#72328 = CARTESIAN_POINT ( 'NONE',  ( -0.1958661417322833942, -0.3392501089628018884, -2.582040313157166977 ) ) ;
#72329 = DIRECTION ( 'NONE',  ( 0.000000000000000000, -0.000000000000000000, 1.000000000000000000 ) ) ;
#72330 = CARTESIAN_POINT ( 'NONE',  ( 1.443569553805774897, 0.1283753931104748280, 0.1820866141732283561 ) ) ;
#72331 = CARTESIAN_POINT ( 'NONE',  ( -1.148293963254592542, -0.6692913385826773087, -0.1292274648535924053 ) ) ;
#72332 = CARTESIAN_POINT ( 'NONE',  ( 1.318897637795276356, 0.1660481256975883668, -0.3530559997133364547 ) ) ;
#72333 = CARTESIAN_POINT ( 'NONE',  ( 0.1049643490035303689, 0.3917322834645670104, -2.597769028871390606 ) ) ;
#72334 = CARTESIAN_POINT ( 'NONE',  ( 1.509186351706037543, -0.004921259842519576551, 0.3153832671262227771 ) ) ;
#72335 = CARTESIAN_POINT ( 'NONE',  ( 0.3280839895013130669, -0.4281496062992127816, -0.4176697321401328100 ) ) ;
#72336 = CARTESIAN_POINT ( 'NONE',  ( -0.5708661417322825615, -0.5400638737290844871, 0.3530559997133364547 ) ) ;
#72337 = CARTESIAN_POINT ( 'NONE',  ( 1.541994750656168645, 0.2952755905511810774, -0.1292274648535930714 ) ) ;
#72338 = CARTESIAN_POINT ( 'NONE',  ( 3.890345922373659615, 2.716830163678111365, 0.5314960629921260393 ) ) ;
#72339 = CARTESIAN_POINT ( 'NONE',  ( 0.8333333333333340365, 0.1771653543307087075, -0.09757992244046823083 ) ) ;
#72340 = EDGE_CURVE ( 'NONE', #24792, #19878, #67362, .T. ) ;
#72341 = CARTESIAN_POINT ( 'NONE',  ( -0.1998031496062991907, -0.3460692066303959757, -1.640419947506561726 ) ) ;
#72342 = ORIENTED_EDGE ( 'NONE', *, *, #40988, .F. ) ;
#72343 = CARTESIAN_POINT ( 'NONE',  ( 0.3917322834645670104, 0.1049643490035304660, -0.2788907068579546400 ) ) ;
#72344 = ORIENTED_EDGE ( 'NONE', *, *, #10031, .T. ) ;
#72345 = CARTESIAN_POINT ( 'NONE',  ( -0.3805774278215216522, -0.4281496062992127816, -0.4176697321401328100 ) ) ;
#72346 = CARTESIAN_POINT ( 'NONE',  ( 1.522309711286089939, -0.6046776061558809534, -0.2411417322834644161 ) ) ;
#72347 = CARTESIAN_POINT ( 'NONE',  ( 0.2427821522309719648, -0.05778040916215522460, 0.4822834645669289988 ) ) ;
#72348 = CARTESIAN_POINT ( 'NONE',  ( -0.4068241469816264999, -0.3690944881889763329, 0.3153832671262228327 ) ) ;
#72349 = CARTESIAN_POINT ( 'NONE',  ( 1.122047244094488860, -0.5400638737290845981, -0.3530559997133363437 ) ) ;
#72350 = EDGE_CURVE ( 'NONE', #32475, #22642, #2264, .T. ) ;
#72351 = CARTESIAN_POINT ( 'NONE',  ( -0.6233595800524928121, -0.3162353388693409650, -0.4822834645669289433 ) ) ;
#72352 = CARTESIAN_POINT ( 'NONE',  ( 0.2296587926509192634, -0.05778040916215560624, -0.4822834645669293319 ) ) ;
#72353 = CARTESIAN_POINT ( 'NONE',  ( -1.561679790026246017, -0.4281496062992127816, -0.4176697321401328100 ) ) ;
#72354 = CARTESIAN_POINT ( 'NONE',  ( 0.8661417322834652488, -0.1870078740157480879, -0.4822834645669291653 ) ) ;
#72355 = CARTESIAN_POINT ( 'NONE',  ( 1.049868766404200349, 0.2306618581243848609, 0.2411417322834645549 ) ) ;
#72356 = CARTESIAN_POINT ( 'NONE',  ( 0.3917322834645670104, 2.398668435337828261E-17, -0.5826771653543306728 ) ) ;
#72357 = CARTESIAN_POINT ( 'NONE',  ( 0.1574803149606306130, -0.1870078740157480601, -0.3641732283464567677 ) ) ;
#72358 = ORIENTED_EDGE ( 'NONE', *, *, #38868, .T. ) ;
#72359 = CARTESIAN_POINT ( 'NONE',  ( 0.3949938075777409408, 0.1058382717557500574, -1.069553805774278388 ) ) ;
#72360 = ORIENTED_EDGE ( 'NONE', *, *, #25498, .T. ) ;
#72361 = CARTESIAN_POINT ( 'NONE',  ( -0.2624671916010490880, 0.1283753931104746893, -0.1820866141732285504 ) ) ;
#72362 = CARTESIAN_POINT ( 'NONE',  ( 0.1574803149606306130, -0.1870078740157480879, -0.4822834645669291653 ) ) ;
#72363 = CARTESIAN_POINT ( 'NONE',  ( -1.407440972164865967, 1.192216805462484874, 0.3257083040380834293 ) ) ;
#72364 = CARTESIAN_POINT ( 'NONE',  ( -0.2755905511811018171, 0.2952755905511811885, 0.000000000000000000 ) ) ;
#72365 = CARTESIAN_POINT ( 'NONE',  ( -0.4330708661417315697, 0.2952755905511811885, 0.000000000000000000 ) ) ;
#72366 = CARTESIAN_POINT ( 'NONE',  ( -0.8333333333333323711, 0.2952755905511811885, 0.1292274648535926551 ) ) ;
#72367 = CARTESIAN_POINT ( 'NONE',  ( -1.207349081364828880, 0.2306618581243847221, -0.2411417322834647770 ) ) ;
#72368 = CARTESIAN_POINT ( 'NONE',  ( 1.391076115485564868, 0.1283753931104746893, -0.1820866141732285504 ) ) ;
#72369 = FACE_OUTER_BOUND ( 'NONE', #9169, .T. ) ;
#72370 = CARTESIAN_POINT ( 'NONE',  ( 1.614173228346457378, 0.7166040191147859950, -0.1372047244094476148 ) ) ;
#72371 = CARTESIAN_POINT ( 'NONE',  ( 1.082677165354331228, -0.4536011799217367080, 0.2665933059059888421 ) ) ;
#72372 = CARTESIAN_POINT ( 'NONE',  ( 0.5774278215223104249, 0.2306618581243848609, 0.2411417322834645549 ) ) ;
#72373 = CARTESIAN_POINT ( 'NONE',  ( 0.2034120734908144990, -0.6692913385826771977, 0.1292274648535927661 ) ) ;
#72374 = CARTESIAN_POINT ( 'NONE',  ( -0.2925321140481930704, -0.2925321140481933480, -1.161417322834645383 ) ) ;
#72375 = CARTESIAN_POINT ( 'NONE',  ( -2.554262525012222174, 1.537401574803149984, 0.4744094488188970171 ) ) ;
#72376 = CARTESIAN_POINT ( 'NONE',  ( -0.2925321140481932369, 0.2925321140481931259, -0.7263779527559056648 ) ) ;
#72377 = CARTESIAN_POINT ( 'NONE',  ( -0.3996062992125986590, 0.1070741851644051723, -0.7395013123359580609 ) ) ;
#72378 = CARTESIAN_POINT ( 'NONE',  ( -0.6364829396325453192, -0.3162353388693405765, 0.4822834645669290543 ) ) ;
#72379 = CARTESIAN_POINT ( 'NONE',  ( -0.4091458600556405756, 0.2362204724409446288, -0.1837270341207349056 ) ) ;
#72380 = CARTESIAN_POINT ( 'NONE',  ( -0.1958661417322834220, -0.3392501089628018884, -2.197506561679789971 ) ) ;
#72381 = CARTESIAN_POINT ( 'NONE',  ( -1.187664041994749731, -0.2845877964562159024, 0.3641732283464567677 ) ) ;
#72382 = CARTESIAN_POINT ( 'NONE',  ( 0.8661417322834652488, -0.1870078740157480879, -0.4822834645669291653 ) ) ;
#72383 = CARTESIAN_POINT ( 'NONE',  ( 0.9317585301837276734, 0.05413385826771626580, -0.4176697321401330321 ) ) ;
#72384 = CARTESIAN_POINT ( 'NONE',  ( -0.3805774278215216522, -0.004921259842519576551, 0.3153832671262227771 ) ) ;
#72385 = CARTESIAN_POINT ( 'NONE',  ( 0.5577427821522314977, -0.3162353388693409650, -0.4822834645669289433 ) ) ;
#72386 = CARTESIAN_POINT ( 'NONE',  ( -0.2362204724409451284, 0.4091458600556402425, -1.822178477690288512 ) ) ;
#72387 = CARTESIAN_POINT ( 'NONE',  ( 0.06561679790026316017, -0.3690944881889763329, 0.3153832671262228327 ) ) ;
#72388 = CARTESIAN_POINT ( 'NONE',  ( -0.2427821522309703550, -0.05778040916215560624, -0.4822834645669293319 ) ) ;
#72389 = CARTESIAN_POINT ( 'NONE',  ( 0.1974969037888706092, -0.3420746716998660508, -1.585958005249344493 ) ) ;
#72390 = CARTESIAN_POINT ( 'NONE',  ( -1.732283464566928277, -0.1870078740157479769, 0.4822834645669291653 ) ) ;
#72391 = CARTESIAN_POINT ( 'NONE',  ( 0.5446194225721792126, -0.08942795157528024563, -0.3641732283464568787 ) ) ;
#72392 = CARTESIAN_POINT ( 'NONE',  ( 1.391076115485564868, 0.1283753931104746893, -0.1820866141732285504 ) ) ;
#72393 = CARTESIAN_POINT ( 'NONE',  ( -0.5774278215223089816, 0.2306618581243847221, -0.2411417322834647770 ) ) ;
#72394 = CARTESIAN_POINT ( 'NONE',  ( -0.5380577427821514602, -0.004921259842519576551, 0.3153832671262227771 ) ) ;
#72395 = CARTESIAN_POINT ( 'NONE',  ( 1.080276388343102000E-18, 0.000000000000000000, -0.1771653543307086798 ) ) ;
#72396 = CARTESIAN_POINT ( 'NONE',  ( -0.7283464566929126471, 0.1660481256975883668, -0.3530559997133364547 ) ) ;
#72398 = B_SPLINE_CURVE_WITH_KNOTS ( 'NONE', 3,
 ( #18033, #76513, #62220, #12125 ),
 .UNSPECIFIED., .F., .F.,
 ( 4, 4 ),
 ( 0.000000000000000000, 0.001510660848375622615 ),
 .UNSPECIFIED. ) ;
#72397 = CARTESIAN_POINT ( 'NONE',  ( -0.5118110236220466680, 0.2952755905511811885, 0.000000000000000000 ) ) ;
#72399 = CARTESIAN_POINT ( 'NONE',  ( -0.1706036745406816491, 0.05413385826771626580, -0.4176697321401330321 ) ) ;
#72400 = CARTESIAN_POINT ( 'NONE',  ( 0.3460692066303958092, 0.1998031496062993018, -2.570209973753280863 ) ) ;
#72401 = CARTESIAN_POINT ( 'NONE',  ( 4.797336870675655290E-17, -0.3917322834645669549, -1.891056799703724645 ) ) ;
#72402 = CARTESIAN_POINT ( 'NONE',  ( -1.901964908973693635, 1.119136672863556559, -0.2244172274864991157 ) ) ;
#72403 = CARTESIAN_POINT ( 'NONE',  ( 0.7349081364829403995, 0.1283753931104748280, 0.1820866141732283561 ) ) ;
#72404 = CARTESIAN_POINT ( 'NONE',  ( 1.194225721784777594, -0.4281496062992127816, -0.4176697321401328100 ) ) ;
#72405 = CARTESIAN_POINT ( 'NONE',  ( -1.410761154855642463, -0.08942795157527998196, 0.3641732283464567121 ) ) ;
#72406 = CARTESIAN_POINT ( 'NONE',  ( -1.141732283464566011, -0.5511811023622047445, 6.969142054262312111E-17 ) ) ;
#72407 = CARTESIAN_POINT ( 'NONE',  ( -0.7086614173228339419, -0.1870078740157480879, -0.4822834645669291653 ) ) ;
#72408 = CARTESIAN_POINT ( 'NONE',  ( -0.03280839895013062252, 0.1771653543307087075, -0.09757992244046823083 ) ) ;
#72409 = CARTESIAN_POINT ( 'NONE',  ( -0.2917607380149855878, 0.04688787658492848259, 5.873221924710888331 ) ) ;
#72410 = CARTESIAN_POINT ( 'NONE',  ( 1.240157480314961314, -0.4536011799217367080, 0.2665933059059888421 ) ) ;
#72411 = CARTESIAN_POINT ( 'NONE',  ( 0.2821522309711292364, 0.2952755905511810774, -0.1292274648535930714 ) ) ;
#72412 = CARTESIAN_POINT ( 'NONE',  ( -0.3996062992125984925, -0.1070741851644056858, 0.1922572178477690297 ) ) ;
#72413 = CARTESIAN_POINT ( 'NONE',  ( -0.6036745406824141069, 0.2306618581243848609, 0.2411417322834645549 ) ) ;
#72414 = CARTESIAN_POINT ( 'NONE',  ( 0.3917322834645670104, -0.1049643490035303411, -1.613517060367454237 ) ) ;
#72415 = CARTESIAN_POINT ( 'NONE',  ( 1.607611548556431069, 0.1771653543307087630, 0.09757992244046791164 ) ) ;
#72416 = CARTESIAN_POINT ( 'NONE',  ( 0.6692913385826778638, -0.6692913385826771977, 8.415575281601705876E-17 ) ) ;
#72417 = CARTESIAN_POINT ( 'NONE',  ( -0.006561679790025524116, -0.05778040916215560624, -0.4822834645669293319 ) ) ;
#72418 = CARTESIAN_POINT ( 'NONE',  ( 0.01312335958005323398, -0.3690944881889765550, -0.3153832671262227771 ) ) ;
#72419 = CARTESIAN_POINT ( 'NONE',  ( 1.586052503253845503, 1.023622047244095556, 0.1653254495020588799 ) ) ;
#72420 = CARTESIAN_POINT ( 'NONE',  ( -0.2362204724409440182, -0.1870078740157479769, 0.3641732283464567677 ) ) ;
#72421 = CARTESIAN_POINT ( 'NONE',  ( 0.7808398950131241190, -0.05778040916215560624, -0.4822834645669293319 ) ) ;
#72422 = CARTESIAN_POINT ( 'NONE',  ( -0.6102362204724400829, 0.07958543189024085140, 0.2665933059059887866 ) ) ;
#72423 = CARTESIAN_POINT ( 'NONE',  ( 0.1070741851644054776, -0.3996062992125984925, -0.9494750656167976199 ) ) ;
#72424 = CARTESIAN_POINT ( 'NONE',  ( -0.9711286089238838626, 0.2306618581243847221, -0.2411417322834647770 ) ) ;
#72425 = CARTESIAN_POINT ( 'NONE',  ( 0.1968503937007881344, 0.2066929133858268208, 0.000000000000000000 ) ) ;
#72426 = ORIENTED_EDGE ( 'NONE', *, *, #58379, .F. ) ;
#72427 = CARTESIAN_POINT ( 'NONE',  ( -1.017060367454067249, -0.05778040916215522460, 0.4822834645669289988 ) ) ;
#72428 = CARTESIAN_POINT ( 'NONE',  ( -1.023622047244094002, -0.1870078740157480601, -0.3641732283464567677 ) ) ;
#72429 = CARTESIAN_POINT ( 'NONE',  ( 0.1706036745406830368, 0.05413385826771666132, 0.4176697321401328100 ) ) ;
#72430 = CARTESIAN_POINT ( 'NONE',  ( -1.581364829396324945, -0.3162353388693405765, 0.4822834645669290543 ) ) ;
#72431 = CARTESIAN_POINT ( 'NONE',  ( -0.6364829396325453192, -0.05778040916215560624, -0.4822834645669293319 ) ) ;
#72432 = CARTESIAN_POINT ( 'NONE',  ( 0.4744094488189052328, 1.546091976385118638, -2.170146923806634653 ) ) ;
#72434 = CARTESIAN_POINT ( 'NONE',  ( 0.7283464566929140904, -0.5400638737290845981, -0.3530559997133363437 ) ) ;
#72433 = CARTESIAN_POINT ( 'NONE',  ( -0.5314960629921122726, 2.559055118110236560, -3.937007874015763687 ) ) ;
#72435 = CARTESIAN_POINT ( 'NONE',  ( 1.069553805774278832, 0.2952755905511810774, -0.1292274648535930714 ) ) ;
#72436 = CARTESIAN_POINT ( 'NONE',  ( 0.1958661417322836440, -0.3392501089628017219, -2.288713910761154935 ) ) ;
#72437 = CARTESIAN_POINT ( 'NONE',  ( 1.614173228346457378, 0.2952755905511811885, 0.000000000000000000 ) ) ;
#72438 = CARTESIAN_POINT ( 'NONE',  ( -1.220472440944881054, 0.2952755905511811885, 0.000000000000000000 ) ) ;
#72439 = ADVANCED_FACE ( 'NONE', ( #79200 ), #35855, .T. ) ;
#72440 = CARTESIAN_POINT ( 'NONE',  ( -0.3996062992125987146, 0.1070741851644051862, -0.6627296587926508886 ) ) ;
#72441 = ORIENTED_EDGE ( 'NONE', *, *, #19638, .T. ) ;
#72442 = CARTESIAN_POINT ( 'NONE',  ( -0.3543307086614165824, 0.1771653543307087630, 0.000000000000000000 ) ) ;
#72443 = CARTESIAN_POINT ( 'NONE',  ( -0.3917322834645670104, -7.196005306013484475E-17, -2.236220472440944906 ) ) ;
#72444 = VERTEX_POINT ( 'NONE', #39626 ) ;
#72445 = CARTESIAN_POINT ( 'NONE',  ( 0.2493438320209980519, -0.4281496062992127816, -0.4176697321401328100 ) ) ;
#72446 = CARTESIAN_POINT ( 'NONE',  ( 0.1771653543307093182, 0.1660481256975885056, 0.3530559997133364547 ) ) ;
#72447 = CARTESIAN_POINT ( 'NONE',  ( -0.8070866141732276899, 0.1660481256975883668, -0.3530559997133364547 ) ) ;
#72448 = CARTESIAN_POINT ( 'NONE',  ( 1.469816272965879911, -0.6046776061558807314, 0.2411417322834647770 ) ) ;
#72449 = CARTESIAN_POINT ( 'NONE',  ( -1.043307086614172041, -0.4536011799217367080, 0.2665933059059888421 ) ) ;
#72450 = CARTESIAN_POINT ( 'NONE',  ( 0.04809640131873983010, 1.065410365535384596, -1.583836855790661913 ) ) ;
#72451 = CARTESIAN_POINT ( 'NONE',  ( 0.7283464566929143125, 0.1660481256975885056, 0.3530559997133364547 ) ) ;
#72452 = CARTESIAN_POINT ( 'NONE',  ( 0.4396325459317590445, -0.5511811023622046335, 0.09757992244046803654 ) ) ;
#72453 = CARTESIAN_POINT ( 'NONE',  ( -0.4790026246719152336, -0.05778040916215560624, -0.4822834645669293319 ) ) ;
#72454 = CARTESIAN_POINT ( 'NONE',  ( -0.2867679344610366554, 0.2867679344610365444, -1.044600106790339433 ) ) ;
#72455 = CARTESIAN_POINT ( 'NONE',  ( -1.358267716535432434, -0.5400638737290844871, 0.3530559997133364547 ) ) ;
#72456 = CARTESIAN_POINT ( 'NONE',  ( -1.548556430446193399, 0.1283753931104748280, 0.1820866141732283561 ) ) ;
#72457 = CARTESIAN_POINT ( 'NONE',  ( 1.305774278215223960, -0.6692913385826771977, 0.1292274648535927661 ) ) ;
#72458 = CYLINDRICAL_SURFACE ( 'NONE', #5999, 0.4921259842519685179 ) ;
#72459 = ORIENTED_EDGE ( 'NONE', *, *, #1460, .T. ) ;
#72460 = CARTESIAN_POINT ( 'NONE',  ( -0.1958661417322836995, 0.3392501089628017219, -2.529546874836956949 ) ) ;
#72461 = CARTESIAN_POINT ( 'NONE',  ( -0.05905511811023545637, 0.1660481256975885056, 0.3530559997133364547 ) ) ;
#72462 = VERTEX_POINT ( 'NONE', #21516 ) ;
#72463 = CARTESIAN_POINT ( 'NONE',  ( 0.7349081364829402885, -0.5023911411419708095, -0.1820866141732282451 ) ) ;
#72464 = CARTESIAN_POINT ( 'NONE',  ( -1.384514435695537005, 0.2952755905511811885, 0.1292274648535926551 ) ) ;
#72465 = CARTESIAN_POINT ( 'NONE',  ( 1.148293963254593653, 0.2952755905511810774, -0.1292274648535930714 ) ) ;
#72466 = CARTESIAN_POINT ( 'NONE',  ( 1.207349081364829990, -0.6046776061558809534, -0.2411417322834644161 ) ) ;
#72467 = CARTESIAN_POINT ( 'NONE',  ( 0.1771653543307093182, 0.1660481256975885056, 0.3530559997133364547 ) ) ;
#72468 = CARTESIAN_POINT ( 'NONE',  ( -0.4330708661417315697, -0.6692913385826771977, 8.415575281601705876E-17 ) ) ;
#72469 = CARTESIAN_POINT ( 'NONE',  ( -0.3392501089628017219, -0.1958661417322836718, -1.711942257217847763 ) ) ;
#72470 = CARTESIAN_POINT ( 'NONE',  ( -1.351706036745406347, 0.05413385826771626580, -0.4176697321401330321 ) ) ;
#72471 = CARTESIAN_POINT ( 'NONE',  ( -0.7742782152230962556, -0.4281496062992127816, -0.4176697321401328100 ) ) ;
#72472 = CARTESIAN_POINT ( 'NONE',  ( -0.4724409448818890911, -0.1870078740157480601, -0.3641732283464567677 ) ) ;
#72473 = CARTESIAN_POINT ( 'NONE',  ( 2.556891461833387336, 2.729656616209943376, -0.5314960629921260393 ) ) ;
#72474 = CARTESIAN_POINT ( 'NONE',  ( -0.4724409448818890911, -0.1870078740157479769, 0.4822834645669291653 ) ) ;
#72475 = CARTESIAN_POINT ( 'NONE',  ( -1.191111281560509383, -2.567464376874931580E-15, -0.4445507791589072832 ) ) ;
#72476 = CARTESIAN_POINT ( 'NONE',  ( 0.5971128608923890191, -0.6692913385826771977, 0.1292274648535927661 ) ) ;
#72477 = CARTESIAN_POINT ( 'NONE',  ( -0.3460692066303960868, 0.1998031496062990242, -1.916010498687664043 ) ) ;
#72478 = PLANE ( 'NONE',  #67131 ) ;
#72479 = CARTESIAN_POINT ( 'NONE',  ( -0.1049868766404193215, -0.6046776061558807314, 0.2411417322834647770 ) ) ;
#72481 = CARTESIAN_POINT ( 'NONE',  ( -0.9120734908136473029, 0.2066929133858267931, 0.1054918080437490802 ) ) ;
#72480 = CARTESIAN_POINT ( 'NONE',  ( 0.8267716535433078384, -0.5511811023622047445, 6.969142054262312111E-17 ) ) ;
#72482 = CARTESIAN_POINT ( 'NONE',  ( -0.1265901696524986964, -0.4724409448818899238, -0.7788713910761155823 ) ) ;
#72483 = CARTESIAN_POINT ( 'NONE',  ( 1.312335958005250269, -0.5023911411419708095, 0.1820866141732285504 ) ) ;
#72484 = CARTESIAN_POINT ( 'NONE',  ( 1.115485564304462551, 0.05413385826771666132, 0.4176697321401328100 ) ) ;
#72485 = CARTESIAN_POINT ( 'NONE',  ( 0.2891555358219910499, -0.2891555358219909944, -0.01771653543307087977 ) ) ;
#72486 = CARTESIAN_POINT ( 'NONE',  ( -0.2362204724409442680, -0.1870078740157480879, -0.4822834645669291653 ) ) ;
#72487 = DIRECTION ( 'NONE',  ( 1.000000000000000000, 0.000000000000000000, 0.000000000000000000 ) ) ;
#72488 = CARTESIAN_POINT ( 'NONE',  ( -1.706036745406823485, 0.2306618581243848609, 0.2411417322834645549 ) ) ;
#72489 = CARTESIAN_POINT ( 'NONE',  ( -0.2952755905511804668, 0.1660481256975885056, 0.3530559997133364547 ) ) ;
#72490 = CARTESIAN_POINT ( 'NONE',  ( 0.2891555358219910499, 0.2891555358219910499, -0.6870078740157480324 ) ) ;
#72491 = CARTESIAN_POINT ( 'NONE',  ( 1.161417322834646493, -0.5400638737290844871, 0.3530559997133364547 ) ) ;
#72492 = CARTESIAN_POINT ( 'NONE',  ( 0.6036745406824153282, -0.6046776061558807314, 0.2411417322834647770 ) ) ;
#72493 = CARTESIAN_POINT ( 'NONE',  ( 0.8005249343832028242, -0.3690944881889765550, -0.3153832671262227771 ) ) ;
#72494 = CARTESIAN_POINT ( 'NONE',  ( 0.3128952852777661664, 1.406554901604258889, 0.008038607527843355527 ) ) ;
#72495 = CARTESIAN_POINT ( 'NONE',  ( 0.5118110236220480003, -0.5511811023622047445, 6.969142054262312111E-17 ) ) ;
#72496 = CARTESIAN_POINT ( 'NONE',  ( -1.089942661822471459, 0.000000000000000000, 0.3464511005275205946 ) ) ;
#72497 = CARTESIAN_POINT ( 'NONE',  ( -0.3460692066303957537, -0.1998031496062994405, -1.389107611548556553 ) ) ;
#72498 = CARTESIAN_POINT ( 'NONE',  ( 0.6036745406824154392, 0.2306618581243847221, -0.2411417322834647770 ) ) ;
#72499 = CARTESIAN_POINT ( 'NONE',  ( -0.3917322834645671215, 0.1049643490035301469, -0.4973753280839895430 ) ) ;
#72501 = CARTESIAN_POINT ( 'NONE',  ( -0.4677827689124922084, 0.03937007874015747977, -2.154527559055118946 ) ) ;
#72500 = CARTESIAN_POINT ( 'NONE',  ( 0.2034120734908144990, -0.6692913385826771977, 0.1292274648535927661 ) ) ;
#72502 = CARTESIAN_POINT ( 'NONE',  ( -0.3499960723095488779, 0.3045081538226084295, -0.01928741089222630462 ) ) ;
#72503 = CARTESIAN_POINT ( 'NONE',  ( 0.6167979002624678353, -0.3690944881889763329, 0.3153832671262228327 ) ) ;
#72504 = CARTESIAN_POINT ( 'NONE',  ( 0.3608923884514443348, -0.6692913385826771977, 0.1292274648535927661 ) ) ;
#72505 = CARTESIAN_POINT ( 'NONE',  ( -0.4697171261336051673, 1.606100245667703819, 2.158884350236656591 ) ) ;
#72506 = CARTESIAN_POINT ( 'NONE',  ( -0.9383202099737524282, -0.08942795157527998196, 0.3641732283464567121 ) ) ;
#72507 = CARTESIAN_POINT ( 'NONE',  ( -1.115485564304461219, -0.4281496062992124485, 0.4176697321401328655 ) ) ;
#72508 = CARTESIAN_POINT ( 'NONE',  ( -1.443569553805773564, -0.6046776061558807314, 0.2411417322834647770 ) ) ;
#72509 = CARTESIAN_POINT ( 'NONE',  ( 0.4461942257217856311, 0.2306618581243847221, -0.2411417322834647770 ) ) ;
#72510 = CARTESIAN_POINT ( 'NONE',  ( -1.568241469816272105, -0.2845877964562161244, -0.3641732283464567121 ) ) ;
#72511 = DIRECTION ( 'NONE',  ( 0.000000000000000000, 0.000000000000000000, -1.000000000000000000 ) ) ;
#72512 = CARTESIAN_POINT ( 'NONE',  ( 0.6364829396325465405, -0.05778040916215522460, 0.4822834645669289988 ) ) ;
#72513 = CARTESIAN_POINT ( 'NONE',  ( 0.3460692066303958092, 0.1998031496062993018, 0.1069553805774277888 ) ) ;
#72514 = CARTESIAN_POINT ( 'NONE',  ( 0.000000000000000000, 0.7086614173228346081, 0.000000000000000000 ) ) ;
#72515 = CARTESIAN_POINT ( 'NONE',  ( 1.469816272965879911, -0.6046776061558807314, 0.2411417322834647770 ) ) ;
#72516 = B_SPLINE_CURVE_WITH_KNOTS ( 'NONE', 3,
 ( #78167, #46569, #13351, #13772 ),
 .UNSPECIFIED., .F., .F.,
 ( 4, 4 ),
 ( 3.593986969189856797E-07, 0.001287825409103297717 ),
 .UNSPECIFIED. ) ;
#72517 = CARTESIAN_POINT ( 'NONE',  ( -1.404199475065615932, -0.004921259842519576551, 0.3153832671262227771 ) ) ;
#72518 = CARTESIAN_POINT ( 'NONE',  ( 1.240157480314961314, 0.07958543189024071263, -0.2665933059059888421 ) ) ;
#72519 = CARTESIAN_POINT ( 'NONE',  ( -1.358267716535432434, -0.4536011799217367080, 0.2665933059059888421 ) ) ;
#72520 = CARTESIAN_POINT ( 'NONE',  ( -0.6824146981627288167, 0.1283753931104748280, 0.1820866141732283561 ) ) ;
#72521 = CARTESIAN_POINT ( 'NONE',  ( 1.607611548556431069, 0.2952755905511811885, 0.1292274648535926551 ) ) ;
#72522 = CARTESIAN_POINT ( 'NONE',  ( 0.5183727034120741983, 0.1771653543307087075, -0.09757992244046823083 ) ) ;
#72523 = CARTESIAN_POINT ( 'NONE',  ( 0.03937007874015833325, -0.6692913385826771977, 8.415575281601705876E-17 ) ) ;
#72524 = CARTESIAN_POINT ( 'NONE',  ( 1.279527559055118724, 0.1660481256975885056, 0.3530559997133364547 ) ) ;
#72525 = CARTESIAN_POINT ( 'NONE',  ( 0.1574803149606306130, -0.1870078740157480879, -0.4822834645669291653 ) ) ;
#72526 = CARTESIAN_POINT ( 'NONE',  ( 0.2690288713910767848, -0.5511811023622048555, -0.09757992244046775898 ) ) ;
#72527 = CARTESIAN_POINT ( 'NONE',  ( 1.410761154855643795, -0.3162353388693405765, 0.4822834645669290543 ) ) ;
#72528 = ADVANCED_FACE ( 'NONE', ( #64881 ), #26405, .F. ) ;
#72529 =( BOUNDED_CURVE ( )  B_SPLINE_CURVE ( 2, ( #19469, #40088, #6425, #65775, #32094, #51433, #77136, #6840, #45119, #58173, #80891, #74157, #67843 ),
 .UNSPECIFIED., .F., .F. ) 
 B_SPLINE_CURVE_WITH_KNOTS ( ( 3, 2, 2, 2, 2, 2, 3 ),
 ( 0.7308514478433235650, 0.7310606060606060774, 0.7348484848484848619, 0.7386363636363636465, 0.7424242424242424310, 0.7462121212121212155, 0.7464212794294037279 ),
 .UNSPECIFIED. ) 
 CURVE ( )  GEOMETRIC_REPRESENTATION_ITEM ( )  RATIONAL_B_SPLINE_CURVE ( ( 0.9964447847208419695, 0.9981185001348091834, 1.000000000000000000, 0.9659258262890683122, 1.000000000000000000, 0.9659258262890683122, 1.000000000000000000, 0.9659258262890683122, 1.000000000000000000, 0.9659258262890683122, 1.000000000000000000, 0.9981185001348091834, 0.9964447847208420805 ) ) 
 REPRESENTATION_ITEM ( '' )  );
#72530 = CARTESIAN_POINT ( 'NONE',  ( -0.2165354330708654795, 0.1012011053420777407, 0.2882089793578256898 ) ) ;
#72531 = CARTESIAN_POINT ( 'NONE',  ( -0.9317585301837263412, 0.05413385826771666132, 0.4176697321401328100 ) ) ;
#72532 = CARTESIAN_POINT ( 'NONE',  ( 0.3460692066303959757, -0.1998031496062991907, -0.7349081364829396223 ) ) ;
#72533 = CARTESIAN_POINT ( 'NONE',  ( 0.3458507752293908943, 0.3458507752293908943, -1.159448818897637734 ) ) ;
#72534 = CARTESIAN_POINT ( 'NONE',  ( -0.9383202099737524282, -0.3162353388693409650, -0.4822834645669289433 ) ) ;
#72535 = CARTESIAN_POINT ( 'NONE',  ( -0.07217847769028813698, -0.3162353388693409650, -0.4822834645669289433 ) ) ;
#72536 = CARTESIAN_POINT ( 'NONE',  ( -0.1998031496062991907, -0.3460692066303959757, -2.585301837270341352 ) ) ;
#72537 = CARTESIAN_POINT ( 'NONE',  ( -9.674558042662121740E-17, 0.3949938075777409963, -1.889763779527559029 ) ) ;
#72538 = CARTESIAN_POINT ( 'NONE',  ( -0.1049643490035307020, 0.3917322834645669549, -0.6286089238845143923 ) ) ;
#72539 = EDGE_CURVE ( 'NONE', #2386, #70474, #23761, .T. ) ;
#72540 = DIRECTION ( 'NONE',  ( 0.000000000000000000, 0.000000000000000000, -1.000000000000000000 ) ) ;
#72541 = CARTESIAN_POINT ( 'NONE',  ( -1.456692913385826182, -0.5511811023622047445, 6.969142054262312111E-17 ) ) ;
#72542 = CARTESIAN_POINT ( 'NONE',  ( 0.3917322834645670104, -0.1049643490035303411, -0.8910761154855640909 ) ) ;
#72543 = CARTESIAN_POINT ( 'NONE',  ( -1.699475065616797398, 0.2952755905511811885, 0.1292274648535926551 ) ) ;
#72544 = CARTESIAN_POINT ( 'NONE',  ( -0.3392501089628018329, -0.1958661417322836440, 0.02495369898393883651 ) ) ;
#72545 = CARTESIAN_POINT ( 'NONE',  ( 0.3871391076115493490, -0.3162353388693405765, 0.4822834645669290543 ) ) ;
#72546 = CARTESIAN_POINT ( 'NONE',  ( -0.6430446194225716283, -0.3690944881889763329, 0.3153832671262228327 ) ) ;
#72547 = CARTESIAN_POINT ( 'NONE',  ( 0.9383202099737536495, -0.3162353388693405765, 0.4822834645669290543 ) ) ;
#72548 = CARTESIAN_POINT ( 'NONE',  ( 0.2821522309711292364, -0.6692913385826771977, 0.1292274648535927661 ) ) ;
#72549 = CARTESIAN_POINT ( 'NONE',  ( -0.4359958488159647039, 1.724409448818897905, -2.094141031014960408 ) ) ;
#72550 = CARTESIAN_POINT ( 'NONE',  ( -0.3996062992125987146, 0.1070741851644051862, -2.395013123359580387 ) ) ;
#72551 = CARTESIAN_POINT ( 'NONE',  ( 0.1958661417322834775, 0.3392501089628018884, -1.243457635991812582 ) ) ;
#72552 = CARTESIAN_POINT ( 'NONE',  ( 1.286089238845145033, -0.6046776061558809534, -0.2411417322834644161 ) ) ;
#72553 = CARTESIAN_POINT ( 'NONE',  ( 0.02624671916010564918, 0.2306618581243848609, 0.2411417322834645549 ) ) ;
#72554 = CARTESIAN_POINT ( 'NONE',  ( 1.482939632545932307, 0.05413385826771626580, -0.4176697321401330321 ) ) ;
#72555 = CARTESIAN_POINT ( 'NONE',  ( 0.7742782152230979209, 0.05413385826771626580, -0.4176697321401330321 ) ) ;
#72556 = CARTESIAN_POINT ( 'NONE',  ( -0.1049643490035302024, -0.3917322834645671215, -0.4717847769028871152 ) ) ;
#72557 = CARTESIAN_POINT ( 'NONE',  ( 0.1181102362204730916, -0.6692913385826771977, 8.415575281601705876E-17 ) ) ;
#72558 = CARTESIAN_POINT ( 'NONE',  ( 0.6758530183727039509, -0.6692913385826771977, 0.1292274648535927661 ) ) ;
#72559 = CARTESIAN_POINT ( 'NONE',  ( 0.01968503937007957949, -0.5400638737290845981, -0.3530559997133363437 ) ) ;
#72560 = CARTESIAN_POINT ( 'NONE',  ( 0.8989501312335964611, 0.1771653543307087630, 0.09757992244046791164 ) ) ;
#72561 = CARTESIAN_POINT ( 'NONE',  ( -1.325459317585300889, -0.4281496062992127816, -0.4176697321401328100 ) ) ;
#72562 = CARTESIAN_POINT ( 'NONE',  ( -1.601049868766403650, -0.6046776061558807314, 0.2411417322834647770 ) ) ;
#72563 = CARTESIAN_POINT ( 'NONE',  ( 0.8136482939632553313, 0.2306618581243848609, 0.2411417322834645549 ) ) ;
#72564 = CARTESIAN_POINT ( 'NONE',  ( 0.06766049032769154425, -0.3859888145975187701, -1.929133858267717549 ) ) ;
#72565 = CARTESIAN_POINT ( 'NONE',  ( -9.594673741351313045E-17, 0.3917322834645670104, -1.724409448818897683 ) ) ;
#72566 = ORIENTED_EDGE ( 'NONE', *, *, #15170, .F. ) ;
#72567 = CARTESIAN_POINT ( 'NONE',  ( 0.2925321140481932369, -0.2925321140481932369, -0.2559055118110236116 ) ) ;
#72568 = ORIENTED_EDGE ( 'NONE', *, *, #61281, .T. ) ;
#72569 = CARTESIAN_POINT ( 'NONE',  ( 1.115485564304462551, -0.4281496062992127816, -0.4176697321401328100 ) ) ;
#72570 = CARTESIAN_POINT ( 'NONE',  ( 0.3740157480314966754, 0.07958543189024071263, -0.2665933059059888421 ) ) ;
#72571 = DIRECTION ( 'NONE',  ( -0.000000000000000000, 1.000000000000000000, 0.000000000000000000 ) ) ;
#72572 = DIRECTION ( 'NONE',  ( -0.000000000000000000, -1.000000000000000000, -0.000000000000000000 ) ) ;
#72573 = CARTESIAN_POINT ( 'NONE',  ( -0.4359958488159582091, 1.724409448818897905, -3.937007874015763687 ) ) ;
#72574 = CARTESIAN_POINT ( 'NONE',  ( 0.2867679344610365999, -0.2867679344610365444, -1.127952755905512028 ) ) ;
#72575 = CARTESIAN_POINT ( 'NONE',  ( 1.482939632545932307, 0.05413385826771626580, -0.4176697321401330321 ) ) ;
#72576 = CARTESIAN_POINT ( 'NONE',  ( 0.4744094488189112280, 1.569730808353063445, -3.908320185825790993 ) ) ;
#72577 = CARTESIAN_POINT ( 'NONE',  ( -0.2034120734908131112, -0.6692913385826773087, -0.1292274648535924053 ) ) ;
#72578 = CARTESIAN_POINT ( 'NONE',  ( 1.181102362204724976, -0.1870078740157480879, -0.4822834645669291653 ) ) ;
#72579 = ORIENTED_EDGE ( 'NONE', *, *, #32099, .F. ) ;
#72580 = CARTESIAN_POINT ( 'NONE',  ( -1.489501312335957062, -0.3162353388693409650, -0.4822834645669289433 ) ) ;
#72581 = CARTESIAN_POINT ( 'NONE',  ( -39.19291338582677753, 5.691349986800547090E-15, 0.000000000000000000 ) ) ;
#72582 = DIRECTION ( 'NONE',  ( 0.4570218192499936327, 0.000000000000000000, -0.8894554832758219121 ) ) ;
#72583 = CARTESIAN_POINT ( 'NONE',  ( 1.541994750656168645, 0.1771653543307087075, -0.09757992244046823083 ) ) ;
#72584 = DIRECTION ( 'NONE',  ( 1.000000000000000000, 0.000000000000000000, 0.000000000000000000 ) ) ;
#72585 = B_SPLINE_CURVE_WITH_KNOTS ( 'NONE', 3,
 ( #53086, #65333, #33749, #51831 ),
 .UNSPECIFIED., .F., .F.,
 ( 4, 4 ),
 ( 1.999999999897049408E-07, 0.006970199999999935128 ),
 .UNSPECIFIED. ) ;
#72586 = CARTESIAN_POINT ( 'NONE',  ( -1.076115485564303809, -0.5023911411419708095, -0.1820866141732282451 ) ) ;
#72587 = CARTESIAN_POINT ( 'NONE',  ( -1.496062992125983815, -0.1870078740157479769, 0.4822834645669291653 ) ) ;
#72588 = CARTESIAN_POINT ( 'NONE',  ( 0.6692913385826778638, -0.6692913385826771977, 8.415575281601705876E-17 ) ) ;
#72589 = ORIENTED_EDGE ( 'NONE', *, *, #44487, .F. ) ;
#72591 = CARTESIAN_POINT ( 'NONE',  ( -0.4330708661417315697, 0.2066929133858268208, 0.000000000000000000 ) ) ;
#72590 = CARTESIAN_POINT ( 'NONE',  ( 1.437007874015748810, -0.5400638737290845981, -0.3530559997133363437 ) ) ;
#72592 = CARTESIAN_POINT ( 'NONE',  ( -0.7283464566929126471, 0.07958543189024071263, -0.2665933059059888421 ) ) ;
#72593 = CARTESIAN_POINT ( 'NONE',  ( 0.7414698162729663755, 0.2952755905511811885, 0.1292274648535926551 ) ) ;
#72594 = CARTESIAN_POINT ( 'NONE',  ( -1.712598425196849572, 0.1660481256975885056, 0.3530559997133364547 ) ) ;
#72595 = CARTESIAN_POINT ( 'NONE',  ( 0.1049643490035304522, -0.3917322834645668994, -1.267697219651231499 ) ) ;
#72596 = CARTESIAN_POINT ( 'NONE',  ( -0.9383202099737524282, -0.08942795157527998196, 0.3641732283464567121 ) ) ;
#72597 = ADVANCED_FACE ( 'NONE', ( #10554 ), #16047, .T. ) ;
#72598 = CARTESIAN_POINT ( 'NONE',  ( -1.410761154855641575, -0.2845877964562161244, -0.3641732283464567121 ) ) ;
#72599 = CARTESIAN_POINT ( 'NONE',  ( -1.559171609364246924, 0.3937007874015748254, 0.4177787735906735578 ) ) ;
#72600 = CARTESIAN_POINT ( 'NONE',  ( 0.4790026246719167324, -0.05778040916215522460, 0.4822834645669289988 ) ) ;
#72601 = CARTESIAN_POINT ( 'NONE',  ( -1.010498687664041384, -0.004921259842519576551, 0.3153832671262227771 ) ) ;
#72602 = CARTESIAN_POINT ( 'NONE',  ( -0.1968503937007867743, -0.5511811023622047445, 6.969142054262312111E-17 ) ) ;
#72603 = CARTESIAN_POINT ( 'NONE',  ( -0.3740157480314953431, -0.5400638737290845981, -0.3530559997133363437 ) ) ;
#72604 = CARTESIAN_POINT ( 'NONE',  ( 1.620734908136483465, -0.6692913385826771977, 0.1292274648535927661 ) ) ;
#72605 = CARTESIAN_POINT ( 'NONE',  ( 0.1958661417322836718, -0.3392501089628017219, -0.2460823079078234277 ) ) ;
#72606 = CARTESIAN_POINT ( 'NONE',  ( 0.5643044619422579178, -0.4281496062992127816, -0.4176697321401328100 ) ) ;
#72607 = CARTESIAN_POINT ( 'NONE',  ( 2.795275590551181466, 2.165354330708662012, 0.000000000000000000 ) ) ;
#72608 = CARTESIAN_POINT ( 'NONE',  ( 0.2362204724409449064, 0.4091458600556404646, -1.480971128608923548 ) ) ;
#72609 = CARTESIAN_POINT ( 'NONE',  ( -0.6430446194225716283, -0.4281496062992124485, 0.4176697321401328655 ) ) ;
#72610 = CARTESIAN_POINT ( 'NONE',  ( -0.2755905511811018171, 0.1771653543307087630, 0.000000000000000000 ) ) ;
#72611 = CARTESIAN_POINT ( 'NONE',  ( -1.312335958005248715, 0.2306618581243848609, 0.2411417322834645549 ) ) ;
#72612 = CARTESIAN_POINT ( 'NONE',  ( 0.5511811023622055217, -0.1870078740157479769, 0.3641732283464567677 ) ) ;
#72613 = CARTESIAN_POINT ( 'NONE',  ( -0.8333333333333323711, -0.5511811023622048555, -0.09757992244046775898 ) ) ;
#72614 = CARTESIAN_POINT ( 'NONE',  ( -1.240157480314959759, 0.1660481256975885056, 0.3530559997133364547 ) ) ;
#72615 = CARTESIAN_POINT ( 'NONE',  ( -1.555118110236219930, 0.1660481256975885056, 0.3530559997133364547 ) ) ;
#72616 = CARTESIAN_POINT ( 'NONE',  ( -1.450131233595799651, 0.2952755905511810774, -0.1292274648535930714 ) ) ;
#72617 = FACE_OUTER_BOUND ( 'NONE', #20157, .T. ) ;
#72618 = CARTESIAN_POINT ( 'NONE',  ( 0.9055118110236227702, 0.1771653543307087630, 0.000000000000000000 ) ) ;
#72619 = CARTESIAN_POINT ( 'NONE',  ( 0.4133858267716541968, 0.1660481256975885056, 0.3530559997133364547 ) ) ;
#72620 = CYLINDRICAL_SURFACE ( 'NONE', #75716, 3.937007874015748143 ) ;
#72621 = CARTESIAN_POINT ( 'NONE',  ( 1.476377952755906220, 0.07958543189024071263, -0.2665933059059888421 ) ) ;
#72622 = EDGE_LOOP ( 'NONE', ( #37772, #13780, #37937, #9315 ) ) ;
#72623 = CARTESIAN_POINT ( 'NONE',  ( 0.3996062992125985480, 2.446882876249141654E-17, -2.872047244094488416 ) ) ;
#72624 = CARTESIAN_POINT ( 'NONE',  ( -1.286089238845143479, 0.1283753931104746893, -0.1820866141732285504 ) ) ;
#72625 = CARTESIAN_POINT ( 'NONE',  ( -0.5118110236220466680, 0.2952755905511811885, 0.000000000000000000 ) ) ;
#72626 = CARTESIAN_POINT ( 'NONE',  ( 0.2952755905511816326, -0.5400638737290844871, 0.3530559997133364547 ) ) ;
#72627 = CARTESIAN_POINT ( 'NONE',  ( -1.404199475065615932, -0.004921259842519576551, 0.3153832671262227771 ) ) ;
#72628 = CARTESIAN_POINT ( 'NONE',  ( -0.2925321140481930149, -0.2925321140481933480, -1.710629921259842812 ) ) ;
#72629 = CARTESIAN_POINT ( 'NONE',  ( -1.476377952755905110, -0.5400638737290845981, -0.3530559997133363437 ) ) ;
#72630 = CARTESIAN_POINT ( 'NONE',  ( 0.6233595800524942554, -0.05778040916215560624, -0.4822834645669293319 ) ) ;
#72631 = CARTESIAN_POINT ( 'NONE',  ( 0.07874015748031558404, -0.1870078740157479769, 0.4822834645669291653 ) ) ;
#72632 = CARTESIAN_POINT ( 'NONE',  ( 1.227034120734908917, -0.6692913385826771977, 0.1292274648535927661 ) ) ;
#72633 = LINE ( 'NONE', #14576, #21125 ) ;
#72634 = CARTESIAN_POINT ( 'NONE',  ( 0.3996062992125986035, 0.1070741851644054776, -1.384514435695537671 ) ) ;
#72635 = CARTESIAN_POINT ( 'NONE',  ( 4.837279021331060870E-17, -0.3949938075777409963, -0.7086614173228346081 ) ) ;
#72636 = CARTESIAN_POINT ( 'NONE',  ( 0.1049643490035303689, 0.3917322834645670104, -0.1430446194225721279 ) ) ;
#72637 = CARTESIAN_POINT ( 'NONE',  ( -0.3018372703412066094, -0.004921259842519576551, 0.3153832671262227771 ) ) ;
#72638 = CARTESIAN_POINT ( 'NONE',  ( -0.4396325459317579898, 0.2952755905511811885, 0.1292274648535926551 ) ) ;
#72639 = CARTESIAN_POINT ( 'NONE',  ( 0.9580052493438326877, 0.05413385826771666132, 0.4176697321401328100 ) ) ;
#72640 = CARTESIAN_POINT ( 'NONE',  ( 0.3949938075777409408, -0.1058382717557499186, -1.920603674540682260 ) ) ;
#72641 = CARTESIAN_POINT ( 'NONE',  ( -0.05905511811023545637, 0.07958543189024085140, 0.2665933059059887866 ) ) ;
#72642 = CARTESIAN_POINT ( 'NONE',  ( -1.279527559055116948, 0.1660481256975883668, -0.3530559997133364547 ) ) ;
#72643 = CARTESIAN_POINT ( 'NONE',  ( -1.456692913385826182, 0.2952755905511811885, 0.000000000000000000 ) ) ;
#72644 = CARTESIAN_POINT ( 'NONE',  ( 0.4091458600556404646, -0.2362204724409448231, -1.837270341207349000 ) ) ;
#72645 = CARTESIAN_POINT ( 'NONE',  ( 0.3588842212257977726, 0.1584414948821297187, -2.755905511811021835 ) ) ;
#72646 = ORIENTED_EDGE ( 'NONE', *, *, #45034, .F. ) ;
#72647 = ORIENTED_EDGE ( 'NONE', *, *, #48636, .T. ) ;
#72648 = CARTESIAN_POINT ( 'NONE',  ( 1.338582677165355062, -0.1870078740157480879, -0.4822834645669291653 ) ) ;
#72649 = CARTESIAN_POINT ( 'NONE',  ( -1.607611548556429737, -0.6692913385826771977, 0.1292274648535927661 ) ) ;
#72651 = CARTESIAN_POINT ( 'NONE',  ( -1.286089238845143479, 0.2306618581243847221, -0.2411417322834647770 ) ) ;
#72650 = CARTESIAN_POINT ( 'NONE',  ( -1.220472440944881054, -0.5511811023622047445, 6.969142054262312111E-17 ) ) ;
#72652 = CARTESIAN_POINT ( 'NONE',  ( -0.2867679344610366554, 0.2867679344610365444, -2.461922941436009094 ) ) ;
#72653 = CARTESIAN_POINT ( 'NONE',  ( 0.2486400153428833526, 3.421639014772782816E-16, 0.3464511005275203726 ) ) ;
#72654 = CARTESIAN_POINT ( 'NONE',  ( 1.049868766404200349, 0.2306618581243848609, 0.2411417322834645549 ) ) ;
#72655 = CARTESIAN_POINT ( 'NONE',  ( -1.653543307086613234, -0.1870078740157480879, -0.4822834645669291653 ) ) ;
#72656 = CARTESIAN_POINT ( 'NONE',  ( -0.2230971128608915943, -0.4281496062992127816, -0.4176697321401328100 ) ) ;
#72657 = CARTESIAN_POINT ( 'NONE',  ( -0.02624671916010428221, -0.6046776061558807314, 0.2411417322834647770 ) ) ;
#72658 = ADVANCED_FACE ( 'NONE', ( #35804 ), #80850, .T. ) ;
#72659 = VECTOR ( 'NONE', #9631, 39.37007874015748854 ) ;
#72660 = CARTESIAN_POINT ( 'NONE',  ( -1.423884514435694859, -0.05778040916215560624, -0.4822834645669293319 ) ) ;
#72661 = CARTESIAN_POINT ( 'NONE',  ( -0.3917322834645669549, -7.196005306013483243E-17, -2.796568610727347082 ) ) ;
#72662 = CARTESIAN_POINT ( 'NONE',  ( 0.6955380577427828781, 0.05413385826771626580, -0.4176697321401330321 ) ) ;
#72663 = CARTESIAN_POINT ( 'NONE',  ( -9.594673741351313045E-17, 0.3917322834645670104, -1.724409448818897683 ) ) ;
#72664 = CARTESIAN_POINT ( 'NONE',  ( -1.286089238845143479, 0.1283753931104746893, -0.1820866141732285504 ) ) ;
#72665 = EDGE_LOOP ( 'NONE', ( #59590, #17296, #76281, #38488 ) ) ;
#72666 = CARTESIAN_POINT ( 'NONE',  ( -0.1974969037888703871, -0.3420746716998661063, -2.427821522309711266 ) ) ;
#72667 = ORIENTED_EDGE ( 'NONE', *, *, #8579, .F. ) ;
#72668 = DIRECTION ( 'NONE',  ( 0.000000000000000000, -1.000000000000000000, 0.000000000000000000 ) ) ;
#72669 = CARTESIAN_POINT ( 'NONE',  ( -0.9973753280839886548, -0.6046776061558809534, -0.2411417322834644161 ) ) ;
#72670 = CARTESIAN_POINT ( 'NONE',  ( -1.404199475065615932, -0.4281496062992127816, -0.4176697321401328100 ) ) ;
#72671 = CARTESIAN_POINT ( 'NONE',  ( -0.1070741851644056997, 0.3996062992125986035, -0.7939632545931758489 ) ) ;
#72672 = CARTESIAN_POINT ( 'NONE',  ( -1.587926509186350810, -0.4281496062992124485, 0.4176697321401328655 ) ) ;
#72673 = CARTESIAN_POINT ( 'NONE',  ( -1.496062992125983815, -0.1870078740157480879, -0.4822834645669291653 ) ) ;
#72674 = DIRECTION ( 'NONE',  ( -1.000000000000000000, -3.083952846180990281E-16, 0.000000000000000000 ) ) ;
#72675 = CARTESIAN_POINT ( 'NONE',  ( -0.3249695492770445782, -2.567464376874931580E-15, -0.4445507791589072832 ) ) ;
#72676 = CARTESIAN_POINT ( 'NONE',  ( -0.1958661417322836718, 0.3392501089628017219, -0.09776902887139117537 ) ) ;
#72677 = CARTESIAN_POINT ( 'NONE',  ( -0.04593175853018302557, 0.1771653543307087630, 0.09757992244046791164 ) ) ;
#72678 = CARTESIAN_POINT ( 'NONE',  ( 0.1958661417322836440, -0.3392501089628017219, -0.6489501312335959060 ) ) ;
#72679 = CARTESIAN_POINT ( 'NONE',  ( -0.9514435695538050464, -0.2845877964562159024, 0.3641732283464567677 ) ) ;
#72680 = CARTESIAN_POINT ( 'NONE',  ( -1.312335958005248715, 0.2306618581243848609, 0.2411417322834645549 ) ) ;
#72681 = CARTESIAN_POINT ( 'NONE',  ( 0.9383202099737536495, -0.3162353388693405765, 0.4822834645669290543 ) ) ;
#72682 = CARTESIAN_POINT ( 'NONE',  ( -0.7152230971128602510, -0.3162353388693405765, 0.4822834645669290543 ) ) ;
#72683 = CARTESIAN_POINT ( 'NONE',  ( 0.5314960629921396951, 2.687614851728676424, -3.900966923095589234 ) ) ;
#72684 = ORIENTED_EDGE ( 'NONE', *, *, #66179, .F. ) ;
#72685 = CARTESIAN_POINT ( 'NONE',  ( -1.437007874015747477, 0.1660481256975883668, -0.3530559997133364547 ) ) ;
#72686 = CARTESIAN_POINT ( 'NONE',  ( 0.8464566929133865436, 0.1660481256975883668, -0.3530559997133364547 ) ) ;
#72687 = CARTESIAN_POINT ( 'NONE',  ( -1.450131233595799651, -0.5511811023622046335, 0.09757992244046803654 ) ) ;
#72688 = CARTESIAN_POINT ( 'NONE',  ( -0.1150178391344491569, 1.057423598266512332, 0.2689098498627903733 ) ) ;
#72689 = CARTESIAN_POINT ( 'NONE',  ( 0.4724409448818896462, 0.1265901696524990294, -1.069553805774278166 ) ) ;
#72690 = CARTESIAN_POINT ( 'NONE',  ( 1.923433685342916144, 1.142877263639046959, -0.2639061591570168175 ) ) ;
#72691 = ADVANCED_FACE ( 'NONE', ( #55965 ), #74115, .F. ) ;
#72692 = CARTESIAN_POINT ( 'NONE',  ( -0.3917322834645670104, -7.196005306013484475E-17, -0.8188976377952754682 ) ) ;
#72693 = CARTESIAN_POINT ( 'NONE',  ( -0.1958661417322836718, 0.3392501089628017219, -2.617454068241469756 ) ) ;
#72694 = CARTESIAN_POINT ( 'NONE',  ( -0.4133858267716528645, -0.5400638737290844871, 0.3530559997133364547 ) ) ;
#72695 = CARTESIAN_POINT ( 'NONE',  ( -1.325459317585300889, -0.004921259842519576551, 0.3153832671262227771 ) ) ;
#72696 = CARTESIAN_POINT ( 'NONE',  ( -0.1070741851644056997, 0.3996062992125984925, -0.2408136482939632061 ) ) ;
#72698 = CARTESIAN_POINT ( 'NONE',  ( -0.4668652553835747621, 1.622068519643040219, 2.571961977011489875 ) ) ;
#72697 = CARTESIAN_POINT ( 'NONE',  ( -1.706036745406823485, 0.2306618581243848609, 0.2411417322834645549 ) ) ;
#72699 = CARTESIAN_POINT ( 'NONE',  ( -1.266404199475064773, -0.3162353388693405765, 0.4822834645669290543 ) ) ;
#72700 = CARTESIAN_POINT ( 'NONE',  ( -0.4068241469816267775, 0.05413385826771626580, -0.4176697321401330321 ) ) ;
#72701 = CARTESIAN_POINT ( 'NONE',  ( -0.3392501089628019439, 0.1958661417322832554, 0.05120041814404382302 ) ) ;
#72702 = CARTESIAN_POINT ( 'NONE',  ( 0.4133858267716541968, -0.4536011799217368745, -0.2665933059059886201 ) ) ;
#72703 = DIRECTION ( 'NONE',  ( 1.000000000000000000, 0.000000000000000000, 0.000000000000000000 ) ) ;
#72704 = CARTESIAN_POINT ( 'NONE',  ( 0.4527559055118117182, 0.07958543189024071263, -0.2665933059059888421 ) ) ;
#72705 = CARTESIAN_POINT ( 'NONE',  ( 0.9055118110236227702, -0.5511811023622047445, 6.969142054262312111E-17 ) ) ;
#72706 = CARTESIAN_POINT ( 'NONE',  ( 0.9186351706036751663, -0.6046776061558807314, 0.2411417322834647770 ) ) ;
#72707 = CARTESIAN_POINT ( 'NONE',  ( 0.1771653543307093182, -0.4536011799217368745, -0.2665933059059886201 ) ) ;
#72708 = CARTESIAN_POINT ( 'NONE',  ( 0.3917322834645669549, 0.1049643490035304660, -2.006561679790026531 ) ) ;
#72709 = CARTESIAN_POINT ( 'NONE',  ( -1.351706036745406347, -0.4281496062992124485, 0.4176697321401328655 ) ) ;
#72710 = CARTESIAN_POINT ( 'NONE',  ( 0.06561679790026316017, -0.004921259842519870586, -0.3153832671262229437 ) ) ;
#72711 = CARTESIAN_POINT ( 'NONE',  ( -1.404199475065615932, -0.3690944881889765550, -0.3153832671262227771 ) ) ;
#72712 = CARTESIAN_POINT ( 'NONE',  ( -0.4724409448818895907, -0.1265901696524993070, -0.4376640419947506744 ) ) ;
#72713 = CARTESIAN_POINT ( 'NONE',  ( -1.010498687664041384, -0.004921259842519576551, 0.3153832671262227771 ) ) ;
#72714 = CARTESIAN_POINT ( 'NONE',  ( -0.4744094488188934089, 1.553403318890016482, -1.016821367227985329 ) ) ;
#72715 = CARTESIAN_POINT ( 'NONE',  ( -0.1574803149606292529, -0.1870078740157480879, -0.4822834645669291653 ) ) ;
#72716 = LINE ( 'NONE', #47024, #66680 ) ;
#72717 = CARTESIAN_POINT ( 'NONE',  ( 0.4330708661417329575, -0.5511811023622047445, 6.969142054262312111E-17 ) ) ;
#72718 = CARTESIAN_POINT ( 'NONE',  ( -0.4068241469816267775, -0.004921259842519870586, -0.3153832671262229437 ) ) ;
#72719 = CARTESIAN_POINT ( 'NONE',  ( -0.2887139107611542133, -0.6046776061558809534, -0.2411417322834644161 ) ) ;
#72720 = CARTESIAN_POINT ( 'NONE',  ( -1.679790026246718693, 0.2306618581243847221, -0.2411417322834647770 ) ) ;
#72721 = CARTESIAN_POINT ( 'NONE',  ( -1.187664041994749731, -0.2845877964562159024, 0.3641732283464567677 ) ) ;
#72722 = CARTESIAN_POINT ( 'NONE',  ( 0.000000000000000000, 0.000000000000000000, -1.929133858267716661 ) ) ;
#72723 = CARTESIAN_POINT ( 'NONE',  ( 0.6824146981627303710, -0.6046776061558807314, 0.2411417322834647770 ) ) ;
#72724 = MECHANICAL_DESIGN_GEOMETRIC_PRESENTATION_REPRESENTATION (  '', ( #52567 ), #27049 ) ;
#72725 = ORIENTED_EDGE ( 'NONE', *, *, #40855, .T. ) ;
#72726 = CARTESIAN_POINT ( 'NONE',  ( -0.2925321140481932369, 0.2925321140481931259, -1.513779527559054872 ) ) ;
#72727 = FACE_OUTER_BOUND ( 'NONE', #16696, .T. ) ;
#72728 = CARTESIAN_POINT ( 'NONE',  ( -0.05249343832020938322, -0.5023911411419708095, -0.1820866141732282451 ) ) ;
#72729 = CARTESIAN_POINT ( 'NONE',  ( -1.358267716535432434, -0.5400638737290844871, 0.3530559997133364547 ) ) ;
#72730 = CARTESIAN_POINT ( 'NONE',  ( 1.607611548556431069, -0.6692913385826773087, -0.1292274648535924053 ) ) ;
#72731 = CARTESIAN_POINT ( 'NONE',  ( 1.272965879265092637, -0.4281496062992127816, -0.4176697321401328100 ) ) ;
#72732 = CARTESIAN_POINT ( 'NONE',  ( -0.7217847769028863381, -0.004921259842519870586, -0.3153832671262229437 ) ) ;
#72733 = CARTESIAN_POINT ( 'NONE',  ( 0.2925321140481931814, -0.2925321140481931259, -0.01771653543307089365 ) ) ;
#72734 = CARTESIAN_POINT ( 'NONE',  ( 0.7349081364829402885, -0.6046776061558809534, -0.2411417322834644161 ) ) ;
#72735 = CARTESIAN_POINT ( 'NONE',  ( 0.3460692066303959202, 0.1998031496062993295, -0.1312335958005249603 ) ) ;
#72736 = CARTESIAN_POINT ( 'NONE',  ( -9.594673741351313045E-17, 0.3917322834645670659, -2.358943200296274689 ) ) ;
#72737 = CARTESIAN_POINT ( 'NONE',  ( -3.869764100875850765, 2.739927440807262471, -0.5314960629921260393 ) ) ;
#72738 = CARTESIAN_POINT ( 'NONE',  ( 1.496062992125984703, -0.1870078740157480601, -0.3641732283464567677 ) ) ;
#72739 = CARTESIAN_POINT ( 'NONE',  ( -1.141732283464566011, -0.6692913385826771977, 8.415575281601705876E-17 ) ) ;
#72740 = CARTESIAN_POINT ( 'NONE',  ( 1.332020997375328974, -0.05778040916215560624, -0.4822834645669293319 ) ) ;
#72741 = CARTESIAN_POINT ( 'NONE',  ( 0.1049643490035304938, -0.3917322834645669549, -2.532152230971127960 ) ) ;
#72742 = CARTESIAN_POINT ( 'NONE',  ( 1.410761154855643795, -0.08942795157528024563, -0.3641732283464568787 ) ) ;
#72743 = CARTESIAN_POINT ( 'NONE',  ( 0.006561679790026889343, -0.3162353388693409650, -0.4822834645669289433 ) ) ;
#72744 = CARTESIAN_POINT ( 'NONE',  ( -0.3805774278215216522, 0.05413385826771666132, 0.4176697321401328100 ) ) ;
#72745 = CARTESIAN_POINT ( 'NONE',  ( 1.666666666666667185, 0.05413385826771666132, 0.4176697321401328100 ) ) ;
#72746 = CARTESIAN_POINT ( 'NONE',  ( 3.846978723397335376, 2.751923335154144556, 0.5314960629921260393 ) ) ;
#72747 = CARTESIAN_POINT ( 'NONE',  ( 0.4527559055118117182, -0.4536011799217367080, 0.2665933059059888421 ) ) ;
#72748 = ORIENTED_EDGE ( 'NONE', *, *, #82059, .F. ) ;
#72749 = CARTESIAN_POINT ( 'NONE',  ( 0.3392501089628018329, 0.1958661417322835607, -0.4429327016086107571 ) ) ;
#72750 = ORIENTED_EDGE ( 'NONE', *, *, #9628, .F. ) ;
#72751 = CARTESIAN_POINT ( 'NONE',  ( -0.2887139107611542133, 0.2306618581243848609, 0.2411417322834645549 ) ) ;
#72752 = CARTESIAN_POINT ( 'NONE',  ( 1.397637795275591177, -0.5400638737290844871, 0.3530559997133364547 ) ) ;
#72753 = CARTESIAN_POINT ( 'NONE',  ( 0.2690288713910767848, 0.2952755905511811885, 0.1292274648535926551 ) ) ;
#72754 = CARTESIAN_POINT ( 'NONE',  ( -0.2165354330708654795, 0.07958543189024085140, 0.2665933059059887866 ) ) ;
#72755 = CARTESIAN_POINT ( 'NONE',  ( 1.364829396325460076, 0.2306618581243848609, 0.2411417322834645549 ) ) ;
#72756 = CARTESIAN_POINT ( 'NONE',  ( -1.115485564304461219, 0.05413385826771626580, -0.4176697321401330321 ) ) ;
#72757 = CARTESIAN_POINT ( 'NONE',  ( -0.03937007874015669567, -0.6692913385826771977, 8.415575281601705876E-17 ) ) ;
#72758 = CARTESIAN_POINT ( 'NONE',  ( -0.9842519685039365918, -0.6692913385826771977, 8.415575281601705876E-17 ) ) ;
#72759 = CARTESIAN_POINT ( 'NONE',  ( 0.9711286089238851948, 0.2306618581243848609, 0.2411417322834645549 ) ) ;
#72760 = CARTESIAN_POINT ( 'NONE',  ( 1.049868766404200127, -0.6046776061558809534, -0.2411417322834644161 ) ) ;
#72761 = CARTESIAN_POINT ( 'NONE',  ( 1.062992125984252745, 0.2952755905511811885, 0.000000000000000000 ) ) ;
#72762 = CARTESIAN_POINT ( 'NONE',  ( 0.3917322834645669549, 0.1049643490035304660, -0.7467191601049868455 ) ) ;
#72763 = CARTESIAN_POINT ( 'NONE',  ( -0.06561679790026180015, -0.004921259842519576551, 0.3153832671262227771 ) ) ;
#72764 = EDGE_LOOP ( 'NONE', ( #6389, #53196, #8058, #1572 ) ) ;
#72765 = CARTESIAN_POINT ( 'NONE',  ( 0.2891555358219910499, 0.2891555358219910499, -1.082677165354330784 ) ) ;
#72766 = ORIENTED_EDGE ( 'NONE', *, *, #80939, .T. ) ;
#72767 = CARTESIAN_POINT ( 'NONE',  ( -0.7217847769028863381, -0.004921259842519870586, -0.3153832671262229437 ) ) ;
#72768 = CARTESIAN_POINT ( 'NONE',  ( -0.1181102362204717315, -0.6692913385826771977, 8.415575281601705876E-17 ) ) ;
#72769 = CARTESIAN_POINT ( 'NONE',  ( 2.554262525012303442, 1.528780496884629025, 0.4744094488188976277 ) ) ;
#72770 = CARTESIAN_POINT ( 'NONE',  ( -0.3608923884514428360, -0.6692913385826773087, -0.1292274648535924053 ) ) ;
#72771 = CARTESIAN_POINT ( 'NONE',  ( -0.2230971128608915943, -0.4281496062992127816, -0.4176697321401328100 ) ) ;
#72772 = CARTESIAN_POINT ( 'NONE',  ( -0.8792650918635160906, -0.4281496062992124485, 0.4176697321401328655 ) ) ;
#72773 = CARTESIAN_POINT ( 'NONE',  ( -1.607611548556429737, -0.6692913385826771977, 0.1292274648535927661 ) ) ;
#72774 = CARTESIAN_POINT ( 'NONE',  ( 1.437007874015748810, -0.4536011799217368745, -0.2665933059059886201 ) ) ;
#72775 = CARTESIAN_POINT ( 'NONE',  ( -1.614173228346455824, 0.2952755905511811885, 0.000000000000000000 ) ) ;
#72776 = CARTESIAN_POINT ( 'NONE',  ( 0.2710308418177483358, 0.1175056764482960842, 5.568898341878665725 ) ) ;
#72777 = CARTESIAN_POINT ( 'NONE',  ( 0.4461942257217855201, -0.5023911411419708095, 0.1820866141732285504 ) ) ;
#72778 = CARTESIAN_POINT ( 'NONE',  ( 0.1049868766404206816, 0.2306618581243848609, 0.2411417322834645549 ) ) ;
#72779 = CARTESIAN_POINT ( 'NONE',  ( 0.2493438320209980519, 0.05413385826771666132, 0.4176697321401328100 ) ) ;
#72780 = ORIENTED_EDGE ( 'NONE', *, *, #53024, .T. ) ;
#72781 = CARTESIAN_POINT ( 'NONE',  ( 0.3460692066303959202, 0.1998031496062993295, -1.548556430446194287 ) ) ;
#72782 = CARTESIAN_POINT ( 'NONE',  ( -0.6167979002624665030, 0.009842519685039463617, 0.3409548833797002576 ) ) ;
#72783 = CARTESIAN_POINT ( 'NONE',  ( 0.3996062992125984925, 0.1070741851644054637, -0.9888451443569553634 ) ) ;
#72784 = CARTESIAN_POINT ( 'NONE',  ( 0.3996062992125984925, 0.1070741851644054637, -0.5164041994750655507 ) ) ;
#72785 = CARTESIAN_POINT ( 'NONE',  ( -0.7349081364829390672, 0.2306618581243847221, -0.2411417322834647770 ) ) ;
#72786 = CARTESIAN_POINT ( 'NONE',  ( 0.4091458600556403535, 0.2362204724409449896, -0.1312335958005249326 ) ) ;
#72787 = CARTESIAN_POINT ( 'NONE',  ( -0.1958661417322836718, 0.3392501089628017219, -2.302493438320210029 ) ) ;
#72788 = CARTESIAN_POINT ( 'NONE',  ( -1.423884514435694859, -0.08942795157528024563, -0.3641732283464568787 ) ) ;
#72789 = CARTESIAN_POINT ( 'NONE',  ( 0.8989501312335963501, -0.6692913385826773087, -0.1292274648535924053 ) ) ;
#72790 = CARTESIAN_POINT ( 'NONE',  ( 0.9580052493438327987, -0.4281496062992127816, -0.4176697321401328100 ) ) ;
#72791 = CARTESIAN_POINT ( 'NONE',  ( -0.02624671916010428221, 0.1283753931104746893, -0.1820866141732285504 ) ) ;
#72792 = CARTESIAN_POINT ( 'NONE',  ( 0.1312335958005255154, -0.6046776061558807314, 0.2411417322834647770 ) ) ;
#72793 = CARTESIAN_POINT ( 'NONE',  ( 0.1265901696524990294, -0.4724409448818896462, -1.894356955380577023 ) ) ;
#72794 = CARTESIAN_POINT ( 'NONE',  ( 0.09842519685039434474, 0.07958543189024085140, 0.2665933059059887866 ) ) ;
#72795 = CARTESIAN_POINT ( 'NONE',  ( 0.006561679790026889343, -0.05778040916215522460, 0.4822834645669289988 ) ) ;
#72796 = CARTESIAN_POINT ( 'NONE',  ( -0.3949938075777409963, -7.255918531996591613E-17, -1.690944881889764329 ) ) ;
#72797 = EDGE_CURVE ( 'NONE', #3191, #45375, #82879, .T. ) ;
#72798 = CARTESIAN_POINT ( 'NONE',  ( 1.561679790026247350, -0.3690944881889763329, 0.3153832671262228327 ) ) ;
#72799 = CARTESIAN_POINT ( 'NONE',  ( 0.1246719160104994284, -0.5511811023622046335, 0.09757992244046803654 ) ) ;
#72800 = CARTESIAN_POINT ( 'NONE',  ( 1.437007874015748810, -0.4536011799217368745, -0.2665933059059886201 ) ) ;
#72801 = CARTESIAN_POINT ( 'NONE',  ( -1.305774278215222184, -0.6692913385826773087, -0.1292274648535924053 ) ) ;
#72802 = CARTESIAN_POINT ( 'NONE',  ( -0.5839895013123351797, -0.5511811023622046335, 0.09757992244046803654 ) ) ;
#72803 = CARTESIAN_POINT ( 'NONE',  ( -1.034321223653607236, 5.987370802660155681E-15, -0.4118484887281962936 ) ) ;
#72804 = CARTESIAN_POINT ( 'NONE',  ( -0.8989501312335946848, 0.2952755905511810774, -0.1292274648535930714 ) ) ;
#72805 = CARTESIAN_POINT ( 'NONE',  ( -0.7349081364829387342, -0.6046776061558807314, 0.2411417322834647770 ) ) ;
#72806 = CARTESIAN_POINT ( 'NONE',  ( 0.1706036745406830368, -0.4281496062992127816, -0.4176697321401328100 ) ) ;
#72807 = CARTESIAN_POINT ( 'NONE',  ( 0.1998031496062994128, -0.3460692066303957537, -2.530839895013123453 ) ) ;
#72808 = CARTESIAN_POINT ( 'NONE',  ( -0.3392501089628019439, 0.1958661417322832554, -2.153523991304775009 ) ) ;
#72809 = LINE ( 'NONE', #47951, #26063 ) ;
#72810 = CARTESIAN_POINT ( 'NONE',  ( 0.8070866141732289112, -0.4536011799217368745, -0.2665933059059886201 ) ) ;
#72811 = CARTESIAN_POINT ( 'NONE',  ( 0.8333333333333340365, 0.2952755905511810774, -0.1292274648535930714 ) ) ;
#72812 = CARTESIAN_POINT ( 'NONE',  ( -1.299212598425196097, -0.5511811023622047445, 6.969142054262312111E-17 ) ) ;
#72813 = EDGE_CURVE ( 'NONE', #25966, #23493, #42106, .T. ) ;
#72814 = CARTESIAN_POINT ( 'NONE',  ( 0.9973753280839902091, -0.6046776061558807314, 0.2411417322834647770 ) ) ;
#72815 = CARTESIAN_POINT ( 'NONE',  ( -1.102362204724408601, -0.1870078740157479769, 0.3641732283464567677 ) ) ;
#72816 = CARTESIAN_POINT ( 'NONE',  ( -0.6561679790026240244, -0.6046776061558807314, 0.2411417322834647770 ) ) ;
#72817 = CARTESIAN_POINT ( 'NONE',  ( 0.07217847769028949700, -0.2845877964562159024, 0.3641732283464567677 ) ) ;
#72818 = CARTESIAN_POINT ( 'NONE',  ( -0.8768409086929770391, 5.410171027439680070E-15, -0.4118484887281949058 ) ) ;
#72819 = CARTESIAN_POINT ( 'NONE',  ( 0.8202099737532813073, 0.1771653543307087630, 0.09757992244046791164 ) ) ;
#72820 = EDGE_CURVE ( 'NONE', #36098, #7338, #29886, .T. ) ;
#72821 = CARTESIAN_POINT ( 'NONE',  ( 0.1640419947506569498, -0.3162353388693409650, -0.4822834645669289433 ) ) ;
#72822 = CARTESIAN_POINT ( 'NONE',  ( -0.1070741851644051862, -0.3996062992125986590, -0.1489501312335958227 ) ) ;
#72823 = CARTESIAN_POINT ( 'NONE',  ( -0.8202099737532801971, -0.6692913385826771977, 0.1292274648535927661 ) ) ;
#72824 = CARTESIAN_POINT ( 'NONE',  ( 0.3917322834645669549, 0.1049643490035304660, -1.311679790026246906 ) ) ;
#72825 = CARTESIAN_POINT ( 'NONE',  ( 1.069553805774278610, -0.5511811023622046335, 0.09757992244046803654 ) ) ;
#72826 = CARTESIAN_POINT ( 'NONE',  ( 0.5774278215223104249, 0.2306618581243848609, 0.2411417322834645549 ) ) ;
#72827 = CARTESIAN_POINT ( 'NONE',  ( -0.4199475065616791736, -0.6046776061558807314, 0.2411417322834647770 ) ) ;
#72828 = CARTESIAN_POINT ( 'NONE',  ( -0.4265091863517051496, -0.5511811023622046335, 0.09757992244046803654 ) ) ;
#72829 = DIRECTION ( 'NONE',  ( 0.000000000000000000, 0.000000000000000000, -1.000000000000000000 ) ) ;
#72830 = CARTESIAN_POINT ( 'NONE',  ( 0.1443569553805781891, -0.004921259842519870586, -0.3153832671262229437 ) ) ;
#72831 = CARTESIAN_POINT ( 'NONE',  ( 0.2427821522309719648, -0.05778040916215522460, 0.4822834645669289988 ) ) ;
#72832 = CARTESIAN_POINT ( 'NONE',  ( -0.9251968503937002541, 0.07958543189024085140, 0.2665933059059887866 ) ) ;
#72833 = CARTESIAN_POINT ( 'NONE',  ( 0.3996062992125986035, -0.1070741851644052972, -1.133202099737532720 ) ) ;
#72834 = CARTESIAN_POINT ( 'NONE',  ( -0.9580052493438311334, 0.05413385826771626580, -0.4176697321401330321 ) ) ;
#72835 = CARTESIAN_POINT ( 'NONE',  ( 0.8558026128237107288, -1.283732188437465593E-15, -0.4281993546915538462 ) ) ;
#72836 = ORIENTED_EDGE ( 'NONE', *, *, #77992, .T. ) ;
#72837 = CARTESIAN_POINT ( 'NONE',  ( -0.9514435695538050464, -0.2845877964562159024, 0.3641732283464567677 ) ) ;
#72838 = CARTESIAN_POINT ( 'NONE',  ( -0.02624671916010428221, -0.6046776061558807314, 0.2411417322834647770 ) ) ;
#72839 = ADVANCED_FACE ( 'NONE', ( #42515 ), #2993, .T. ) ;
#72840 = CARTESIAN_POINT ( 'NONE',  ( 0.3979867861068622781, 0.002674255378527819714, -1.220472440944881942 ) ) ;
#72841 = CARTESIAN_POINT ( 'NONE',  ( -0.7414698162729651543, -0.6692913385826771977, 0.1292274648535927661 ) ) ;
#72842 = CARTESIAN_POINT ( 'NONE',  ( -2.795275590551181910, 1.850393700787402729, -6.635626899597537341E-17 ) ) ;
#72844 = CARTESIAN_POINT ( 'NONE',  ( 1.102362204724410155, -0.1870078740157479769, 0.4822834645669291653 ) ) ;
#72843 = CARTESIAN_POINT ( 'NONE',  ( 1.033630966599880630, -4.927456884911482678E-16, 0.4445507791589062840 ) ) ;
#72845 = CARTESIAN_POINT ( 'NONE',  ( 0.6889763779527566800, -0.5400638737290844871, 0.3530559997133364547 ) ) ;
#72846 = DIRECTION ( 'NONE',  ( 0.000000000000000000, 0.000000000000000000, 1.000000000000000000 ) ) ;
#72847 = CARTESIAN_POINT ( 'NONE',  ( 1.463254593175853824, 0.2952755905511810774, -0.1292274648535930714 ) ) ;
#72848 = CARTESIAN_POINT ( 'NONE',  ( -1.509186351706035767, 0.05413385826771626580, -0.4176697321401330321 ) ) ;
#72849 = CARTESIAN_POINT ( 'NONE',  ( 0.3996062992125986035, 0.1070741851644054776, -0.5971128608923884640 ) ) ;
#72851 = ADVANCED_FACE ( 'NONE', ( #54318 ), #17292, .F. ) ;
#72850 = ORIENTED_EDGE ( 'NONE', *, *, #50355, .F. ) ;
#72852 = CARTESIAN_POINT ( 'NONE',  ( -0.5643044619422565855, -0.3690944881889763329, 0.3153832671262228327 ) ) ;
#72853 = CARTESIAN_POINT ( 'NONE',  ( -0.1049643490035307020, 0.3917322834645669549, -2.203412073490814027 ) ) ;
#72854 = ORIENTED_EDGE ( 'NONE', *, *, #21327, .F. ) ;
#72855 = CARTESIAN_POINT ( 'NONE',  ( 0.6496062992125991586, 0.1660481256975885056, 0.3530559997133364547 ) ) ;
#72856 = CARTESIAN_POINT ( 'NONE',  ( -0.02624671916010428221, -0.6046776061558807314, 0.2411417322834647770 ) ) ;
#72857 = CARTESIAN_POINT ( 'NONE',  ( -0.8595800524934373854, -0.05778040916215522460, 0.4822834645669289988 ) ) ;
#72858 = CARTESIAN_POINT ( 'NONE',  ( 1.666666666666667185, 0.05413385826771666132, 0.4176697321401328100 ) ) ;
#72859 = CARTESIAN_POINT ( 'NONE',  ( -1.082677165354329896, -0.4536011799217368745, -0.2665933059059886201 ) ) ;
#72860 = CARTESIAN_POINT ( 'NONE',  ( 0.2362204724409451007, -0.4091458600556402980, -2.058398950131233640 ) ) ;
#72861 = CARTESIAN_POINT ( 'NONE',  ( 0.5511811023622055217, -0.1870078740157479769, 0.4822834645669291653 ) ) ;
#72862 = CARTESIAN_POINT ( 'NONE',  ( 0.5118110236220478892, 0.1771653543307087630, 0.000000000000000000 ) ) ;
#72863 = CARTESIAN_POINT ( 'NONE',  ( -1.010498687664041384, 0.05413385826771666132, 0.4176697321401328100 ) ) ;
#72864 = CARTESIAN_POINT ( 'NONE',  ( 0.3917322834645669549, 2.398668435337827645E-17, -1.772946563483252858 ) ) ;
#72865 = CARTESIAN_POINT ( 'NONE',  ( -1.391076115485563314, -0.6046776061558809534, -0.2411417322834644161 ) ) ;
#72866 = CARTESIAN_POINT ( 'NONE',  ( -1.587926509186350810, -0.3690944881889763329, 0.3153832671262228327 ) ) ;
#72867 = EDGE_CURVE ( 'NONE', #15345, #60855, #74532, .T. ) ;
#72868 = CARTESIAN_POINT ( 'NONE',  ( 1.207349081364829990, 0.2306618581243848609, 0.2411417322834645549 ) ) ;
#72869 = CARTESIAN_POINT ( 'NONE',  ( 1.469816272965879911, -0.5023911411419708095, 0.1820866141732285504 ) ) ;
#72870 = VERTEX_POINT ( 'NONE', #3819 ) ;
#72871 = CARTESIAN_POINT ( 'NONE',  ( 0.2891555358219910499, -0.2891555358219909944, 0.05905511811023616414 ) ) ;
#72872 = CARTESIAN_POINT ( 'NONE',  ( -0.4790026246719152336, -0.05778040916215560624, -0.4822834645669293319 ) ) ;
#72873 = VERTEX_POINT ( 'NONE', #10955 ) ;
#72874 = CARTESIAN_POINT ( 'NONE',  ( 0.5643044619422579178, -0.3690944881889765550, -0.3153832671262227771 ) ) ;
#72875 = CARTESIAN_POINT ( 'NONE',  ( -1.233595800524933894, 0.2306618581243848609, 0.2411417322834645549 ) ) ;
#72876 = CARTESIAN_POINT ( 'NONE',  ( 0.8661417322834652488, -0.1870078740157480879, -0.4822834645669291653 ) ) ;
#72877 = CARTESIAN_POINT ( 'NONE',  ( 0.8202099737532813073, 0.2952755905511811885, 0.1292274648535926551 ) ) ;
#72878 = CARTESIAN_POINT ( 'NONE',  ( 0.3674540682414705883, 0.2306618581243847221, -0.2411417322834647770 ) ) ;
#72879 = CARTESIAN_POINT ( 'NONE',  ( -0.5643044619422565855, -0.4281496062992124485, 0.4176697321401328655 ) ) ;
#72880 = CARTESIAN_POINT ( 'NONE',  ( 0.1958661417322834775, 0.3392501089628018884, -1.646325459317585338 ) ) ;
#72881 = CARTESIAN_POINT ( 'NONE',  ( -1.706036745406823485, 0.2306618581243848609, 0.2411417322834645549 ) ) ;
#72882 = CARTESIAN_POINT ( 'NONE',  ( -0.7939632545931750718, -0.05778040916215560624, -0.4822834645669293319 ) ) ;
#72883 = CARTESIAN_POINT ( 'NONE',  ( -0.4068241469816264999, -0.3690944881889763329, 0.3153832671262228327 ) ) ;
#72884 = CARTESIAN_POINT ( 'NONE',  ( 1.305774278215223960, -0.6692913385826771977, 0.1292274648535927661 ) ) ;
#72885 = CARTESIAN_POINT ( 'NONE',  ( 1.502624671916010790, -0.05778040916215522460, 0.4822834645669289988 ) ) ;
#72886 = CARTESIAN_POINT ( 'NONE',  ( -0.3083989501312330295, -0.05778040916215522460, 0.4822834645669289988 ) ) ;
#72887 = DIRECTION ( 'NONE',  ( 1.000000000000000000, 0.000000000000000000, 0.000000000000000000 ) ) ;
#72888 = CARTESIAN_POINT ( 'NONE',  ( 0.7939632545931766261, -0.05778040916215522460, 0.4822834645669289988 ) ) ;
#72889 = CARTESIAN_POINT ( 'NONE',  ( 0.3996062992125986590, -0.1070741851644053111, -1.843832020997375309 ) ) ;
#72890 = CARTESIAN_POINT ( 'NONE',  ( -1.436417322834643739, 2.401574803149606474, -0.3149606299212598381 ) ) ;
#72891 = CARTESIAN_POINT ( 'NONE',  ( -0.1706036745406816491, 0.05413385826771626580, -0.4176697321401330321 ) ) ;
#72893 = CARTESIAN_POINT ( 'NONE',  ( 0.4848630542936502308, 1.968099216065431811, -0.4919401540133077622 ) ) ;
#72892 = CARTESIAN_POINT ( 'NONE',  ( 1.023622047244095334, -0.1870078740157479769, 0.3641732283464567677 ) ) ;
#72894 = CARTESIAN_POINT ( 'NONE',  ( 0.4724409448818897572, -0.1265901696524988906, -0.8182414698162727706 ) ) ;
#72895 = CARTESIAN_POINT ( 'NONE',  ( 1.391076115485564868, 0.1283753931104746893, -0.1820866141732285504 ) ) ;
#72896 = CARTESIAN_POINT ( 'NONE',  ( 1.286089238845145033, 0.2306618581243848609, 0.2411417322834645549 ) ) ;
#72897 = CARTESIAN_POINT ( 'NONE',  ( -0.3420746716998662729, 0.1974969037888702206, 0.05446194225721785048 ) ) ;
#72898 = CARTESIAN_POINT ( 'NONE',  ( -0.4265091863517051496, 0.2952755905511810774, -0.1292274648535930714 ) ) ;
#72899 = CARTESIAN_POINT ( 'NONE',  ( 2.543486866223389153, 2.716535433070866645, 0.5314960629921260393 ) ) ;
#72900 = CARTESIAN_POINT ( 'NONE',  ( 1.253280839895013710, -0.2845877964562159024, 0.3641732283464567677 ) ) ;
#72901 = CARTESIAN_POINT ( 'NONE',  ( -0.03937007874015669567, -0.6692913385826771977, 8.415575281601705876E-17 ) ) ;
#72902 = CARTESIAN_POINT ( 'NONE',  ( 0.2891555358219910499, 0.2891555358219910499, -0.3720472440944882497 ) ) ;
#72903 = CARTESIAN_POINT ( 'NONE',  ( 1.200787401574803681, 0.1660481256975885056, 0.3530559997133364547 ) ) ;
#72904 = CARTESIAN_POINT ( 'NONE',  ( 0.7086614173228352742, -0.1870078740157480879, -0.4822834645669291653 ) ) ;
#72905 = CARTESIAN_POINT ( 'NONE',  ( 0.4658792650918641698, -0.08942795157528024563, -0.3641732283464568787 ) ) ;
#72906 = CARTESIAN_POINT ( 'NONE',  ( 0.000000000000000000, 2.185039370078740273, 0.000000000000000000 ) ) ;
#72907 = CARTESIAN_POINT ( 'NONE',  ( 0.3346456692913393205, -0.4536011799217368745, -0.2665933059059886201 ) ) ;
#72908 = DIRECTION ( 'NONE',  ( -0.000000000000000000, -1.000000000000000000, -0.000000000000000000 ) ) ;
#72909 = CARTESIAN_POINT ( 'NONE',  ( -0.1070741851644056997, 0.3996062992125984925, -1.185695538057742526 ) ) ;
#72910 = CARTESIAN_POINT ( 'NONE',  ( 0.8727034120734913358, -0.05778040916215522460, 0.4822834645669289988 ) ) ;
#72911 = CARTESIAN_POINT ( 'NONE',  ( -0.3917322834645671215, 0.1049643490035301469, -1.284776902887139194 ) ) ;
#72912 = CARTESIAN_POINT ( 'NONE',  ( 0.9348729704079946634, -8.644661201599092366E-16, -0.4445507791589066171 ) ) ;
#72913 = CARTESIAN_POINT ( 'NONE',  ( -0.4012318369997560086, -0.2492710286714439338, -0.07052317558243419160 ) ) ;
#72914 = CARTESIAN_POINT ( 'NONE',  ( 5.463695987328526437E-16, -0.1870078740157479769, 0.3641732283464567677 ) ) ;
#72915 = EDGE_CURVE ( 'NONE', #43005, #32472, #18364, .T. ) ;
#72916 = CARTESIAN_POINT ( 'NONE',  ( -0.07874015748031421014, -0.1870078740157479769, 0.4822834645669291653 ) ) ;
#72917 = CARTESIAN_POINT ( 'NONE',  ( 1.574803149606299746, -0.1870078740157480601, -0.3641732283464567677 ) ) ;
#72918 = CARTESIAN_POINT ( 'NONE',  ( -1.404199475065615932, -0.004921259842519576551, 0.3153832671262227771 ) ) ;
#72919 = CARTESIAN_POINT ( 'NONE',  ( -1.049868766404198794, 0.2306618581243847221, -0.2411417322834647770 ) ) ;
#72920 = CARTESIAN_POINT ( 'NONE',  ( 0.7086614173228353852, -0.1870078740157479769, 0.4822834645669291653 ) ) ;
#72921 = CARTESIAN_POINT ( 'NONE',  ( 1.515748031496063408, 0.1660481256975885056, 0.3530559997133364547 ) ) ;
#72922 = CARTESIAN_POINT ( 'NONE',  ( 0.3049517105654749871, 8.471767977567108961E-16, -0.4445507791589058955 ) ) ;
#72923 = CARTESIAN_POINT ( 'NONE',  ( 0.6955380577427828781, 0.05413385826771626580, -0.4176697321401330321 ) ) ;
#72924 = CARTESIAN_POINT ( 'NONE',  ( -0.4724409448818898682, -8.678599364036362592E-17, -2.793307086614173151 ) ) ;
#72925 = CARTESIAN_POINT ( 'NONE',  ( 1.594488188976378673, -0.5400638737290845981, -0.3530559997133363437 ) ) ;
#72926 = CARTESIAN_POINT ( 'NONE',  ( 0.8530183727034128527, -0.4281496062992124485, 0.4176697321401328655 ) ) ;
#72927 = CLOSED_SHELL ( 'NONE', ( #11014, #1297, #55620, #27002, #62389, #71382, #14869, #36321, #6346, #59217, #44030, #80245, #40409, #10309, #12372, #7943 ) ) ;
#72928 = CARTESIAN_POINT ( 'NONE',  ( -1.443569553805773564, -0.5023911411419708095, 0.1820866141732285504 ) ) ;
#72929 = CARTESIAN_POINT ( 'NONE',  ( 1.397637795275591177, 0.07958543189024071263, -0.2665933059059888421 ) ) ;
#72930 = CARTESIAN_POINT ( 'NONE',  ( -1.384514435695537005, -0.5511811023622048555, -0.09757992244046775898 ) ) ;
#72931 = CARTESIAN_POINT ( 'NONE',  ( -0.8989501312335946848, -0.5511811023622046335, 0.09757992244046803654 ) ) ;
#72932 = CARTESIAN_POINT ( 'NONE',  ( 1.522309711286089939, -0.6046776061558809534, -0.2411417322834644161 ) ) ;
#72933 = CARTESIAN_POINT ( 'NONE',  ( 0.5446194225721792126, -0.08942795157528024563, -0.3641732283464568787 ) ) ;
#72934 = CARTESIAN_POINT ( 'NONE',  ( 0.2099737532808405305, -0.6046776061558807314, 0.2411417322834647770 ) ) ;
#72935 = CARTESIAN_POINT ( 'NONE',  ( 1.062992125984252745, -0.6692913385826771977, 8.415575281601705876E-17 ) ) ;
#72936 = CARTESIAN_POINT ( 'NONE',  ( 0.08530183727034192087, -0.05778040916215522460, 0.4822834645669289988 ) ) ;
#72937 = CARTESIAN_POINT ( 'NONE',  ( -0.05249343832020938322, -0.5023911411419708095, -0.1820866141732282451 ) ) ;
#72938 = CARTESIAN_POINT ( 'NONE',  ( 1.292650918635171564, 0.2952755905511811885, 0.1292274648535926551 ) ) ;
#72939 = CARTESIAN_POINT ( 'NONE',  ( -1.574803149606298192, -0.1870078740157480879, -0.4822834645669291653 ) ) ;
#72940 = CARTESIAN_POINT ( 'NONE',  ( -0.9973753280839886548, -0.6046776061558809534, -0.2411417322834644161 ) ) ;
#72941 = CARTESIAN_POINT ( 'NONE',  ( 0.1998031496062992740, 0.3460692066303959757, -0.6167979002624671692 ) ) ;
#72942 = CARTESIAN_POINT ( 'NONE',  ( -0.2749671762622359350, 1.142275244175160909, 0.1498262158730659654 ) ) ;
#72943 = CARTESIAN_POINT ( 'NONE',  ( -0.6627296587926501115, 0.2952755905511810774, -0.1292274648535930714 ) ) ;
#72944 = CARTESIAN_POINT ( 'NONE',  ( 0.01968503937007930540, 0.1660481256975885056, 0.3530559997133364547 ) ) ;
#72945 = CARTESIAN_POINT ( 'NONE',  ( -0.1265901696524993347, 0.4724409448818895907, -0.006561679790026246628 ) ) ;
#72946 = CARTESIAN_POINT ( 'NONE',  ( 0.1974969037888706369, -0.3420746716998659953, -2.139107611548556331 ) ) ;
#72947 = VERTEX_POINT ( 'NONE', #42920 ) ;
#72949 = CARTESIAN_POINT ( 'NONE',  ( -0.3917322834645670104, -7.196005306013484475E-17, -0.9763779527559053317 ) ) ;
#72948 = AXIS2_PLACEMENT_3D ( 'NONE', #34502, #41634, #15987 ) ;
#72950 = CARTESIAN_POINT ( 'NONE',  ( 0.9776902887139113929, 0.2952755905511811885, 0.1292274648535926551 ) ) ;
#72951 = CARTESIAN_POINT ( 'NONE',  ( 0.000000000000000000, 0.000000000000000000, -0.4921259842519685179 ) ) ;
#72952 = CARTESIAN_POINT ( 'NONE',  ( -1.161417322834644716, -0.4536011799217368745, -0.2665933059059886201 ) ) ;
#72953 = CARTESIAN_POINT ( 'NONE',  ( 0.1049643490035303689, 0.3917322834645670104, -1.087926509186351476 ) ) ;
#72954 = CARTESIAN_POINT ( 'NONE',  ( 1.568241469816273437, -0.2845877964562159024, 0.3641732283464567677 ) ) ;
#72955 = CARTESIAN_POINT ( 'NONE',  ( 4.797336870675655290E-17, -0.3917322834645669549, -0.1587733351367961454 ) ) ;
#72956 = CARTESIAN_POINT ( 'NONE',  ( -0.02624671916010428221, 0.2306618581243847221, -0.2411417322834647770 ) ) ;
#72957 = CARTESIAN_POINT ( 'NONE',  ( -0.5971128608923877978, 0.1771653543307087630, 0.09757992244046791164 ) ) ;
#72958 = CARTESIAN_POINT ( 'NONE',  ( 0.6758530183727039509, 0.2952755905511810774, -0.1292274648535930714 ) ) ;
#72959 = CARTESIAN_POINT ( 'NONE',  ( 0.4068241469816279987, -0.4281496062992127816, -0.4176697321401328100 ) ) ;
#72960 = CARTESIAN_POINT ( 'NONE',  ( -0.4562720003150207426, 1.668198494846153457, -2.130121299646748234 ) ) ;
#72961 = CARTESIAN_POINT ( 'NONE',  ( 0.4724409448818898682, 2.892866454678787531E-17, -1.062992125984252079 ) ) ;
#72962 = CARTESIAN_POINT ( 'NONE',  ( -0.1958661417322833942, -0.3392501089628018884, -1.479678108432757933 ) ) ;
#72963 = CARTESIAN_POINT ( 'NONE',  ( 1.148293963254593875, -0.6692913385826771977, 0.1292274648535927661 ) ) ;
#72964 = CARTESIAN_POINT ( 'NONE',  ( 0.1968503937007881344, 0.2952755905511811885, 0.000000000000000000 ) ) ;
#72965 = CARTESIAN_POINT ( 'NONE',  ( -0.9251968503937002541, -0.5400638737290845981, -0.3530559997133363437 ) ) ;
#72966 = CARTESIAN_POINT ( 'NONE',  ( -1.581364829396324945, -0.05778040916215560624, -0.4822834645669293319 ) ) ;
#72967 = CARTESIAN_POINT ( 'NONE',  ( 0.9383202099737538715, -0.05778040916215560624, -0.4822834645669293319 ) ) ;
#72968 = CARTESIAN_POINT ( 'NONE',  ( 0.3392501089628018329, 0.1958661417322835607, -0.3733595800524935338 ) ) ;
#72969 = CARTESIAN_POINT ( 'NONE',  ( -0.4396325459317579898, 0.2952755905511811885, 0.1292274648535926551 ) ) ;
#72970 = CARTESIAN_POINT ( 'NONE',  ( 0.4855643044619430415, -0.4281496062992127816, -0.4176697321401328100 ) ) ;
#72971 = CARTESIAN_POINT ( 'NONE',  ( -0.03937007874015669567, 0.2952755905511811885, 0.000000000000000000 ) ) ;
#72972 = CARTESIAN_POINT ( 'NONE',  ( 0.8398950131233602345, -0.5023911411419708095, 0.1820866141732285504 ) ) ;
#72973 = CARTESIAN_POINT ( 'NONE',  ( -1.528871391076114250, 0.2952755905511810774, -0.1292274648535930714 ) ) ;
#72974 = CARTESIAN_POINT ( 'NONE',  ( -1.535433070866141225, 0.2952755905511811885, 0.000000000000000000 ) ) ;
#72975 = CARTESIAN_POINT ( 'NONE',  ( 0.6955380577427828781, 0.05413385826771626580, -0.4176697321401330321 ) ) ;
#72976 = CARTESIAN_POINT ( 'NONE',  ( -0.1265901696524993347, 0.4724409448818896462, -0.5557742782152230721 ) ) ;
#72977 = CARTESIAN_POINT ( 'NONE',  ( -0.1958661417322836718, 0.3392501089628017219, -2.209973753280840114 ) ) ;
#72978 = VERTEX_POINT ( 'NONE', #36612 ) ;
#72979 = CARTESIAN_POINT ( 'NONE',  ( 0.1998031496062994405, -0.3460692066303958092, -0.5643044619422572516 ) ) ;
#72980 = VERTEX_POINT ( 'NONE', #23162 ) ;
#72981 = CARTESIAN_POINT ( 'NONE',  ( 1.220472440944882608, 0.2952755905511811885, 0.000000000000000000 ) ) ;
#72982 = CARTESIAN_POINT ( 'NONE',  ( 0.7414698162729663755, -0.5511811023622048555, -0.09757992244046775898 ) ) ;
#72983 = CARTESIAN_POINT ( 'NONE',  ( 2.400767430980333376E-17, -0.2726377952755905665, 0.07874015748031495954 ) ) ;
#72984 = CARTESIAN_POINT ( 'NONE',  ( 3.900966923095589678, 2.755905511811024056, -0.5314960629921260393 ) ) ;
#72985 =( NAMED_UNIT ( * ) PLANE_ANGLE_UNIT ( ) SI_UNIT ( $, .RADIAN. ) );
#72986 = CARTESIAN_POINT ( 'NONE',  ( -0.3392501089628019995, 0.1958661417322832277, -1.213254593175852936 ) ) ;
#72987 = CARTESIAN_POINT ( 'NONE',  ( -0.1998031496062991630, -0.3460692066303959202, -2.032152230971128848 ) ) ;
#72988 = CARTESIAN_POINT ( 'NONE',  ( -1.620734908136482577, 0.2952755905511811885, 0.1292274648535926551 ) ) ;
#72989 = TOROIDAL_SURFACE ( 'NONE', #25920, 1.178877988035069047, 0.01968503937007873988 ) ;
#72990 = CARTESIAN_POINT ( 'NONE',  ( -0.2493438320209966919, 0.05413385826771626580, -0.4176697321401330321 ) ) ;
#72991 = CARTESIAN_POINT ( 'NONE',  ( 1.305774278215223960, 0.2952755905511810774, -0.1292274648535930714 ) ) ;
#72992 = VERTEX_POINT ( 'NONE', #62291 ) ;
#72993 = CARTESIAN_POINT ( 'NONE',  ( -1.686351706036744558, 0.2952755905511810774, -0.1292274648535930714 ) ) ;
#72994 = CARTESIAN_POINT ( 'NONE',  ( 1.614173228346457378, -0.5511811023622047445, 6.969142054262312111E-17 ) ) ;
#72995 = APPLICATION_PROTOCOL_DEFINITION ( 'draft international standard', 'automotive_design', 1998, #45472 ) ;
#72996 = CARTESIAN_POINT ( 'NONE',  ( 1.574803149606299746, -0.1870078740157480601, -0.3641732283464567677 ) ) ;
#72997 = CARTESIAN_POINT ( 'NONE',  ( 0.3460692066303958092, 0.1998031496062993018, -1.940288713910761409 ) ) ;
#72998 = CARTESIAN_POINT ( 'NONE',  ( -1.391076115485563314, -0.5023911411419708095, -0.1820866141732282451 ) ) ;
#72999 = CARTESIAN_POINT ( 'NONE',  ( -0.3392501089628017219, -0.1958661417322836718, 0.1128608923884514836 ) ) ;
#73000 = CARTESIAN_POINT ( 'NONE',  ( 0.3740157480314966754, -0.5400638737290844871, 0.3530559997133364547 ) ) ;
#73001 = ORIENTED_EDGE ( 'NONE', *, *, #67409, .F. ) ;
#73003 = DIRECTION ( 'NONE',  ( 0.000000000000000000, 1.601283208593975810E-15, -1.000000000000000000 ) ) ;
#73002 = CARTESIAN_POINT ( 'NONE',  ( 1.561679790026247350, 0.05413385826771626580, -0.4176697321401330321 ) ) ;
#73004 = CARTESIAN_POINT ( 'NONE',  ( -0.9383202099737524282, -0.08942795157527998196, 0.3641732283464567121 ) ) ;
#73005 = CARTESIAN_POINT ( 'NONE',  ( 0.6824146981627303710, -0.6046776061558807314, 0.2411417322834647770 ) ) ;
#73006 = CARTESIAN_POINT ( 'NONE',  ( 1.430446194225722500, -0.004921259842519576551, 0.3153832671262227771 ) ) ;
#73007 = CARTESIAN_POINT ( 'NONE',  ( -0.1049643490035301746, -0.3917322834645670659, -1.097093545110549462 ) ) ;
#73008 = AXIS2_PLACEMENT_3D ( 'NONE', #53870, #47561, #21075 ) ;
#73009 = CARTESIAN_POINT ( 'NONE',  ( -0.8070866141732276899, -0.4536011799217367080, 0.2665933059059888421 ) ) ;
#73010 = CARTESIAN_POINT ( 'NONE',  ( -1.437007874015747477, 0.07958543189024071263, -0.2665933059059888421 ) ) ;
#73011 = CARTESIAN_POINT ( 'NONE',  ( -1.220472440944882386, 0.000000000000000000, -0.4445507791589061175 ) ) ;
#73012 = CARTESIAN_POINT ( 'NONE',  ( 0.4461942257217855201, -0.6046776061558807314, 0.2411417322834647770 ) ) ;
#73013 = CARTESIAN_POINT ( 'NONE',  ( -1.036745406824146176, -0.3690944881889763329, 0.3153832671262228327 ) ) ;
#73014 = CARTESIAN_POINT ( 'NONE',  ( -0.2952755905511804668, 0.07958543189024085140, 0.2665933059059887866 ) ) ;
#73015 = CARTESIAN_POINT ( 'NONE',  ( -0.3083989501312330295, -0.05778040916215522460, 0.4822834645669289988 ) ) ;
#73016 = CARTESIAN_POINT ( 'NONE',  ( -1.555118110236219930, -0.4536011799217368745, -0.2665933059059886201 ) ) ;
#73017 = CARTESIAN_POINT ( 'NONE',  ( -0.1049643490035302301, -0.3917322834645671770, -0.06891695357711476178 ) ) ;
#73018 = CARTESIAN_POINT ( 'NONE',  ( 0.8595800524934390507, -0.05778040916215560624, -0.4822834645669293319 ) ) ;
#73019 =( BOUNDED_CURVE ( )  B_SPLINE_CURVE ( 2, ( #70373, #12728, #64064, #30005, #32916, #57734, #6820, #19448, #26175, #45941, #32490, #72059, #522 ),
 .UNSPECIFIED., .F., .F. ) 
 B_SPLINE_CURVE_WITH_KNOTS ( ( 3, 2, 2, 2, 2, 2, 3 ),
 ( 0.6399423569342326257, 0.6401515151515151381, 0.6439393939393940336, 0.6477272727272727071, 0.6515151515151516026, 0.6553030303030302761, 0.6555121885203127885 ),
 .UNSPECIFIED. ) 
 CURVE ( )  GEOMETRIC_REPRESENTATION_ITEM ( )  RATIONAL_B_SPLINE_CURVE ( ( 0.9964447847208418585, 0.9981185001348090724, 1.000000000000000000, 0.9659258262890683122, 1.000000000000000000, 0.9659258262890683122, 1.000000000000000000, 0.9659258262890683122, 1.000000000000000000, 0.9659258262890683122, 1.000000000000000000, 0.9981185001348091834, 0.9964447847208420805 ) ) 
 REPRESENTATION_ITEM ( '' )  );
#73020 = CARTESIAN_POINT ( 'NONE',  ( 0.8764808517432199908, -2.398893483443748302E-16, 0.4281993546915529580 ) ) ;
#73021 = CARTESIAN_POINT ( 'NONE',  ( -0.4091458600556402980, -0.2362204724409451284, -1.546587926509186639 ) ) ;
#73022 = CARTESIAN_POINT ( 'NONE',  ( -0.7414698162729651543, 0.2952755905511810774, -0.1292274648535930714 ) ) ;
#73023 = CARTESIAN_POINT ( 'NONE',  ( -0.2099737532808391705, -0.5023911411419708095, -0.1820866141732282451 ) ) ;
#73024 = CARTESIAN_POINT ( 'NONE',  ( -1.332020997375327642, -0.05778040916215522460, 0.4822834645669289988 ) ) ;
#73025 = CARTESIAN_POINT ( 'NONE',  ( 0.3543307086614181922, -0.5511811023622047445, 6.969142054262312111E-17 ) ) ;
#73026 = CARTESIAN_POINT ( 'NONE',  ( -0.8070866141732276899, -0.4536011799217367080, 0.2665933059059888421 ) ) ;
#73027 = CARTESIAN_POINT ( 'NONE',  ( -1.076115485564303809, 0.2306618581243848609, 0.2411417322834645549 ) ) ;
#73028 = CARTESIAN_POINT ( 'NONE',  ( 1.581364829396326277, -0.08942795157527998196, 0.3641732283464567121 ) ) ;
#73029 = CARTESIAN_POINT ( 'NONE',  ( 1.272965879265092637, -0.4281496062992127816, -0.4176697321401328100 ) ) ;
#73030 = CARTESIAN_POINT ( 'NONE',  ( 1.089589480386154330, 0.004960608223779187052, -0.3437734562760187962 ) ) ;
#73031 = CARTESIAN_POINT ( 'NONE',  ( 0.9645669291338591078, -0.4536011799217368745, -0.2665933059059886201 ) ) ;
#73032 = CARTESIAN_POINT ( 'NONE',  ( 0.4658792650918641698, -0.05778040916215560624, -0.4822834645669293319 ) ) ;
#73033 = CARTESIAN_POINT ( 'NONE',  ( 0.2017716535433070613, -0.2017716535433070890, -0.3937007874015748254 ) ) ;
#73034 = CARTESIAN_POINT ( 'NONE',  ( 1.443569553805774897, 0.1283753931104748280, 0.1820866141732283561 ) ) ;
#73035 = VERTEX_POINT ( 'NONE', #41291 ) ;
#73036 = B_SPLINE_CURVE_WITH_KNOTS ( 'NONE', 3,
 ( #59387, #8473, #40456, #9304 ),
 .UNSPECIFIED., .F., .F.,
 ( 4, 4 ),
 ( 0.07436403195037320779, 0.07455104739251885992 ),
 .UNSPECIFIED. ) ;
#73037 = CARTESIAN_POINT ( 'NONE',  ( 0.1070741851644054776, -0.3996062992125984925, -2.839238845144356649 ) ) ;
#73038 = CARTESIAN_POINT ( 'NONE',  ( -1.141732283464566011, 0.1771653543307087630, 0.000000000000000000 ) ) ;
#73039 = CARTESIAN_POINT ( 'NONE',  ( -0.4002624671916004129, -0.3162353388693405765, 0.4822834645669290543 ) ) ;
#73040 = CARTESIAN_POINT ( 'NONE',  ( 0.4527559055118117182, -0.5400638737290844871, 0.3530559997133364547 ) ) ;
#73041 = CARTESIAN_POINT ( 'NONE',  ( -1.581364829396324945, -0.2845877964562159024, 0.3641732283464567677 ) ) ;
#73042 = CARTESIAN_POINT ( 'NONE',  ( -0.1998031496062991630, -0.3460692066303959202, -1.874671916010498762 ) ) ;
#73043 = CARTESIAN_POINT ( 'NONE',  ( -1.430446194225721390, -0.4281496062992124485, 0.4176697321401328655 ) ) ;
#73044 = CARTESIAN_POINT ( 'NONE',  ( 0.2755905511811031494, 0.2952755905511811885, 0.000000000000000000 ) ) ;
#73045 = CARTESIAN_POINT ( 'NONE',  ( -0.08530183727034056085, -0.3162353388693405765, 0.4822834645669290543 ) ) ;
#73046 = CARTESIAN_POINT ( 'NONE',  ( 1.351706036745407458, -0.4281496062992127816, -0.4176697321401328100 ) ) ;
#73047 = CARTESIAN_POINT ( 'NONE',  ( -0.1070741851644051862, -0.3996062992125986035, -0.9363517060367454459 ) ) ;
#73048 = CARTESIAN_POINT ( 'NONE',  ( 0.3460692066303959757, -0.1998031496062991907, -1.364829396325459188 ) ) ;
#73049 = CARTESIAN_POINT ( 'NONE',  ( 0.2891555358219910499, -0.2891555358219909944, -1.043307086614173373 ) ) ;
#73050 = CARTESIAN_POINT ( 'NONE',  ( -9.787531504996567848E-17, 0.3996062992125986035, -2.677165354330708347 ) ) ;
#73051 = CARTESIAN_POINT ( 'NONE',  ( -0.4359958488159811907, 1.724409448818897905, 2.630268417803910186 ) ) ;
#73052 = AXIS2_PLACEMENT_3D ( 'NONE', #72722, #15069, #40725 ) ;
#73053 = CARTESIAN_POINT ( 'NONE',  ( 0.1049643490035303689, 0.3917322834645670104, -0.3005249343832020470 ) ) ;
#73054 = CARTESIAN_POINT ( 'NONE',  ( -0.07874015748031421014, -0.1870078740157480601, -0.3641732283464567677 ) ) ;
#73055 = CARTESIAN_POINT ( 'NONE',  ( -0.4199475065616791736, 0.2306618581243847221, -0.2411417322834647770 ) ) ;
#73056 = CARTESIAN_POINT ( 'NONE',  ( 0.9776902887139113929, 0.2952755905511811885, 0.1292274648535926551 ) ) ;
#73057 = CARTESIAN_POINT ( 'NONE',  ( 0.1058382717557500852, -0.3949938075777408852, -1.736876640419947826 ) ) ;
#73058 = CARTESIAN_POINT ( 'NONE',  ( 0.03280839895013198948, -0.5511811023622048555, -0.09757992244046775898 ) ) ;
#73059 = CARTESIAN_POINT ( 'NONE',  ( -1.128608923884513837, 0.2306618581243847221, -0.2411417322834647770 ) ) ;
#73060 = CARTESIAN_POINT ( 'NONE',  ( 1.522309711286089939, -0.6046776061558809534, -0.2411417322834644161 ) ) ;
#73061 = CARTESIAN_POINT ( 'NONE',  ( 0.4091458600556403535, 0.2362204724409449896, -1.863517060367454015 ) ) ;
#73062 = CARTESIAN_POINT ( 'NONE',  ( 0.3814249188612239272, -0.08989863709124447377, -2.755905511811024500 ) ) ;
#73063 = ORIENTED_EDGE ( 'NONE', *, *, #11002, .T. ) ;
#73064 = VERTEX_POINT ( 'NONE', #66976 ) ;
#73065 = CARTESIAN_POINT ( 'NONE',  ( 1.108923884514436242, -0.05778040916215522460, 0.4822834645669289988 ) ) ;
#73066 = AXIS2_PLACEMENT_3D ( 'NONE', #62390, #28338, #47688 ) ;
#73067 = CARTESIAN_POINT ( 'NONE',  ( -1.548556430446193399, 0.2306618581243848609, 0.2411417322834645549 ) ) ;
#73069 = CARTESIAN_POINT ( 'NONE',  ( -1.161417322834644716, 0.1660481256975885056, 0.3530559997133364547 ) ) ;
#73068 = CARTESIAN_POINT ( 'NONE',  ( -1.259842519685038686, -0.1870078740157480601, -0.3641732283464567677 ) ) ;
#73070 = CARTESIAN_POINT ( 'NONE',  ( -0.1958661417322836440, 0.3392501089628016664, -2.612841576606612204 ) ) ;
#73071 = DIRECTION ( 'NONE',  ( -0.000000000000000000, -1.000000000000000000, -0.000000000000000000 ) ) ;
#73072 = CARTESIAN_POINT ( 'NONE',  ( 1.167979002624672580, -0.4281496062992124485, 0.4176697321401328655 ) ) ;
#73073 = CARTESIAN_POINT ( 'NONE',  ( -1.469816272965878357, -0.6046776061558809534, -0.2411417322834644161 ) ) ;
#73074 = CARTESIAN_POINT ( 'NONE',  ( -0.09842519685039295696, 0.1660481256975883668, -0.3530559997133364547 ) ) ;
#73075 = CARTESIAN_POINT ( 'NONE',  ( -0.006561679790025524116, -0.3162353388693405765, 0.4822834645669290543 ) ) ;
#73076 = CARTESIAN_POINT ( 'NONE',  ( -1.292650918635170010, 0.2952755905511810774, -0.1292274648535930714 ) ) ;
#73077 = CARTESIAN_POINT ( 'NONE',  ( -0.1049643490035301746, -0.3917322834645670659, -2.829377009677478405 ) ) ;
#73078 = CARTESIAN_POINT ( 'NONE',  ( 0.8202099737532813073, 0.2952755905511811885, 0.1292274648535926551 ) ) ;
#73079 = CARTESIAN_POINT ( 'NONE',  ( -0.3917322834645671215, 0.1049643490035301469, -1.914698162729658648 ) ) ;
#73080 = CARTESIAN_POINT ( 'NONE',  ( -1.194225721784776262, -0.3690944881889763329, 0.3153832671262228327 ) ) ;
#73081 = ORIENTED_EDGE ( 'NONE', *, *, #11466, .F. ) ;
#73082 = CARTESIAN_POINT ( 'NONE',  ( 0.1058382717557500713, -0.3949938075777409408, -2.290026246719159886 ) ) ;
#73083 = ORIENTED_EDGE ( 'NONE', *, *, #42797, .F. ) ;
#73084 = DIRECTION ( 'NONE',  ( 0.000000000000000000, 0.000000000000000000, -1.000000000000000000 ) ) ;
#73085 = CARTESIAN_POINT ( 'NONE',  ( -1.548556430446193399, 0.2306618581243848609, 0.2411417322834645549 ) ) ;
#73086 = CARTESIAN_POINT ( 'NONE',  ( 1.574803149606299746, -0.1870078740157479769, 0.4822834645669291653 ) ) ;
#73087 = CARTESIAN_POINT ( 'NONE',  ( 0.1998031496062994405, -0.3460692066303958092, -0.5643044619422572516 ) ) ;
#73088 = DIRECTION ( 'NONE',  ( 0.000000000000000000, -1.000000000000000000, -0.000000000000000000 ) ) ;
#73089 = LINE ( 'NONE', #40266, #4732 ) ;
#73090 = CARTESIAN_POINT ( 'NONE',  ( 0.5314960629921371416, 2.755905511811024056, -3.184294706754629001 ) ) ;
#73091 = FACE_OUTER_BOUND ( 'NONE', #77825, .T. ) ;
#73092 = CARTESIAN_POINT ( 'NONE',  ( 0.3917322834645670104, 2.398668435337828261E-17, 0.1122047244094487306 ) ) ;
#73093 = CARTESIAN_POINT ( 'NONE',  ( -0.3937007874015740483, -0.1870078740157479769, 0.3641732283464567677 ) ) ;
#73094 = CARTESIAN_POINT ( 'NONE',  ( -0.9251968503937002541, 0.07958543189024085140, 0.2665933059059887866 ) ) ;
#73095 = CARTESIAN_POINT ( 'NONE',  ( -1.095800524934382292, -0.3162353388693409650, -0.4822834645669289433 ) ) ;
#73096 = CARTESIAN_POINT ( 'NONE',  ( 0.7611548556430451917, -0.6046776061558807314, 0.2411417322834647770 ) ) ;
#73097 = CARTESIAN_POINT ( 'NONE',  ( -0.9055118110236215490, -0.6692913385826771977, 8.415575281601705876E-17 ) ) ;
#73098 = CARTESIAN_POINT ( 'NONE',  ( 0.5314960629921393620, 2.755905511811024056, -3.826707563893390951 ) ) ;
#73099 = ORIENTED_EDGE ( 'NONE', *, *, #41242, .F. ) ;
#73100 = CARTESIAN_POINT ( 'NONE',  ( -1.541994750656167090, -0.6692913385826773087, -0.1292274648535924053 ) ) ;
#73101 = CARTESIAN_POINT ( 'NONE',  ( -1.574803149606298636, -0.1870078740157479769, 0.3641732283464567677 ) ) ;
#73102 = SHAPE_REPRESENTATION_RELATIONSHIP ( 'NONE' , 'NONE' ,  #7298, #79514 ) ;
#73103 = CARTESIAN_POINT ( 'NONE',  ( -0.2362204724409451284, 0.4091458600556402425, -1.430446194225721834 ) ) ;
#73104 = CARTESIAN_POINT ( 'NONE',  ( 2.019766021329699512, 1.253539720428401560, -0.3811758253793051110 ) ) ;
#73105 = EDGE_CURVE ( 'NONE', #44550, #712, #75408, .T. ) ;
#73106 = CARTESIAN_POINT ( 'NONE',  ( 0.1958661417322834775, 0.3392501089628018884, -0.7664041994750655507 ) ) ;
#73107 = CARTESIAN_POINT ( 'NONE',  ( 0.2867679344610366554, -0.2867679344610365444, -2.387795275590551380 ) ) ;
#73108 = CARTESIAN_POINT ( 'NONE',  ( -0.3018372703412066094, -0.4281496062992127816, -0.4176697321401328100 ) ) ;
#73109 = CARTESIAN_POINT ( 'NONE',  ( 1.437007874015748810, -0.5400638737290845981, -0.3530559997133363437 ) ) ;
#73110 = CARTESIAN_POINT ( 'NONE',  ( 0.1070741851644054776, -0.3996062992125984925, -0.1620734908136483299 ) ) ;
#73112 = CARTESIAN_POINT ( 'NONE',  ( 2.170146923806595129, 1.537401574803149984, 0.4744094488188975722 ) ) ;
#73111 = FACE_OUTER_BOUND ( 'NONE', #66454, .T. ) ;
#73113 = CARTESIAN_POINT ( 'NONE',  ( -1.364829396325458521, 0.2306618581243847221, -0.2411417322834647770 ) ) ;
#73114 = CARTESIAN_POINT ( 'NONE',  ( -0.7414698162729651543, 0.2952755905511810774, -0.1292274648535930714 ) ) ;
#73115 = CARTESIAN_POINT ( 'NONE',  ( 0.2867679344610365999, 0.2867679344610365999, 0.09713217667422754942 ) ) ;
#73116 = CARTESIAN_POINT ( 'NONE',  ( 0.5839895013123367340, -0.5511811023622048555, -0.09757992244046775898 ) ) ;
#73117 = CARTESIAN_POINT ( 'NONE',  ( -0.3917322834645671215, 0.1049643490035301469, -0.1174540682414699083 ) ) ;
#73118 = CIRCLE ( 'NONE', #34181, 0.09842519685039351207 ) ;
#73119 = CARTESIAN_POINT ( 'NONE',  ( 0.4658792650918641698, -0.08942795157528024563, -0.3641732283464568787 ) ) ;
#73120 = CARTESIAN_POINT ( 'NONE',  ( 0.7742782152230978099, -0.3690944881889763329, 0.3153832671262228327 ) ) ;
#73121 = CARTESIAN_POINT ( 'NONE',  ( 1.089238845144357537, -0.4281496062992124485, 0.4176697321401328655 ) ) ;
#73122 = UNCERTAINTY_MEASURE_WITH_UNIT (LENGTH_MEASURE( 1.000000000000000082E-05 ), #36337, 'distance_accuracy_value', 'NONE');
#73123 = CARTESIAN_POINT ( 'NONE',  ( -0.2034120734908128059, 0.1771653543307087630, 0.09757992244046791164 ) ) ;
#73124 = CARTESIAN_POINT ( 'NONE',  ( -0.1049643490035302024, -0.3917322834645671215, -1.796587926509185973 ) ) ;
#73125 = CARTESIAN_POINT ( 'NONE',  ( -1.384514435695537005, -0.6692913385826773087, -0.1292274648535924053 ) ) ;
#73126 = CARTESIAN_POINT ( 'NONE',  ( -0.08530183727034056085, -0.08942795157528024563, -0.3641732283464568787 ) ) ;
#73127 = CARTESIAN_POINT ( 'NONE',  ( -1.194225721784776262, -0.3690944881889763329, 0.3153832671262228327 ) ) ;
#73128 = CARTESIAN_POINT ( 'NONE',  ( 0.3458507752293908943, -0.3458507752293908943, -0.3326771653543306728 ) ) ;
#73129 = CARTESIAN_POINT ( 'NONE',  ( -0.8005249343832011588, -0.004921259842519870586, -0.3153832671262229437 ) ) ;
#73130 = CARTESIAN_POINT ( 'NONE',  ( -0.1509186351706028884, -0.3162353388693409650, -0.4822834645669289433 ) ) ;
#73131 = DIRECTION ( 'NONE',  ( 1.000000000000000000, -0.000000000000000000, -0.000000000000000000 ) ) ;
#73132 = AXIS2_PLACEMENT_3D ( 'NONE', #63045, #81181, #35720 ) ;
#73133 = CARTESIAN_POINT ( 'NONE',  ( 0.3412073490813655186, 0.1283753931104748280, 0.1820866141732283561 ) ) ;
#73134 = CARTESIAN_POINT ( 'NONE',  ( -0.4396325459317579898, 0.1771653543307087630, 0.09757992244046791164 ) ) ;
#73135 = CARTESIAN_POINT ( 'NONE',  ( -0.5183727034120726440, 0.2952755905511811885, 0.1292274648535926551 ) ) ;
#73136 = CARTESIAN_POINT ( 'NONE',  ( -1.614173228346456268, -0.6692913385826771977, 8.415575281601705876E-17 ) ) ;
#73137 = CARTESIAN_POINT ( 'NONE',  ( -1.082677165354329896, -0.4536011799217368745, -0.2665933059059886201 ) ) ;
#73138 = DIRECTION ( 'NONE',  ( 0.000000000000000000, -1.000000000000000000, 0.000000000000000000 ) ) ;
#73139 = ADVANCED_FACE ( 'NONE', ( #18511 ), #65339, .F. ) ;
#73140 = CARTESIAN_POINT ( 'NONE',  ( 0.5971128608923891301, 0.2952755905511810774, -0.1292274648535930714 ) ) ;
#73141 = CARTESIAN_POINT ( 'NONE',  ( -0.1070741851644056997, 0.3996062992125984925, -1.658136482939632117 ) ) ;
#73142 = FACE_OUTER_BOUND ( 'NONE', #26961, .T. ) ;
#73143 = CARTESIAN_POINT ( 'NONE',  ( -0.2887139107611542133, 0.1283753931104748280, 0.1820866141732283561 ) ) ;
#73144 = CARTESIAN_POINT ( 'NONE',  ( -0.1377952755905504645, 0.1660481256975885056, 0.3530559997133364547 ) ) ;
#73145 = CARTESIAN_POINT ( 'NONE',  ( -1.646981627296586703, -0.05778040916215522460, 0.4822834645669289988 ) ) ;
#73146 = CARTESIAN_POINT ( 'NONE',  ( -1.574803149606298192, -0.1870078740157480601, -0.3641732283464567677 ) ) ;
#73147 = CARTESIAN_POINT ( 'NONE',  ( 1.227034120734908917, 0.2952755905511810774, -0.1292274648535930714 ) ) ;
#73148 = CARTESIAN_POINT ( 'NONE',  ( -0.8530183727034112984, -0.3690944881889765550, -0.3153832671262227771 ) ) ;
#73149 = CARTESIAN_POINT ( 'NONE',  ( -1.091663011964304042, -2.570477104772672414E-15, 0.4118477457933002461 ) ) ;
#73150 = CARTESIAN_POINT ( 'NONE',  ( 0.1070741851644054915, -0.3996062992125986035, -0.2427821522309711322 ) ) ;
#73151 = CARTESIAN_POINT ( 'NONE',  ( -0.1049643490035307158, 0.3917322834645670104, -2.365504880086300776 ) ) ;
#73152 = CARTESIAN_POINT ( 'NONE',  ( -1.614173228346457378, 0.2753471884572480932, 0.1372047244094471985 ) ) ;
#73153 = CARTESIAN_POINT ( 'NONE',  ( 1.161417322834646271, 0.07958543189024071263, -0.2665933059059888421 ) ) ;
#73154 = CARTESIAN_POINT ( 'NONE',  ( 0.7020997375328090762, -0.05778040916215560624, -0.4822834645669293319 ) ) ;
#73155 = CARTESIAN_POINT ( 'NONE',  ( -0.1049643490035307020, 0.3917322834645669549, -2.610892388451443225 ) ) ;
#73156 = CARTESIAN_POINT ( 'NONE',  ( 1.227034120734908917, 0.1771653543307087075, -0.09757992244046823083 ) ) ;
#73157 = EDGE_CURVE ( 'NONE', #55671, #3211, #47905, .T. ) ;
#73158 = CARTESIAN_POINT ( 'NONE',  ( 0.07217847769028949700, -0.3162353388693405765, 0.4822834645669290543 ) ) ;
#73159 = CARTESIAN_POINT ( 'NONE',  ( -0.6036745406824141069, -0.6046776061558809534, -0.2411417322834644161 ) ) ;
#73160 = CARTESIAN_POINT ( 'NONE',  ( 1.515748031496063408, 0.1660481256975885056, 0.3530559997133364547 ) ) ;
#73161 = CARTESIAN_POINT ( 'NONE',  ( -0.2362204724409447953, -0.4091458600556404646, -0.6955380577427822120 ) ) ;
#73162 = CARTESIAN_POINT ( 'NONE',  ( -0.5314960629921349211, 2.716535433070866645, 2.543486866223387377 ) ) ;
#73163 = CARTESIAN_POINT ( 'NONE',  ( 0.1771653543307093182, 0.07958543189024085140, 0.2665933059059887866 ) ) ;
#73164 = VERTEX_POINT ( 'NONE', #15067 ) ;
#73165 = CARTESIAN_POINT ( 'NONE',  ( 0.2867679344610366554, 0.2867679344610366554, -0.2920140664380071471 ) ) ;
#73166 = ORIENTED_EDGE ( 'NONE', *, *, #25084, .T. ) ;
#73167 = CARTESIAN_POINT ( 'NONE',  ( -0.6036745406824141069, 0.2306618581243848609, 0.2411417322834645549 ) ) ;
#73168 = CARTESIAN_POINT ( 'NONE',  ( 1.469816272965879911, 0.2306618581243847221, -0.2411417322834647770 ) ) ;
#73169 = CARTESIAN_POINT ( 'NONE',  ( 0.4330708661417329575, 0.2952755905511811885, 0.000000000000000000 ) ) ;
#73170 = CARTESIAN_POINT ( 'NONE',  ( -0.2887139107611542133, -0.5023911411419708095, -0.1820866141732282451 ) ) ;
#73171 = AXIS2_PLACEMENT_3D ( 'NONE', #22177, #9964, #29317 ) ;
#73172 = CARTESIAN_POINT ( 'NONE',  ( 0.9514435695538062676, -0.3162353388693409650, -0.4822834645669289433 ) ) ;
#73173 = CARTESIAN_POINT ( 'NONE',  ( -1.049868766404198794, -0.6046776061558807314, 0.2411417322834647770 ) ) ;
#73174 = CARTESIAN_POINT ( 'NONE',  ( -0.2230971128608915943, -0.4281496062992127816, -0.4176697321401328100 ) ) ;
#73175 = CARTESIAN_POINT ( 'NONE',  ( -0.9711286089238838626, -0.6046776061558807314, 0.2411417322834647770 ) ) ;
#73176 = CARTESIAN_POINT ( 'NONE',  ( 1.089238845144357537, -0.4281496062992124485, 0.4176697321401328655 ) ) ;
#73177 = CARTESIAN_POINT ( 'NONE',  ( 1.095800524934383846, -0.3162353388693405765, 0.4822834645669290543 ) ) ;
#73178 = CARTESIAN_POINT ( 'NONE',  ( 0.8464566929133866546, -0.5400638737290844871, 0.3530559997133364547 ) ) ;
#73179 = CARTESIAN_POINT ( 'NONE',  ( 4.797336870675656522E-17, -0.3917322834645670104, -0.7007874015748030150 ) ) ;
#73180 = CARTESIAN_POINT ( 'NONE',  ( -0.09186351706036663400, -0.3690944881889763329, 0.3153832671262228327 ) ) ;
#73181 = ORIENTED_EDGE ( 'NONE', *, *, #49228, .F. ) ;
#73182 = CARTESIAN_POINT ( 'NONE',  ( 0.3949938075777409408, 0.1058382717557500574, -1.227034120734908473 ) ) ;
#73183 = ORIENTED_EDGE ( 'NONE', *, *, #42934, .F. ) ;
#73184 = CARTESIAN_POINT ( 'NONE',  ( -0.8530183727034112984, -0.3690944881889765550, -0.3153832671262227771 ) ) ;
#73185 = CARTESIAN_POINT ( 'NONE',  ( 0.07874015748031558404, -0.1870078740157479769, 0.4822834645669291653 ) ) ;
#73186 = CARTESIAN_POINT ( 'NONE',  ( 2.860656214895214156, 1.077434660671929167, 0.1173752429317640178 ) ) ;
#73187 = CARTESIAN_POINT ( 'NONE',  ( -0.1115485564304456306, 0.2952755905511810774, -0.1292274648535930714 ) ) ;
#73188 = CARTESIAN_POINT ( 'NONE',  ( -0.3346456692913377662, -0.5400638737290844871, 0.3530559997133364547 ) ) ;
#73189 = CARTESIAN_POINT ( 'NONE',  ( -1.272965879265091305, 0.05413385826771626580, -0.4176697321401330321 ) ) ;
#73190 = CARTESIAN_POINT ( 'NONE',  ( -1.364829396325458521, 0.2306618581243847221, -0.2411417322834647770 ) ) ;
#73191 = AXIS2_PLACEMENT_3D ( 'NONE', #81776, #49346, #56890 ) ;
#73192 = CARTESIAN_POINT ( 'NONE',  ( 1.220472440944882608, 0.1771653543307087630, 0.000000000000000000 ) ) ;
#73193 = CARTESIAN_POINT ( 'NONE',  ( 0.4724409448818898682, 2.892866454678787531E-17, -1.062992125984252079 ) ) ;
#73194 = CARTESIAN_POINT ( 'NONE',  ( 0.2489800900487909585, 0.1588251575432187424, 5.781310865041811908 ) ) ;
#73195 = CARTESIAN_POINT ( 'NONE',  ( 0.5249343832021003964, 0.1283753931104746893, -0.1820866141732285504 ) ) ;
#73196 = CARTESIAN_POINT ( 'NONE',  ( 8.195543980992789655E-16, -0.1870078740157480879, -0.4822834645669291653 ) ) ;
#73197 = CARTESIAN_POINT ( 'NONE',  ( 0.1574803149606306130, -0.1870078740157480879, -0.4822834645669291653 ) ) ;
#73198 = ORIENTED_EDGE ( 'NONE', *, *, #21598, .T. ) ;
#73199 = CARTESIAN_POINT ( 'NONE',  ( -0.3460692066303960868, 0.1998031496062990242, -1.601049868766404094 ) ) ;
#73200 = CARTESIAN_POINT ( 'NONE',  ( -0.5905511811023615998, 0.2952755905511811885, 0.000000000000000000 ) ) ;
#73201 = ORIENTED_EDGE ( 'NONE', *, *, #58706, .F. ) ;
#73202 = CARTESIAN_POINT ( 'NONE',  ( 0.2925321140481932369, 0.2925321140481932369, -1.316929133858267598 ) ) ;
#73203 = CARTESIAN_POINT ( 'NONE',  ( -0.1998031496062991630, -0.3460692066303959202, -0.6148293963254594097 ) ) ;
#73204 = CARTESIAN_POINT ( 'NONE',  ( -0.4527559055118102749, 0.1660481256975885056, 0.3530559997133364547 ) ) ;
#73205 = CARTESIAN_POINT ( 'NONE',  ( -0.2362204724409451284, 0.4091458600556402425, 0.1443569553805774397 ) ) ;
#73206 = CARTESIAN_POINT ( 'NONE',  ( -0.3917322834645671215, 0.1049643490035301469, -2.479658792650918375 ) ) ;
#73207 = CARTESIAN_POINT ( 'NONE',  ( -1.456692913385826182, 0.1771653543307087630, 0.000000000000000000 ) ) ;
#73208 = CARTESIAN_POINT ( 'NONE',  ( 0.9842519685039375910, 0.2952755905511811885, 0.000000000000000000 ) ) ;
#73209 = CARTESIAN_POINT ( 'NONE',  ( 0.7283464566929143125, 0.1660481256975885056, 0.3530559997133364547 ) ) ;
#73210 = CARTESIAN_POINT ( 'NONE',  ( -0.3083989501312330295, -0.2845877964562161244, -0.3641732283464567121 ) ) ;
#73211 = CARTESIAN_POINT ( 'NONE',  ( 0.2296587926509192634, -0.05778040916215560624, -0.4822834645669293319 ) ) ;
#73212 = CARTESIAN_POINT ( 'NONE',  ( -0.3458507752293906723, -0.3458507752293910609, -1.868110236220472453 ) ) ;
#73213 = CARTESIAN_POINT ( 'NONE',  ( 0.09186351706036827158, -0.004921259842519576551, 0.3153832671262227771 ) ) ;
#73214 = CARTESIAN_POINT ( 'NONE',  ( -0.5577427821522301654, -0.05778040916215560624, -0.4822834645669293319 ) ) ;
#73215 = CARTESIAN_POINT ( 'NONE',  ( 0.1974969037888706092, -0.3420746716998660508, -1.743438320209973913 ) ) ;
#73216 = CARTESIAN_POINT ( 'NONE',  ( -1.620734908136482577, -0.6692913385826773087, -0.1292274648535924053 ) ) ;
#73217 = CARTESIAN_POINT ( 'NONE',  ( 0.09842519685039434474, -0.4536011799217368745, -0.2665933059059886201 ) ) ;
#73218 = CARTESIAN_POINT ( 'NONE',  ( 1.541994750656168645, 0.1771653543307087075, -0.09757992244046823083 ) ) ;
#73219 = CARTESIAN_POINT ( 'NONE',  ( -1.187664041994750175, -0.05778040916215560624, -0.4822834645669293319 ) ) ;
#73220 = CARTESIAN_POINT ( 'NONE',  ( -0.8858267716535425107, -0.4536011799217367080, 0.2665933059059888421 ) ) ;
#73221 = LINE ( 'NONE', #60585, #9051 ) ;
#73222 = CARTESIAN_POINT ( 'NONE',  ( -1.351706036745406347, 0.05413385826771626580, -0.4176697321401330321 ) ) ;
#73223 = CARTESIAN_POINT ( 'NONE',  ( -0.7086614173228339419, -0.1870078740157479769, 0.4822834645669291653 ) ) ;
#73224 = CARTESIAN_POINT ( 'NONE',  ( 0.02624671916010564918, -0.6046776061558809534, -0.2411417322834644161 ) ) ;
#73225 = CARTESIAN_POINT ( 'NONE',  ( 0.3996062992125985480, 2.446882876249141654E-17, -2.399606299212598604 ) ) ;
#73226 = CARTESIAN_POINT ( 'NONE',  ( -0.3392501089628018329, -0.1958661417322836440, -2.494731340386139529 ) ) ;
#73227 = CARTESIAN_POINT ( 'NONE',  ( -2.167269426034507784, 1.502969453419624513, -0.4732359647714766693 ) ) ;
#73228 = CARTESIAN_POINT ( 'NONE',  ( 0.3083989501312343062, -0.08942795157528024563, -0.3641732283464568787 ) ) ;
#73229 = CARTESIAN_POINT ( 'NONE',  ( 1.141732283464567566, 0.2952755905511811885, 0.000000000000000000 ) ) ;
#73230 = CARTESIAN_POINT ( 'NONE',  ( -1.174540682414697335, -0.2845877964562161244, -0.3641732283464567121 ) ) ;
#73231 = CARTESIAN_POINT ( 'NONE',  ( 1.279527559055118724, -0.5400638737290845981, -0.3530559997133363437 ) ) ;
#73232 = CARTESIAN_POINT ( 'NONE',  ( -1.391076115485563758, 0.1283753931104748280, 0.1820866141732283561 ) ) ;
#73233 = CARTESIAN_POINT ( 'NONE',  ( -0.4461942257217840213, 0.2306618581243848609, 0.2411417322834645549 ) ) ;
#73234 = CARTESIAN_POINT ( 'NONE',  ( 0.1246719160104994284, 0.1771653543307087075, -0.09757992244046823083 ) ) ;
#73235 = CARTESIAN_POINT ( 'NONE',  ( 5.785732909357575061E-17, -0.4724409448818898682, -0.8661417322834645827 ) ) ;
#73236 = CARTESIAN_POINT ( 'NONE',  ( 0.5380577427821529035, -0.004921259842519870586, -0.3153832671262229437 ) ) ;
#73237 = PRODUCT_DEFINITION_FORMATION_WITH_SPECIFIED_SOURCE ( 'ANY', '', #3024, .NOT_KNOWN. ) ;
#73238 = EDGE_CURVE ( 'NONE', #81942, #69331, #8939, .T. ) ;
#73239 = CARTESIAN_POINT ( 'NONE',  ( 0.07874015748031558404, -0.1870078740157479769, 0.4822834645669291653 ) ) ;
#73240 = CARTESIAN_POINT ( 'NONE',  ( 0.2925321140481932369, -0.2925321140481931814, -0.4901574803149606474 ) ) ;
#73241 = ADVANCED_FACE ( 'NONE', ( #72312 ), #71892, .F. ) ;
#73242 = CARTESIAN_POINT ( 'NONE',  ( -0.8070866141732276899, -0.5400638737290844871, 0.3530559997133364547 ) ) ;
#73243 = CARTESIAN_POINT ( 'NONE',  ( -0.3392501089628017219, -0.1958661417322836718, -1.711942257217847763 ) ) ;
#73244 = CARTESIAN_POINT ( 'NONE',  ( 1.108923884514436242, -0.08942795157527998196, 0.3641732283464567121 ) ) ;
#73245 = CARTESIAN_POINT ( 'NONE',  ( 0.1377952755905518800, 0.1660481256975883668, -0.3530559997133364547 ) ) ;
#73246 = CARTESIAN_POINT ( 'NONE',  ( -0.3412073490813641308, 0.2306618581243847221, -0.2411417322834647770 ) ) ;
#73247 = CARTESIAN_POINT ( 'NONE',  ( -0.2493438320209966919, -0.3690944881889763329, 0.3153832671262228327 ) ) ;
#73248 = CARTESIAN_POINT ( 'NONE',  ( 1.010849322905839287, 0.004960608223778500969, -0.3437734562760191848 ) ) ;
#73249 = CARTESIAN_POINT ( 'NONE',  ( -0.2690288713910754526, -0.5511811023622046335, 0.09757992244046803654 ) ) ;
#73250 = CARTESIAN_POINT ( 'NONE',  ( 0.3083989501312343062, -0.05778040916215560624, -0.4822834645669293319 ) ) ;
#73251 = CARTESIAN_POINT ( 'NONE',  ( -0.8530183727034112984, -0.3690944881889765550, -0.3153832671262227771 ) ) ;
#73253 = CARTESIAN_POINT ( 'NONE',  ( 0.2925321140481932369, -0.2925321140481931814, -0.9625984251968502381 ) ) ;
#73252 = AXIS2_PLACEMENT_3D ( 'NONE', #60763, #2701, #54442 ) ;
#73254 = CARTESIAN_POINT ( 'NONE',  ( -1.082677165354329896, -0.5400638737290845981, -0.3530559997133363437 ) ) ;
#73255 = CARTESIAN_POINT ( 'NONE',  ( 0.1702530392988864383, 0.004960608223778963273, 0.3437734562760189072 ) ) ;
#73256 = ORIENTED_EDGE ( 'NONE', *, *, #57249, .F. ) ;
#73257 = CARTESIAN_POINT ( 'NONE',  ( -1.030183727034119867, -0.08942795157528024563, -0.3641732283464568787 ) ) ;
#73258 = CARTESIAN_POINT ( 'NONE',  ( -0.5183727034120726440, -0.6692913385826773087, -0.1292274648535924053 ) ) ;
#73259 = CARTESIAN_POINT ( 'NONE',  ( -1.561679790026246017, 0.05413385826771666132, 0.4176697321401328100 ) ) ;
#73260 = CARTESIAN_POINT ( 'NONE',  ( -1.141732283464566011, 0.2952755905511811885, 0.000000000000000000 ) ) ;
#73261 = CARTESIAN_POINT ( 'NONE',  ( -0.2362204724409447953, -0.4091458600556404646, -2.112860892388451539 ) ) ;
#73262 = ADVANCED_FACE ( 'NONE', ( #2847 ), #55946, .F. ) ;
#73263 = CARTESIAN_POINT ( 'NONE',  ( 1.410761154855643795, -0.05778040916215560624, -0.4822834645669293319 ) ) ;
#73264 = CARTESIAN_POINT ( 'NONE',  ( 0.8333333333333340365, -0.6692913385826771977, 0.1292274648535927661 ) ) ;
#73265 = CARTESIAN_POINT ( 'NONE',  ( 1.568241469816273437, -0.3162353388693405765, 0.4822834645669290543 ) ) ;
#73266 = DIRECTION ( 'NONE',  ( 0.000000000000000000, 0.000000000000000000, 1.000000000000000000 ) ) ;
#73267 = EDGE_CURVE ( 'NONE', #58699, #8650, #67243, .T. ) ;
#73268 = CARTESIAN_POINT ( 'NONE',  ( -1.725721784776902190, -0.05778040916215522460, 0.4822834645669289988 ) ) ;
#73269 = CARTESIAN_POINT ( 'NONE',  ( 0.1998031496062992740, 0.3460692066303959757, -0.6167979002624671692 ) ) ;
#73270 = ORIENTED_EDGE ( 'NONE', *, *, #76295, .F. ) ;
#73271 = CARTESIAN_POINT ( 'NONE',  ( -0.5052493438320203589, 0.1771653543307087075, -0.09757992244046823083 ) ) ;
#73272 = CARTESIAN_POINT ( 'NONE',  ( 0.3392501089628018329, 0.1958661417322835607, -2.328083989501312345 ) ) ;
#73273 = EDGE_LOOP ( 'NONE', ( #46346, #60316, #36100, #17598 ) ) ;
#73274 = CARTESIAN_POINT ( 'NONE',  ( 0.9973753280839902091, 0.2306618581243847221, -0.2411417322834647770 ) ) ;
#73276 = CARTESIAN_POINT ( 'NONE',  ( 5.463695987328526437E-16, -0.1870078740157479769, 0.4822834645669291653 ) ) ;
#73275 = PRODUCT_RELATED_PRODUCT_CATEGORY ( 'part', '', ( #3024 ) ) ;
#73277 = CARTESIAN_POINT ( 'NONE',  ( -0.6889763779527552368, 0.1660481256975885056, 0.3530559997133364547 ) ) ;
#73278 = CARTESIAN_POINT ( 'NONE',  ( 1.377952755905512472, 0.2952755905511811885, 0.000000000000000000 ) ) ;
#73279 = CARTESIAN_POINT ( 'NONE',  ( -1.489501312335957062, -0.08942795157527998196, 0.3641732283464567121 ) ) ;
#73280 = CARTESIAN_POINT ( 'NONE',  ( 0.03820975525947114398, 1.064507315957821998, -1.600359255881266041 ) ) ;
#73281 = CARTESIAN_POINT ( 'NONE',  ( 0.5446194225721792126, -0.3162353388693405765, 0.4822834645669290543 ) ) ;
#73282 = CARTESIAN_POINT ( 'NONE',  ( 0.6627296587926515548, 0.1771653543307087630, 0.09757992244046791164 ) ) ;
#73283 = CARTESIAN_POINT ( 'NONE',  ( -0.6496062992125976043, 0.1660481256975883668, -0.3530559997133364547 ) ) ;
#73284 = CARTESIAN_POINT ( 'NONE',  ( -0.1049643490035306742, 0.3917322834645668994, -1.503917692092176628 ) ) ;
#73285 = CARTESIAN_POINT ( 'NONE',  ( -1.299212598425196097, 0.2952755905511811885, 0.000000000000000000 ) ) ;
#73286 = CARTESIAN_POINT ( 'NONE',  ( 8.318810292902001717E-17, 2.401574803149606474, 0.4915354330708643360 ) ) ;
#73287 = CARTESIAN_POINT ( 'NONE',  ( 0.8595800524934390507, -0.3162353388693405765, 0.4822834645669290543 ) ) ;
#73288 = CARTESIAN_POINT ( 'NONE',  ( 1.135170603674541256, -0.5511811023622048555, -0.09757992244046775898 ) ) ;
#73289 = ORIENTED_EDGE ( 'NONE', *, *, #46574, .T. ) ;
#73290 = CARTESIAN_POINT ( 'NONE',  ( -0.3917322834645670659, -7.196005306013484475E-17, -2.713273908957691827 ) ) ;
#73291 = CARTESIAN_POINT ( 'NONE',  ( -0.5643044619422565855, -0.4281496062992124485, 0.4176697321401328655 ) ) ;
#73292 = EDGE_LOOP ( 'NONE', ( #73836, #49247, #34786, #50805 ) ) ;
#73293 = CARTESIAN_POINT ( 'NONE',  ( 0.2821522309711292364, -0.5511811023622046335, 0.09757992244046803654 ) ) ;
#73294 = CARTESIAN_POINT ( 'NONE',  ( -1.089238845144356427, 0.05413385826771666132, 0.4176697321401328100 ) ) ;
#73295 = CARTESIAN_POINT ( 'NONE',  ( 0.8267716535433077274, 0.2952755905511811885, 0.000000000000000000 ) ) ;
#73296 = CARTESIAN_POINT ( 'NONE',  ( 0.9055118110236227702, -0.6692913385826771977, 8.415575281601705876E-17 ) ) ;
#73297 = CARTESIAN_POINT ( 'NONE',  ( 0.02624671916010564918, 0.2306618581243848609, 0.2411417322834645549 ) ) ;
#73298 = CARTESIAN_POINT ( 'NONE',  ( -0.5511811023622038563, -0.1870078740157479769, 0.4822834645669291653 ) ) ;
#73299 = CARTESIAN_POINT ( 'NONE',  ( 4.797336870675656522E-17, -0.3917322834645670104, -2.053149606299212948 ) ) ;
#73300 = CARTESIAN_POINT ( 'NONE',  ( -1.587926509186350810, -0.4281496062992124485, 0.4176697321401328655 ) ) ;
#73301 = CARTESIAN_POINT ( 'NONE',  ( -0.5118110236220466680, 0.2952755905511811885, 0.000000000000000000 ) ) ;
#73302 = EDGE_CURVE ( 'NONE', #9114, #29875, #39901, .T. ) ;
#73303 = CARTESIAN_POINT ( 'NONE',  ( -0.4461942257217840213, -0.5023911411419708095, -0.1820866141732282451 ) ) ;
#73304 = CARTESIAN_POINT ( 'NONE',  ( 1.213910761154856299, 0.2952755905511811885, 0.1292274648535926551 ) ) ;
#73305 = CARTESIAN_POINT ( 'NONE',  ( 1.620734908136483465, -0.6692913385826771977, 0.1292274648535927661 ) ) ;
#73306 = CARTESIAN_POINT ( 'NONE',  ( -0.8923884514435688198, 0.2306618581243847221, -0.2411417322834647770 ) ) ;
#73307 = CARTESIAN_POINT ( 'NONE',  ( 0.2925321140481932369, -0.2925321140481931814, -0.01771653543307087630 ) ) ;
#73308 = CARTESIAN_POINT ( 'NONE',  ( 0.6364829396325465405, -0.05778040916215522460, 0.4822834645669289988 ) ) ;
#73309 = CARTESIAN_POINT ( 'NONE',  ( -0.3460692066303960868, 0.1998031496062990242, -2.073490813648294129 ) ) ;
#73310 = CARTESIAN_POINT ( 'NONE',  ( -0.6912002312465808096, 1.909921115055098095, -0.5309055118110235227 ) ) ;
#73311 = CARTESIAN_POINT ( 'NONE',  ( -0.2296587926509179312, -0.05778040916215522460, 0.4822834645669289988 ) ) ;
#73312 = AXIS2_PLACEMENT_3D ( 'NONE', #12771, #43078, #76740 ) ;
#73313 = CARTESIAN_POINT ( 'NONE',  ( -1.358267716535432434, -0.4536011799217367080, 0.2665933059059888421 ) ) ;
#73314 = CARTESIAN_POINT ( 'NONE',  ( 0.9908136482939640111, -0.5511811023622046335, 0.09757992244046803654 ) ) ;
#73315 = CARTESIAN_POINT ( 'NONE',  ( 0.3458507752293908943, -0.3458507752293908943, -0.8051181102362205966 ) ) ;
#73316 = CARTESIAN_POINT ( 'NONE',  ( 1.253280839895013710, -0.08942795157528024563, -0.3641732283464568787 ) ) ;
#73317 = CARTESIAN_POINT ( 'NONE',  ( 0.7677165354330716118, -0.5400638737290844871, 0.3530559997133364547 ) ) ;
#73318 = AXIS2_PLACEMENT_3D ( 'NONE', #60019, #48216, #60845 ) ;
#73319 = CARTESIAN_POINT ( 'NONE',  ( -0.3420746716998660508, -0.1974969037888706924, -0.4442257217847768724 ) ) ;
#73320 = CARTESIAN_POINT ( 'NONE',  ( -0.4461942257217840213, 0.2306618581243848609, 0.2411417322834645549 ) ) ;
#73321 = DIRECTION ( 'NONE',  ( -0.7071067811865489050, -0.000000000000000000, 0.7071067811865460184 ) ) ;
#73322 = CARTESIAN_POINT ( 'NONE',  ( 1.443569553805774897, 0.1283753931104748280, 0.1820866141732283561 ) ) ;
#73323 = CARTESIAN_POINT ( 'NONE',  ( -0.5118110236220466680, -0.6692913385826771977, 8.415575281601705876E-17 ) ) ;
#73324 = CARTESIAN_POINT ( 'NONE',  ( -0.2891555358219911054, 0.2891555358219909388, -0.4114173228346456046 ) ) ;
#73325 = CARTESIAN_POINT ( 'NONE',  ( 1.332020997375329197, -0.3162353388693405765, 0.4822834645669290543 ) ) ;
#73326 = CARTESIAN_POINT ( 'NONE',  ( 0.02624671916010564918, 0.2306618581243848609, 0.2411417322834645549 ) ) ;
#73327 = CARTESIAN_POINT ( 'NONE',  ( 0.6561679790026253567, -0.5023911411419708095, -0.1820866141732282451 ) ) ;
#73328 = CARTESIAN_POINT ( 'NONE',  ( -0.1090865357759267934, 1.075440515114686191, -1.116837428146558064 ) ) ;
#73329 = CARTESIAN_POINT ( 'NONE',  ( 0.3477690288713918276, -0.5511811023622048555, -0.09757992244046775898 ) ) ;
#73330 = CARTESIAN_POINT ( 'NONE',  ( -1.069553805774277722, 0.2066929133858267931, 0.1054918080437490802 ) ) ;
#73331 = ADVANCED_FACE ( 'NONE', ( #1605 ), #73562, .T. ) ;
#73332 = CARTESIAN_POINT ( 'NONE',  ( 0.1998031496062992463, 0.3460692066303959202, -1.323490813648294129 ) ) ;
#73333 = CARTESIAN_POINT ( 'NONE',  ( 0.9580052493438327987, -0.4281496062992127816, -0.4176697321401328100 ) ) ;
#73334 = CARTESIAN_POINT ( 'NONE',  ( 0.3917322834645669549, 0.1049643490035304660, -1.061679790026246462 ) ) ;
#73335 = CARTESIAN_POINT ( 'NONE',  ( 1.673228346456693494, 0.07958543189024085140, 0.2665933059059887866 ) ) ;
#73336 = FACE_OUTER_BOUND ( 'NONE', #42005, .T. ) ;
#73337 = CARTESIAN_POINT ( 'NONE',  ( -0.03937007874015669567, -0.5511811023622047445, 6.969142054262312111E-17 ) ) ;
#73338 = B_SPLINE_CURVE_WITH_KNOTS ( 'NONE', 3,
 ( #75544, #76365, #81864, #57393 ),
 .UNSPECIFIED., .F., .F.,
 ( 4, 4 ),
 ( 0.1208891233417057898, 0.1223338575624300234 ),
 .UNSPECIFIED. ) ;
#73339 = CARTESIAN_POINT ( 'NONE',  ( 0.2034120734908144990, -0.6692913385826771977, 0.1292274648535927661 ) ) ;
#73340 = CARTESIAN_POINT ( 'NONE',  ( 1.515748031496063408, 0.07958543189024085140, 0.2665933059059887866 ) ) ;
#73341 = CARTESIAN_POINT ( 'NONE',  ( -1.535433070866141225, 0.1771653543307087630, 0.000000000000000000 ) ) ;
#73342 = CARTESIAN_POINT ( 'NONE',  ( -1.332020997375327642, -0.3162353388693409650, -0.4822834645669289433 ) ) ;
#73343 = CARTESIAN_POINT ( 'NONE',  ( 0.6364829396325465405, -0.3162353388693409650, -0.4822834645669289433 ) ) ;
#73344 = CARTESIAN_POINT ( 'NONE',  ( 1.581364829396326277, -0.3162353388693409650, -0.4822834645669289433 ) ) ;
#73345 = ADVANCED_FACE ( 'NONE', ( #47028 ), #79463, .T. ) ;
#73346 = CARTESIAN_POINT ( 'NONE',  ( 0.4724409448818897017, 0.1265901696524990294, -0.2014435695538057958 ) ) ;
#73347 = CARTESIAN_POINT ( 'NONE',  ( 0.7742782152230978099, -0.4281496062992124485, 0.4176697321401328655 ) ) ;
#73348 = CARTESIAN_POINT ( 'NONE',  ( 1.167979002624672580, -0.4281496062992124485, 0.4176697321401328655 ) ) ;
#73349 = CARTESIAN_POINT ( 'NONE',  ( 0.8464566929133866546, -0.5400638737290844871, 0.3530559997133364547 ) ) ;
#73350 = CARTESIAN_POINT ( 'NONE',  ( -1.660104986876639543, -0.08942795157528024563, -0.3641732283464568787 ) ) ;
#73351 = CARTESIAN_POINT ( 'NONE',  ( 1.108923884514436686, -0.2845877964562161244, -0.3641732283464567121 ) ) ;
#73352 = CARTESIAN_POINT ( 'NONE',  ( 1.640419947506562393, -0.4281496062992124485, 0.4176697321401328655 ) ) ;
#73353 = CARTESIAN_POINT ( 'NONE',  ( -0.7152230971128602510, -0.2845877964562159024, 0.3641732283464567677 ) ) ;
#73354 = CARTESIAN_POINT ( 'NONE',  ( 0.4133858267716541968, -0.4536011799217368745, -0.2665933059059886201 ) ) ;
#73355 = CARTESIAN_POINT ( 'NONE',  ( 0.006561679790026889343, -0.3162353388693409650, -0.4822834645669289433 ) ) ;
#73356 = CARTESIAN_POINT ( 'NONE',  ( 0.7611548556430451917, -0.6046776061558807314, 0.2411417322834647770 ) ) ;
#73357 = CARTESIAN_POINT ( 'NONE',  ( -0.1706036745406816491, 0.05413385826771626580, -0.4176697321401330321 ) ) ;
#73358 = CARTESIAN_POINT ( 'NONE',  ( 0.2755905511811031494, -0.5511811023622047445, 6.969142054262312111E-17 ) ) ;
#73359 = CARTESIAN_POINT ( 'NONE',  ( 1.318897637795276356, 0.1660481256975883668, -0.3530559997133364547 ) ) ;
#73360 = PLANE ( 'NONE',  #67557 ) ;
#73361 = CARTESIAN_POINT ( 'NONE',  ( -1.010498687664041384, -0.4281496062992127816, -0.4176697321401328100 ) ) ;
#73362 = CARTESIAN_POINT ( 'NONE',  ( 0.3996062992125986035, 2.446882876249141962E-17, -0.9055118110236221041 ) ) ;
#73363 = CARTESIAN_POINT ( 'NONE',  ( 2.167714792466672868, 1.572145545125847033, -0.4734416007054413345 ) ) ;
#73365 = AXIS2_PLACEMENT_3D ( 'NONE', #49371, #16166, #11083 ) ;
#73364 = CARTESIAN_POINT ( 'NONE',  ( -0.7874015748031489847, -0.1870078740157480879, -0.4822834645669291653 ) ) ;
#73366 = CARTESIAN_POINT ( 'NONE',  ( -0.5511811023622041894, -0.1870078740157480879, -0.4822834645669291653 ) ) ;
#73367 = CARTESIAN_POINT ( 'NONE',  ( 0.4724409448818898682, 2.892866454678787531E-17, 0.03937007874015747977 ) ) ;
#73368 = CARTESIAN_POINT ( 'NONE',  ( -0.1974969037888703871, -0.3420746716998661063, -2.427821522309711266 ) ) ;
#73369 = ORIENTED_EDGE ( 'NONE', *, *, #30564, .F. ) ;
#73370 = CARTESIAN_POINT ( 'NONE',  ( 0.8070866141732289112, -0.4536011799217368745, -0.2665933059059886201 ) ) ;
#73371 = CARTESIAN_POINT ( 'NONE',  ( 0.1958661417322834775, 0.3392501089628018884, -0.7664041994750655507 ) ) ;
#73372 = CARTESIAN_POINT ( 'NONE',  ( 1.279527559055118724, 0.1660481256975885056, 0.3530559997133364547 ) ) ;
#73373 = FACE_OUTER_BOUND ( 'NONE', #5171, .T. ) ;
#73374 = CARTESIAN_POINT ( 'NONE',  ( -1.404199475065615932, -0.004921259842519576551, 0.3153832671262227771 ) ) ;
#73375 = CARTESIAN_POINT ( 'NONE',  ( 1.620734908136483465, -0.6692913385826771977, 0.1292274648535927661 ) ) ;
#73376 = CARTESIAN_POINT ( 'NONE',  ( -1.437007874015747477, -0.5400638737290844871, 0.3530559997133364547 ) ) ;
#73377 = CARTESIAN_POINT ( 'NONE',  ( -0.3917322834645668994, -0.1049643490035306742, -0.2834452511472947966 ) ) ;
#73378 = CARTESIAN_POINT ( 'NONE',  ( -0.1443569553805765515, -0.4281496062992127816, -0.4176697321401328100 ) ) ;
#73379 = CARTESIAN_POINT ( 'NONE',  ( -0.3018372703412066094, -0.004921259842519576551, 0.3153832671262227771 ) ) ;
#73380 = CARTESIAN_POINT ( 'NONE',  ( 0.8530183727034126306, 0.05413385826771626580, -0.4176697321401330321 ) ) ;
#73381 = CARTESIAN_POINT ( 'NONE',  ( -0.1837270341207343505, -0.6046776061558807314, 0.2411417322834647770 ) ) ;
#73382 = CARTESIAN_POINT ( 'NONE',  ( 0.4840268112322921312, 0.02791078216816386681, 0.4328096321851896966 ) ) ;
#73383 = CARTESIAN_POINT ( 'NONE',  ( 2.795275590551181910, 1.771653543307087242, 0.000000000000000000 ) ) ;
#73384 = CARTESIAN_POINT ( 'NONE',  ( 0.1049643490035304799, -0.3917322834645670104, -1.499363147802836860 ) ) ;
#73385 = CARTESIAN_POINT ( 'NONE',  ( 0.7480314960629927956, 0.2952755905511811885, 0.000000000000000000 ) ) ;
#73386 = CARTESIAN_POINT ( 'NONE',  ( 0.2230971128608929543, 0.05413385826771626580, -0.4176697321401330321 ) ) ;
#73387 = CARTESIAN_POINT ( 'NONE',  ( -1.062992125984250968, -0.6692913385826771977, 8.415575281601705876E-17 ) ) ;
#73388 = EDGE_CURVE ( 'NONE', #62716, #53039, #58662, .T. ) ;
#73389 = CARTESIAN_POINT ( 'NONE',  ( 1.036745406824147508, -0.4281496062992127816, -0.4176697321401328100 ) ) ;
#73390 = CARTESIAN_POINT ( 'NONE',  ( 0.8398950131233602345, -0.6046776061558807314, 0.2411417322834647770 ) ) ;
#73391 = CARTESIAN_POINT ( 'NONE',  ( -0.2867679344610365999, 0.2867679344610364889, -1.049212598425196763 ) ) ;
#73392 = CARTESIAN_POINT ( 'NONE',  ( -0.3937007874015740483, -0.1870078740157480879, -0.4822834645669291653 ) ) ;
#73393 = CARTESIAN_POINT ( 'NONE',  ( 0.4593175853018380828, 0.05413385826771626580, -0.4176697321401330321 ) ) ;
#73394 = CARTESIAN_POINT ( 'NONE',  ( 0.1115485564304470323, 0.2952755905511811885, 0.1292274648535926551 ) ) ;
#73395 = ADVANCED_FACE ( 'NONE', ( #8333 ), #33999, .F. ) ;
#73396 = CARTESIAN_POINT ( 'NONE',  ( 0.8005249343832028242, -0.3690944881889765550, -0.3153832671262227771 ) ) ;
#73397 = CARTESIAN_POINT ( 'NONE',  ( -1.299212598425196097, -0.6692913385826771977, 8.415575281601705876E-17 ) ) ;
#73398 = CARTESIAN_POINT ( 'NONE',  ( -1.627296587926508442, -0.6046776061558809534, -0.2411417322834644161 ) ) ;
#73399 = CARTESIAN_POINT ( 'NONE',  ( 0.3412073490813655186, 0.2306618581243848609, 0.2411417322834645549 ) ) ;
#73400 = CARTESIAN_POINT ( 'NONE',  ( 0.1181102362204724532, -0.04921259842519685318, -0.08523872084492505052 ) ) ;
#73401 = CARTESIAN_POINT ( 'NONE',  ( -0.3917322834645671215, 0.1049643490035301469, -2.229658792650918819 ) ) ;
#73402 = ORIENTED_EDGE ( 'NONE', *, *, #72915, .T. ) ;
#73403 = ORIENTED_EDGE ( 'NONE', *, *, #9959, .T. ) ;
#73404 = CARTESIAN_POINT ( 'NONE',  ( 0.9776902887139113929, -0.6692913385826773087, -0.1292274648535924053 ) ) ;
#73405 = CARTESIAN_POINT ( 'NONE',  ( 0.5905511811023629321, -0.5511811023622047445, 6.969142054262312111E-17 ) ) ;
#73406 = VECTOR ( 'NONE', #51660, 39.37007874015748143 ) ;
#73407 = AXIS2_PLACEMENT_3D ( 'NONE', #7058, #71876, #72703 ) ;
#73409 = CARTESIAN_POINT ( 'NONE',  ( -0.7767023820430439818, -3.623651218081290895E-15, 0.4118477457932994690 ) ) ;
#73408 = CARTESIAN_POINT ( 'NONE',  ( 0.4562955581495489743, 1.668131542012062596, 2.130163876373972531 ) ) ;
#73410 = B_SPLINE_CURVE_WITH_KNOTS ( 'NONE', 3,
 ( #48909, #55627, #48081, #81336 ),
 .UNSPECIFIED., .F., .F.,
 ( 4, 4 ),
 ( 0.000000000000000000, 0.001493228121701133636 ),
 .UNSPECIFIED. ) ;
#73411 = DIRECTION ( 'NONE',  ( -0.8660254037844433705, 0.000000000000000000, 0.4999999999999920064 ) ) ;
#73412 = LENGTH_MEASURE_WITH_UNIT ( LENGTH_MEASURE( 0.02539999999999999897 ), #42231 );
#73413 = CARTESIAN_POINT ( 'NONE',  ( 0.3392501089628018329, 0.1958661417322835607, -1.318241469816273215 ) ) ;
#73414 = CARTESIAN_POINT ( 'NONE',  ( 0.3996062992125985480, 2.446882876249141654E-17, -2.399606299212598604 ) ) ;
#73415 = CARTESIAN_POINT ( 'NONE',  ( -0.7349081364829387342, -0.6046776061558807314, 0.2411417322834647770 ) ) ;
#73416 = CARTESIAN_POINT ( 'NONE',  ( -0.5971128608923877978, 0.2952755905511811885, 0.1292274648535926551 ) ) ;
#73417 = CARTESIAN_POINT ( 'NONE',  ( 1.135170603674541256, 0.2952755905511811885, 0.1292274648535926551 ) ) ;
#73418 = ORIENTED_EDGE ( 'NONE', *, *, #34082, .F. ) ;
#73419 = CARTESIAN_POINT ( 'NONE',  ( 1.240157480314961314, -0.5400638737290844871, 0.3530559997133364547 ) ) ;
#73420 = CARTESIAN_POINT ( 'NONE',  ( -1.169606216052558434, -4.983732387537991731E-15, 0.3791483426435189874 ) ) ;
#73421 = DIRECTION ( 'NONE',  ( 1.000000000000000000, -0.000000000000000000, -0.000000000000000000 ) ) ;
#73422 = CARTESIAN_POINT ( 'NONE',  ( -0.2925321140481932369, 0.2925321140481930704, -2.143700787401574104 ) ) ;
#73423 = CARTESIAN_POINT ( 'NONE',  ( -1.522309711286088607, -0.5023911411419708095, 0.1820866141732285504 ) ) ;
#73424 = CARTESIAN_POINT ( 'NONE',  ( 1.614173228346456712, 0.000000000000000000, 0.1372047244094478646 ) ) ;
#73425 = CARTESIAN_POINT ( 'NONE',  ( 0.1049868766404206816, 0.2306618581243848609, 0.2411417322834645549 ) ) ;
#73426 = AXIS2_PLACEMENT_3D ( 'NONE', #31360, #22994, #62122 ) ;
#73427 = CARTESIAN_POINT ( 'NONE',  ( 1.469816272965879911, -0.6046776061558807314, 0.2411417322834647770 ) ) ;
#73428 = CARTESIAN_POINT ( 'NONE',  ( -1.102362204724408601, -0.1870078740157479769, 0.3641732283464567677 ) ) ;
#73429 = CARTESIAN_POINT ( 'NONE',  ( 0.5971128608923891301, 0.2952755905511810774, -0.1292274648535930714 ) ) ;
#73430 = CARTESIAN_POINT ( 'NONE',  ( 1.332020997375328974, -0.08942795157528024563, -0.3641732283464568787 ) ) ;
#73431 = CARTESIAN_POINT ( 'NONE',  ( -0.1049643490035301746, -0.3917322834645670659, -1.412054175031808967 ) ) ;
#73432 = CARTESIAN_POINT ( 'NONE',  ( -0.9055118110236215490, 0.1771653543307087630, 0.000000000000000000 ) ) ;
#73433 = CARTESIAN_POINT ( 'NONE',  ( 1.482939632545932307, -0.4281496062992124485, 0.4176697321401328655 ) ) ;
#73434 = DIRECTION ( 'NONE',  ( 0.000000000000000000, 0.000000000000000000, 1.000000000000000000 ) ) ;
#73435 = CARTESIAN_POINT ( 'NONE',  ( -0.09842519685039295696, 0.1660481256975883668, -0.3530559997133364547 ) ) ;
#73436 = CARTESIAN_POINT ( 'NONE',  ( -1.476377952755905110, 0.07958543189024085140, 0.2665933059059887866 ) ) ;
#73437 = CARTESIAN_POINT ( 'NONE',  ( -0.1574803149606292529, -0.1870078740157479769, 0.3641732283464567677 ) ) ;
#73438 = CARTESIAN_POINT ( 'NONE',  ( -0.4593175853018366950, 0.05413385826771666132, 0.4176697321401328100 ) ) ;
#73439 = CARTESIAN_POINT ( 'NONE',  ( 1.692913385826772421, 0.2952755905511811885, 0.000000000000000000 ) ) ;
#73440 = CARTESIAN_POINT ( 'NONE',  ( 0.1049643490035303967, 0.3917322834645670659, -0.6200980559393196589 ) ) ;
#73441 = CARTESIAN_POINT ( 'NONE',  ( 0.3871391076115492380, -0.05778040916215560624, -0.4822834645669293319 ) ) ;
#73442 = B_SPLINE_CURVE_WITH_KNOTS ( 'NONE', 3,
 ( #76304, #63242, #51419, #51843 ),
 .UNSPECIFIED., .F., .F.,
 ( 4, 4 ),
 ( 0.05218731980467040954, 0.05362944292333594182 ),
 .UNSPECIFIED. ) ;
#73443 =( BOUNDED_SURFACE ( )  B_SPLINE_SURFACE ( 1, 2, ( 
 ( #79751, #35529, #48150, #9442, #27966, #73845, #16185, #14937, #34288, #79332, #61191, #21652, #3547, #3130, #59950, #35113, #2305, #8203, #47312, #53624, #73002, #41832, #47728, #15354, #59532, #29213, #54880, #9034, #33868, #1889, #28795, #41015, #2717, #46896, #73427, #27549, #53207, #78919, #21241, #72590, #66701, #34708, #40596, #66278, #60369, #67111, #28377, #54458, #54038, #80172, #22486, #43887, #5599, #48975, #17838, #50208, #36759, #37585, #24942, #56112, #4772, #81818, #76320, #30448, #10696, #24128, #82628, #67939, #50615, #56932, #36351, #75499, #42244, #10281, #49390, #61617, #62027, #11103, #31266, #35947, #82224, #11930, #49797, #3959, #43473, #68759, #55694, #29622, #55282, #80992, #23305, #69169, #4363, #75906, #11520, #37177, #23719, #74674, #17020, #62856, #30031, #42659, #63258, #75084, #56522, #68357, #5192, #81402, #17431, #43062, #62435, #30857, #24544, #18245, #69584, #27039, #37996, #39673, #6847, #52700, #548, #20317, #63672, #71665, #19903, #64931, #38831, #18650, #45551, #58179, #59031, #14016, #51439, #44294, #77569, #1386, #12340, #31684, #44704, #6013, #77142, #45127, #51864, #39248, #77988, #83039, #975, #57343, #13181, #65366, #26201, #71248, #58607, #13594, #25778, #7269, #7701, #32517, #32941, #69985, #57761, #51025, #25362, #64095, #76724, #70400, #123, #33368, #45970, #26629, #19056, #64510, #12756, #38414, #52283, #6431, #32102, #19475, #70833, #40094, #42457, #35743, #1795, #78410, #48359, #16404, #33779, #55495, #61411, #68157, #74474, #60998, #10501, #23520, #55083, #54677, #80792, #46390, #61828, #21154, #36155, #4168, #16821, #72085, #27457, #74058, #14849, #3346, #23109, #80388, #14442, #40509, #81205, #65781, #8113, #59442, #42050, #46809, #29832, #67746, #22700, #9665, #53116, #20739, #78827, #10080, #35334, #72500, #48775, #67332, #3760, #29011, #29425, #59711, #72362, #40773, #27312, #28146, #15535, #46668, #78685, #14710, #66883, #21008, #1247, #40365, #73185, #58464, #41195, #47493, #26896, #66045, #32795, #65215, #827, #53802, #65642, #26486, #8383, #52137, #77844, #45823, #58888, #20173, #7972, #59298, #34048, #53397, #8794, #13868, #15119, #71522, #52971, #79515, #2066, #27732, #72768, #79104, #39956, #21423, #2487, #47077, #66458, #39527, #71943, #7554, #33225, #78264, #52555, #20595, #14295, #46247, #34470, #60136, #21830, #33635, #1655, #75257, #16779, #47907, #68117, #74017, #55867, #79934, #36522, #36116, #9623, #34886, #23067, #48735, #73612, #49563, #10462, #10862, #17195, #67703, #62198, #17601, #55454, #3722, #81163, #60547, #30205, #3306, #4535, #81580, #42828, #2898, #67290, #74432, #80348, #10039, #23479, #29386, #28562, #54218, #61788, #35703, #4128, #43233, #22249, #15954, #35294, #41600, #61372, #55046, #42417, #29793, #68521, #60956, #74853, #28971, #80753, #23897, #49146, #9213, #54638, #22661, #16364, #48320, #42009, #57102, #70157, #77316, #24712, #18010, #19646, #31027, #24302, #37355, #50380, #297, #70575, #12510, #6601, #63434, #68930, #51611, #76492, #49972, #44466, #76078, #32273, #56291, #12929, #38171, #69347, #11279, #82797, #25121, #75670, #25953, #63845, #38589, #76896, #44063, #64267, #36938, #31861, #5770, #57520, #62616, #57933, #63028, #4958, #30626, #19226, #81988, #43644, #50791, #56695, #69755, #83211, #31439, #11701, #5366, #6183, #12101, #82394, #18422, #37759, #18819, #25533, #51198, #44876, #53292, #59197, #7870, #26794, #718, #79413, #27210, #39424, #7021, #66360, #52451, #59612, #71420, #26376, #33948, #8282, #15019, #58786, #65108, #40675, #20071, #45307, #53704, #64682, #8698, #33534, #71002, #52873, #46976, #32689, #34369, #46562, #1967, #78583, #2390, #27630, #77740, #28046, #60034, #78161, #13345, #38999, #58356, #52036, #1556, #45723, #20909, #72670, #13767, #7446, #72261, #79004, #14609, #33116, #21323, #1144, #20492, #46146, #71841, #14191, #40263, #39848, #65539, #65946, #48950, #66785, #81377, #49364, #56088, #43447, #82199, #3937, #5168, #9120, #17408, #43856, #4747, #81793, #62834, #30420, #30004, #17814, #75880, #11076, #24104, #31241 ),
 ( #49773, #30832, #56907, #18221, #69559, #63235, #73086, #68332, #36327, #36733, #24517, #56497, #75473, #10671, #50183, #11907, #55257, #74651, #62002, #37561, #4338, #5575, #69145, #16992, #11495, #42635, #21732, #55668, #23690, #75060, #47395, #62408, #43038, #15436, #41097, #35924, #68734, #61591, #29596, #37149, #80966, #23280, #63647, #38805, #32915, #33344, #44269, #18626, #12314, #19029, #25334, #26604, #20292, #44677, #521, #96, #26174, #5986, #64904, #31657, #70372, #7241, #51836, #64481, #58581, #77114, #77962, #65337, #39646, #13565, #57315, #7672, #45940, #32073, #82603, #58152, #24921, #76296, #37972, #50997, #69960, #57733, #25749, #32489, #19875, #947, #83012, #52256, #76695, #19447, #71638, #6819, #77540, #39219, #45524, #6403, #71222, #13990, #70801, #50588, #12727, #38386, #64063, #51412, #45098, #13154, #27428, #40485, #73732, #60666, #2604, #80052, #53513, #59006, #41715, #66578, #14416, #34589, #66163, #22371, #46365, #3014, #28262, #59414, #1361, #72888, #15237, #40069, #16069, #60256, #28681, #66998, #34169, #54342, #67407, #21954, #79221, #47612, #27013, #48030, #53089, #9742, #52675, #9330, #78382, #33753, #40897, #46785, #59832, #73308, #21537, #20713, #72058, #53924, #2185, #72476, #65756, #8089, #1771, #78801, #47197, #21126, #35000, #8913, #79636, #8503, #14825, #27853, #15656, #41315, #80467, #56405, #42540, #49679, #61495, #74139, #24011, #81700, #5073, #48855, #29503, #30742, #10163, #69463, #43757, #54761, #82104, #23596, #35413, #17315, #37053, #22778, #24417, #36637, #75371, #68638, #55163, #62313, #36234, #4650, #16483, #17717, #42130, #80873, #43345, #30321, #74969, #69047, #29908, #50087, #18125, #49267, #81280, #42943, #61078, #10977, #3843, #55989, #75783, #3428, #29091, #48439, #23185, #67825, #4246, #11396, #61904, #35829, #74556, #55572, #16901, #68242, #62736, #10577, #25652, #64383, #76603, #63964, #32812, #69869, #70275, #843, #76195, #19770, #39119, #37468, #7139, #51733, #418, #3359, #70698, #77859, #18533, #31977, #26501, #50903, #18934, #51314, #20188, #52153, #13462, #44582, #77435, #6301, #32389, #50492, #77017, #44999, #19349, #45423, #63141, #13051, #71119, #45839, #64800, #58479, #11813, #5482, #57216, #25238, #38704, #31142, #56809, #6719, #82918, #82508, #24824, #44176, #37878, #12629, #12221, #38288, #63552, #58052, #5886, #26074, #31559, #57637, #52988, #59315, #27328, #21848, #27749, #78701, #65233, #9231, #66901, #14727, #47512, #79534, #8811, #46685, #8399, #52572, #53413, #73204, #22268, #33242, #7570, #1264, #7988, #14312, #15554, #34904, #2918, #39972, #58904, #40380, #40791, #66063, #26912, #65659, #34066, #60567, #79955, #28164, #41213, #2084, #66476, #21024, #59729, #28581, #46264, #72378, #54238, #78280, #71537, #13885, #39544, #20612, #53820, #60153, #79122, #47095, #71959, #33652, #21439, #1671, #72785, #15135, #34487, #2505, #62636, #49582, #3741, #4556, #16799, #68541, #3326, #36134, #81183, #61807, #81600, #15973, #49166, #30226, #82008, #17621, #68950, #4980, #41620, #10059, #61392, #4147, #75278, #55889, #74872, #35722, #23917, #43253, #80367, #74036, #29405, #11300, #55064, #36959, #42848, #16383, #17215, #42029, #47926, #80772, #23087, #48754, #30646, #29812, #74453, #67309, #56311, #73631, #42436, #9644, #35313, #10881, #68136, #10481, #28990, #55473, #60975, #54656, #22680, #48339, #67723, #23500, #36542, #62218, #45326, #44084, #25552, #25141, #51219, #5386, #6620, #31047, #69778, #32291, #76916, #63865, #57951, #18840, #19664, #7042, #38190, #70177, #6202, #58377, #12529, #76098, #31880, #64702, #49993, #32711, #56717, #50401, #37780, #51631, #63456, #25972, #19245, #18442, #44896, #12122, #24323, #5791, #31461, #57123, #319, #57540, #82817, #18031, #71021, #13365, #50810, #77335, #39018, #70595, #76511, #44485, #82414, #83231, #75690, #43665, #69367, #11721, #37377, #12949, #38607, #63047, #24733, #64285, #1985, #1576, #27648, #65131, #66377, #7466, #20512, #8714, #53310, #40282, #34385, #78603, #79429, #66801, #14627, #46582, #65964, #34807, #72280, #52473, #8300 ) ),
 .UNSPECIFIED., .F., .F., .F. ) 
 B_SPLINE_SURFACE_WITH_KNOTS ( ( 2, 2 ),
 ( 3, 2, 2, 2, 2, 2, 2, 2, 2, 2, 2, 2, 2, 2, 2, 2, 2, 2, 2, 2, 2, 2, 2, 2, 2, 2, 2, 2, 2, 2, 2, 2, 2, 2, 2, 2, 2, 2, 2, 2, 2, 2, 2, 2, 2, 2, 2, 2, 2, 2, 2, 2, 2, 2, 2, 2, 2, 2, 2, 2, 2, 2, 2, 2, 2, 2, 2, 2, 2, 2, 2, 2, 2, 2, 2, 2, 2, 2, 2, 2, 2, 2, 2, 2, 2, 2, 2, 2, 2, 2, 2, 2, 2, 2, 2, 2, 2, 2, 2, 2, 2, 2, 2, 2, 2, 2, 2, 2, 2, 2, 2, 2, 2, 2, 2, 2, 2, 2, 2, 2, 2, 2, 2, 2, 2, 2, 2, 2, 2, 2, 2, 2, 2, 2, 2, 2, 2, 2, 2, 2, 2, 2, 2, 2, 2, 2, 2, 2, 2, 2, 2, 2, 2, 2, 2, 2, 2, 2, 2, 2, 2, 2, 2, 2, 2, 2, 2, 2, 2, 2, 2, 2, 2, 2, 2, 2, 2, 2, 2, 2, 2, 2, 2, 2, 2, 2, 2, 2, 2, 2, 2, 2, 2, 2, 2, 2, 2, 2, 2, 2, 2, 2, 2, 2, 2, 2, 2, 2, 2, 2, 2, 2, 2, 2, 2, 2, 2, 2, 2, 2, 2, 2, 2, 2, 2, 2, 2, 2, 2, 2, 2, 2, 2, 2, 2, 2, 2, 2, 2, 2, 2, 2, 2, 2, 2, 2, 2, 2, 2, 2, 2, 2, 2, 2, 2, 3 ),
 ( 0.000000000000000000, 1.000000000000000000 ),
 ( 0.000000000000000000, 0.003787878787878787984, 0.007575757575757575968, 0.01136363636363636395, 0.01515151515151515194, 0.01893939393939393992, 0.02272727272727272790, 0.02651515151515151589, 0.03030303030303030387, 0.03409090909090908839, 0.03787878787878787984, 0.04166666666666666435, 0.04545454545454545581, 0.04924242424242424032, 0.05303030303030303177, 0.05681818181818181629, 0.06060606060606060774, 0.06439393939393939226, 0.06818181818181817677, 0.07196969696969697516, 0.07575757575757575968, 0.07954545454545454419, 0.08333333333333332871, 0.08712121212121212710, 0.09090909090909091161, 0.09469696969696969613, 0.09848484848484848064, 0.1022727272727272790, 0.1060606060606060635, 0.1098484848484848481, 0.1136363636363636326, 0.1174242424242424310, 0.1212121212121212155, 0.1250000000000000000, 0.1287878787878787845, 0.1325757575757575690, 0.1363636363636363535, 0.1401515151515151381, 0.1439393939393939503, 0.1477272727272727348, 0.1515151515151515194, 0.1553030303030303039, 0.1590909090909090884, 0.1628787878787878729, 0.1666666666666666574, 0.1704545454545454419, 0.1742424242424242542, 0.1780303030303030387, 0.1818181818181818232, 0.1856060606060606077, 0.1893939393939393923, 0.1931818181818181768, 0.1969696969696969613, 0.2007575757575757458, 0.2045454545454545581, 0.2083333333333333426, 0.2121212121212121271, 0.2159090909090909116, 0.2196969696969696961, 0.2234848484848484806, 0.2272727272727272652, 0.2310606060606060497, 0.2348484848484848619, 0.2386363636363636465, 0.2424242424242424310, 0.2462121212121212155, 0.2500000000000000000, 0.2537878787878787845, 0.2575757575757575690, 0.2613636363636363535, 0.2651515151515151381, 0.2689393939393939226, 0.2727272727272727071, 0.2765151515151514916, 0.2803030303030302761, 0.2840909090909091161, 0.2878787878787879007, 0.2916666666666666852, 0.2954545454545454697, 0.2992424242424242542, 0.3030303030303030387, 0.3068181818181818232, 0.3106060606060606077, 0.3143939393939393923, 0.3181818181818181768, 0.3219696969696969613, 0.3257575757575757458, 0.3295454545454545303, 0.3333333333333333148, 0.3371212121212120993, 0.3409090909090908839, 0.3446969696969697239, 0.3484848484848485084, 0.3522727272727272929, 0.3560606060606060774, 0.3598484848484848619, 0.3636363636363636465, 0.3674242424242424310, 0.3712121212121212155, 0.3750000000000000000, 0.3787878787878787845, 0.3825757575757575690, 0.3863636363636363535, 0.3901515151515151381, 0.3939393939393939226, 0.3977272727272727071, 0.4015151515151514916, 0.4053030303030302761, 0.4090909090909091161, 0.4128787878787879007, 0.4166666666666666852, 0.4204545454545454697, 0.4242424242424242542, 0.4280303030303030387, 0.4318181818181818232, 0.4356060606060606077, 0.4393939393939393923, 0.4431818181818181768, 0.4469696969696969613, 0.4507575757575757458, 0.4545454545454545303, 0.4583333333333333148, 0.4621212121212120993, 0.4659090909090908839, 0.4696969696969697239, 0.4734848484848485084, 0.4772727272727272929, 0.4810606060606060774, 0.4848484848484848619, 0.4886363636363636465, 0.4924242424242424310, 0.4962121212121212155, 0.5000000000000000000, 0.5037878787878787845, 0.5075757575757575690, 0.5113636363636363535, 0.5151515151515151381, 0.5189393939393939226, 0.5227272727272727071, 0.5265151515151514916, 0.5303030303030302761, 0.5340909090909090606, 0.5378787878787878451, 0.5416666666666666297, 0.5454545454545454142, 0.5492424242424241987, 0.5530303030303029832, 0.5568181818181817677, 0.5606060606060605522, 0.5643939393939394478, 0.5681818181818182323, 0.5719696969696970168, 0.5757575757575758013, 0.5795454545454545858, 0.5833333333333333703, 0.5871212121212121549, 0.5909090909090909394, 0.5946969696969697239, 0.5984848484848485084, 0.6022727272727272929, 0.6060606060606060774, 0.6098484848484848619, 0.6136363636363636465, 0.6174242424242424310, 0.6212121212121212155, 0.6250000000000000000, 0.6287878787878787845, 0.6325757575757575690, 0.6363636363636363535, 0.6401515151515151381, 0.6439393939393939226, 0.6477272727272727071, 0.6515151515151514916, 0.6553030303030302761, 0.6590909090909090606, 0.6628787878787878451, 0.6666666666666666297, 0.6704545454545454142, 0.6742424242424241987, 0.6780303030303029832, 0.6818181818181817677, 0.6856060606060605522, 0.6893939393939394478, 0.6931818181818182323, 0.6969696969696970168, 0.7007575757575758013, 0.7045454545454545858, 0.7083333333333333703, 0.7121212121212121549, 0.7159090909090909394, 0.7196969696969697239, 0.7234848484848485084, 0.7272727272727272929, 0.7310606060606060774, 0.7348484848484848619, 0.7386363636363636465, 0.7424242424242424310, 0.7462121212121212155, 0.7500000000000000000, 0.7537878787878787845, 0.7575757575757575690, 0.7613636363636363535, 0.7651515151515151381, 0.7689393939393939226, 0.7727272727272727071, 0.7765151515151514916, 0.7803030303030302761, 0.7840909090909090606, 0.7878787878787878451, 0.7916666666666666297, 0.7954545454545454142, 0.7992424242424241987, 0.8030303030303029832, 0.8068181818181817677, 0.8106060606060605522, 0.8143939393939394478, 0.8181818181818182323, 0.8219696969696970168, 0.8257575757575758013, 0.8295454545454545858, 0.8333333333333333703, 0.8371212121212121549, 0.8409090909090909394, 0.8446969696969697239, 0.8484848484848485084, 0.8522727272727272929, 0.8560606060606060774, 0.8598484848484848619, 0.8636363636363636465, 0.8674242424242424310, 0.8712121212121212155, 0.8750000000000000000, 0.8787878787878787845, 0.8825757575757575690, 0.8863636363636363535, 0.8901515151515151381, 0.8939393939393939226, 0.8977272727272727071, 0.9015151515151514916, 0.9053030303030302761, 0.9090909090909090606, 0.9128787878787878451, 0.9166666666666666297, 0.9204545454545454142, 0.9242424242424241987, 0.9280303030303029832, 0.9318181818181817677, 0.9356060606060605522, 0.9393939393939394478, 0.9431818181818182323, 0.9469696969696970168, 0.9507575757575758013, 0.9545454545454545858, 0.9583333333333333703, 0.9621212121212121549, 0.9659090909090909394 ),
 .UNSPECIFIED. ) 
 GEOMETRIC_REPRESENTATION_ITEM ( )  RATIONAL_B_SPLINE_SURFACE ( (
 ( 1.000000000000000000, 0.9659258262890683122, 1.000000000000000000, 0.9659258262890683122, 1.000000000000000000, 0.9659258262890683122, 1.000000000000000000, 0.9659258262890683122, 1.000000000000000000, 0.9659258262890683122, 1.000000000000000000, 0.9659258262890683122, 1.000000000000000000, 0.9659258262890683122, 1.000000000000000000, 0.9659258262890683122, 1.000000000000000000, 0.9659258262890683122, 1.000000000000000000, 0.9659258262890683122, 1.000000000000000000, 0.9659258262890683122, 1.000000000000000000, 0.9659258262890683122, 1.000000000000000000, 0.9659258262890683122, 1.000000000000000000, 0.9659258262890683122, 1.000000000000000000, 0.9659258262890683122, 1.000000000000000000, 0.9659258262890683122, 1.000000000000000000, 0.9659258262890683122, 1.000000000000000000, 0.9659258262890683122, 1.000000000000000000, 0.9659258262890683122, 1.000000000000000000, 0.9659258262890683122, 1.000000000000000000, 0.9659258262890683122, 1.000000000000000000, 0.9659258262890683122, 1.000000000000000000, 0.9659258262890683122, 1.000000000000000000, 0.9659258262890683122, 1.000000000000000000, 0.9659258262890683122, 1.000000000000000000, 0.9659258262890683122, 1.000000000000000000, 0.9659258262890683122, 1.000000000000000000, 0.9659258262890683122, 1.000000000000000000, 0.9659258262890683122, 1.000000000000000000, 0.9659258262890683122, 1.000000000000000000, 0.9659258262890683122, 1.000000000000000000, 0.9659258262890683122, 1.000000000000000000, 0.9659258262890683122, 1.000000000000000000, 0.9659258262890683122, 1.000000000000000000, 0.9659258262890683122, 1.000000000000000000, 0.9659258262890683122, 1.000000000000000000, 0.9659258262890683122, 1.000000000000000000, 0.9659258262890683122, 1.000000000000000000, 0.9659258262890683122, 1.000000000000000000, 0.9659258262890683122, 1.000000000000000000, 0.9659258262890683122, 1.000000000000000000, 0.9659258262890683122, 1.000000000000000000, 0.9659258262890683122, 1.000000000000000000, 0.9659258262890683122, 1.000000000000000000, 0.9659258262890683122, 1.000000000000000000, 0.9659258262890683122, 1.000000000000000000, 0.9659258262890683122, 1.000000000000000000, 0.9659258262890683122, 1.000000000000000000, 0.9659258262890683122, 1.000000000000000000, 0.9659258262890683122, 1.000000000000000000, 0.9659258262890683122, 1.000000000000000000, 0.9659258262890683122, 1.000000000000000000, 0.9659258262890683122, 1.000000000000000000, 0.9659258262890683122, 1.000000000000000000, 0.9659258262890683122, 1.000000000000000000, 0.9659258262890683122, 1.000000000000000000, 0.9659258262890683122, 1.000000000000000000, 0.9659258262890683122, 1.000000000000000000, 0.9659258262890683122, 1.000000000000000000, 0.9659258262890683122, 1.000000000000000000, 0.9659258262890683122, 1.000000000000000000, 0.9659258262890683122, 1.000000000000000000, 0.9659258262890683122, 1.000000000000000000, 0.9659258262890683122, 1.000000000000000000, 0.9659258262890683122, 1.000000000000000000, 0.9659258262890683122, 1.000000000000000000, 0.9659258262890683122, 1.000000000000000000, 0.9659258262890683122, 1.000000000000000000, 0.9659258262890683122, 1.000000000000000000, 0.9659258262890683122, 1.000000000000000000, 0.9659258262890683122, 1.000000000000000000, 0.9659258262890683122, 1.000000000000000000, 0.9659258262890683122, 1.000000000000000000, 0.9659258262890683122, 1.000000000000000000, 0.9659258262890683122, 1.000000000000000000, 0.9659258262890683122, 1.000000000000000000, 0.9659258262890683122, 1.000000000000000000, 0.9659258262890683122, 1.000000000000000000, 0.9659258262890683122, 1.000000000000000000, 0.9659258262890683122, 1.000000000000000000, 0.9659258262890683122, 1.000000000000000000, 0.9659258262890683122, 1.000000000000000000, 0.9659258262890683122, 1.000000000000000000, 0.9659258262890683122, 1.000000000000000000, 0.9659258262890683122, 1.000000000000000000, 0.9659258262890683122, 1.000000000000000000, 0.9659258262890683122, 1.000000000000000000, 0.9659258262890683122, 1.000000000000000000, 0.9659258262890683122, 1.000000000000000000, 0.9659258262890683122, 1.000000000000000000, 0.9659258262890683122, 1.000000000000000000, 0.9659258262890683122, 1.000000000000000000, 0.9659258262890683122, 1.000000000000000000, 0.9659258262890683122, 1.000000000000000000, 0.9659258262890683122, 1.000000000000000000, 0.9659258262890683122, 1.000000000000000000, 0.9659258262890683122, 1.000000000000000000, 0.9659258262890683122, 1.000000000000000000, 0.9659258262890683122, 1.000000000000000000, 0.9659258262890683122, 1.000000000000000000, 0.9659258262890683122, 1.000000000000000000, 0.9659258262890683122, 1.000000000000000000, 0.9659258262890683122, 1.000000000000000000, 0.9659258262890683122, 1.000000000000000000, 0.9659258262890683122, 1.000000000000000000, 0.9659258262890683122, 1.000000000000000000, 0.9659258262890683122, 1.000000000000000000, 0.9659258262890683122, 1.000000000000000000, 0.9659258262890683122, 1.000000000000000000, 0.9659258262890683122, 1.000000000000000000, 0.9659258262890683122, 1.000000000000000000, 0.9659258262890683122, 1.000000000000000000, 0.9659258262890683122, 1.000000000000000000, 0.9659258262890683122, 1.000000000000000000, 0.9659258262890683122, 1.000000000000000000, 0.9659258262890683122, 1.000000000000000000, 0.9659258262890683122, 1.000000000000000000, 0.9659258262890683122, 1.000000000000000000, 0.9659258262890683122, 1.000000000000000000, 0.9659258262890683122, 1.000000000000000000, 0.9659258262890683122, 1.000000000000000000, 0.9659258262890683122, 1.000000000000000000, 0.9659258262890683122, 1.000000000000000000, 0.9659258262890683122, 1.000000000000000000, 0.9659258262890683122, 1.000000000000000000, 0.9659258262890683122, 1.000000000000000000, 0.9659258262890683122, 1.000000000000000000, 0.9659258262890683122, 1.000000000000000000, 0.9659258262890683122, 1.000000000000000000, 0.9659258262890683122, 1.000000000000000000, 0.9659258262890683122, 1.000000000000000000, 0.9659258262890683122, 1.000000000000000000, 0.9659258262890683122, 1.000000000000000000, 0.9659258262890683122, 1.000000000000000000, 0.9659258262890683122, 1.000000000000000000, 0.9659258262890683122, 1.000000000000000000, 0.9659258262890683122, 1.000000000000000000, 0.9659258262890683122, 1.000000000000000000, 0.9659258262890683122, 1.000000000000000000, 0.9659258262890683122, 1.000000000000000000, 0.9659258262890683122, 1.000000000000000000, 0.9659258262890683122, 1.000000000000000000, 0.9659258262890683122, 1.000000000000000000, 0.9659258262890683122, 1.000000000000000000, 0.9659258262890683122, 1.000000000000000000, 0.9659258262890683122, 1.000000000000000000, 0.9659258262890683122, 1.000000000000000000, 0.9659258262890683122, 1.000000000000000000, 0.9659258262890683122, 1.000000000000000000, 0.9659258262890683122, 1.000000000000000000, 0.9659258262890683122, 1.000000000000000000, 0.9659258262890683122, 1.000000000000000000, 0.9659258262890683122, 1.000000000000000000, 0.9659258262890683122, 1.000000000000000000, 0.9659258262890683122, 1.000000000000000000, 0.9659258262890683122, 1.000000000000000000, 0.9659258262890683122, 1.000000000000000000, 0.9659258262890683122, 1.000000000000000000, 0.9659258262890683122, 1.000000000000000000, 0.9659258262890683122, 1.000000000000000000, 0.9659258262890683122, 1.000000000000000000, 0.9659258262890683122, 1.000000000000000000, 0.9659258262890683122, 1.000000000000000000, 0.9659258262890683122, 1.000000000000000000, 0.9659258262890683122, 1.000000000000000000, 0.9659258262890683122, 1.000000000000000000, 0.9659258262890683122, 1.000000000000000000, 0.9659258262890683122, 1.000000000000000000, 0.9659258262890683122, 1.000000000000000000, 0.9659258262890683122, 1.000000000000000000, 0.9659258262890683122, 1.000000000000000000, 0.9659258262890683122, 1.000000000000000000, 0.9659258262890683122, 1.000000000000000000, 0.9659258262890683122, 1.000000000000000000, 0.9659258262890683122, 1.000000000000000000, 0.9659258262890683122, 1.000000000000000000, 0.9659258262890683122, 1.000000000000000000, 0.9659258262890683122, 1.000000000000000000, 0.9659258262890683122, 1.000000000000000000, 0.9659258262890683122, 1.000000000000000000, 0.9659258262890683122, 1.000000000000000000, 0.9659258262890683122, 1.000000000000000000, 0.9659258262890683122, 1.000000000000000000, 0.9659258262890683122, 1.000000000000000000, 0.9659258262890683122, 1.000000000000000000, 0.9659258262890683122, 1.000000000000000000, 0.9659258262890683122, 1.000000000000000000, 0.9659258262890683122, 1.000000000000000000, 0.9659258262890683122, 1.000000000000000000, 0.9659258262890683122, 1.000000000000000000, 0.9659258262890683122, 1.000000000000000000, 0.9659258262890683122, 1.000000000000000000, 0.9659258262890683122, 1.000000000000000000, 0.9659258262890683122, 1.000000000000000000, 0.9659258262890683122, 1.000000000000000000, 0.9659258262890683122, 1.000000000000000000, 0.9659258262890683122, 1.000000000000000000, 0.9659258262890683122, 1.000000000000000000, 0.9659258262890683122, 1.000000000000000000, 0.9659258262890683122, 1.000000000000000000, 0.9659258262890683122, 1.000000000000000000, 0.9659258262890683122, 1.000000000000000000, 0.9659258262890683122, 1.000000000000000000, 0.9659258262890683122, 1.000000000000000000, 0.9659258262890683122, 1.000000000000000000, 0.9659258262890683122, 1.000000000000000000, 0.9659258262890683122, 1.000000000000000000, 0.9659258262890683122, 1.000000000000000000, 0.9659258262890683122, 1.000000000000000000, 0.9659258262890683122, 1.000000000000000000, 0.9659258262890683122, 1.000000000000000000, 0.9659258262890683122, 1.000000000000000000, 0.9659258262890683122, 1.000000000000000000, 0.9659258262890683122, 1.000000000000000000, 0.9659258262890683122, 1.000000000000000000, 0.9659258262890683122, 1.000000000000000000, 0.9659258262890683122, 1.000000000000000000, 0.9659258262890683122, 1.000000000000000000, 0.9659258262890683122, 1.000000000000000000, 0.9659258262890683122, 1.000000000000000000, 0.9659258262890683122, 1.000000000000000000, 0.9659258262890683122, 1.000000000000000000, 0.9659258262890683122, 1.000000000000000000, 0.9659258262890683122, 1.000000000000000000, 0.9659258262890683122, 1.000000000000000000, 0.9659258262890683122, 1.000000000000000000, 0.9659258262890683122, 1.000000000000000000, 0.9659258262890683122, 1.000000000000000000, 0.9659258262890683122, 1.000000000000000000, 0.9659258262890683122, 1.000000000000000000, 0.9659258262890683122, 1.000000000000000000, 0.9659258262890683122, 1.000000000000000000, 0.9659258262890683122, 1.000000000000000000, 0.9659258262890683122, 1.000000000000000000, 0.9659258262890683122, 1.000000000000000000, 0.9659258262890683122, 1.000000000000000000, 0.9659258262890683122, 1.000000000000000000, 0.9659258262890683122, 1.000000000000000000, 0.9659258262890683122, 1.000000000000000000, 0.9659258262890683122, 1.000000000000000000, 0.9659258262890683122, 1.000000000000000000, 0.9659258262890683122, 1.000000000000000000, 0.9659258262890683122, 1.000000000000000000, 0.9659258262890683122, 1.000000000000000000, 0.9659258262890683122, 1.000000000000000000, 0.9659258262890683122, 1.000000000000000000, 0.9659258262890683122, 1.000000000000000000, 0.9659258262890683122, 1.000000000000000000, 0.9659258262890683122, 1.000000000000000000, 0.9659258262890683122, 1.000000000000000000, 0.9659258262890683122, 1.000000000000000000, 0.9659258262890683122, 1.000000000000000000, 0.9659258262890683122, 1.000000000000000000, 0.9659258262890683122, 1.000000000000000000, 0.9659258262890683122, 1.000000000000000000),
 ( 1.000000000000000000, 0.9659258262890683122, 1.000000000000000000, 0.9659258262890683122, 1.000000000000000000, 0.9659258262890683122, 1.000000000000000000, 0.9659258262890683122, 1.000000000000000000, 0.9659258262890683122, 1.000000000000000000, 0.9659258262890683122, 1.000000000000000000, 0.9659258262890683122, 1.000000000000000000, 0.9659258262890683122, 1.000000000000000000, 0.9659258262890683122, 1.000000000000000000, 0.9659258262890683122, 1.000000000000000000, 0.9659258262890683122, 1.000000000000000000, 0.9659258262890683122, 1.000000000000000000, 0.9659258262890683122, 1.000000000000000000, 0.9659258262890683122, 1.000000000000000000, 0.9659258262890683122, 1.000000000000000000, 0.9659258262890683122, 1.000000000000000000, 0.9659258262890683122, 1.000000000000000000, 0.9659258262890683122, 1.000000000000000000, 0.9659258262890683122, 1.000000000000000000, 0.9659258262890683122, 1.000000000000000000, 0.9659258262890683122, 1.000000000000000000, 0.9659258262890683122, 1.000000000000000000, 0.9659258262890683122, 1.000000000000000000, 0.9659258262890683122, 1.000000000000000000, 0.9659258262890683122, 1.000000000000000000, 0.9659258262890683122, 1.000000000000000000, 0.9659258262890683122, 1.000000000000000000, 0.9659258262890683122, 1.000000000000000000, 0.9659258262890683122, 1.000000000000000000, 0.9659258262890683122, 1.000000000000000000, 0.9659258262890683122, 1.000000000000000000, 0.9659258262890683122, 1.000000000000000000, 0.9659258262890683122, 1.000000000000000000, 0.9659258262890683122, 1.000000000000000000, 0.9659258262890683122, 1.000000000000000000, 0.9659258262890683122, 1.000000000000000000, 0.9659258262890683122, 1.000000000000000000, 0.9659258262890683122, 1.000000000000000000, 0.9659258262890683122, 1.000000000000000000, 0.9659258262890683122, 1.000000000000000000, 0.9659258262890683122, 1.000000000000000000, 0.9659258262890683122, 1.000000000000000000, 0.9659258262890683122, 1.000000000000000000, 0.9659258262890683122, 1.000000000000000000, 0.9659258262890683122, 1.000000000000000000, 0.9659258262890683122, 1.000000000000000000, 0.9659258262890683122, 1.000000000000000000, 0.9659258262890683122, 1.000000000000000000, 0.9659258262890683122, 1.000000000000000000, 0.9659258262890683122, 1.000000000000000000, 0.9659258262890683122, 1.000000000000000000, 0.9659258262890683122, 1.000000000000000000, 0.9659258262890683122, 1.000000000000000000, 0.9659258262890683122, 1.000000000000000000, 0.9659258262890683122, 1.000000000000000000, 0.9659258262890683122, 1.000000000000000000, 0.9659258262890683122, 1.000000000000000000, 0.9659258262890683122, 1.000000000000000000, 0.9659258262890683122, 1.000000000000000000, 0.9659258262890683122, 1.000000000000000000, 0.9659258262890683122, 1.000000000000000000, 0.9659258262890683122, 1.000000000000000000, 0.9659258262890683122, 1.000000000000000000, 0.9659258262890683122, 1.000000000000000000, 0.9659258262890683122, 1.000000000000000000, 0.9659258262890683122, 1.000000000000000000, 0.9659258262890683122, 1.000000000000000000, 0.9659258262890683122, 1.000000000000000000, 0.9659258262890683122, 1.000000000000000000, 0.9659258262890683122, 1.000000000000000000, 0.9659258262890683122, 1.000000000000000000, 0.9659258262890683122, 1.000000000000000000, 0.9659258262890683122, 1.000000000000000000, 0.9659258262890683122, 1.000000000000000000, 0.9659258262890683122, 1.000000000000000000, 0.9659258262890683122, 1.000000000000000000, 0.9659258262890683122, 1.000000000000000000, 0.9659258262890683122, 1.000000000000000000, 0.9659258262890683122, 1.000000000000000000, 0.9659258262890683122, 1.000000000000000000, 0.9659258262890683122, 1.000000000000000000, 0.9659258262890683122, 1.000000000000000000, 0.9659258262890683122, 1.000000000000000000, 0.9659258262890683122, 1.000000000000000000, 0.9659258262890683122, 1.000000000000000000, 0.9659258262890683122, 1.000000000000000000, 0.9659258262890683122, 1.000000000000000000, 0.9659258262890683122, 1.000000000000000000, 0.9659258262890683122, 1.000000000000000000, 0.9659258262890683122, 1.000000000000000000, 0.9659258262890683122, 1.000000000000000000, 0.9659258262890683122, 1.000000000000000000, 0.9659258262890683122, 1.000000000000000000, 0.9659258262890683122, 1.000000000000000000, 0.9659258262890683122, 1.000000000000000000, 0.9659258262890683122, 1.000000000000000000, 0.9659258262890683122, 1.000000000000000000, 0.9659258262890683122, 1.000000000000000000, 0.9659258262890683122, 1.000000000000000000, 0.9659258262890683122, 1.000000000000000000, 0.9659258262890683122, 1.000000000000000000, 0.9659258262890683122, 1.000000000000000000, 0.9659258262890683122, 1.000000000000000000, 0.9659258262890683122, 1.000000000000000000, 0.9659258262890683122, 1.000000000000000000, 0.9659258262890683122, 1.000000000000000000, 0.9659258262890683122, 1.000000000000000000, 0.9659258262890683122, 1.000000000000000000, 0.9659258262890683122, 1.000000000000000000, 0.9659258262890683122, 1.000000000000000000, 0.9659258262890683122, 1.000000000000000000, 0.9659258262890683122, 1.000000000000000000, 0.9659258262890683122, 1.000000000000000000, 0.9659258262890683122, 1.000000000000000000, 0.9659258262890683122, 1.000000000000000000, 0.9659258262890683122, 1.000000000000000000, 0.9659258262890683122, 1.000000000000000000, 0.9659258262890683122, 1.000000000000000000, 0.9659258262890683122, 1.000000000000000000, 0.9659258262890683122, 1.000000000000000000, 0.9659258262890683122, 1.000000000000000000, 0.9659258262890683122, 1.000000000000000000, 0.9659258262890683122, 1.000000000000000000, 0.9659258262890683122, 1.000000000000000000, 0.9659258262890683122, 1.000000000000000000, 0.9659258262890683122, 1.000000000000000000, 0.9659258262890683122, 1.000000000000000000, 0.9659258262890683122, 1.000000000000000000, 0.9659258262890683122, 1.000000000000000000, 0.9659258262890683122, 1.000000000000000000, 0.9659258262890683122, 1.000000000000000000, 0.9659258262890683122, 1.000000000000000000, 0.9659258262890683122, 1.000000000000000000, 0.9659258262890683122, 1.000000000000000000, 0.9659258262890683122, 1.000000000000000000, 0.9659258262890683122, 1.000000000000000000, 0.9659258262890683122, 1.000000000000000000, 0.9659258262890683122, 1.000000000000000000, 0.9659258262890683122, 1.000000000000000000, 0.9659258262890683122, 1.000000000000000000, 0.9659258262890683122, 1.000000000000000000, 0.9659258262890683122, 1.000000000000000000, 0.9659258262890683122, 1.000000000000000000, 0.9659258262890683122, 1.000000000000000000, 0.9659258262890683122, 1.000000000000000000, 0.9659258262890683122, 1.000000000000000000, 0.9659258262890683122, 1.000000000000000000, 0.9659258262890683122, 1.000000000000000000, 0.9659258262890683122, 1.000000000000000000, 0.9659258262890683122, 1.000000000000000000, 0.9659258262890683122, 1.000000000000000000, 0.9659258262890683122, 1.000000000000000000, 0.9659258262890683122, 1.000000000000000000, 0.9659258262890683122, 1.000000000000000000, 0.9659258262890683122, 1.000000000000000000, 0.9659258262890683122, 1.000000000000000000, 0.9659258262890683122, 1.000000000000000000, 0.9659258262890683122, 1.000000000000000000, 0.9659258262890683122, 1.000000000000000000, 0.9659258262890683122, 1.000000000000000000, 0.9659258262890683122, 1.000000000000000000, 0.9659258262890683122, 1.000000000000000000, 0.9659258262890683122, 1.000000000000000000, 0.9659258262890683122, 1.000000000000000000, 0.9659258262890683122, 1.000000000000000000, 0.9659258262890683122, 1.000000000000000000, 0.9659258262890683122, 1.000000000000000000, 0.9659258262890683122, 1.000000000000000000, 0.9659258262890683122, 1.000000000000000000, 0.9659258262890683122, 1.000000000000000000, 0.9659258262890683122, 1.000000000000000000, 0.9659258262890683122, 1.000000000000000000, 0.9659258262890683122, 1.000000000000000000, 0.9659258262890683122, 1.000000000000000000, 0.9659258262890683122, 1.000000000000000000, 0.9659258262890683122, 1.000000000000000000, 0.9659258262890683122, 1.000000000000000000, 0.9659258262890683122, 1.000000000000000000, 0.9659258262890683122, 1.000000000000000000, 0.9659258262890683122, 1.000000000000000000, 0.9659258262890683122, 1.000000000000000000, 0.9659258262890683122, 1.000000000000000000, 0.9659258262890683122, 1.000000000000000000, 0.9659258262890683122, 1.000000000000000000, 0.9659258262890683122, 1.000000000000000000, 0.9659258262890683122, 1.000000000000000000, 0.9659258262890683122, 1.000000000000000000, 0.9659258262890683122, 1.000000000000000000, 0.9659258262890683122, 1.000000000000000000, 0.9659258262890683122, 1.000000000000000000, 0.9659258262890683122, 1.000000000000000000, 0.9659258262890683122, 1.000000000000000000, 0.9659258262890683122, 1.000000000000000000, 0.9659258262890683122, 1.000000000000000000, 0.9659258262890683122, 1.000000000000000000, 0.9659258262890683122, 1.000000000000000000, 0.9659258262890683122, 1.000000000000000000, 0.9659258262890683122, 1.000000000000000000, 0.9659258262890683122, 1.000000000000000000, 0.9659258262890683122, 1.000000000000000000, 0.9659258262890683122, 1.000000000000000000, 0.9659258262890683122, 1.000000000000000000, 0.9659258262890683122, 1.000000000000000000, 0.9659258262890683122, 1.000000000000000000, 0.9659258262890683122, 1.000000000000000000, 0.9659258262890683122, 1.000000000000000000, 0.9659258262890683122, 1.000000000000000000, 0.9659258262890683122, 1.000000000000000000, 0.9659258262890683122, 1.000000000000000000, 0.9659258262890683122, 1.000000000000000000, 0.9659258262890683122, 1.000000000000000000, 0.9659258262890683122, 1.000000000000000000, 0.9659258262890683122, 1.000000000000000000, 0.9659258262890683122, 1.000000000000000000, 0.9659258262890683122, 1.000000000000000000, 0.9659258262890683122, 1.000000000000000000, 0.9659258262890683122, 1.000000000000000000, 0.9659258262890683122, 1.000000000000000000, 0.9659258262890683122, 1.000000000000000000, 0.9659258262890683122, 1.000000000000000000, 0.9659258262890683122, 1.000000000000000000, 0.9659258262890683122, 1.000000000000000000, 0.9659258262890683122, 1.000000000000000000, 0.9659258262890683122, 1.000000000000000000, 0.9659258262890683122, 1.000000000000000000, 0.9659258262890683122, 1.000000000000000000, 0.9659258262890683122, 1.000000000000000000, 0.9659258262890683122, 1.000000000000000000, 0.9659258262890683122, 1.000000000000000000, 0.9659258262890683122, 1.000000000000000000, 0.9659258262890683122, 1.000000000000000000, 0.9659258262890683122, 1.000000000000000000, 0.9659258262890683122, 1.000000000000000000, 0.9659258262890683122, 1.000000000000000000, 0.9659258262890683122, 1.000000000000000000, 0.9659258262890683122, 1.000000000000000000, 0.9659258262890683122, 1.000000000000000000, 0.9659258262890683122, 1.000000000000000000, 0.9659258262890683122, 1.000000000000000000, 0.9659258262890683122, 1.000000000000000000, 0.9659258262890683122, 1.000000000000000000, 0.9659258262890683122, 1.000000000000000000, 0.9659258262890683122, 1.000000000000000000, 0.9659258262890683122, 1.000000000000000000, 0.9659258262890683122, 1.000000000000000000, 0.9659258262890683122, 1.000000000000000000, 0.9659258262890683122, 1.000000000000000000, 0.9659258262890683122, 1.000000000000000000, 0.9659258262890683122, 1.000000000000000000, 0.9659258262890683122, 1.000000000000000000, 0.9659258262890683122, 1.000000000000000000, 0.9659258262890683122, 1.000000000000000000, 0.9659258262890683122, 1.000000000000000000, 0.9659258262890683122, 1.000000000000000000, 0.9659258262890683122, 1.000000000000000000) ) ) 
 REPRESENTATION_ITEM ( '' )  SURFACE ( )  );
#73444 = DIRECTION ( 'NONE',  ( -5.329070518200751394E-15, 0.000000000000000000, -1.000000000000000000 ) ) ;
#73445 = CARTESIAN_POINT ( 'NONE',  ( 0.4724409448818898682, 2.892866454678787531E-17, -1.612204724409448842 ) ) ;
#73446 = CARTESIAN_POINT ( 'NONE',  ( -0.7874015748031489847, -0.1870078740157479769, 0.4822834645669291653 ) ) ;
#73447 = CARTESIAN_POINT ( 'NONE',  ( -0.1246719160104980823, 0.1771653543307087630, 0.09757992244046791164 ) ) ;
#73448 = CARTESIAN_POINT ( 'NONE',  ( -1.541994750656167090, -0.6692913385826773087, -0.1292274648535924053 ) ) ;
#73449 = CARTESIAN_POINT ( 'NONE',  ( 0.03280839895013198948, -0.6692913385826773087, -0.1292274648535924053 ) ) ;
#73450 = CARTESIAN_POINT ( 'NONE',  ( 0.4986876640419954376, -0.5023911411419708095, -0.1820866141732282451 ) ) ;
#73451 = CARTESIAN_POINT ( 'NONE',  ( -0.7611548556430438595, 0.1283753931104748280, 0.1820866141732283561 ) ) ;
#73452 = CARTESIAN_POINT ( 'NONE',  ( -1.220472440944881054, 0.2952755905511811885, 0.000000000000000000 ) ) ;
#73453 = CARTESIAN_POINT ( 'NONE',  ( 1.574803149606299746, -0.1870078740157479769, 0.3641732283464567677 ) ) ;
#73454 = CARTESIAN_POINT ( 'NONE',  ( 1.502624671916010790, -0.05778040916215522460, 0.4822834645669289988 ) ) ;
#73455 = CARTESIAN_POINT ( 'NONE',  ( 0.2240801135442004322, 1.118954560528815589, 1.901799418834396738 ) ) ;
#73456 = CARTESIAN_POINT ( 'NONE',  ( 0.6824146981627303710, -0.5023911411419708095, 0.1820866141732285504 ) ) ;
#73457 = CARTESIAN_POINT ( 'NONE',  ( 0.7020997375328090762, -0.3162353388693405765, 0.4822834645669290543 ) ) ;
#73458 = DIRECTION ( 'NONE',  ( 8.659560562354908206E-17, -0.7071067811865496822, 0.7071067811865454633 ) ) ;
#73459 = CARTESIAN_POINT ( 'NONE',  ( 1.522309711286089939, -0.5023911411419708095, -0.1820866141732282451 ) ) ;
#73460 = VERTEX_POINT ( 'NONE', #69299 ) ;
#73461 = CARTESIAN_POINT ( 'NONE',  ( -0.7939632545931750718, -0.05778040916215560624, -0.4822834645669293319 ) ) ;
#73462 = CARTESIAN_POINT ( 'NONE',  ( -0.1998031496062991630, -0.3460692066303959202, -2.819553805774277944 ) ) ;
#73463 = CARTESIAN_POINT ( 'NONE',  ( -1.371391076115484609, -0.5511811023622046335, 0.09757992244046803654 ) ) ;
#73464 = CARTESIAN_POINT ( 'NONE',  ( -0.6167979002624665030, -0.4281496062992127816, -0.4176697321401328100 ) ) ;
#73465 = CARTESIAN_POINT ( 'NONE',  ( 0.3215223097112867578, -0.05778040916215522460, 0.4822834645669289988 ) ) ;
#73466 = VECTOR ( 'NONE', #23410, 39.37007874015748143 ) ;
#73467 = CARTESIAN_POINT ( 'NONE',  ( -1.692913385826770645, 0.1771653543307087630, 0.000000000000000000 ) ) ;
#73468 = CARTESIAN_POINT ( 'NONE',  ( 0.2925321140481932369, 0.2925321140481932369, -2.104330708661417582 ) ) ;
#73469 = CARTESIAN_POINT ( 'NONE',  ( -1.377952755905511140, 0.2952755905511811885, 0.000000000000000000 ) ) ;
#73470 = VECTOR ( 'NONE', #2164, 39.37007874015748143 ) ;
#73471 = VECTOR ( 'NONE', #58695, 39.37007874015748143 ) ;
#73472 = CARTESIAN_POINT ( 'NONE',  ( 0.3477690288713918276, -0.6692913385826773087, -0.1292274648535924053 ) ) ;
#73473 = CARTESIAN_POINT ( 'NONE',  ( -0.1377952755905504645, -0.5400638737290845981, -0.3530559997133363437 ) ) ;
#73474 = CARTESIAN_POINT ( 'NONE',  ( 1.049868766404200127, -0.6046776061558809534, -0.2411417322834644161 ) ) ;
#73475 = CARTESIAN_POINT ( 'NONE',  ( 1.646981627296588035, -0.3162353388693405765, 0.4822834645669290543 ) ) ;
#73476 = CARTESIAN_POINT ( 'NONE',  ( 0.3996062992125986035, 0.1070741851644054776, -1.699475065616798064 ) ) ;
#73477 = CARTESIAN_POINT ( 'NONE',  ( 0.3420746716998660508, -0.1974969037888703871, -1.207349081364829324 ) ) ;
#73478 = CARTESIAN_POINT ( 'NONE',  ( 0.1070741851644054915, -0.3996062992125986035, -2.447506561679789527 ) ) ;
#73479 = CARTESIAN_POINT ( 'NONE',  ( -0.4724409448818898682, -8.678599364036362592E-17, -0.6692913385826770867 ) ) ;
#73480 = CARTESIAN_POINT ( 'NONE',  ( 0.1049643490035304799, -0.3917322834645669549, -0.07742782152230966164 ) ) ;
#73481 = CARTESIAN_POINT ( 'NONE',  ( -0.2034120734908131112, -0.5511811023622048555, -0.09757992244046775898 ) ) ;
#73482 = CARTESIAN_POINT ( 'NONE',  ( -0.1706036745406816491, -0.4281496062992124485, 0.4176697321401328655 ) ) ;
#73483 = CARTESIAN_POINT ( 'NONE',  ( 0.9908136482939640111, 0.2952755905511810774, -0.1292274648535930714 ) ) ;
#73484 = CARTESIAN_POINT ( 'NONE',  ( -0.3949938075777411073, 0.1058382717557497660, -2.156824146981627610 ) ) ;
#73485 = CARTESIAN_POINT ( 'NONE',  ( -0.09186351706036663400, -0.3690944881889763329, 0.3153832671262228327 ) ) ;
#73486 = CARTESIAN_POINT ( 'NONE',  ( -1.030183727034119867, -0.3162353388693405765, 0.4822834645669290543 ) ) ;
#73487 = CARTESIAN_POINT ( 'NONE',  ( 1.089238845144357537, -0.4281496062992124485, 0.4176697321401328655 ) ) ;
#73488 = CARTESIAN_POINT ( 'NONE',  ( -0.4724409448818899238, 0.1265901696524986686, -1.922572178477689908 ) ) ;
#73489 = CARTESIAN_POINT ( 'NONE',  ( -0.06873123812452887338, -2.191421614605370878E-15, 0.4445507791589071167 ) ) ;
#73490 = AXIS2_PLACEMENT_3D ( 'NONE', #20602, #77850, #40780 ) ;
#73491 = ORIENTED_EDGE ( 'NONE', *, *, #60347, .T. ) ;
#73492 = EDGE_CURVE ( 'NONE', #41772, #76682, #28921, .T. ) ;
#73493 = ORIENTED_EDGE ( 'NONE', *, *, #66096, .F. ) ;
#73494 = CARTESIAN_POINT ( 'NONE',  ( 0.9251968503937015864, -0.5400638737290844871, 0.3530559997133364547 ) ) ;
#73495 = CARTESIAN_POINT ( 'NONE',  ( 1.469816272965879911, 0.1283753931104746893, -0.1820866141732285504 ) ) ;
#73497 = CARTESIAN_POINT ( 'NONE',  ( -1.017060367454067249, -0.05778040916215522460, 0.4822834645669289988 ) ) ;
#73496 = CARTESIAN_POINT ( 'NONE',  ( -1.023622047244093558, -0.1870078740157479769, 0.3641732283464567677 ) ) ;
#73498 = CARTESIAN_POINT ( 'NONE',  ( -0.1958661417322834497, -0.3392501089628018884, -2.822815329887452318 ) ) ;
#73499 = DIRECTION ( 'NONE',  ( -1.000000000000000000, -0.000000000000000000, -0.000000000000000000 ) ) ;
#73500 = CARTESIAN_POINT ( 'NONE',  ( 1.299212598425197429, -0.6692913385826771977, 8.415575281601705876E-17 ) ) ;
#73501 = CARTESIAN_POINT ( 'NONE',  ( 0.3458507752293908943, -0.3458507752293908943, -2.460629921259842146 ) ) ;
#73502 = CARTESIAN_POINT ( 'NONE',  ( -0.2034120734908131112, -0.6692913385826773087, -0.1292274648535924053 ) ) ;
#73503 = CARTESIAN_POINT ( 'NONE',  ( -0.5774278215223089816, 0.2306618581243847221, -0.2411417322834647770 ) ) ;
#73504 = CARTESIAN_POINT ( 'NONE',  ( -1.345144356955379816, -0.3162353388693405765, 0.4822834645669290543 ) ) ;
#73505 = CARTESIAN_POINT ( 'NONE',  ( 0.1049643490035304938, -0.3917322834645669549, -0.01246719160104995359 ) ) ;
#73506 = CARTESIAN_POINT ( 'NONE',  ( 0.1640419947506569498, -0.05778040916215522460, 0.4822834645669289988 ) ) ;
#73507 = CARTESIAN_POINT ( 'NONE',  ( 0.1049643490035303689, 0.3917322834645670104, -2.032808398950130879 ) ) ;
#73508 = CARTESIAN_POINT ( 'NONE',  ( -1.181102362204723644, -0.1870078740157479769, 0.3641732283464567677 ) ) ;
#73509 = ORIENTED_EDGE ( 'NONE', *, *, #51081, .F. ) ;
#73510 = CARTESIAN_POINT ( 'NONE',  ( 0.3949938075777411073, -0.1058382717557499464, -2.316272965879265122 ) ) ;
#73511 = ORIENTED_EDGE ( 'NONE', *, *, #11002, .F. ) ;
#73512 = CARTESIAN_POINT ( 'NONE',  ( 0.2460629921259842590, 0.000000000000000000, 0.1279527559055117503 ) ) ;
#73513 = CARTESIAN_POINT ( 'NONE',  ( -1.686351706036744558, 0.2952755905511810774, -0.1292274648535930714 ) ) ;
#73514 = CARTESIAN_POINT ( 'NONE',  ( -0.1998031496062994683, 0.3460692066303958092, -0.9580052493438320216 ) ) ;
#73515 = CARTESIAN_POINT ( 'NONE',  ( -1.614173228346456268, -0.6692913385826771977, 8.415575281601705876E-17 ) ) ;
#73516 = CARTESIAN_POINT ( 'NONE',  ( -0.9285414500055709786, 1.724409448818897905, 0.6299212598425196763 ) ) ;
#73517 = DIRECTION ( 'NONE',  ( 0.000000000000000000, 0.000000000000000000, 1.000000000000000000 ) ) ;
#73518 = CARTESIAN_POINT ( 'NONE',  ( -0.3412073490813641308, 0.2306618581243847221, -0.2411417322834647770 ) ) ;
#73519 = CARTESIAN_POINT ( 'NONE',  ( 0.3392501089628018329, 0.1958661417322835607, -0.05839895013123368173 ) ) ;
#73520 = CARTESIAN_POINT ( 'NONE',  ( -0.4461942257217840213, -0.5023911411419708095, -0.1820866141732282451 ) ) ;
#73521 = CARTESIAN_POINT ( 'NONE',  ( -0.9317585301837263412, -0.004921259842519576551, 0.3153832671262227771 ) ) ;
#73522 = CARTESIAN_POINT ( 'NONE',  ( -1.056430446194224881, -0.6692913385826771977, 0.1292274648535927661 ) ) ;
#73523 = CARTESIAN_POINT ( 'NONE',  ( 0.4330708661417329575, -0.6692913385826771977, 8.415575281601705876E-17 ) ) ;
#73524 = CARTESIAN_POINT ( 'NONE',  ( -0.7217847769028863381, -0.4281496062992124485, 0.4176697321401328655 ) ) ;
#73525 = CARTESIAN_POINT ( 'NONE',  ( 0.1958661417322834775, 0.3392501089628018884, 0.02099737532808403431 ) ) ;
#73526 = VERTEX_POINT ( 'NONE', #81940 ) ;
#73527 = CARTESIAN_POINT ( 'NONE',  ( -1.489501312335957062, -0.05778040916215522460, 0.4822834645669289988 ) ) ;
#73528 = FACE_OUTER_BOUND ( 'NONE', #29484, .T. ) ;
#73529 = SHAPE_REPRESENTATION_RELATIONSHIP ( 'NONE' , 'NONE' ,  #82043, #68561 ) ;
#73530 = AXIS2_PLACEMENT_3D ( 'NONE', #20873, #72226, #46941 ) ;
#73531 = CARTESIAN_POINT ( 'NONE',  ( -0.4724409448818898682, -8.678599364036362592E-17, -1.456692913385826849 ) ) ;
#73532 = CARTESIAN_POINT ( 'NONE',  ( 1.947231901457292969, 1.169463170161823440, -0.3010181502270611320 ) ) ;
#73533 = CARTESIAN_POINT ( 'NONE',  ( -9.594673741351313045E-17, 0.3917322834645670104, -0.7795275590551180578 ) ) ;
#73534 =( BOUNDED_CURVE ( )  B_SPLINE_CURVE ( 2, ( #33781, #59444, #34195, #13596, #79247, #20319, #77571, #21155, #14851, #39675, #39250, #977, #58609 ),
 .UNSPECIFIED., .F., .F. ) 
 B_SPLINE_CURVE_WITH_KNOTS ( ( 3, 2, 2, 2, 2, 2, 3 ),
 ( 0.5831241751160508580, 0.5833333333333333703, 0.5871212121212121549, 0.5909090909090909394, 0.5946969696969697239, 0.5984848484848485084, 0.5986940067021310208 ),
 .UNSPECIFIED. ) 
 CURVE ( )  GEOMETRIC_REPRESENTATION_ITEM ( )  RATIONAL_B_SPLINE_CURVE ( ( 0.9964447847208419695, 0.9981185001348091834, 1.000000000000000000, 0.9659258262890683122, 1.000000000000000000, 0.9659258262890683122, 1.000000000000000000, 0.9659258262890683122, 1.000000000000000000, 0.9659258262890683122, 1.000000000000000000, 0.9981185001348091834, 0.9964447847208420805 ) ) 
 REPRESENTATION_ITEM ( '' )  );
#73535 = CIRCLE ( 'NONE', #29116, 0.4724409448818898682 ) ;
#73536 = CARTESIAN_POINT ( 'NONE',  ( -0.3917322834645671215, 0.1049643490035301469, -2.322178477690288290 ) ) ;
#73537 = CARTESIAN_POINT ( 'NONE',  ( -0.5446194225721777693, -0.05778040916215522460, 0.4822834645669289988 ) ) ;
#73538 = CARTESIAN_POINT ( 'NONE',  ( 1.548556430446194954, 0.2306618581243847221, -0.2411417322834647770 ) ) ;
#73539 = CIRCLE ( 'NONE', #60059, 1.220472440944881942 ) ;
#73540 = CARTESIAN_POINT ( 'NONE',  ( 0.1998031496062992463, 0.3460692066303959202, -0.2211286089238845565 ) ) ;
#73542 = CYLINDRICAL_SURFACE ( 'NONE', #26401, 0.4921259842519685179 ) ;
#73541 = CARTESIAN_POINT ( 'NONE',  ( -0.7478466213799872531, 2.204724409448818978, -0.5309055118110235227 ) ) ;
#73543 = CARTESIAN_POINT ( 'NONE',  ( -1.227034120734907585, 0.2952755905511811885, 0.1292274648535926551 ) ) ;
#73544 = CARTESIAN_POINT ( 'NONE',  ( -0.8202099737532801971, -0.6692913385826771977, 0.1292274648535927661 ) ) ;
#73545 = CARTESIAN_POINT ( 'NONE',  ( 4.797336870675655290E-17, -0.3917322834645669549, -0.1587733351367961454 ) ) ;
#73546 = CARTESIAN_POINT ( 'NONE',  ( 0.3280839895013130669, -0.004921259842519576551, 0.3153832671262227771 ) ) ;
#73547 = CARTESIAN_POINT ( 'NONE',  ( 0.3917322834645670104, 2.398668435337828261E-17, -0.3602362204724410266 ) ) ;
#73548 = CARTESIAN_POINT ( 'NONE',  ( 0.2230971128608932319, -0.3690944881889763329, 0.3153832671262228327 ) ) ;
#73549 = CARTESIAN_POINT ( 'NONE',  ( 0.9448818897637802916, -0.1870078740157479769, 0.3641732283464567677 ) ) ;
#73550 = CARTESIAN_POINT ( 'NONE',  ( 0.8202099737532813073, 0.2952755905511811885, 0.1292274648535926551 ) ) ;
#73551 = CARTESIAN_POINT ( 'NONE',  ( -0.1771653543307080136, 0.07958543189024071263, -0.2665933059059888421 ) ) ;
#73552 = CARTESIAN_POINT ( 'NONE',  ( -0.3917322834645669549, -0.1049643490035306603, -2.400262467191600635 ) ) ;
#73553 = CARTESIAN_POINT ( 'NONE',  ( 1.404199475065617264, -0.4281496062992124485, 0.4176697321401328655 ) ) ;
#73554 = CARTESIAN_POINT ( 'NONE',  ( -1.207349081364828436, -0.5023911411419708095, 0.1820866141732285504 ) ) ;
#73555 = CARTESIAN_POINT ( 'NONE',  ( -0.2362204724409447953, -0.4091458600556404646, -0.4573490813648293796 ) ) ;
#73556 = CARTESIAN_POINT ( 'NONE',  ( -0.7677165354330699465, -0.4536011799217368745, -0.2665933059059886201 ) ) ;
#73557 = CARTESIAN_POINT ( 'NONE',  ( 0.08530183727034192087, -0.05778040916215522460, 0.4822834645669289988 ) ) ;
#73558 = CARTESIAN_POINT ( 'NONE',  ( 1.692913385826772421, 0.1771653543307087630, 0.000000000000000000 ) ) ;
#73559 = CARTESIAN_POINT ( 'NONE',  ( 0.6692913385826777528, 0.1771653543307087630, 0.000000000000000000 ) ) ;
#73560 = CARTESIAN_POINT ( 'NONE',  ( -0.1837270341207343505, -0.5023911411419708095, 0.1820866141732285504 ) ) ;
#73561 = CARTESIAN_POINT ( 'NONE',  ( -0.6561679790026240244, 0.2306618581243847221, -0.2411417322834647770 ) ) ;
#73562 = PLANE ( 'NONE',  #11639 ) ;
#73563 = CARTESIAN_POINT ( 'NONE',  ( -1.614173228346456712, 2.401574803149606474, 0.1372047244094477536 ) ) ;
#73564 = CARTESIAN_POINT ( 'NONE',  ( 0.3608923884514443348, -0.6692913385826771977, 0.1292274648535927661 ) ) ;
#73565 = CARTESIAN_POINT ( 'NONE',  ( -0.1998031496062991630, -0.3460692066303959202, -1.559711286089238591 ) ) ;
#73566 = CARTESIAN_POINT ( 'NONE',  ( 1.607611548556431069, 0.2952755905511811885, 0.1292274648535926551 ) ) ;
#73567 = CARTESIAN_POINT ( 'NONE',  ( -0.2362204724409442680, -0.1870078740157480601, -0.3641732283464567677 ) ) ;
#73568 = CARTESIAN_POINT ( 'NONE',  ( 0.01312335958005323398, 0.05413385826771666132, 0.4176697321401328100 ) ) ;
#73569 = CARTESIAN_POINT ( 'NONE',  ( -1.384514435695537005, -0.6692913385826773087, -0.1292274648535924053 ) ) ;
#73570 = CARTESIAN_POINT ( 'NONE',  ( 1.679790026246720025, 0.2306618581243848609, 0.2411417322834645549 ) ) ;
#73571 = CARTESIAN_POINT ( 'NONE',  ( 1.482939632545932307, -0.4281496062992124485, 0.4176697321401328655 ) ) ;
#73572 = CARTESIAN_POINT ( 'NONE',  ( -0.5643044619422565855, -0.004921259842519870586, -0.3153832671262229437 ) ) ;
#73573 = CARTESIAN_POINT ( 'NONE',  ( -0.2925321140481932369, 0.2925321140481930704, -0.2539370078740156855 ) ) ;
#73574 = CARTESIAN_POINT ( 'NONE',  ( -0.1998031496062991907, -0.3460692066303959757, -0.3805774278215223183 ) ) ;
#73575 = CARTESIAN_POINT ( 'NONE',  ( 0.1049643490035304799, -0.3917322834645670104, -2.759205667487876656 ) ) ;
#73576 = CARTESIAN_POINT ( 'NONE',  ( 1.502624671916010790, -0.08942795157527998196, 0.3641732283464567121 ) ) ;
#73577 = CARTESIAN_POINT ( 'NONE',  ( 1.213910761154856299, -0.5511811023622048555, -0.09757992244046775898 ) ) ;
#73578 = CARTESIAN_POINT ( 'NONE',  ( 3.937007874015748143, 1.537401574803149984, -0.4744094488188970171 ) ) ;
#73579 = CARTESIAN_POINT ( 'NONE',  ( 0.9842519685039375910, 0.2952755905511811885, 0.000000000000000000 ) ) ;
#73580 = CARTESIAN_POINT ( 'NONE',  ( -0.3420746716998660508, -0.1974969037888706924, -1.074146981627296826 ) ) ;
#73581 = CARTESIAN_POINT ( 'NONE',  ( 1.207349081364829990, 0.1283753931104748280, 0.1820866141732283561 ) ) ;
#73582 = ADVANCED_FACE ( 'NONE', ( #68068 ), #74385, .F. ) ;
#73583 = CARTESIAN_POINT ( 'NONE',  ( -0.07217847769028787330, -0.05778040916215522460, 0.4822834645669289988 ) ) ;
#73584 = CARTESIAN_POINT ( 'NONE',  ( -0.2952755905511803003, -0.5400638737290845981, -0.3530559997133363437 ) ) ;
#73585 = CARTESIAN_POINT ( 'NONE',  ( -3.910253683044872197, 1.664255196667159042, 0.4582455874901649184 ) ) ;
#73586 = CONICAL_SURFACE ( 'NONE', #74904, 0.09842519685039351207, 1.029744258676652091 ) ;
#73587 = CARTESIAN_POINT ( 'NONE',  ( 0.2362204724409451007, -0.4091458600556402980, -0.7217847769028871152 ) ) ;
#73588 = CONICAL_SURFACE ( 'NONE', #14474, 0.2755905511811031494, 0.7853981633974284060 ) ;
#73589 = DIRECTION ( 'NONE',  ( 0.000000000000000000, -0.000000000000000000, -1.000000000000000000 ) ) ;
#73590 = CARTESIAN_POINT ( 'NONE',  ( 0.5511811023622054106, -0.1870078740157480601, -0.3641732283464567677 ) ) ;
#73591 = ORIENTED_EDGE ( 'NONE', *, *, #4963, .T. ) ;
#73592 = CARTESIAN_POINT ( 'NONE',  ( 0.2867679344610366554, 0.2867679344610366554, -0.4494943813986370107 ) ) ;
#73593 = ORIENTED_EDGE ( 'NONE', *, *, #79585, .T. ) ;
#73594 = EDGE_CURVE ( 'NONE', #25136, #23894, #45097, .T. ) ;
#73595 = CARTESIAN_POINT ( 'NONE',  ( -0.3280839895013117347, -0.4281496062992124485, 0.4176697321401328655 ) ) ;
#73596 = CARTESIAN_POINT ( 'NONE',  ( 0.8661417322834652488, -0.1870078740157480879, -0.4822834645669291653 ) ) ;
#73597 = CARTESIAN_POINT ( 'NONE',  ( 0.2952755905511819101, 0.1660481256975883668, -0.3530559997133364547 ) ) ;
#73598 = CARTESIAN_POINT ( 'NONE',  ( -0.4265091863517051496, -0.5511811023622046335, 0.09757992244046803654 ) ) ;
#73599 = CARTESIAN_POINT ( 'NONE',  ( 0.9186351706036752773, 0.2306618581243847221, -0.2411417322834647770 ) ) ;
#73600 = CARTESIAN_POINT ( 'NONE',  ( -0.9580052493438311334, 0.05413385826771626580, -0.4176697321401330321 ) ) ;
#73601 = CARTESIAN_POINT ( 'NONE',  ( -0.3543307086614165824, -0.6692913385826771977, 8.415575281601705876E-17 ) ) ;
#73602 = CARTESIAN_POINT ( 'NONE',  ( -0.7217847769028863381, 0.05413385826771626580, -0.4176697321401330321 ) ) ;
#73603 = CARTESIAN_POINT ( 'NONE',  ( 1.384514435695538337, -0.6692913385826771977, 0.1292274648535927661 ) ) ;
#73604 = CARTESIAN_POINT ( 'NONE',  ( 0.8398950131233602345, 0.2306618581243847221, -0.2411417322834647770 ) ) ;
#73605 = CARTESIAN_POINT ( 'NONE',  ( 0.7283464566929143125, 0.1660481256975885056, 0.3530559997133364547 ) ) ;
#73606 = CARTESIAN_POINT ( 'NONE',  ( 0.1958661417322834775, 0.3392501089628018884, -0.4514435695538057125 ) ) ;
#73607 = CARTESIAN_POINT ( 'NONE',  ( 0.2165354330708668673, -0.4536011799217367080, 0.2665933059059888421 ) ) ;
#73608 = ORIENTED_EDGE ( 'NONE', *, *, #28505, .T. ) ;
#73609 = CARTESIAN_POINT ( 'NONE',  ( 0.2891555358219910499, 0.2891555358219910499, -0.9251968503937008093 ) ) ;
#73610 = ORIENTED_EDGE ( 'NONE', *, *, #38141, .F. ) ;
#73611 = CARTESIAN_POINT ( 'NONE',  ( -1.049868766404198794, 0.1283753931104746893, -0.1820866141732285504 ) ) ;
#73612 = CARTESIAN_POINT ( 'NONE',  ( -0.3412073490813641308, 0.2306618581243847221, -0.2411417322834647770 ) ) ;
#73613 = CARTESIAN_POINT ( 'NONE',  ( -1.436918669920151492, 1.161451126500848918, 0.2894072871544302039 ) ) ;
#73614 = CARTESIAN_POINT ( 'NONE',  ( -0.3215223097112853146, -0.3162353388693405765, 0.4822834645669290543 ) ) ;
#73615 = CARTESIAN_POINT ( 'NONE',  ( -0.5971128608923877978, 0.2952755905511811885, 0.1292274648535926551 ) ) ;
#73616 = CARTESIAN_POINT ( 'NONE',  ( -1.423884514435694859, -0.05778040916215560624, -0.4822834645669293319 ) ) ;
#73617 = CARTESIAN_POINT ( 'NONE',  ( -1.574803149606298636, -0.1870078740157479769, 0.4822834645669291653 ) ) ;
#73618 = CARTESIAN_POINT ( 'NONE',  ( 1.010498687664042716, -0.3690944881889763329, 0.3153832671262228327 ) ) ;
#73619 = CARTESIAN_POINT ( 'NONE',  ( 0.2362204724409451007, -0.4091458600556402980, -1.036745406824147064 ) ) ;
#73620 = FACE_OUTER_BOUND ( 'NONE', #76179, .T. ) ;
#73621 = CARTESIAN_POINT ( 'NONE',  ( 0.5839895013123367340, -0.5511811023622048555, -0.09757992244046775898 ) ) ;
#73622 = CARTESIAN_POINT ( 'NONE',  ( 0.1312335958005257930, 0.2306618581243847221, -0.2411417322834647770 ) ) ;
#73623 = CARTESIAN_POINT ( 'NONE',  ( 0.5380577427821529035, -0.4281496062992124485, 0.4176697321401328655 ) ) ;
#73624 = ORIENTED_EDGE ( 'NONE', *, *, #81513, .T. ) ;
#73625 = CARTESIAN_POINT ( 'NONE',  ( 0.1070741851644054915, -0.3996062992125986035, -1.502624671916010346 ) ) ;
#73626 = CYLINDRICAL_SURFACE ( 'NONE', #77548, 0.4744094488188972947 ) ;
#73627 = ORIENTED_EDGE ( 'NONE', *, *, #13177, .F. ) ;
#73628 = CARTESIAN_POINT ( 'NONE',  ( 0.3996062992125984925, 0.1070741851644054637, -1.146325459317585116 ) ) ;
#73629 = CARTESIAN_POINT ( 'NONE',  ( -0.1070741851644051862, -0.3996062992125986590, -0.6213910761154856077 ) ) ;
#73630 = CARTESIAN_POINT ( 'NONE',  ( -0.5380577427821514602, -0.3690944881889765550, -0.3153832671262227771 ) ) ;
#73631 = CARTESIAN_POINT ( 'NONE',  ( -1.069553805774277722, 0.2952755905511811885, 0.1292274648535926551 ) ) ;
#73632 = CARTESIAN_POINT ( 'NONE',  ( -0.3458507752293909498, 0.3458507752293907833, 0.1377952755905511861 ) ) ;
#73633 = CARTESIAN_POINT ( 'NONE',  ( 0.1958661417322834775, 0.3392501089628018884, -2.591207349081364519 ) ) ;
#73634 = CARTESIAN_POINT ( 'NONE',  ( -1.581364829396324945, -0.08942795157528024563, -0.3641732283464568787 ) ) ;
#73635 = CARTESIAN_POINT ( 'NONE',  ( 0.8858267716535438430, -0.5400638737290845981, -0.3530559997133363437 ) ) ;
#73636 = CARTESIAN_POINT ( 'NONE',  ( 0.3412073490813655186, -0.6046776061558809534, -0.2411417322834644161 ) ) ;
#73637 = CARTESIAN_POINT ( 'NONE',  ( -0.4921259842519677963, 0.07958543189024071263, -0.2665933059059888421 ) ) ;
#73638 = CARTESIAN_POINT ( 'NONE',  ( 0.03937007874015806264, 0.2952755905511811885, 0.000000000000000000 ) ) ;
#73639 = CARTESIAN_POINT ( 'NONE',  ( 0.2362204724409449064, 0.4091458600556404646, -2.110892388451443225 ) ) ;
#73640 = CARTESIAN_POINT ( 'NONE',  ( -0.1574803149606292529, -0.1870078740157480601, -0.3641732283464567677 ) ) ;
#73641 = CARTESIAN_POINT ( 'NONE',  ( -0.5708661417322828946, 0.1660481256975883668, -0.3530559997133364547 ) ) ;
#73642 = CARTESIAN_POINT ( 'NONE',  ( -0.1058382717557497660, -0.3949938075777411073, -1.723753280839894986 ) ) ;
#73643 = CARTESIAN_POINT ( 'NONE',  ( -1.706036745406823485, 0.2306618581243848609, 0.2411417322834645549 ) ) ;
#73644 = CARTESIAN_POINT ( 'NONE',  ( 0.2296587926509192634, -0.08942795157528024563, -0.3641732283464568787 ) ) ;
#73645 = CARTESIAN_POINT ( 'NONE',  ( 1.450131233595801428, -0.5511811023622048555, -0.09757992244046775898 ) ) ;
#73646 = CARTESIAN_POINT ( 'NONE',  ( -1.259842519685038686, -0.1870078740157479769, 0.4822834645669291653 ) ) ;
#73647 = CARTESIAN_POINT ( 'NONE',  ( -0.9055118110236215490, -0.5511811023622047445, 6.969142054262312111E-17 ) ) ;
#73648 = DIRECTION ( 'NONE',  ( 1.000000000000000000, -0.000000000000000000, -0.000000000000000000 ) ) ;
#73649 = CARTESIAN_POINT ( 'NONE',  ( -1.266404199475064773, -0.3162353388693405765, 0.4822834645669290543 ) ) ;
#73650 = CARTESIAN_POINT ( 'NONE',  ( -0.1115485564304453947, -0.6692913385826771977, 0.1292274648535927661 ) ) ;
#73651 = CARTESIAN_POINT ( 'NONE',  ( 0.3996062992125986035, -0.1070741851644052972, -2.393044619422572072 ) ) ;
#73653 = CARTESIAN_POINT ( 'NONE',  ( -0.3917322834645670659, 0.1049643490035301607, -2.317565986055430738 ) ) ;
#73652 = AXIS2_PLACEMENT_3D ( 'NONE', #82958, #40, #18571 ) ;
#73654 = CARTESIAN_POINT ( 'NONE',  ( 0.5314960629920858493, 2.755905511811024056, 3.831929248781932973 ) ) ;
#73655 = CARTESIAN_POINT ( 'NONE',  ( 0.4068241469816281097, -0.004921259842519576551, 0.3153832671262227771 ) ) ;
#73656 = CARTESIAN_POINT ( 'NONE',  ( 1.069553805774278610, -0.6692913385826771977, 0.1292274648535927661 ) ) ;
#73657 = CARTESIAN_POINT ( 'NONE',  ( -1.351706036745406347, -0.004921259842519870586, -0.3153832671262229437 ) ) ;
#73658 = CARTESIAN_POINT ( 'NONE',  ( 1.095800524934383846, -0.05778040916215560624, -0.4822834645669293319 ) ) ;
#73659 = CARTESIAN_POINT ( 'NONE',  ( -1.633858267716534529, -0.4536011799217368745, -0.2665933059059886201 ) ) ;
#73660 = EDGE_CURVE ( 'NONE', #73693, #22261, #10999, .T. ) ;
#73661 = CARTESIAN_POINT ( 'NONE',  ( -0.6036745406824141069, 0.2306618581243848609, 0.2411417322834645549 ) ) ;
#73662 = CARTESIAN_POINT ( 'NONE',  ( 0.1902887139107617975, -0.5511811023622048555, -0.09757992244046775898 ) ) ;
#73663 = CARTESIAN_POINT ( 'NONE',  ( 0.4724409448818898127, -0.1265901696524988629, -0.8989501312335956840 ) ) ;
#73664 = CARTESIAN_POINT ( 'NONE',  ( 0.4658792650918640033, -0.2845877964562159024, 0.3641732283464567677 ) ) ;
#73665 = CARTESIAN_POINT ( 'NONE',  ( 0.03280839895013198948, -0.6692913385826773087, -0.1292274648535924053 ) ) ;
#73666 = CARTESIAN_POINT ( 'NONE',  ( 0.1998031496062994128, -0.3460692066303957537, -0.3261154855643044748 ) ) ;
#73667 = CARTESIAN_POINT ( 'NONE',  ( -1.240157480314959759, 0.1660481256975885056, 0.3530559997133364547 ) ) ;
#73668 = CARTESIAN_POINT ( 'NONE',  ( 0.3392501089628018329, 0.1958661417322835607, -1.790682414698162805 ) ) ;
#73669 = CARTESIAN_POINT ( 'NONE',  ( 1.187664041994751285, -0.2845877964562161244, -0.3641732283464567121 ) ) ;
#73670 = CARTESIAN_POINT ( 'NONE',  ( -0.1246719160104980823, -0.6692913385826773087, -0.1292274648535924053 ) ) ;
#73671 = CARTESIAN_POINT ( 'NONE',  ( -0.2952755905511803003, -0.5400638737290845981, -0.3530559997133363437 ) ) ;
#73672 = CARTESIAN_POINT ( 'NONE',  ( -0.5708661417322825615, -0.4536011799217367080, 0.2665933059059888421 ) ) ;
#73673 = CARTESIAN_POINT ( 'NONE',  ( 1.194225721784777594, 0.05413385826771666132, 0.4176697321401328100 ) ) ;
#73674 = CARTESIAN_POINT ( 'NONE',  ( -0.4461942257217840213, -0.5023911411419708095, -0.1820866141732282451 ) ) ;
#73675 = CARTESIAN_POINT ( 'NONE',  ( 0.2362204724409456558, -0.1870078740157479769, 0.4822834645669291653 ) ) ;
#73676 = B_SPLINE_CURVE_WITH_KNOTS ( 'NONE', 3,
 ( #10863, #54639, #61373, #62199, #3723, #23898, #42829 ),
 .UNSPECIFIED., .F., .F.,
 ( 4, 3, 4 ),
 ( 1.734723475976807094E-18, 0.001246230184515564584, 0.002492489877932635520 ),
 .UNSPECIFIED. ) ;
#73677 = CARTESIAN_POINT ( 'NONE',  ( -0.6758530183727028406, -0.5511811023622048555, -0.09757992244046775898 ) ) ;
#73678 = CARTESIAN_POINT ( 'NONE',  ( 0.1998031496062992463, 0.3460692066303959202, -1.008530183727034180 ) ) ;
#73679 = CARTESIAN_POINT ( 'NONE',  ( -1.338582677165353729, -0.1870078740157479769, 0.4822834645669291653 ) ) ;
#73680 = DIRECTION ( 'NONE',  ( 0.000000000000000000, -1.000000000000000000, 0.000000000000000000 ) ) ;
#73681 = EDGE_LOOP ( 'NONE', ( #56307, #5323, #7674, #41581 ) ) ;
#73682 = CARTESIAN_POINT ( 'NONE',  ( -1.174540682414697335, -0.2845877964562161244, -0.3641732283464567121 ) ) ;
#73683 = CARTESIAN_POINT ( 'NONE',  ( -0.2493438320209966919, 0.05413385826771626580, -0.4176697321401330321 ) ) ;
#73684 = DIRECTION ( 'NONE',  ( -0.000000000000000000, -1.000000000000000000, -0.000000000000000000 ) ) ;
#73685 = CARTESIAN_POINT ( 'NONE',  ( -1.220472440944881054, -0.6692913385826771977, 8.415575281601705876E-17 ) ) ;
#73686 = FACE_OUTER_BOUND ( 'NONE', #42320, .T. ) ;
#73687 = CARTESIAN_POINT ( 'NONE',  ( 1.200787401574803681, 0.1660481256975885056, 0.3530559997133364547 ) ) ;
#73688 = CARTESIAN_POINT ( 'NONE',  ( 0.8661417322834653598, -0.1870078740157479769, 0.4822834645669291653 ) ) ;
#73689 = DIRECTION ( 'NONE',  ( 0.000000000000000000, 1.000000000000000000, -0.000000000000000000 ) ) ;
#73690 = CARTESIAN_POINT ( 'NONE',  ( 0.2945438235763075396, -0.02380624310431164736, 5.877921531841206360 ) ) ;
#73691 = CARTESIAN_POINT ( 'NONE',  ( -1.587926509186350810, -0.4281496062992124485, 0.4176697321401328655 ) ) ;
#73692 = CARTESIAN_POINT ( 'NONE',  ( 0.1070741851644053527, 0.3996062992125986590, -0.4658792650918635592 ) ) ;
#73693 = VERTEX_POINT ( 'NONE', #24251 ) ;
#73694 = CARTESIAN_POINT ( 'NONE',  ( -0.4790026246719152336, -0.08942795157528024563, -0.3641732283464568787 ) ) ;
#73695 = CARTESIAN_POINT ( 'NONE',  ( 0.3392501089628018329, 0.1958661417322835607, -2.013123359580052618 ) ) ;
#73696 = ORIENTED_EDGE ( 'NONE', *, *, #47963, .T. ) ;
#73697 = CARTESIAN_POINT ( 'NONE',  ( 0.9842519685039375910, 0.2952755905511811885, 0.000000000000000000 ) ) ;
#73698 = CARTESIAN_POINT ( 'NONE',  ( -0.4921259842519677963, -0.5400638737290844871, 0.3530559997133364547 ) ) ;
#73699 = CARTESIAN_POINT ( 'NONE',  ( -1.089238845144356427, -0.4281496062992127816, -0.4176697321401328100 ) ) ;
#73700 = CARTESIAN_POINT ( 'NONE',  ( 1.679790026246720025, 0.2306618581243848609, 0.2411417322834645549 ) ) ;
#73701 = CARTESIAN_POINT ( 'NONE',  ( -1.377952755905511140, -0.5511811023622047445, 6.969142054262312111E-17 ) ) ;
#73702 = CARTESIAN_POINT ( 'NONE',  ( -0.4470293165555038195, 1.696956328257585911, -2.611628156437945325 ) ) ;
#73703 = CARTESIAN_POINT ( 'NONE',  ( 0.5183727034120741983, -0.6692913385826771977, 0.1292274648535927661 ) ) ;
#73704 = CARTESIAN_POINT ( 'NONE',  ( -0.8005249343832011588, 0.05413385826771626580, -0.4176697321401330321 ) ) ;
#73705 = CARTESIAN_POINT ( 'NONE',  ( -0.3917322834645668994, -0.1049643490035306742, -1.543287770832334038 ) ) ;
#73706 = CARTESIAN_POINT ( 'NONE',  ( -1.246719160104985846, -0.4281496062992127816, -0.4176697321401328100 ) ) ;
#73707 = DIRECTION ( 'NONE',  ( 0.000000000000000000, 0.000000000000000000, 1.000000000000000000 ) ) ;
#73708 = CARTESIAN_POINT ( 'NONE',  ( 0.8202099737532814183, -0.6692913385826773087, -0.1292274648535924053 ) ) ;
#73709 = CARTESIAN_POINT ( 'NONE',  ( 1.174540682414699111, -0.2845877964562159024, 0.3641732283464567677 ) ) ;
#73710 = ORIENTED_EDGE ( 'NONE', *, *, #48095, .T. ) ;
#73711 = CARTESIAN_POINT ( 'NONE',  ( -9.594673741351313045E-17, 0.3917322834645670659, -2.831384145178164058 ) ) ;
#73712 = CARTESIAN_POINT ( 'NONE',  ( -0.2427821522309703550, -0.3162353388693405765, 0.4822834645669290543 ) ) ;
#73713 = ORIENTED_EDGE ( 'NONE', *, *, #16758, .T. ) ;
#73714 = AXIS2_PLACEMENT_3D ( 'NONE', #44032, #42082, #82765 ) ;
#73715 = CARTESIAN_POINT ( 'NONE',  ( 0.1968503937007881344, 0.1771653543307087630, 0.000000000000000000 ) ) ;
#73716 = CARTESIAN_POINT ( 'NONE',  ( -1.187664041994750175, -0.05778040916215560624, -0.4822834645669293319 ) ) ;
#73717 = CARTESIAN_POINT ( 'NONE',  ( 0.7939632545931766261, -0.05778040916215522460, 0.4822834645669289988 ) ) ;
#73718 = CARTESIAN_POINT ( 'NONE',  ( 0.9973753280839902091, 0.2306618581243847221, -0.2411417322834647770 ) ) ;
#73719 = CARTESIAN_POINT ( 'NONE',  ( -0.1115485564304456306, 0.2952755905511810774, -0.1292274648535930714 ) ) ;
#73720 = CARTESIAN_POINT ( 'NONE',  ( 0.3917322834645670104, 0.1049643490035304660, -1.223772596621734321 ) ) ;
#73721 = CARTESIAN_POINT ( 'NONE',  ( -0.8727034120734901146, -0.3162353388693405765, 0.4822834645669290543 ) ) ;
#73722 = CARTESIAN_POINT ( 'NONE',  ( 0.1049643490035304938, -0.3917322834645669549, -2.059711286089238591 ) ) ;
#73723 = CARTESIAN_POINT ( 'NONE',  ( -1.509186351706035767, 0.05413385826771626580, -0.4176697321401330321 ) ) ;
#73724 = CARTESIAN_POINT ( 'NONE',  ( -0.6233595800524928121, -0.3162353388693409650, -0.4822834645669289433 ) ) ;
#73725 = CARTESIAN_POINT ( 'NONE',  ( -0.4921259842519677963, 0.07958543189024071263, -0.2665933059059888421 ) ) ;
#73726 = CARTESIAN_POINT ( 'NONE',  ( 1.253280839895013710, -0.05778040916215560624, -0.4822834645669293319 ) ) ;
#73727 = CARTESIAN_POINT ( 'NONE',  ( 1.430446194225722500, -0.4281496062992127816, -0.4176697321401328100 ) ) ;
#73728 = EDGE_CURVE ( 'NONE', #47922, #55882, #78404, .T. ) ;
#73729 = CARTESIAN_POINT ( 'NONE',  ( -0.7808398950131225646, -0.05778040916215522460, 0.4822834645669289988 ) ) ;
#73730 = CARTESIAN_POINT ( 'NONE',  ( -0.3460692066303957537, -0.1998031496062994405, 0.02821522309711285356 ) ) ;
#73731 = EDGE_CURVE ( 'NONE', #32285, #60118, #65419, .T. ) ;
#73732 = CARTESIAN_POINT ( 'NONE',  ( 0.9055118110236227702, -0.6692913385826771977, 8.415575281601705876E-17 ) ) ;
#73733 = CARTESIAN_POINT ( 'NONE',  ( 0.3996062992125986035, 2.446882876249141962E-17, -1.692913385826771533 ) ) ;
#73734 = CARTESIAN_POINT ( 'NONE',  ( 3.912496512833623985, 1.354998764345328510, 0.4387572725319323075 ) ) ;
#73735 = EDGE_CURVE ( 'NONE', #11499, #4976, #56686, .T. ) ;
#73736 = CARTESIAN_POINT ( 'NONE',  ( 0.01312335958005323398, -0.4281496062992127816, -0.4176697321401328100 ) ) ;
#73737 = CARTESIAN_POINT ( 'NONE',  ( -1.167979002624671470, -0.004921259842519576551, 0.3153832671262227771 ) ) ;
#73738 = CARTESIAN_POINT ( 'NONE',  ( 0.7020997375328090762, -0.2845877964562159024, 0.3641732283464567677 ) ) ;
#73739 = CARTESIAN_POINT ( 'NONE',  ( 0.3458507752293908943, -0.3458507752293908943, -0.4901574803149606474 ) ) ;
#73740 = CARTESIAN_POINT ( 'NONE',  ( 1.069553805774278832, 0.1771653543307087075, -0.09757992244046823083 ) ) ;
#73741 = CARTESIAN_POINT ( 'NONE',  ( 0.6233595800524939223, -0.3162353388693405765, 0.4822834645669290543 ) ) ;
#73742 = CARTESIAN_POINT ( 'NONE',  ( -0.1058382717557497660, -0.3949938075777411073, -0.4639107611548556331 ) ) ;
#73743 = CARTESIAN_POINT ( 'NONE',  ( -0.1771653543307080136, -0.5400638737290844871, 0.3530559997133364547 ) ) ;
#73744 = PLANE ( 'NONE',  #74135 ) ;
#73745 = CARTESIAN_POINT ( 'NONE',  ( 1.181102362204724976, -0.1870078740157480601, -0.3641732283464567677 ) ) ;
#73746 = CARTESIAN_POINT ( 'NONE',  ( -0.5839895013123351797, 0.2952755905511810774, -0.1292274648535930714 ) ) ;
#73747 = CARTESIAN_POINT ( 'NONE',  ( 0.3949938075777408852, 0.1058382717557500435, -0.5164041994750657727 ) ) ;
#73748 = CARTESIAN_POINT ( 'NONE',  ( 1.128608923884515169, -0.6046776061558809534, -0.2411417322834644161 ) ) ;
#73749 = CARTESIAN_POINT ( 'NONE',  ( 0.1968503937007881344, 0.2952755905511811885, 0.000000000000000000 ) ) ;
#73750 = CARTESIAN_POINT ( 'NONE',  ( 0.6627296587926517768, -0.5511811023622048555, -0.09757992244046775898 ) ) ;
#73751 = DIRECTION ( 'NONE',  ( 0.000000000000000000, 0.000000000000000000, -1.000000000000000000 ) ) ;
#73752 = CARTESIAN_POINT ( 'NONE',  ( 0.1771653543307093182, -0.4536011799217368745, -0.2665933059059886201 ) ) ;
#73753 = DIRECTION ( 'NONE',  ( -1.000000000000000000, -0.000000000000000000, -0.000000000000000000 ) ) ;
#73754 = CARTESIAN_POINT ( 'NONE',  ( 0.3996062992125986035, -0.1070741851644052972, -1.290682414698162805 ) ) ;
#73755 = CARTESIAN_POINT ( 'NONE',  ( 0.6364829396325465405, -0.3162353388693409650, -0.4822834645669289433 ) ) ;
#73756 = EDGE_CURVE ( 'NONE', #46664, #73939, #75208, .T. ) ;
#73757 = CARTESIAN_POINT ( 'NONE',  ( 0.1049643490035303689, 0.3917322834645670104, -0.9304461942257216123 ) ) ;
#73758 = CARTESIAN_POINT ( 'NONE',  ( 1.640419947506562393, -0.3690944881889763329, 0.3153832671262228327 ) ) ;
#73759 = CARTESIAN_POINT ( 'NONE',  ( 0.1246719160104994284, 0.2952755905511810219, -0.1292274648535930437 ) ) ;
#73760 = CARTESIAN_POINT ( 'NONE',  ( -0.05905511811023545637, -0.4536011799217368745, -0.2665933059059886201 ) ) ;
#73761 = CARTESIAN_POINT ( 'NONE',  ( -0.006561679790025524116, -0.05778040916215560624, -0.4822834645669293319 ) ) ;
#73762 = CARTESIAN_POINT ( 'NONE',  ( 1.417322834645670104, -0.1870078740157480601, -0.3641732283464567677 ) ) ;
#73763 = CARTESIAN_POINT ( 'NONE',  ( -1.548556430446193399, 0.1283753931104748280, 0.1820866141732283561 ) ) ;
#73764 = CARTESIAN_POINT ( 'NONE',  ( -1.404199475065615932, 0.05413385826771666132, 0.4176697321401328100 ) ) ;
#73765 = CARTESIAN_POINT ( 'NONE',  ( 0.6036745406824154392, 0.2306618581243847221, -0.2411417322834647770 ) ) ;
#73766 = CARTESIAN_POINT ( 'NONE',  ( 1.220472440944882608, 0.2952755905511811885, 0.000000000000000000 ) ) ;
#73767 =( BOUNDED_CURVE ( )  B_SPLINE_CURVE ( 1, ( #48180, #74288 ),
 .UNSPECIFIED., .F., .F. ) 
 B_SPLINE_CURVE_WITH_KNOTS ( ( 2, 2 ),
 ( 4.933119884809045175E-18, 0.002000000000000006981 ),
 .UNSPECIFIED. ) 
 CURVE ( )  GEOMETRIC_REPRESENTATION_ITEM ( )  RATIONAL_B_SPLINE_CURVE ( ( 0.9875488213027523443, 0.9875488213027523443 ) ) 
 REPRESENTATION_ITEM ( '' )  );
#73768 = FACE_BOUND ( 'NONE', #52825, .T. ) ;
#73769 = CARTESIAN_POINT ( 'NONE',  ( 0.3477690288713918276, 0.2952755905511811885, 0.1292274648535926551 ) ) ;
#73770 = CARTESIAN_POINT ( 'NONE',  ( 1.227034120734908917, 0.2952755905511810774, -0.1292274648535930714 ) ) ;
#73771 = CARTESIAN_POINT ( 'NONE',  ( 0.9580052493438327987, -0.4281496062992127816, -0.4176697321401328100 ) ) ;
#73772 = CARTESIAN_POINT ( 'NONE',  ( 0.6561679790026253567, -0.5023911411419708095, -0.1820866141732282451 ) ) ;
#73773 = CARTESIAN_POINT ( 'NONE',  ( 1.463254593175853824, -0.6692913385826771977, 0.1292274648535927661 ) ) ;
#73774 = CARTESIAN_POINT ( 'NONE',  ( -0.6496062992125976043, 0.07958543189024071263, -0.2665933059059888421 ) ) ;
#73775 = CARTESIAN_POINT ( 'NONE',  ( 0.5314960629921264834, 0.07958543189024071263, -0.2665933059059888421 ) ) ;
#73776 = CARTESIAN_POINT ( 'NONE',  ( 0.1837270341207357105, -0.6046776061558809534, -0.2411417322834644161 ) ) ;
#73777 = CARTESIAN_POINT ( 'NONE',  ( 0.8661417322834652488, -0.1870078740157480879, -0.4822834645669291653 ) ) ;
#73778 = CARTESIAN_POINT ( 'NONE',  ( -0.5052493438320203589, 0.2952755905511810774, -0.1292274648535930714 ) ) ;
#73779 = CARTESIAN_POINT ( 'NONE',  ( 0.2887139107611556010, -0.5023911411419708095, 0.1820866141732285504 ) ) ;
#73780 = CARTESIAN_POINT ( 'NONE',  ( 0.6364829396325465405, -0.05778040916215522460, 0.4822834645669289988 ) ) ;
#73781 = CARTESIAN_POINT ( 'NONE',  ( -1.633215945612316311, 1.138418561298297771, 0.2566901766734876467 ) ) ;
#73782 = CARTESIAN_POINT ( 'NONE',  ( -0.8595800524934373854, -0.3162353388693409650, -0.4822834645669289433 ) ) ;
#73784 = CARTESIAN_POINT ( 'NONE',  ( -0.1998031496062991907, -0.3460692066303959757, -1.167979002624671914 ) ) ;
#73783 = PLANE ( 'NONE',  #52692 ) ;
#73785 = CARTESIAN_POINT ( 'NONE',  ( 2.149112266099340918, 1.629972608277047819, -0.4653577321740515194 ) ) ;
#73786 = CARTESIAN_POINT ( 'NONE',  ( -0.9120734908136475250, -0.6692913385826773087, -0.1292274648535924053 ) ) ;
#73787 = CARTESIAN_POINT ( 'NONE',  ( -0.2755905511811018171, 0.2952755905511811885, 0.000000000000000000 ) ) ;
#73788 = CARTESIAN_POINT ( 'NONE',  ( -1.157146581871515012E-16, 0.4724409448818898682, 0.1574803149606299191 ) ) ;
#73789 = CARTESIAN_POINT ( 'NONE',  ( 0.1058382717557499880, 0.3949938075777411073, -2.198162729658792891 ) ) ;
#73790 = EDGE_LOOP ( 'NONE', ( #44326, #17993, #79697, #75239 ) ) ;
#73791 = CARTESIAN_POINT ( 'NONE',  ( 0.6561679790026253567, -0.5023911411419708095, -0.1820866141732282451 ) ) ;
#73792 = CARTESIAN_POINT ( 'NONE',  ( -0.3392501089628019995, 0.1958661417322832277, -0.9632545931758529356 ) ) ;
#73793 = CARTESIAN_POINT ( 'NONE',  ( 0.9645669291338588858, 0.1660481256975885056, 0.3530559997133364547 ) ) ;
#73794 = LINE ( 'NONE', #54406, #54879 ) ;
#73795 = CARTESIAN_POINT ( 'NONE',  ( -1.535433070866141225, 0.1771653543307087630, 0.000000000000000000 ) ) ;
#73796 = CARTESIAN_POINT ( 'NONE',  ( 1.450131233595801428, -0.6692913385826773087, -0.1292274648535924053 ) ) ;
#73797 = CARTESIAN_POINT ( 'NONE',  ( -1.502624671916009680, -0.05778040916215560624, -0.4822834645669293319 ) ) ;
#73798 = CARTESIAN_POINT ( 'NONE',  ( 0.2755905511811031494, 0.2952755905511811885, 0.000000000000000000 ) ) ;
#73799 = CARTESIAN_POINT ( 'NONE',  ( 0.2867679344610365999, 0.2867679344610365999, -0.2178284532470323442 ) ) ;
#73800 = EDGE_CURVE ( 'NONE', #29072, #20803, #25143, .T. ) ;
#73801 = CARTESIAN_POINT ( 'NONE',  ( 0.01312335958005323398, -0.4281496062992127816, -0.4176697321401328100 ) ) ;
#73802 = CARTESIAN_POINT ( 'NONE',  ( -0.7349081364829390672, 0.1283753931104746893, -0.1820866141732285504 ) ) ;
#73803 = CARTESIAN_POINT ( 'NONE',  ( 0.9251968503937015864, -0.5400638737290844871, 0.3530559997133364547 ) ) ;
#73804 = CARTESIAN_POINT ( 'NONE',  ( -0.05249343832020938322, -0.6046776061558809534, -0.2411417322834644161 ) ) ;
#73805 = CARTESIAN_POINT ( 'NONE',  ( -0.3458507752293909498, 0.3458507752293908388, -0.01968503937007873988 ) ) ;
#73806 = CARTESIAN_POINT ( 'NONE',  ( 0.1265901696524989184, 0.4724409448818898127, -1.095800524934382958 ) ) ;
#73807 = CARTESIAN_POINT ( 'NONE',  ( -0.1049643490035307158, 0.3917322834645670104, -1.578103305283151681 ) ) ;
#73808 = CARTESIAN_POINT ( 'NONE',  ( 0.9383202099737538715, -0.05778040916215560624, -0.4822834645669293319 ) ) ;
#73809 = CARTESIAN_POINT ( 'NONE',  ( 0.2427821522309716595, -0.3162353388693409650, -0.4822834645669289433 ) ) ;
#73810 = CARTESIAN_POINT ( 'NONE',  ( -0.8792650918635160906, -0.4281496062992124485, 0.4176697321401328655 ) ) ;
#73811 = CARTESIAN_POINT ( 'NONE',  ( 1.286089238845145033, 0.2306618581243848609, 0.2411417322834645549 ) ) ;
#73812 = CARTESIAN_POINT ( 'NONE',  ( 0.6102362204724416372, 0.1660481256975883668, -0.3530559997133364547 ) ) ;
#73813 = CARTESIAN_POINT ( 'NONE',  ( 0.2867679344610365999, -0.2867679344610365444, -1.127952755905512028 ) ) ;
#73814 = CARTESIAN_POINT ( 'NONE',  ( -0.3871391076115479057, -0.3162353388693409650, -0.4822834645669289433 ) ) ;
#73815 = CARTESIAN_POINT ( 'NONE',  ( 0.7217847769028878924, 0.05413385826771666132, 0.4176697321401328100 ) ) ;
#73816 = CARTESIAN_POINT ( 'NONE',  ( -0.01312335958005186876, 0.05413385826771626580, -0.4176697321401330321 ) ) ;
#73817 = CARTESIAN_POINT ( 'NONE',  ( 0.7349081364829403995, 0.1283753931104748280, 0.1820866141732283561 ) ) ;
#73818 = CARTESIAN_POINT ( 'NONE',  ( -1.377952755905511140, 0.2952755905511811885, 0.000000000000000000 ) ) ;
#73819 = DIRECTION ( 'NONE',  ( -3.491481338843132961E-15, -0.000000000000000000, 1.000000000000000000 ) ) ;
#73820 = CARTESIAN_POINT ( 'NONE',  ( 0.2755905511811031494, -0.6692913385826771977, 8.415575281601705876E-17 ) ) ;
#73821 = DIRECTION ( 'NONE',  ( -0.000000000000000000, 1.000000000000000000, -0.000000000000000000 ) ) ;
#73822 = CARTESIAN_POINT ( 'NONE',  ( 0.1958661417322836440, -0.3392501089628017219, -2.446194225721784576 ) ) ;
#73823 = VERTEX_POINT ( 'NONE', #56243 ) ;
#73824 = EDGE_LOOP ( 'NONE', ( #1981, #67884, #6598, #31421 ) ) ;
#73825 = CARTESIAN_POINT ( 'NONE',  ( 1.272965879265092637, -0.4281496062992127816, -0.4176697321401328100 ) ) ;
#73826 = CARTESIAN_POINT ( 'NONE',  ( 0.7086614173228352742, -0.1870078740157480601, -0.3641732283464567677 ) ) ;
#73828 = PLANE ( 'NONE',  #27690 ) ;
#73827 = DIRECTION ( 'NONE',  ( 0.000000000000000000, 0.000000000000000000, 1.000000000000000000 ) ) ;
#73829 = CARTESIAN_POINT ( 'NONE',  ( -0.4574222058066962360, 1.664230899554594467, 3.910347713755335963 ) ) ;
#73830 =( CONVERSION_BASED_UNIT ( 'INCH', #73412 ) LENGTH_UNIT ( ) NAMED_UNIT ( #17997 ) );
#73831 = CARTESIAN_POINT ( 'NONE',  ( 0.1958661417322836440, -0.3392501089628017219, -1.436351706036745446 ) ) ;
#73832 = CARTESIAN_POINT ( 'NONE',  ( 0.1998031496062994128, -0.3460692066303957537, -2.215879265091863726 ) ) ;
#73833 = CARTESIAN_POINT ( 'NONE',  ( -0.9973753280839886548, 0.2306618581243848609, 0.2411417322834645549 ) ) ;
#73834 = CARTESIAN_POINT ( 'NONE',  ( -0.7874015748031489847, -0.1870078740157479769, 0.4822834645669291653 ) ) ;
#73835 = CARTESIAN_POINT ( 'NONE',  ( 0.6561679790026253567, 0.2306618581243848609, 0.2411417322834645549 ) ) ;
#73836 = ORIENTED_EDGE ( 'NONE', *, *, #82527, .F. ) ;
#73837 = CARTESIAN_POINT ( 'NONE',  ( 1.463254593175853824, 0.2952755905511810774, -0.1292274648535930714 ) ) ;
#73838 = CARTESIAN_POINT ( 'NONE',  ( -1.122045408380372367, 1.062996467714767634, 0.03161692930310931043 ) ) ;
#73839 = CONTEXT_DEPENDENT_SHAPE_REPRESENTATION ( #83101, #1638 ) ;
#73840 = CARTESIAN_POINT ( 'NONE',  ( -1.895394334970792016, 2.755905511811024056, -0.5314960629921260393 ) ) ;
#73841 = CARTESIAN_POINT ( 'NONE',  ( 0.1998031496062992463, 0.3460692066303959202, -1.953412073490813805 ) ) ;
#73842 = CARTESIAN_POINT ( 'NONE',  ( -1.358267716535432434, -0.4536011799217367080, 0.2665933059059888421 ) ) ;
#73843 = CARTESIAN_POINT ( 'NONE',  ( 1.614173228346457378, 0.7794589730111999293, 0.1372047244094478369 ) ) ;
#73844 = CARTESIAN_POINT ( 'NONE',  ( 0.1312335958005257930, 0.2306618581243847221, -0.2411417322834647770 ) ) ;
#73846 = CARTESIAN_POINT ( 'NONE',  ( -0.9285414500055713116, 0.000000000000000000, 0.6299212598425196763 ) ) ;
#73845 = CARTESIAN_POINT ( 'NONE',  ( 1.660104986876641320, -0.05778040916215522460, 0.4822834645669289988 ) ) ;
#73847 = CARTESIAN_POINT ( 'NONE',  ( -1.266404199475064773, -0.2845877964562159024, 0.3641732283464567677 ) ) ;
#73848 = CARTESIAN_POINT ( 'NONE',  ( 0.2362204724409456558, -0.1870078740157479769, 0.4822834645669291653 ) ) ;
#73849 = CARTESIAN_POINT ( 'NONE',  ( 1.476377952755906220, 0.07958543189024071263, -0.2665933059059888421 ) ) ;
#73850 = CARTESIAN_POINT ( 'NONE',  ( -0.1049643490035306742, 0.3917322834645668994, -1.188957062170916679 ) ) ;
#73851 = CARTESIAN_POINT ( 'NONE',  ( -1.108923884514435132, -0.2845877964562159024, 0.3641732283464567677 ) ) ;
#73852 = CARTESIAN_POINT ( 'NONE',  ( 1.548556430446194954, 0.2306618581243847221, -0.2411417322834647770 ) ) ;
#73853 = CARTESIAN_POINT ( 'NONE',  ( 2.620894764083865347, 1.710972922415818331, -0.4417590601942915640 ) ) ;
#73854 = CARTESIAN_POINT ( 'NONE',  ( -0.2952755905511804668, 0.1660481256975885056, 0.3530559997133364547 ) ) ;
#73855 = CARTESIAN_POINT ( 'NONE',  ( -1.220472440944881054, -0.5511811023622047445, 6.969142054262312111E-17 ) ) ;
#73856 = CARTESIAN_POINT ( 'NONE',  ( -0.4330708661417315697, 0.1771653543307087630, 0.000000000000000000 ) ) ;
#73857 = CARTESIAN_POINT ( 'NONE',  ( -0.6102362204724400829, 0.1660481256975885056, 0.3530559997133364547 ) ) ;
#73858 = CARTESIAN_POINT ( 'NONE',  ( -1.437007874015747477, 0.07958543189024071263, -0.2665933059059888421 ) ) ;
#73859 = CARTESIAN_POINT ( 'NONE',  ( -0.2867679344610365444, -0.2867679344610367664, -0.5282345388789521090 ) ) ;
#73860 = CARTESIAN_POINT ( 'NONE',  ( 0.2165354330708668673, 0.1660481256975883668, -0.3530559997133364547 ) ) ;
#73861 = CARTESIAN_POINT ( 'NONE',  ( 0.8785612751854029456, 3.421639014772782816E-16, 0.3464511005275203726 ) ) ;
#73862 = CARTESIAN_POINT ( 'NONE',  ( 0.4724409448818897572, -0.1265901696524988906, -2.078083989501312345 ) ) ;
#73863 = CARTESIAN_POINT ( 'NONE',  ( -1.023622047244094002, -0.1870078740157480879, -0.4822834645669291653 ) ) ;
#73864 = CARTESIAN_POINT ( 'NONE',  ( -0.6299212598425188991, -0.1870078740157479769, 0.3641732283464567677 ) ) ;
#73865 = ADVANCED_FACE ( 'NONE', ( #61741 ), #10325, .T. ) ;
#73866 = CARTESIAN_POINT ( 'NONE',  ( 0.7984992590978667870, -1.206088964116209378E-16, 0.3954974714151466841 ) ) ;
#73867 = CARTESIAN_POINT ( 'NONE',  ( -0.1246719160104980823, -0.6692913385826773087, -0.1292274648535924053 ) ) ;
#73868 = CARTESIAN_POINT ( 'NONE',  ( 0.5118110236220480003, -0.5511811023622047445, 6.969142054262312111E-17 ) ) ;
#73869 = CARTESIAN_POINT ( 'NONE',  ( -0.8792650918635160906, -0.004921259842519870586, -0.3153832671262229437 ) ) ;
#73870 = CARTESIAN_POINT ( 'NONE',  ( -1.633858267716534529, -0.5400638737290845981, -0.3530559997133363437 ) ) ;
#73871 = CARTESIAN_POINT ( 'NONE',  ( -1.528871391076114250, 0.2952755905511810774, -0.1292274648535930714 ) ) ;
#73872 = CARTESIAN_POINT ( 'NONE',  ( 1.364829396325460076, 0.2306618581243848609, 0.2411417322834645549 ) ) ;
#73873 = CARTESIAN_POINT ( 'NONE',  ( 0.4672469119858274067, 1.453788974454132132, 2.153180749494128854 ) ) ;
#73874 = CARTESIAN_POINT ( 'NONE',  ( 0.9186351706036752773, 0.1283753931104746893, -0.1820866141732285504 ) ) ;
#73875 = CARTESIAN_POINT ( 'NONE',  ( 0.7217847769028878924, 0.05413385826771666132, 0.4176697321401328100 ) ) ;
#73876 = ADVANCED_FACE ( 'NONE', ( #75622 ), #9991, .T. ) ;
#73877 = FACE_OUTER_BOUND ( 'NONE', #22354, .T. ) ;
#73878 = CARTESIAN_POINT ( 'NONE',  ( 1.502624671916010790, -0.2845877964562161244, -0.3641732283464567121 ) ) ;
#73879 = ORIENTED_EDGE ( 'NONE', *, *, #9980, .T. ) ;
#73880 = CARTESIAN_POINT ( 'NONE',  ( -1.325459317585300889, 0.05413385826771666132, 0.4176697321401328100 ) ) ;
#73881 = CARTESIAN_POINT ( 'NONE',  ( -0.9514435695538050464, -0.05778040916215560624, -0.4822834645669293319 ) ) ;
#73882 = CARTESIAN_POINT ( 'NONE',  ( 0.2624671916010504757, -0.6046776061558809534, -0.2411417322834644161 ) ) ;
#73883 = CARTESIAN_POINT ( 'NONE',  ( -1.299212598425196097, -0.5511811023622047445, 6.969142054262312111E-17 ) ) ;
#73884 = CARTESIAN_POINT ( 'NONE',  ( 0.3996062992125986035, -0.1070741851644052972, -2.078083989501312345 ) ) ;
#73885 = CARTESIAN_POINT ( 'NONE',  ( 1.548556430446194954, -0.5023911411419708095, 0.1820866141732285504 ) ) ;
#73886 = CARTESIAN_POINT ( 'NONE',  ( 0.4199475065616805614, 0.2306618581243848609, 0.2411417322834645549 ) ) ;
#73887 = CARTESIAN_POINT ( 'NONE',  ( 0.7677165354330716118, -0.5400638737290844871, 0.3530559997133364547 ) ) ;
#73888 = CARTESIAN_POINT ( 'NONE',  ( 1.653543307086614789, -0.1870078740157479769, 0.4822834645669291653 ) ) ;
#73889 = CARTESIAN_POINT ( 'NONE',  ( 0.2925321140481932369, 0.2925321140481932369, -1.870078740157480546 ) ) ;
#73890 = CARTESIAN_POINT ( 'NONE',  ( -0.3949938075777409408, -0.1058382717557502933, -0.9908136482939633449 ) ) ;
#73891 = CARTESIAN_POINT ( 'NONE',  ( 0.3460692066303959202, 0.1998031496062993295, -2.650918635170603554 ) ) ;
#73892 = DIRECTION ( 'NONE',  ( -0.000000000000000000, 1.000000000000000000, -0.000000000000000000 ) ) ;
#73893 = CARTESIAN_POINT ( 'NONE',  ( -0.2867679344610366554, 0.2867679344610365444, -0.01181102362204719883 ) ) ;
#73894 = CARTESIAN_POINT ( 'NONE',  ( 0.01312335958005323398, -0.004921259842519576551, 0.3153832671262227771 ) ) ;
#73895 = CARTESIAN_POINT ( 'NONE',  ( -0.2034120734908131112, -0.6692913385826773087, -0.1292274648535924053 ) ) ;
#73896 = CARTESIAN_POINT ( 'NONE',  ( 0.9120734908136489683, -0.6692913385826771977, 0.1292274648535927661 ) ) ;
#73897 = CARTESIAN_POINT ( 'NONE',  ( 0.1058382717557499880, 0.3949938075777409408, -2.274934383202099841 ) ) ;
#73898 = CARTESIAN_POINT ( 'NONE',  ( -0.006561679790025524116, -0.08942795157528024563, -0.3641732283464568787 ) ) ;
#73899 = CARTESIAN_POINT ( 'NONE',  ( -0.9842519685039360366, 0.2952755905511811885, 0.000000000000000000 ) ) ;
#73900 = CARTESIAN_POINT ( 'NONE',  ( 1.128608923884514947, 0.2306618581243848609, 0.2411417322834645549 ) ) ;
#73901 = CARTESIAN_POINT ( 'NONE',  ( 0.3458507752293908943, 0.3458507752293908943, -2.500000000000000444 ) ) ;
#73902 = CARTESIAN_POINT ( 'NONE',  ( 0.3996062992125986035, 0.1070741851644054776, -1.541994750656167978 ) ) ;
#73903 = PLANE ( 'NONE',  #57256 ) ;
#73904 = EDGE_LOOP ( 'NONE', ( #29040, #55259, #25751, #42926 ) ) ;
#73905 = ORIENTED_EDGE ( 'NONE', *, *, #70014, .T. ) ;
#73906 = CARTESIAN_POINT ( 'NONE',  ( 1.187664041994751285, -0.3162353388693409650, -0.4822834645669289433 ) ) ;
#73907 = EDGE_CURVE ( 'NONE', #19973, #38184, #35150, .T. ) ;
#73908 = CARTESIAN_POINT ( 'NONE',  ( -1.719160104986876103, 0.05413385826771666132, 0.4176697321401328100 ) ) ;
#73910 = CARTESIAN_POINT ( 'NONE',  ( -1.450131233595799651, 0.2952755905511810774, -0.1292274648535930714 ) ) ;
#73909 = CARTESIAN_POINT ( 'NONE',  ( -1.017060367454067249, -0.08942795157527998196, 0.3641732283464567121 ) ) ;
#73911 = CARTESIAN_POINT ( 'NONE',  ( -0.1049643490035307020, 0.3917322834645669549, 0.2237532808398949025 ) ) ;
#73912 = CARTESIAN_POINT ( 'NONE',  ( 1.192598508356890630, 4.598214627222820490E-16, 0.3791483426435169335 ) ) ;
#73913 = CARTESIAN_POINT ( 'NONE',  ( 1.213910761154856299, 0.2952755905511811885, 0.1292274648535926551 ) ) ;
#73914 = CARTESIAN_POINT ( 'NONE',  ( -1.450131233595799651, -0.6692913385826771977, 0.1292274648535927661 ) ) ;
#73915 = CARTESIAN_POINT ( 'NONE',  ( -0.05249343832020938322, -0.6046776061558809534, -0.2411417322834644161 ) ) ;
#73916 = CARTESIAN_POINT ( 'NONE',  ( -0.5052493438320203589, -0.6692913385826771977, 0.1292274648535927661 ) ) ;
#73917 = CARTESIAN_POINT ( 'NONE',  ( 1.496062992125984703, -0.1870078740157480879, -0.4822834645669291653 ) ) ;
#73918 = CARTESIAN_POINT ( 'NONE',  ( -0.2867679344610365999, 0.2867679344610364889, -0.1043307086614174151 ) ) ;
#73919 = CARTESIAN_POINT ( 'NONE',  ( 0.07217847769028949700, -0.05778040916215560624, -0.4822834645669293319 ) ) ;
#73920 = CARTESIAN_POINT ( 'NONE',  ( 0.2867679344610365999, 0.2867679344610365999, -2.177165354330708347 ) ) ;
#73921 = CARTESIAN_POINT ( 'NONE',  ( -1.443569553805773564, 0.1283753931104746893, -0.1820866141732285504 ) ) ;
#73922 = ORIENTED_EDGE ( 'NONE', *, *, #34666, .T. ) ;
#73923 = CARTESIAN_POINT ( 'NONE',  ( 0.1974969037888704704, 0.3420746716998660508, -2.191601049868766360 ) ) ;
#73924 = ORIENTED_EDGE ( 'NONE', *, *, #20205, .T. ) ;
#73925 = CARTESIAN_POINT ( 'NONE',  ( -1.220472440944881054, 2.362204724409448620, 0.5309055118110237448 ) ) ;
#73926 = CARTESIAN_POINT ( 'NONE',  ( -1.391076115485563758, 0.2306618581243848609, 0.2411417322834645549 ) ) ;
#73927 = CARTESIAN_POINT ( 'NONE',  ( -0.2925321140481930704, -0.2925321140481933480, -1.161417322834645383 ) ) ;
#73928 = DIRECTION ( 'NONE',  ( 1.000000000000000000, 0.000000000000000000, 0.000000000000000000 ) ) ;
#73929 = CARTESIAN_POINT ( 'NONE',  ( 1.024290093949184799, 1.664773289199195982, -0.4581164262379300856 ) ) ;
#73930 = CARTESIAN_POINT ( 'NONE',  ( -0.9564677561141805562, 0.02791078216816347476, -0.4328096321851898631 ) ) ;
#73931 = DIRECTION ( 'NONE',  ( 1.000000000000000000, 0.000000000000000000, 0.000000000000000000 ) ) ;
#73932 = CARTESIAN_POINT ( 'NONE',  ( 0.2867679344610365999, -0.2867679344610365444, -0.1830708661417323746 ) ) ;
#73933 = CARTESIAN_POINT ( 'NONE',  ( -0.2165354330708654795, 0.07958543189024085140, 0.2665933059059887866 ) ) ;
#73934 = CARTESIAN_POINT ( 'NONE',  ( -0.7611548556430438595, 0.1283753931104748280, 0.1820866141732283561 ) ) ;
#73935 = CARTESIAN_POINT ( 'NONE',  ( -1.122047244094487306, 0.1660481256975883668, -0.3530559997133364547 ) ) ;
#73936 = CARTESIAN_POINT ( 'NONE',  ( 0.4461942257217855201, -0.6046776061558807314, 0.2411417322834647770 ) ) ;
#73937 = CARTESIAN_POINT ( 'NONE',  ( -1.463254593175852492, 0.2952755905511811885, 0.1292274648535926551 ) ) ;
#73938 = CARTESIAN_POINT ( 'NONE',  ( 4.797336870675656522E-17, -0.3917322834645670104, -0.07086614173228342195 ) ) ;
#73939 = VERTEX_POINT ( 'NONE', #54999 ) ;
#73940 = CARTESIAN_POINT ( 'NONE',  ( -1.476377952755905110, 0.1660481256975885056, 0.3530559997133364547 ) ) ;
#73941 = CARTESIAN_POINT ( 'NONE',  ( -1.614173228346456712, 2.094556775020298467, -0.1372047244094478091 ) ) ;
#73942 = CARTESIAN_POINT ( 'NONE',  ( -0.2362204724409451284, 0.4091458600556402425, -1.587926509186351698 ) ) ;
#73943 = CARTESIAN_POINT ( 'NONE',  ( 2.795275590551181910, 1.488513638086842006, 0.000000000000000000 ) ) ;
#73944 = CARTESIAN_POINT ( 'NONE',  ( -0.3917322834645669549, -0.1049643490035306603, -0.8254593175853015552 ) ) ;
#73945 = CARTESIAN_POINT ( 'NONE',  ( 1.614173228346456712, 2.401574803149606474, -0.5309055118110239668 ) ) ;
#73946 = CARTESIAN_POINT ( 'NONE',  ( -0.5905511811023613777, -0.6692913385826771977, 8.415575281601705876E-17 ) ) ;
#73947 = CARTESIAN_POINT ( 'NONE',  ( 1.351706036745407680, 0.05413385826771666132, 0.4176697321401328100 ) ) ;
#73949 = CARTESIAN_POINT ( 'NONE',  ( 0.2362204724409451007, -0.4091458600556402980, -1.981627296587926690 ) ) ;
#73948 = DIRECTION ( 'NONE',  ( -0.000000000000000000, 1.000000000000000000, -0.000000000000000000 ) ) ;
#73950 = CARTESIAN_POINT ( 'NONE',  ( -1.541994750656167090, 0.2952755905511811885, 0.1292274648535926551 ) ) ;
#73951 = CARTESIAN_POINT ( 'NONE',  ( -0.8267716535433065062, -0.6692913385826771977, 8.415575281601705876E-17 ) ) ;
#73952 = CARTESIAN_POINT ( 'NONE',  ( 0.3392501089628018329, -0.1958661417322834497, -0.02753973933627114692 ) ) ;
#73953 = CARTESIAN_POINT ( 'NONE',  ( -0.03937007874015669567, -0.5511811023622047445, 6.969142054262312111E-17 ) ) ;
#73954 = CARTESIAN_POINT ( 'NONE',  ( 0.1958661417322836440, -0.3392501089628017219, -0.3339895013123360679 ) ) ;
#73955 = CARTESIAN_POINT ( 'NONE',  ( -0.2821522309711278487, -0.5511811023622048555, -0.09757992244046775898 ) ) ;
#73956 = CARTESIAN_POINT ( 'NONE',  ( 1.003937007874016185, 0.07958543189024071263, -0.2665933059059888421 ) ) ;
#73957 = CARTESIAN_POINT ( 'NONE',  ( 0.8267716535433077274, 0.2952755905511811885, 0.000000000000000000 ) ) ;
#73958 = UNCERTAINTY_MEASURE_WITH_UNIT (LENGTH_MEASURE( 1.000000000000000082E-05 ), #215, 'distance_accuracy_value', 'NONE');
#73959 = CARTESIAN_POINT ( 'NONE',  ( -0.3280839895013117347, -0.004921259842519870586, -0.3153832671262229437 ) ) ;
#73960 = CARTESIAN_POINT ( 'NONE',  ( -0.1958661417322834220, -0.3392501089628018884, -2.262467191601049699 ) ) ;
#73961 = CARTESIAN_POINT ( 'NONE',  ( -1.535433070866141225, -0.6692913385826771977, 8.415575281601705876E-17 ) ) ;
#73962 = CARTESIAN_POINT ( 'NONE',  ( -1.410761154855641575, -0.2845877964562161244, -0.3641732283464567121 ) ) ;
#73963 = CARTESIAN_POINT ( 'NONE',  ( -0.2362204724409451284, 0.4091458600556402425, -0.2473753280839895152 ) ) ;
#73964 = CARTESIAN_POINT ( 'NONE',  ( 0.2559055118110243332, -0.5400638737290845981, -0.3530559997133363437 ) ) ;
#73965 = EDGE_CURVE ( 'NONE', #21217, #34363, #46590, .T. ) ;
#73966 = CARTESIAN_POINT ( 'NONE',  ( -0.08530183727034056085, -0.3162353388693405765, 0.4822834645669290543 ) ) ;
#73967 = CARTESIAN_POINT ( 'NONE',  ( 1.476377952755906442, -0.4536011799217367080, 0.2665933059059888421 ) ) ;
#73968 = CARTESIAN_POINT ( 'NONE',  ( 0.6561679790026253567, 0.1283753931104748280, 0.1820866141732283561 ) ) ;
#73969 = CARTESIAN_POINT ( 'NONE',  ( -0.2559055118110230564, 0.07958543189024071263, -0.2665933059059888421 ) ) ;
#73970 = CARTESIAN_POINT ( 'NONE',  ( -0.7874015748031489847, -0.1870078740157480879, -0.4822834645669291653 ) ) ;
#73971 = CARTESIAN_POINT ( 'NONE',  ( -1.586052503253845503, 2.125984251968505045, 0.1653254495020588799 ) ) ;
#73972 = DIRECTION ( 'NONE',  ( 0.000000000000000000, 0.000000000000000000, 1.000000000000000000 ) ) ;
#73973 = CARTESIAN_POINT ( 'NONE',  ( 0.2559055118110243332, 0.1660481256975885056, 0.3530559997133364547 ) ) ;
#73974 = CARTESIAN_POINT ( 'NONE',  ( 0.3460692066303958092, 0.1998031496062993018, -1.625328083989501460 ) ) ;
#73975 = CARTESIAN_POINT ( 'NONE',  ( 0.000000000000000000, 2.559055118110236560, 0.000000000000000000 ) ) ;
#73976 = CARTESIAN_POINT ( 'NONE',  ( -0.08530183727034056085, -0.08942795157528024563, -0.3641732283464568787 ) ) ;
#73977 = CARTESIAN_POINT ( 'NONE',  ( -0.1771653543307080136, -0.5400638737290844871, 0.3530559997133364547 ) ) ;
#73978 = LINE ( 'NONE', #16324, #20951 ) ;
#73979 = CARTESIAN_POINT ( 'NONE',  ( 1.528871391076116026, 0.2952755905511811885, 0.1292274648535926551 ) ) ;
#73980 = CARTESIAN_POINT ( 'NONE',  ( 1.410761154855643795, -0.05778040916215560624, -0.4822834645669293319 ) ) ;
#73981 = CARTESIAN_POINT ( 'NONE',  ( 3.937007874015748143, 1.537401574803149984, 2.901595197523589142E-16 ) ) ;
#73982 = CARTESIAN_POINT ( 'NONE',  ( -0.7086614173228339419, -0.1870078740157480601, -0.3641732283464567677 ) ) ;
#73983 = CARTESIAN_POINT ( 'NONE',  ( 0.2925321140481931814, 0.2925321140481931814, -0.3720472440944882497 ) ) ;
#73984 = CARTESIAN_POINT ( 'NONE',  ( -0.3460692066303960868, 0.1998031496062990242, -0.3412073490813647969 ) ) ;
#73985 = CARTESIAN_POINT ( 'NONE',  ( -0.3949938075777409963, -7.255918531996591613E-17, 0.1181102362204723977 ) ) ;
#73986 = AXIS2_PLACEMENT_3D ( 'NONE', #27874, #78821, #34612 ) ;
#73987 = FACE_OUTER_BOUND ( 'NONE', #81908, .T. ) ;
#73988 = CARTESIAN_POINT ( 'NONE',  ( 1.227034120734908917, -0.5511811023622046335, 0.09757992244046803654 ) ) ;
#73989 = CARTESIAN_POINT ( 'NONE',  ( -1.509186351706035767, 0.05413385826771626580, -0.4176697321401330321 ) ) ;
#73990 = CARTESIAN_POINT ( 'NONE',  ( 0.9448818897637802916, -0.1870078740157479769, 0.4822834645669291653 ) ) ;
#73991 = CARTESIAN_POINT ( 'NONE',  ( 4.837279021331061486E-17, -0.3949938075777409963, -1.100393700787401619 ) ) ;
#73992 = CARTESIAN_POINT ( 'NONE',  ( 1.030183727034121421, -0.08942795157527998196, 0.3641732283464567121 ) ) ;
#73993 = CARTESIAN_POINT ( 'NONE',  ( 0.1640419947506569498, -0.3162353388693409650, -0.4822834645669289433 ) ) ;
#73994 = CARTESIAN_POINT ( 'NONE',  ( -1.017060367454067249, -0.05778040916215522460, 0.4822834645669289988 ) ) ;
#73995 = CARTESIAN_POINT ( 'NONE',  ( 1.633858267716535639, -0.5400638737290844871, 0.3530559997133364547 ) ) ;
#73996 = CARTESIAN_POINT ( 'NONE',  ( 0.2362204724409449064, 0.4091458600556404646, -1.089238845144356871 ) ) ;
#73997 = CARTESIAN_POINT ( 'NONE',  ( 0.3460692066303959202, 0.1998031496062993295, -2.335958005249343827 ) ) ;
#73998 = CARTESIAN_POINT ( 'NONE',  ( 0.2755905511811031494, -0.5511811023622047445, 6.969142054262312111E-17 ) ) ;
#73999 = EDGE_LOOP ( 'NONE', ( #31958, #32761, #11261, #20255, #38504, #40670 ) ) ;
#74000 = CARTESIAN_POINT ( 'NONE',  ( -0.3917322834645671770, 0.1049643490035302024, -0.1870271897975872011 ) ) ;
#74001 = EDGE_LOOP ( 'NONE', ( #70788, #7535, #1043 ) ) ;
#74002 = CARTESIAN_POINT ( 'NONE',  ( -0.2952755905511804668, 0.1660481256975885056, 0.3530559997133364547 ) ) ;
#74003 = CARTESIAN_POINT ( 'NONE',  ( 0.01312335958005323398, -0.4281496062992127816, -0.4176697321401328100 ) ) ;
#74004 = CARTESIAN_POINT ( 'NONE',  ( -0.2821522309711278487, -0.5511811023622048555, -0.09757992244046775898 ) ) ;
#74005 = CARTESIAN_POINT ( 'NONE',  ( 0.6955380577427828781, -0.4281496062992124485, 0.4176697321401328655 ) ) ;
#74006 = CARTESIAN_POINT ( 'NONE',  ( -0.7808398950131222316, -0.3162353388693409650, -0.4822834645669289433 ) ) ;
#74007 = CARTESIAN_POINT ( 'NONE',  ( -0.3412073490813641308, -0.6046776061558807314, 0.2411417322834647770 ) ) ;
#74008 = CARTESIAN_POINT ( 'NONE',  ( 0.9973753280839902091, 0.2306618581243847221, -0.2411417322834647770 ) ) ;
#74009 = CARTESIAN_POINT ( 'NONE',  ( 0.9186351706036751663, -0.6046776061558807314, 0.2411417322834647770 ) ) ;
#74010 = CARTESIAN_POINT ( 'NONE',  ( 0.9317585301837276734, 0.05413385826771626580, -0.4176697321401330321 ) ) ;
#74011 = CARTESIAN_POINT ( 'NONE',  ( 0.1958661417322836440, -0.3392501089628017219, -1.028871391076115360 ) ) ;
#74012 = CARTESIAN_POINT ( 'NONE',  ( 0.01312335958005323398, -0.3690944881889765550, -0.3153832671262227771 ) ) ;
#74013 = ORIENTED_EDGE ( 'NONE', *, *, #27995, .T. ) ;
#74014 = CARTESIAN_POINT ( 'NONE',  ( -0.3420746716998661618, 0.1974969037888702206, -0.9711286089238846397 ) ) ;
#74015 = VERTEX_POINT ( 'NONE', #77263 ) ;
#74016 = CARTESIAN_POINT ( 'NONE',  ( -1.023622047244094002, -0.1870078740157480601, -0.3641732283464567677 ) ) ;
#74017 = CARTESIAN_POINT ( 'NONE',  ( -0.2821522309711278487, -0.6692913385826773087, -0.1292274648535924053 ) ) ;
#74018 = CARTESIAN_POINT ( 'NONE',  ( -1.382164990278195615, 1.299212598425196985, 0.4102808022082835571 ) ) ;
#74019 = CARTESIAN_POINT ( 'NONE',  ( -0.5774278215223089816, 0.2306618581243847221, -0.2411417322834647770 ) ) ;
#74020 = CARTESIAN_POINT ( 'NONE',  ( -0.4593175853018366950, 0.05413385826771666132, 0.4176697321401328100 ) ) ;
#74021 = CARTESIAN_POINT ( 'NONE',  ( -1.266404199475064773, -0.05778040916215560624, -0.4822834645669293319 ) ) ;
#74022 = CARTESIAN_POINT ( 'NONE',  ( -1.620734908136482577, -0.6692913385826773087, -0.1292274648535924053 ) ) ;
#74023 = CARTESIAN_POINT ( 'NONE',  ( 1.003937007874016407, -0.4536011799217367080, 0.2665933059059888421 ) ) ;
#74024 = DIRECTION ( 'NONE',  ( 0.000000000000000000, 1.000000000000000000, 0.000000000000000000 ) ) ;
#74025 = CARTESIAN_POINT ( 'NONE',  ( 0.2431881074996896375, 0.1674863405202415556, 5.643916622257989957 ) ) ;
#74026 = CARTESIAN_POINT ( 'NONE',  ( 0.4986876640419954376, 0.1283753931104748280, 0.1820866141732283561 ) ) ;
#74027 = CARTESIAN_POINT ( 'NONE',  ( -0.09842519685039295696, -0.5400638737290844871, 0.3530559997133364547 ) ) ;
#74028 = CARTESIAN_POINT ( 'NONE',  ( 0.2755905511811031494, 0.2952755905511811885, 0.000000000000000000 ) ) ;
#74029 = ORIENTED_EDGE ( 'NONE', *, *, #20687, .T. ) ;
#74030 = CARTESIAN_POINT ( 'NONE',  ( -9.787531504996567848E-17, 0.3996062992125986035, -1.574803149606299302 ) ) ;
#74031 = LINE ( 'NONE', #16794, #27792 ) ;
#74032 = ORIENTED_EDGE ( 'NONE', *, *, #79270, .F. ) ;
#74033 = CARTESIAN_POINT ( 'NONE',  ( -0.3996062992125984925, -0.1070741851644056858, -1.225065616797899937 ) ) ;
#74034 = CARTESIAN_POINT ( 'NONE',  ( 1.535433070866142335, -0.6692913385826771977, 8.415575281601705876E-17 ) ) ;
#74035 = CARTESIAN_POINT ( 'NONE',  ( -0.8202099737532801971, -0.5511811023622046335, 0.09757992244046803654 ) ) ;
#74036 = CARTESIAN_POINT ( 'NONE',  ( -0.9514435695538050464, -0.3162353388693405765, 0.4822834645669290543 ) ) ;
#74037 = CARTESIAN_POINT ( 'NONE',  ( 0.1265901696524989462, 0.4724409448818897572, -0.6233595800524933672 ) ) ;
#74038 = CARTESIAN_POINT ( 'NONE',  ( 0.3917322834645669549, 0.1049643490035304660, -2.414041994750655729 ) ) ;
#74039 = CARTESIAN_POINT ( 'NONE',  ( 1.522309711286089939, 0.2306618581243848609, 0.2411417322834645549 ) ) ;
#74040 = CARTESIAN_POINT ( 'NONE',  ( 0.5905511811023629321, -0.6692913385826771977, 8.415575281601705876E-17 ) ) ;
#74041 = CARTESIAN_POINT ( 'NONE',  ( 0.6824146981627303710, -0.6046776061558807314, 0.2411417322834647770 ) ) ;
#74042 = CARTESIAN_POINT ( 'NONE',  ( -0.5971128608923877978, -0.5511811023622048555, -0.09757992244046775898 ) ) ;
#74043 = CARTESIAN_POINT ( 'NONE',  ( 0.09186351706036799403, -0.4281496062992127816, -0.4176697321401328100 ) ) ;
#74044 = CARTESIAN_POINT ( 'NONE',  ( 5.785732909357575061E-17, -0.4724409448818898682, -2.202755905511811108 ) ) ;
#74045 = CARTESIAN_POINT ( 'NONE',  ( -0.4593175853018364174, -0.3690944881889765550, -0.3153832671262227771 ) ) ;
#74046 = CARTESIAN_POINT ( 'NONE',  ( -0.3543307086614165824, -0.6692913385826771977, 8.415575281601705876E-17 ) ) ;
#74047 = CARTESIAN_POINT ( 'NONE',  ( 0.1974969037888704704, 0.3420746716998660508, -1.795931758530183942 ) ) ;
#74048 = CARTESIAN_POINT ( 'NONE',  ( -1.541994750656167090, 0.2952755905511811885, 0.1292274648535926551 ) ) ;
#74049 = CARTESIAN_POINT ( 'NONE',  ( 0.05249343832021075018, 0.1283753931104746893, -0.1820866141732285504 ) ) ;
#74050 = CARTESIAN_POINT ( 'NONE',  ( 1.358267716535433323, 0.07958543189024085140, 0.2665933059059887866 ) ) ;
#74051 = CARTESIAN_POINT ( 'NONE',  ( -1.023622047244094002, -0.1870078740157480879, -0.4822834645669291653 ) ) ;
#74052 = CIRCLE ( 'NONE', #65935, 1.122047244094488194 ) ;
#74053 = CARTESIAN_POINT ( 'NONE',  ( -0.8530183727034112984, -0.004921259842519576551, 0.3153832671262227771 ) ) ;
#74054 = DIRECTION ( 'NONE',  ( 1.408710688920637755E-15, -1.000000000000000000, 4.918487082195260922E-30 ) ) ;
#74055 = CARTESIAN_POINT ( 'NONE',  ( -1.135170603674539924, -0.6692913385826771977, 0.1292274648535927661 ) ) ;
#74056 = CARTESIAN_POINT ( 'NONE',  ( -0.2887139107611542133, -0.6046776061558809534, -0.2411417322834644161 ) ) ;
#74057 = ADVANCED_FACE ( 'NONE', ( #50742 ), #45254, .F. ) ;
#74058 = CARTESIAN_POINT ( 'NONE',  ( 0.3477690288713918276, -0.6692913385826773087, -0.1292274648535924053 ) ) ;
#74059 = CARTESIAN_POINT ( 'NONE',  ( -0.3917322834645670659, 0.1049643490035301607, -2.475046301016061268 ) ) ;
#74060 = DIRECTION ( 'NONE',  ( -0.000000000000000000, -1.000000000000000000, 0.000000000000000000 ) ) ;
#74061 = CARTESIAN_POINT ( 'NONE',  ( 0.4396325459317593221, 0.1771653543307087075, -0.09757992244046823083 ) ) ;
#74062 = CARTESIAN_POINT ( 'NONE',  ( 1.115485564304462551, 0.05413385826771666132, 0.4176697321401328100 ) ) ;
#74063 = CARTESIAN_POINT ( 'NONE',  ( -1.089238845144356427, -0.004921259842519576551, 0.3153832671262227771 ) ) ;
#74064 = CARTESIAN_POINT ( 'NONE',  ( 1.240157480314961314, 0.1660481256975883668, -0.3530559997133364547 ) ) ;
#74065 = CARTESIAN_POINT ( 'NONE',  ( -1.646981627296586703, -0.2845877964562161244, -0.3641732283464567121 ) ) ;
#74066 = CARTESIAN_POINT ( 'NONE',  ( -1.515748031496062076, 0.1660481256975883668, -0.3530559997133364547 ) ) ;
#74067 = CARTESIAN_POINT ( 'NONE',  ( -0.8858267716535425107, 0.1660481256975883668, -0.3530559997133364547 ) ) ;
#74068 = CARTESIAN_POINT ( 'NONE',  ( 0.08530183727034192087, -0.08942795157527998196, 0.3641732283464567121 ) ) ;
#74069 = CARTESIAN_POINT ( 'NONE',  ( -0.8776378784356294593, 5.410171027439680070E-15, -0.3791483426435165449 ) ) ;
#74070 = CARTESIAN_POINT ( 'NONE',  ( 0.6299212598425204535, -0.1870078740157479769, 0.3641732283464567677 ) ) ;
#74071 = MECHANICAL_DESIGN_GEOMETRIC_PRESENTATION_REPRESENTATION (  '', ( #27010 ), #17590 ) ;
#74072 = CARTESIAN_POINT ( 'NONE',  ( -0.1377952755905504645, -0.5400638737290845981, -0.3530559997133363437 ) ) ;
#74073 = CARTESIAN_POINT ( 'NONE',  ( 0.3996062992125984925, 0.1070741851644054637, -0.2014435695538057958 ) ) ;
#74074 = CARTESIAN_POINT ( 'NONE',  ( -1.003937007874015297, -0.5400638737290845981, -0.3530559997133363437 ) ) ;
#74075 = CARTESIAN_POINT ( 'NONE',  ( -0.3392501089628019995, 0.1958661417322832277, -2.000656167979002920 ) ) ;
#74076 = CARTESIAN_POINT ( 'NONE',  ( 1.102362204724410155, -0.1870078740157479769, 0.3641732283464567677 ) ) ;
#74077 = CARTESIAN_POINT ( 'NONE',  ( 0.1640419947506569498, -0.3162353388693409650, -0.4822834645669289433 ) ) ;
#74078 = CARTESIAN_POINT ( 'NONE',  ( -0.4461942257217840213, -0.6046776061558809534, -0.2411417322834644161 ) ) ;
#74079 = CARTESIAN_POINT ( 'NONE',  ( -0.5249343832020990641, 0.1283753931104748280, 0.1820866141732283561 ) ) ;
#74080 = CARTESIAN_POINT ( 'NONE',  ( 0.4724409448818898682, 0.000000000000000000, -2.755905511811024056 ) ) ;
#74081 = CARTESIAN_POINT ( 'NONE',  ( -0.3608923884514428360, 0.1771653543307087630, 0.09757992244046791164 ) ) ;
#74082 = CARTESIAN_POINT ( 'NONE',  ( 0.4199475065616805614, 0.2306618581243848609, 0.2411417322834645549 ) ) ;
#74083 = CARTESIAN_POINT ( 'NONE',  ( -1.056430446194224881, 0.1771653543307087075, -0.09757992244046823083 ) ) ;
#74084 = CARTESIAN_POINT ( 'NONE',  ( -0.1070741851644051862, -0.3996062992125986590, -1.093832020997375087 ) ) ;
#74085 = CARTESIAN_POINT ( 'NONE',  ( -1.299212598425196097, 0.2952755905511811885, 0.000000000000000000 ) ) ;
#74086 = CARTESIAN_POINT ( 'NONE',  ( 0.2238009295390077091, 2.409604939980833412E-17, -0.3464511005275205946 ) ) ;
#74087 = VERTEX_POINT ( 'NONE', #69708 ) ;
#74088 = CARTESIAN_POINT ( 'NONE',  ( -1.607611548556429737, -0.5511811023622046335, 0.09757992244046803654 ) ) ;
#74089 = CARTESIAN_POINT ( 'NONE',  ( -0.6102362204724400829, 0.1660481256975885056, 0.3530559997133364547 ) ) ;
#74090 = B_SPLINE_CURVE_WITH_KNOTS ( 'NONE', 3,
 ( #33433, #14506, #53179, #34262, #53599, #13661, #27523, #15328, #21215, #66672, #46870, #32586, #58249, #52348, #78477, #59094, #614, #72150, #19968, #45619, #71313, #26270, #72564, #52768, #8591, #2278, #39313, #46457, #33004, #40159, #78055, #66252, #46036, #59508, #8176, #71731, #33842, #14086 ),
 .UNSPECIFIED., .F., .F.,
 ( 4, 2, 2, 2, 2, 2, 2, 2, 2, 2, 2, 2, 2, 2, 2, 2, 2, 2, 4 ),
 ( 9.146428360655323264E-14, 0.003207193274670050703, 0.004810789911959344189, 0.006414386549248637243, 0.007216184867893282034, 0.008017983186537928561, 0.009621579823827219879, 0.01042337814247186814, 0.01122517646111651467, 0.01282877309840580599, 0.01363057141705045078, 0.01443236973569509730, 0.01603596637298438862, 0.01763956301027367821, 0.01924315964756296779, 0.02084675628485226778, 0.02245035292214156084, 0.02405394955943085736, 0.02565754619672015041 ),
 .UNSPECIFIED. ) ;
#74091 = DIRECTION ( 'NONE',  ( 0.000000000000000000, 0.000000000000000000, 1.000000000000000000 ) ) ;
#74092 = CARTESIAN_POINT ( 'NONE',  ( -1.043307086614172041, -0.5400638737290844871, 0.3530559997133364547 ) ) ;
#74093 = CARTESIAN_POINT ( 'NONE',  ( -0.1049643490035302024, -0.3917322834645671215, -1.416666666666666519 ) ) ;
#74094 = DIRECTION ( 'NONE',  ( 0.000000000000000000, 0.000000000000000000, 1.000000000000000000 ) ) ;
#74095 = CARTESIAN_POINT ( 'NONE',  ( 1.417322834645670104, -0.1870078740157480879, -0.4822834645669291653 ) ) ;
#74096 = CARTESIAN_POINT ( 'NONE',  ( 0.3740157480314966754, -0.5400638737290844871, 0.3530559997133364547 ) ) ;
#74097 = CARTESIAN_POINT ( 'NONE',  ( 0.2362204724409449064, 0.000000000000000000, 0.000000000000000000 ) ) ;
#74098 = CARTESIAN_POINT ( 'NONE',  ( 0.1070741851644054637, -0.3996062992125984925, -2.209317585301837639 ) ) ;
#74099 = CARTESIAN_POINT ( 'NONE',  ( -1.679790026246718693, 0.2306618581243847221, -0.2411417322834647770 ) ) ;
#74100 = CARTESIAN_POINT ( 'NONE',  ( 0.3996062992125986590, -0.1070741851644053111, -0.4265091863517060933 ) ) ;
#74101 = EDGE_LOOP ( 'NONE', ( #80526, #36736, #7533, #12114 ) ) ;
#74102 = CARTESIAN_POINT ( 'NONE',  ( -0.9842519685039360366, 0.1771653543307087630, 0.000000000000000000 ) ) ;
#74103 = CARTESIAN_POINT ( 'NONE',  ( 0.1958661417322834775, 0.3392501089628018884, -2.026246719160105236 ) ) ;
#74104 = ORIENTED_EDGE ( 'NONE', *, *, #66020, .T. ) ;
#74105 = CARTESIAN_POINT ( 'NONE',  ( 0.6167979002624678353, -0.4281496062992124485, 0.4176697321401328655 ) ) ;
#74106 = CARTESIAN_POINT ( 'NONE',  ( -0.4658792650918627265, -0.05778040916215522460, 0.4822834645669289988 ) ) ;
#74107 = CARTESIAN_POINT ( 'NONE',  ( -0.9580052493438311334, 0.05413385826771626580, -0.4176697321401330321 ) ) ;
#74108 = CARTESIAN_POINT ( 'NONE',  ( 1.220472440944882608, 0.2952755905511811885, 0.000000000000000000 ) ) ;
#74109 = CARTESIAN_POINT ( 'NONE',  ( -1.233595800524933894, -0.5023911411419708095, -0.1820866141732282451 ) ) ;
#74110 = DIRECTION ( 'NONE',  ( -3.491481338843132961E-15, -0.000000000000000000, 1.000000000000000000 ) ) ;
#74111 = CARTESIAN_POINT ( 'NONE',  ( 0.4790026246719168435, -0.3162353388693409650, -0.4822834645669289433 ) ) ;
#74112 = CARTESIAN_POINT ( 'NONE',  ( -0.8136482939632537770, 0.2306618581243847221, -0.2411417322834647770 ) ) ;
#74113 = CARTESIAN_POINT ( 'NONE',  ( -0.1049643490035301746, -0.3917322834645670659, -1.412054175031808967 ) ) ;
#74114 = CARTESIAN_POINT ( 'NONE',  ( -1.430446194225720724, 0.05413385826771626580, -0.4176697321401330321 ) ) ;
#74115 = CYLINDRICAL_SURFACE ( 'NONE', #45182, 0.2165354330708660069 ) ;
#74116 = CARTESIAN_POINT ( 'NONE',  ( 0.8005249343832028242, -0.4281496062992127816, -0.4176697321401328100 ) ) ;
#74117 = CARTESIAN_POINT ( 'NONE',  ( 0.3917322834645670104, -0.1049643490035303411, -2.873359580052493811 ) ) ;
#74118 = CARTESIAN_POINT ( 'NONE',  ( 1.476377952755906442, -0.4536011799217367080, 0.2665933059059888421 ) ) ;
#74119 = ORIENTED_EDGE ( 'NONE', *, *, #54784, .T. ) ;
#74120 = CARTESIAN_POINT ( 'NONE',  ( -0.3420746716998661618, 0.1974969037888702206, 0.1312335958005248771 ) ) ;
#74121 = CARTESIAN_POINT ( 'NONE',  ( -0.6036745406824141069, -0.6046776061558809534, -0.2411417322834644161 ) ) ;
#74122 = ORIENTED_EDGE ( 'NONE', *, *, #12573, .T. ) ;
#74123 = CARTESIAN_POINT ( 'NONE',  ( 0.5314960629921264834, 0.07958543189024071263, -0.2665933059059888421 ) ) ;
#74124 = CARTESIAN_POINT ( 'NONE',  ( -1.450131233595799651, -0.6692913385826771977, 0.1292274648535927661 ) ) ;
#74125 = CARTESIAN_POINT ( 'NONE',  ( 1.174540682414699111, -0.05778040916215560624, -0.4822834645669293319 ) ) ;
#74126 = CARTESIAN_POINT ( 'NONE',  ( 0.8070866141732288002, 0.1660481256975885056, 0.3530559997133364547 ) ) ;
#74127 =( BOUNDED_CURVE ( )  B_SPLINE_CURVE ( 2, ( #79576, #66943, #68182, #17258, #54281, #16015, #61437, #67352, #49208, #55106, #34946, #73248, #80410 ),
 .UNSPECIFIED., .F., .F. ) 
 B_SPLINE_CURVE_WITH_KNOTS ( ( 3, 2, 2, 2, 2, 2, 3 ),
 ( 0.7763059932978690902, 0.7765151515151516026, 0.7803030303030302761, 0.7840909090909091717, 0.7878787878787878451, 0.7916666666666667407, 0.7918758248839492531 ),
 .UNSPECIFIED. ) 
 CURVE ( )  GEOMETRIC_REPRESENTATION_ITEM ( )  RATIONAL_B_SPLINE_CURVE ( ( 0.9964447847208420805, 0.9981185001348091834, 1.000000000000000000, 0.9659258262890683122, 1.000000000000000000, 0.9659258262890683122, 1.000000000000000000, 0.9659258262890683122, 1.000000000000000000, 0.9659258262890683122, 1.000000000000000000, 0.9981185001348091834, 0.9964447847208420805 ) ) 
 REPRESENTATION_ITEM ( '' )  );
#74128 = CARTESIAN_POINT ( 'NONE',  ( 0.01968503937007930540, 0.1660481256975885056, 0.3530559997133364547 ) ) ;
#74129 = CARTESIAN_POINT ( 'NONE',  ( 0.1958661417322834775, 0.3392501089628018884, -1.085977321031183163 ) ) ;
#74130 = CARTESIAN_POINT ( 'NONE',  ( -0.8792650918635160906, -0.4281496062992124485, 0.4176697321401328655 ) ) ;
#74131 = CARTESIAN_POINT ( 'NONE',  ( 0.3917322834645670104, -0.1049643490035303411, -2.400918635170603554 ) ) ;
#74132 = CARTESIAN_POINT ( 'NONE',  ( -1.594488188976377563, -0.5400638737290844871, 0.3530559997133364547 ) ) ;
#74133 = CARTESIAN_POINT ( 'NONE',  ( -0.9908136482939626788, 0.2952755905511811885, 0.1292274648535926551 ) ) ;
#74134 = CARTESIAN_POINT ( 'NONE',  ( 1.502624671916010790, -0.05778040916215522460, 0.4822834645669289988 ) ) ;
#74135 = AXIS2_PLACEMENT_3D ( 'NONE', #4257, #74567, #48043 ) ;
#74136 = CARTESIAN_POINT ( 'NONE',  ( 1.686351706036745890, 0.2952755905511811885, 0.1292274648535926551 ) ) ;
#74137 = CARTESIAN_POINT ( 'NONE',  ( -0.7545931758530177724, 0.2952755905511811885, 0.1292274648535926551 ) ) ;
#74138 = CARTESIAN_POINT ( 'NONE',  ( -0.3996062992125985480, -7.340648628747423112E-17, 0.04133858267716534335 ) ) ;
#74139 = CARTESIAN_POINT ( 'NONE',  ( 0.4658792650918640033, -0.3162353388693405765, 0.4822834645669290543 ) ) ;
#74140 = CARTESIAN_POINT ( 'NONE',  ( -9.787531504996567848E-17, 0.3996062992125986035, -1.889763779527559251 ) ) ;
#74141 = CARTESIAN_POINT ( 'NONE',  ( -0.6299212598425188991, -0.1870078740157480879, -0.4822834645669291653 ) ) ;
#74142 = CARTESIAN_POINT ( 'NONE',  ( -1.404199475065615932, -0.3690944881889765550, -0.3153832671262227771 ) ) ;
#74143 = CARTESIAN_POINT ( 'NONE',  ( 0.6561679790026253567, -0.5023911411419708095, -0.1820866141732282451 ) ) ;
#74144 = CARTESIAN_POINT ( 'NONE',  ( 1.489501312335958172, -0.05778040916215560624, -0.4822834645669293319 ) ) ;
#74145 = CARTESIAN_POINT ( 'NONE',  ( -0.4724409448818898682, -8.678599364036362592E-17, -0.9035433070866141225 ) ) ;
#74146 = CARTESIAN_POINT ( 'NONE',  ( 0.7414698162729663755, 0.1771653543307087630, 0.09757992244046791164 ) ) ;
#74147 = CARTESIAN_POINT ( 'NONE',  ( 0.6036745406824153282, -0.6046776061558807314, 0.2411417322834647770 ) ) ;
#74148 = CARTESIAN_POINT ( 'NONE',  ( -0.3949938075777408852, -0.1058382717557502933, -0.7526246719160105680 ) ) ;
#74149 = CARTESIAN_POINT ( 'NONE',  ( -0.3805774278215216522, -0.4281496062992127816, -0.4176697321401328100 ) ) ;
#74150 = CARTESIAN_POINT ( 'NONE',  ( 0.5314960629921396951, 2.755905511811024056, -3.937007874015760578 ) ) ;
#74151 = CARTESIAN_POINT ( 'NONE',  ( 1.404199475065617264, -0.3690944881889763329, 0.3153832671262228327 ) ) ;
#74152 = CARTESIAN_POINT ( 'NONE',  ( -0.6955380577427815458, -0.4281496062992127816, -0.4176697321401328100 ) ) ;
#74153 = CARTESIAN_POINT ( 'NONE',  ( -0.3949938075777409963, -7.255918531996591613E-17, -0.2736220472440945017 ) ) ;
#74154 = CARTESIAN_POINT ( 'NONE',  ( 1.246719160104987623, 0.05413385826771626580, -0.4176697321401330321 ) ) ;
#74155 = CARTESIAN_POINT ( 'NONE',  ( 0.1574803149606306130, -0.1870078740157479769, 0.4822834645669291653 ) ) ;
#74156 = CARTESIAN_POINT ( 'NONE',  ( 0.7349081364829403995, 0.1283753931104748280, 0.1820866141732283561 ) ) ;
#74157 = CARTESIAN_POINT ( 'NONE',  ( 0.8533690079452093125, 0.004960608223778500969, -0.3437734562760191848 ) ) ;
#74158 = CARTESIAN_POINT ( 'NONE',  ( -0.1312335958005241554, -0.5023911411419708095, -0.1820866141732282451 ) ) ;
#74159 = CARTESIAN_POINT ( 'NONE',  ( 0.7349081364829402885, -0.5023911411419708095, -0.1820866141732282451 ) ) ;
#74160 = CARTESIAN_POINT ( 'NONE',  ( -1.535433070866141225, -0.6692913385826771977, 8.415575281601705876E-17 ) ) ;
#74161 = CARTESIAN_POINT ( 'NONE',  ( 0.1070741851644053388, 0.3996062992125986035, -1.330052493438320438 ) ) ;
#74162 = CARTESIAN_POINT ( 'NONE',  ( 0.8136482939632553313, -0.6046776061558809534, -0.2411417322834644161 ) ) ;
#74163 = EDGE_CURVE ( 'NONE', #62837, #52448, #38109, .T. ) ;
#74164 = CARTESIAN_POINT ( 'NONE',  ( 0.1958661417322836440, -0.3392501089628017219, -1.028871391076115360 ) ) ;
#74165 = CARTESIAN_POINT ( 'NONE',  ( 1.568241469816273659, -0.08942795157528024563, -0.3641732283464568787 ) ) ;
#74166 = CARTESIAN_POINT ( 'NONE',  ( 0.1458944486102289051, 0.02791078216816508459, -0.4328096321851889194 ) ) ;
#74167 = CARTESIAN_POINT ( 'NONE',  ( -0.1837270341207343505, -0.5023911411419708095, 0.1820866141732285504 ) ) ;
#74168 = CARTESIAN_POINT ( 'NONE',  ( 0.05905511811023709395, -0.5400638737290844871, 0.3530559997133364547 ) ) ;
#74169 = CARTESIAN_POINT ( 'NONE',  ( 1.568241469816273659, -0.08942795157528024563, -0.3641732283464568787 ) ) ;
#74170 = CARTESIAN_POINT ( 'NONE',  ( -1.200787401574802349, 0.07958543189024071263, -0.2665933059059888421 ) ) ;
#74171 = CARTESIAN_POINT ( 'NONE',  ( -1.561679790026246017, 0.05413385826771666132, 0.4176697321401328100 ) ) ;
#74172 = CONICAL_SURFACE ( 'NONE', #9637, 2.637795275590551380, 0.7853981633974500554 ) ;
#74173 = CARTESIAN_POINT ( 'NONE',  ( 0.4133858267716541968, 0.1660481256975885056, 0.3530559997133364547 ) ) ;
#74174 = CARTESIAN_POINT ( 'NONE',  ( 1.187664041994751285, -0.05778040916215522460, 0.4822834645669289988 ) ) ;
#74175 = DIRECTION ( 'NONE',  ( -0.000000000000000000, 0.8660254037844387076, 0.4999999999999998890 ) ) ;
#74176 = CARTESIAN_POINT ( 'NONE',  ( -0.006561679790025524116, -0.3162353388693405765, 0.4822834645669290543 ) ) ;
#74177 = CARTESIAN_POINT ( 'NONE',  ( 1.456692913385827515, -0.6692913385826771977, 8.415575281601705876E-17 ) ) ;
#74178 = CARTESIAN_POINT ( 'NONE',  ( 0.9711286089238851948, -0.6046776061558809534, -0.2411417322834644161 ) ) ;
#74179 = DIRECTION ( 'NONE',  ( -1.000000000000000000, -0.000000000000000000, -0.000000000000000000 ) ) ;
#74180 = CARTESIAN_POINT ( 'NONE',  ( 0.9776902887139113929, -0.5511811023622048555, -0.09757992244046775898 ) ) ;
#74181 = CARTESIAN_POINT ( 'NONE',  ( 1.646981627296588035, -0.3162353388693405765, 0.4822834645669290543 ) ) ;
#74182 = CARTESIAN_POINT ( 'NONE',  ( 0.03937007874015806264, 0.1771653543307087630, 0.000000000000000000 ) ) ;
#74183 = CARTESIAN_POINT ( 'NONE',  ( 0.1509186351706045259, -0.05778040916215560624, -0.4822834645669293319 ) ) ;
#74184 = CARTESIAN_POINT ( 'NONE',  ( 0.8267716535433077274, 0.2952755905511811885, 0.000000000000000000 ) ) ;
#74185 = CARTESIAN_POINT ( 'NONE',  ( -0.4133858267716528645, -0.5400638737290844871, 0.3530559997133364547 ) ) ;
#74186 = ADVANCED_FACE ( 'NONE', ( #71365 ), #12052, .T. ) ;
#74187 = CARTESIAN_POINT ( 'NONE',  ( -0.1902887139107604098, -0.5511811023622046335, 0.09757992244046803654 ) ) ;
#74188 = CARTESIAN_POINT ( 'NONE',  ( 0.6561679790026253567, 0.2306618581243848609, 0.2411417322834645549 ) ) ;
#74189 = CARTESIAN_POINT ( 'NONE',  ( 0.7677165354330716118, 0.07958543189024071263, -0.2665933059059888421 ) ) ;
#74190 = DIRECTION ( 'NONE',  ( 8.462065736472231082E-17, -1.000000000000000000, 0.000000000000000000 ) ) ;
#74192 = FACE_OUTER_BOUND ( 'NONE', #39829, .T. ) ;
#74191 = CARTESIAN_POINT ( 'NONE',  ( -1.056430446194224881, 0.2952755905511810219, -0.1292274648535930437 ) ) ;
#74193 = CARTESIAN_POINT ( 'NONE',  ( -0.1875998866324375958, 1.067055059779716597, 0.2508381535278075281 ) ) ;
#74194 = CARTESIAN_POINT ( 'NONE',  ( -1.318897637795274802, 0.1660481256975885056, 0.3530559997133364547 ) ) ;
#74195 = CARTESIAN_POINT ( 'NONE',  ( -0.3346456692913377662, -0.5400638737290844871, 0.3530559997133364547 ) ) ;
#74196 = CARTESIAN_POINT ( 'NONE',  ( 0.4091458600556404646, -0.2362204724409448231, -0.1049868766404199460 ) ) ;
#74197 = CARTESIAN_POINT ( 'NONE',  ( 4.837279021331060870E-17, -0.3949938075777409963, -2.440944881889763884 ) ) ;
#74198 = ORIENTED_EDGE ( 'NONE', *, *, #47097, .T. ) ;
#74199 = CARTESIAN_POINT ( 'NONE',  ( 0.5905511811023629321, 0.1771653543307087630, 0.000000000000000000 ) ) ;
#74200 = CARTESIAN_POINT ( 'NONE',  ( 0.2867679344610365999, -0.2867679344610365444, -1.035433070866141447 ) ) ;
#74201 = CARTESIAN_POINT ( 'NONE',  ( 1.286089238845145033, 0.2306618581243848609, 0.2411417322834645549 ) ) ;
#74202 = CARTESIAN_POINT ( 'NONE',  ( -0.1265901696524986964, -0.4724409448818899238, -2.434383202099737353 ) ) ;
#74203 = CARTESIAN_POINT ( 'NONE',  ( 0.4935044252197980930, 1.488513638086841118, 0.5309055118110234117 ) ) ;
#74204 = CARTESIAN_POINT ( 'NONE',  ( -1.482939632545930975, -0.3690944881889765550, -0.3153832671262227771 ) ) ;
#74205 = CARTESIAN_POINT ( 'NONE',  ( 1.633858267716535639, -0.5400638737290844871, 0.3530559997133364547 ) ) ;
#74206 = CARTESIAN_POINT ( 'NONE',  ( 1.443569553805774897, 0.1283753931104748280, 0.1820866141732283561 ) ) ;
#74207 = CARTESIAN_POINT ( 'NONE',  ( 0.5708661417322842269, 0.1660481256975885056, 0.3530559997133364547 ) ) ;
#74208 = B_SPLINE_CURVE_WITH_KNOTS ( 'NONE', 3,
 ( #23321, #17035, #81419, #72306, #2011, #15061, #14653, #68373, #55299, #65989, #8327, #33993, #59655, #40717, #27674, #53340, #21367, #66402 ),
 .UNSPECIFIED., .F., .F.,
 ( 4, 2, 2, 2, 2, 2, 2, 2, 4 ),
 ( 0.001226984380451624388, 0.003469327704077891823, 0.004590499365891025432, 0.005151085196797592670, 0.005711671027704158174, 0.006272256858610725412, 0.006832842689517291783, 0.007954014351330434066, 0.01019635767495674639 ),
 .UNSPECIFIED. ) ;
#74209 = CARTESIAN_POINT ( 'NONE',  ( -0.2867679344610366554, 0.2867679344610365444, -0.4146788469478197015 ) ) ;
#74210 = CARTESIAN_POINT ( 'NONE',  ( 0.09186351706036827158, 0.05413385826771666132, 0.4176697321401328100 ) ) ;
#74211 = CARTESIAN_POINT ( 'NONE',  ( -1.003937007874015297, -0.4536011799217368745, -0.2665933059059886201 ) ) ;
#74212 = ADVANCED_FACE ( 'NONE', ( #51147 ), #19175, .T. ) ;
#74213 = CARTESIAN_POINT ( 'NONE',  ( 0.3280839895013130669, 0.05413385826771666132, 0.4176697321401328100 ) ) ;
#74214 = CARTESIAN_POINT ( 'NONE',  ( -0.1640419947506555343, -0.3162353388693405765, 0.4822834645669290543 ) ) ;
#74215 = CARTESIAN_POINT ( 'NONE',  ( 0.5380577427821529035, 0.05413385826771626580, -0.4176697321401330321 ) ) ;
#74216 = CARTESIAN_POINT ( 'NONE',  ( -0.01000891935578489267, 8.471767977567108961E-16, -0.4445507791589058955 ) ) ;
#74217 = CARTESIAN_POINT ( 'NONE',  ( -0.3917322834645670659, -7.196005306013484475E-17, -1.453431389272652696 ) ) ;
#74218 = CARTESIAN_POINT ( 'NONE',  ( 0.9448818897637802916, -0.1870078740157480879, -0.4822834645669291653 ) ) ;
#74219 = CARTESIAN_POINT ( 'NONE',  ( -0.3018372703412066094, 0.05413385826771666132, 0.4176697321401328100 ) ) ;
#74220 = CARTESIAN_POINT ( 'NONE',  ( -1.056430446194224881, -0.6692913385826771977, 0.1292274648535927661 ) ) ;
#74221 = CARTESIAN_POINT ( 'NONE',  ( 1.227034120734908917, -0.6692913385826771977, 0.1292274648535927661 ) ) ;
#74222 = CARTESIAN_POINT ( 'NONE',  ( 0.5577427821522316087, -0.05778040916215522460, 0.4822834645669289988 ) ) ;
#74223 = CARTESIAN_POINT ( 'NONE',  ( 0.1049643490035304938, -0.3917322834645669549, -0.9573490813648293241 ) ) ;
#74224 = CARTESIAN_POINT ( 'NONE',  ( -0.1902887139107604098, -0.6692913385826771977, 0.1292274648535927661 ) ) ;
#74225 = CARTESIAN_POINT ( 'NONE',  ( 0.2821522309711292364, 0.2952755905511810774, -0.1292274648535930714 ) ) ;
#74226 = CARTESIAN_POINT ( 'NONE',  ( -0.6561679790026240244, 0.2306618581243847221, -0.2411417322834647770 ) ) ;
#74227 = CARTESIAN_POINT ( 'NONE',  ( 0.8858267716535438430, 0.07958543189024085140, 0.2665933059059887866 ) ) ;
#74228 = CARTESIAN_POINT ( 'NONE',  ( -1.614173228346456268, -0.6692913385826771977, 8.415575281601705876E-17 ) ) ;
#74229 = CARTESIAN_POINT ( 'NONE',  ( -0.3230994083235659842, 1.189706270649608655, -2.759390867997893348 ) ) ;
#74230 = CARTESIAN_POINT ( 'NONE',  ( 0.3805774278215230400, 0.05413385826771626580, -0.4176697321401330321 ) ) ;
#74231 = CIRCLE ( 'NONE', #79587, 0.1190944881889763746 ) ;
#74232 = CARTESIAN_POINT ( 'NONE',  ( 1.374111565972423831E-16, 0.000000000000000000, -1.122047244094488194 ) ) ;
#74233 = CARTESIAN_POINT ( 'NONE',  ( -0.3917322834645671215, 0.1049643490035301469, -2.544619422572177658 ) ) ;
#74234 = VERTEX_POINT ( 'NONE', #44014 ) ;
#74235 = ORIENTED_EDGE ( 'NONE', *, *, #14670, .T. ) ;
#74236 = CARTESIAN_POINT ( 'NONE',  ( 0.7808398950131241190, -0.05778040916215560624, -0.4822834645669293319 ) ) ;
#74237 = CARTESIAN_POINT ( 'NONE',  ( 0.5118110236220478892, 0.1771653543307087630, 0.000000000000000000 ) ) ;
#74239 = FACE_OUTER_BOUND ( 'NONE', #48640, .T. ) ;
#74238 = DIRECTION ( 'NONE',  ( 0.000000000000000000, -1.000000000000000000, 0.000000000000000000 ) ) ;
#74240 = CARTESIAN_POINT ( 'NONE',  ( 0.3392501089628018884, -0.1958661417322834220, -0.6620734908136483021 ) ) ;
#74241 = CARTESIAN_POINT ( 'NONE',  ( -0.4614848114146354319, 1.648560354533844308, 3.909868722774259453 ) ) ;
#74242 = CARTESIAN_POINT ( 'NONE',  ( 0.3963884504522703911, 0.02578378529929774635, -1.929133858267716883 ) ) ;
#74243 = CARTESIAN_POINT ( 'NONE',  ( 0.1049643490035303689, 0.3917322834645670104, -1.495406824146981117 ) ) ;
#74244 = CARTESIAN_POINT ( 'NONE',  ( -0.1998031496062994405, 0.3460692066303957537, -2.609580052493438274 ) ) ;
#74245 = CARTESIAN_POINT ( 'NONE',  ( 1.017060367454068581, -0.05778040916215560624, -0.4822834645669293319 ) ) ;
#74246 = CARTESIAN_POINT ( 'NONE',  ( -0.6955380577427815458, 0.05413385826771666132, 0.4176697321401328100 ) ) ;
#74247 = CARTESIAN_POINT ( 'NONE',  ( -0.6692913385826764205, -0.6692913385826771977, 8.415575281601705876E-17 ) ) ;
#74248 = CARTESIAN_POINT ( 'NONE',  ( 0.8070866141732288002, 0.1660481256975885056, 0.3530559997133364547 ) ) ;
#74249 = CARTESIAN_POINT ( 'NONE',  ( 1.377952755905512472, -0.6692913385826771977, 8.415575281601705876E-17 ) ) ;
#74250 = CARTESIAN_POINT ( 'NONE',  ( -1.067249829279471429, 1.213052584328227157, 0.3465489493959020839 ) ) ;
#74251 = CONTEXT_DEPENDENT_SHAPE_REPRESENTATION ( #42782, #7686 ) ;
#74252 = CARTESIAN_POINT ( 'NONE',  ( 1.312335958005250269, -0.5023911411419708095, 0.1820866141732285504 ) ) ;
#74253 = CARTESIAN_POINT ( 'NONE',  ( -0.1998031496062994405, 0.3460692066303957537, -1.979658792650918597 ) ) ;
#74254 = CARTESIAN_POINT ( 'NONE',  ( -1.207349081364828436, -0.5023911411419708095, 0.1820866141732285504 ) ) ;
#74255 =( BOUNDED_CURVE ( )  B_SPLINE_CURVE ( 1, ( #35165, #35994 ),
 .UNSPECIFIED., .F., .F. ) 
 B_SPLINE_CURVE_WITH_KNOTS ( ( 2, 2 ),
 ( 3.469446951953614189E-18, 0.002000000000000005246 ),
 .UNSPECIFIED. ) 
 CURVE ( )  GEOMETRIC_REPRESENTATION_ITEM ( )  RATIONAL_B_SPLINE_CURVE ( ( 0.9875488213027523443, 0.9875488213027523443 ) ) 
 REPRESENTATION_ITEM ( '' )  );
#74256 = CARTESIAN_POINT ( 'NONE',  ( -0.3149606299212733274, 2.165354330708661568, 3.924389226575467404 ) ) ;
#74257 = CARTESIAN_POINT ( 'NONE',  ( -0.01312335958005186876, 0.05413385826771626580, -0.4176697321401330321 ) ) ;
#74259 = PLANE ( 'NONE',  #38526 ) ;
#74258 = LINE ( 'NONE', #16599, #69138 ) ;
#74260 = CARTESIAN_POINT ( 'NONE',  ( -0.9842519685039365918, -0.5511811023622047445, 6.969142054262312111E-17 ) ) ;
#74261 = CARTESIAN_POINT ( 'NONE',  ( 0.2099737532808405305, -0.6046776061558807314, 0.2411417322834647770 ) ) ;
#74262 = CARTESIAN_POINT ( 'NONE',  ( 1.115485564304462551, -0.004921259842519576551, 0.3153832671262227771 ) ) ;
#74263 = CARTESIAN_POINT ( 'NONE',  ( -0.1049643490035306742, 0.3917322834645668994, -1.503917692092176628 ) ) ;
#74264 = CARTESIAN_POINT ( 'NONE',  ( -1.128608923884513837, -0.5023911411419708095, 0.1820866141732285504 ) ) ;
#74265 = CARTESIAN_POINT ( 'NONE',  ( 1.371391076115485941, 0.2952755905511811885, 0.1292274648535926551 ) ) ;
#74266 = CARTESIAN_POINT ( 'NONE',  ( 0.06306398308594768354, 1.952040271819099004, 0.3069791477017838055 ) ) ;
#74267 = CARTESIAN_POINT ( 'NONE',  ( -0.3215223097112853146, -0.3162353388693405765, 0.4822834645669290543 ) ) ;
#74268 = CARTESIAN_POINT ( 'NONE',  ( -1.384514435695537005, -0.5511811023622048555, -0.09757992244046775898 ) ) ;
#74269 = CARTESIAN_POINT ( 'NONE',  ( -0.5577427821522301654, -0.05778040916215560624, -0.4822834645669293319 ) ) ;
#74270 = CARTESIAN_POINT ( 'NONE',  ( 1.666666666666667185, 0.05413385826771666132, 0.4176697321401328100 ) ) ;
#74271 = CARTESIAN_POINT ( 'NONE',  ( 0.3392501089628018329, 0.1958661417322835607, -0.6004130165692406207 ) ) ;
#74272 = CARTESIAN_POINT ( 'NONE',  ( 0.4724409448818904789, -0.1870078740157479769, 0.4822834645669291653 ) ) ;
#74273 = CARTESIAN_POINT ( 'NONE',  ( 0.3808816823641231752, -0.09156050430092187165, -1.929133858267716661 ) ) ;
#74274 = CARTESIAN_POINT ( 'NONE',  ( 1.227034120734908917, -0.6692913385826771977, 0.1292274648535927661 ) ) ;
#74275 = CARTESIAN_POINT ( 'NONE',  ( -0.1265901696524993347, 0.4724409448818895907, -2.130577427821522374 ) ) ;
#74276 = CARTESIAN_POINT ( 'NONE',  ( -1.148293963254592542, -0.6692913385826773087, -0.1292274648535924053 ) ) ;
#74277 = CARTESIAN_POINT ( 'NONE',  ( -0.7480314960629914633, 0.1771653543307087630, 0.000000000000000000 ) ) ;
#74278 = CARTESIAN_POINT ( 'NONE',  ( 0.7974104941589355011, -4.927456884911482678E-16, 0.4445507791589062840 ) ) ;
#74279 = CARTESIAN_POINT ( 'NONE',  ( -0.1771653543307080136, 0.1660481256975883668, -0.3530559997133364547 ) ) ;
#74280 = CARTESIAN_POINT ( 'NONE',  ( 0.2230971128608932319, -0.3690944881889763329, 0.3153832671262228327 ) ) ;
#74281 = CARTESIAN_POINT ( 'NONE',  ( -1.023622047244094002, -0.1870078740157480601, -0.3641732283464567677 ) ) ;
#74282 = CARTESIAN_POINT ( 'NONE',  ( -1.450131233595799651, -0.6692913385826771977, 0.1292274648535927661 ) ) ;
#74283 = CARTESIAN_POINT ( 'NONE',  ( -1.574803149606298636, -0.1870078740157479769, 0.4822834645669291653 ) ) ;
#74284 = CARTESIAN_POINT ( 'NONE',  ( 1.574803149606299746, -0.1870078740157480879, -0.4822834645669291653 ) ) ;
#74285 = CARTESIAN_POINT ( 'NONE',  ( 0.03430998917087475092, 1.064156075168071869, 1.851472435485761237 ) ) ;
#74286 = CARTESIAN_POINT ( 'NONE',  ( 0.6036745406824154392, 0.1283753931104746893, -0.1820866141732285504 ) ) ;
#74287 = CARTESIAN_POINT ( 'NONE',  ( 0.8530183727034128527, -0.4281496062992124485, 0.4176697321401328655 ) ) ;
#74288 = CARTESIAN_POINT ( 'NONE',  ( -0.08874907683609993547, 8.471767977567108961E-16, -0.4445507791589058955 ) ) ;
#74289 = CARTESIAN_POINT ( 'NONE',  ( 1.279527559055118724, 0.07958543189024085140, 0.2665933059059887866 ) ) ;
#74290 = ORIENTED_EDGE ( 'NONE', *, *, #8460, .T. ) ;
#74291 = CARTESIAN_POINT ( 'NONE',  ( -1.259842519685038686, -0.1870078740157480879, -0.4822834645669291653 ) ) ;
#74292 = CARTESIAN_POINT ( 'NONE',  ( -0.8070866141732276899, 0.1660481256975883668, -0.3530559997133364547 ) ) ;
#74293 = CARTESIAN_POINT ( 'NONE',  ( 0.1771653543307093182, 0.1660481256975885056, 0.3530559997133364547 ) ) ;
#74294 = CARTESIAN_POINT ( 'NONE',  ( -1.732283464566928277, -0.1870078740157479769, 0.3641732283464567677 ) ) ;
#74295 = CARTESIAN_POINT ( 'NONE',  ( -0.3460692066303957537, -0.1998031496062994405, -2.176509186351706315 ) ) ;
#74296 = CARTESIAN_POINT ( 'NONE',  ( 0.8661417322834652488, -0.1870078740157480879, -0.4822834645669291653 ) ) ;
#74297 = CARTESIAN_POINT ( 'NONE',  ( -1.640419947506561060, -0.4281496062992127816, -0.4176697321401328100 ) ) ;
#74298 = CARTESIAN_POINT ( 'NONE',  ( 0.01968503937007957949, -0.5400638737290845981, -0.3530559997133363437 ) ) ;
#74299 = CARTESIAN_POINT ( 'NONE',  ( 0.5839895013123367340, -0.6692913385826773087, -0.1292274648535924053 ) ) ;
#74300 = CARTESIAN_POINT ( 'NONE',  ( -9.787531504996567848E-17, 0.3996062992125986035, -1.574803149606299302 ) ) ;
#74301 = CARTESIAN_POINT ( 'NONE',  ( -9.674558042662121740E-17, 0.3949938075777409963, -1.259842519685039353 ) ) ;
#74302 = CARTESIAN_POINT ( 'NONE',  ( -0.2925321140481930704, -0.2925321140481933480, -2.421259842519684735 ) ) ;
#74303 = CARTESIAN_POINT ( 'NONE',  ( -1.595398199321656829, 1.013096522517431097, -0.1559797534342478031 ) ) ;
#74304 = CARTESIAN_POINT ( 'NONE',  ( -0.3392501089628019995, 0.1958661417322832277, -0.01837270341207344546 ) ) ;
#74305 = CARTESIAN_POINT ( 'NONE',  ( -0.1574803149606292529, -0.1870078740157479769, 0.3641732283464567677 ) ) ;
#74306 = CARTESIAN_POINT ( 'NONE',  ( -0.6561679790026240244, -0.6046776061558807314, 0.2411417322834647770 ) ) ;
#74307 = CARTESIAN_POINT ( 'NONE',  ( 0.9448818897637802916, -0.1870078740157479769, 0.4822834645669291653 ) ) ;
#74308 = CARTESIAN_POINT ( 'NONE',  ( -0.2891555358219909388, -0.2891555358219912164, -2.183070866141731958 ) ) ;
#74309 = CARTESIAN_POINT ( 'NONE',  ( 0.08530183727034192087, -0.08942795157527998196, 0.3641732283464567121 ) ) ;
#74310 = CARTESIAN_POINT ( 'NONE',  ( -1.194225721784776262, -0.4281496062992124485, 0.4176697321401328655 ) ) ;
#74311 = CARTESIAN_POINT ( 'NONE',  ( 1.194225721784777594, -0.4281496062992127816, -0.4176697321401328100 ) ) ;
#74312 = CARTESIAN_POINT ( 'NONE',  ( -0.3458507752293906723, -0.3458507752293910609, -2.263779527559055094 ) ) ;
#74313 = CARTESIAN_POINT ( 'NONE',  ( -0.1998031496062991907, -0.3460692066303959757, -1.955380577427821454 ) ) ;
#74314 = DIRECTION ( 'NONE',  ( 1.000000000000000000, 0.000000000000000000, 0.000000000000000000 ) ) ;
#74315 = EDGE_CURVE ( 'NONE', #11477, #70359, #23232, .T. ) ;
#74316 = EDGE_LOOP ( 'NONE', ( #59194, #48916, #65899, #65303, #4613, #15754, #65517, #79932, #10860, #43840, #16218, #79930, #61559, #47598 ) ) ;
#74317 = CARTESIAN_POINT ( 'NONE',  ( 0.8005249343832027131, 0.05413385826771666132, 0.4176697321401328100 ) ) ;
#74318 = CARTESIAN_POINT ( 'NONE',  ( 1.213910761154856299, -0.5511811023622048555, -0.09757992244046775898 ) ) ;
#74320 = CARTESIAN_POINT ( 'NONE',  ( -1.502624671916009680, -0.3162353388693405765, 0.4822834645669290543 ) ) ;
#74319 = CARTESIAN_POINT ( 'NONE',  ( -1.482939632545930975, -0.004921259842519576551, 0.3153832671262227771 ) ) ;
#74321 = CARTESIAN_POINT ( 'NONE',  ( 0.3917322834645670104, -0.1049643490035303411, 0.1187664041994749703 ) ) ;
#74322 = CARTESIAN_POINT ( 'NONE',  ( 0.3149606299212737159, 2.165354330708661568, -3.937007874015761022 ) ) ;
#74323 = CARTESIAN_POINT ( 'NONE',  ( 1.200787401574803681, 0.1660481256975885056, 0.3530559997133364547 ) ) ;
#74324 = CARTESIAN_POINT ( 'NONE',  ( -0.1265901696524986964, -0.4724409448818899238, -2.434383202099737353 ) ) ;
#74325 = CARTESIAN_POINT ( 'NONE',  ( -0.6036745406824141069, 0.2306618581243848609, 0.2411417322834645549 ) ) ;
#74326 = CARTESIAN_POINT ( 'NONE',  ( -0.5249343832020990641, -0.6046776061558809534, -0.2411417322834644161 ) ) ;
#74327 = CARTESIAN_POINT ( 'NONE',  ( 1.555118110236221041, -0.5400638737290844871, 0.3530559997133364547 ) ) ;
#74328 = CARTESIAN_POINT ( 'NONE',  ( 0.1049643490035303689, 0.3917322834645670104, -0.2355643044619422921 ) ) ;
#74329 = CARTESIAN_POINT ( 'NONE',  ( 0.08530183727034192087, -0.3162353388693409650, -0.4822834645669289433 ) ) ;
#74330 = CARTESIAN_POINT ( 'NONE',  ( -0.2867679344610364334, -0.2867679344610367109, -2.255905511811023612 ) ) ;
#74331 = CARTESIAN_POINT ( 'NONE',  ( -1.568241469816272105, -0.2845877964562161244, -0.3641732283464567121 ) ) ;
#74332 = VERTEX_POINT ( 'NONE', #62980 ) ;
#74333 = CARTESIAN_POINT ( 'NONE',  ( -0.2891555358219908833, -0.2891555358219912164, -2.578740157480315265 ) ) ;
#74334 = ORIENTED_EDGE ( 'NONE', *, *, #37360, .F. ) ;
#74335 = CARTESIAN_POINT ( 'NONE',  ( -0.01241954290193713825, 2.784432375088962958E-17, -0.3464511005275205946 ) ) ;
#74336 = CARTESIAN_POINT ( 'NONE',  ( -1.732283464566928277, -0.1870078740157479769, 0.4822834645669291653 ) ) ;
#74337 = CARTESIAN_POINT ( 'NONE',  ( 4.893765752498283924E-17, -0.3996062992125986035, -1.181102362204724310 ) ) ;
#74338 = CARTESIAN_POINT ( 'NONE',  ( 1.666666666666667185, -0.004921259842519576551, 0.3153832671262227771 ) ) ;
#74339 = DIRECTION ( 'NONE',  ( -1.000000000000000000, -0.000000000000000000, -0.000000000000000000 ) ) ;
#74340 = DIRECTION ( 'NONE',  ( 0.000000000000000000, 1.000000000000000000, 0.000000000000000000 ) ) ;
#74341 = CARTESIAN_POINT ( 'NONE',  ( -0.3477690288713902178, 0.2952755905511810219, -0.1292274648535930437 ) ) ;
#74342 = EDGE_CURVE ( 'NONE', #21745, #62598, #38119, .T. ) ;
#74343 = CARTESIAN_POINT ( 'NONE',  ( -0.3917322834645669549, -0.1049643490035306603, 0.02690288713910752097 ) ) ;
#74344 = AXIS2_PLACEMENT_3D ( 'NONE', #9068, #34739, #22100 ) ;
#74345 = CARTESIAN_POINT ( 'NONE',  ( -0.5052493438320203589, 0.1771653543307087075, -0.09757992244046823083 ) ) ;
#74346 = CARTESIAN_POINT ( 'NONE',  ( -1.010498687664041384, -0.3690944881889765550, -0.3153832671262227771 ) ) ;
#74347 = CARTESIAN_POINT ( 'NONE',  ( 1.489501312335958172, -0.05778040916215560624, -0.4822834645669293319 ) ) ;
#74348 = ADVANCED_FACE ( 'NONE', ( #5718 ), #72989, .F. ) ;
#74349 = CARTESIAN_POINT ( 'NONE',  ( 0.4724409448818904789, -0.1870078740157479769, 0.4822834645669291653 ) ) ;
#74350 = CARTESIAN_POINT ( 'NONE',  ( -1.187664041994749731, -0.3162353388693405765, 0.4822834645669290543 ) ) ;
#74351 = CARTESIAN_POINT ( 'NONE',  ( -0.3917322834645669549, -0.1049643490035306603, -0.1955380577427821009 ) ) ;
#74352 = ORIENTED_EDGE ( 'NONE', *, *, #3797, .F. ) ;
#74353 = CARTESIAN_POINT ( 'NONE',  ( -1.246719160104985846, -0.4281496062992127816, -0.4176697321401328100 ) ) ;
#74354 = FACE_OUTER_BOUND ( 'NONE', #61676, .T. ) ;
#74355 = SHAPE_REPRESENTATION_RELATIONSHIP ( 'NONE' , 'NONE' ,  #33107, #79614 ) ;
#74356 = CARTESIAN_POINT ( 'NONE',  ( 0.4091458600556403535, 0.2362204724409449896, -1.706036745406824151 ) ) ;
#74357 = CARTESIAN_POINT ( 'NONE',  ( 0.2035438835850314487, 0.2140388612101737920, 0.1320934087364891707 ) ) ;
#74358 = CARTESIAN_POINT ( 'NONE',  ( 0.3392501089628018329, 0.1958661417322835607, -0.5958005249343831800 ) ) ;
#74359 = DIRECTION ( 'NONE',  ( 1.000000000000000000, -0.000000000000000000, -1.692413147294445970E-16 ) ) ;
#74360 = CARTESIAN_POINT ( 'NONE',  ( -0.5839895013123351797, -0.6692913385826771977, 0.1292274648535927661 ) ) ;
#74361 = CARTESIAN_POINT ( 'NONE',  ( 1.541994750656168645, 0.2952755905511810774, -0.1292274648535930714 ) ) ;
#74363 = CARTESIAN_POINT ( 'NONE',  ( 0.1265901696524990572, -0.4724409448818897017, -1.975065616797900159 ) ) ;
#74362 = CARTESIAN_POINT ( 'NONE',  ( -1.587926509186350810, -0.4281496062992124485, 0.4176697321401328655 ) ) ;
#74364 = LINE ( 'NONE', #11625, #7444 ) ;
#74365 = CARTESIAN_POINT ( 'NONE',  ( -0.9514435695538050464, -0.3162353388693405765, 0.4822834645669290543 ) ) ;
#74366 = CARTESIAN_POINT ( 'NONE',  ( 0.3917322834645668994, -0.1049643490035303134, 0.1233788958343325359 ) ) ;
#74367 = CARTESIAN_POINT ( 'NONE',  ( -0.1049868766404193215, 0.1283753931104746893, -0.1820866141732285504 ) ) ;
#74368 = CARTESIAN_POINT ( 'NONE',  ( 0.1958661417322834775, 0.3392501089628018884, -0.2290026246719160941 ) ) ;
#74369 = CARTESIAN_POINT ( 'NONE',  ( -0.2887139107611542133, -0.5023911411419708095, -0.1820866141732282451 ) ) ;
#74370 = CARTESIAN_POINT ( 'NONE',  ( 1.023622047244095112, -0.1870078740157480601, -0.3641732283464567677 ) ) ;
#74371 = CARTESIAN_POINT ( 'NONE',  ( 0.7217847769028878924, -0.4281496062992127816, -0.4176697321401328100 ) ) ;
#74372 = CARTESIAN_POINT ( 'NONE',  ( -0.4133858267716528645, -0.4536011799217367080, 0.2665933059059888421 ) ) ;
#74373 = CARTESIAN_POINT ( 'NONE',  ( 0.3392501089628018329, 0.1958661417322835607, -2.485564304461941987 ) ) ;
#74374 = CARTESIAN_POINT ( 'NONE',  ( 1.548556430446194954, -0.6046776061558807314, 0.2411417322834647770 ) ) ;
#74375 = EDGE_CURVE ( 'NONE', #59008, #80968, #66311, .T. ) ;
#74376 = CARTESIAN_POINT ( 'NONE',  ( -0.9776902887139098386, 0.2952755905511810774, -0.1292274648535930714 ) ) ;
#74377 = CARTESIAN_POINT ( 'NONE',  ( 0.4724409448818898682, 2.892866454678787531E-17, -0.8248031496062991907 ) ) ;
#74378 = CARTESIAN_POINT ( 'NONE',  ( 0.1509186351706042484, -0.3162353388693405765, 0.4822834645669290543 ) ) ;
#74379 = CARTESIAN_POINT ( 'NONE',  ( -0.6233595800524928121, -0.3162353388693409650, -0.4822834645669289433 ) ) ;
#74380 = CARTESIAN_POINT ( 'NONE',  ( -2.570293878819217337, 2.742780005561834322, 0.5314960629921260393 ) ) ;
#74381 = EDGE_CURVE ( 'NONE', #69946, #2588, #77688, .T. ) ;
#74382 = CARTESIAN_POINT ( 'NONE',  ( -0.01312335958005186876, -0.3690944881889763329, 0.3153832671262228327 ) ) ;
#74383 = CARTESIAN_POINT ( 'NONE',  ( -0.3805774278215216522, -0.4281496062992127816, -0.4176697321401328100 ) ) ;
#74384 = CARTESIAN_POINT ( 'NONE',  ( -0.6430446194225712953, 0.05413385826771626580, -0.4176697321401330321 ) ) ;
#74385 = PLANE ( 'NONE',  #54636 ) ;
#74386 = AXIS2_PLACEMENT_3D ( 'NONE', #26743, #66727, #40622 ) ;
#74387 = CARTESIAN_POINT ( 'NONE',  ( 0.1706036745406830368, -0.4281496062992127816, -0.4176697321401328100 ) ) ;
#74388 = CARTESIAN_POINT ( 'NONE',  ( -0.3460692066303957537, -0.1998031496062994405, -2.176509186351706315 ) ) ;
#74389 = ADVANCED_FACE ( 'NONE', ( #70951 ), #34002, .F. ) ;
#74390 = CARTESIAN_POINT ( 'NONE',  ( 1.456692913385827515, 0.2952755905511811885, 0.000000000000000000 ) ) ;
#74391 = CARTESIAN_POINT ( 'NONE',  ( -0.6430446194225716283, -0.3690944881889763329, 0.3153832671262228327 ) ) ;
#74392 = CARTESIAN_POINT ( 'NONE',  ( -0.5774278215223089816, 0.2306618581243847221, -0.2411417322834647770 ) ) ;
#74393 = CARTESIAN_POINT ( 'NONE',  ( 1.594488188976378673, -0.5400638737290845981, -0.3530559997133363437 ) ) ;
#74394 = CARTESIAN_POINT ( 'NONE',  ( 1.437007874015748810, -0.5400638737290845981, -0.3530559997133363437 ) ) ;
#74395 = CARTESIAN_POINT ( 'NONE',  ( -1.555118110236219930, -0.5400638737290845981, -0.3530559997133363437 ) ) ;
#74396 = CARTESIAN_POINT ( 'NONE',  ( -0.8792650918635160906, -0.004921259842519870586, -0.3153832671262229437 ) ) ;
#74397 = CARTESIAN_POINT ( 'NONE',  ( 0.2925321140481931814, 0.2925321140481931814, -0.2145669291338582751 ) ) ;
#74398 = CARTESIAN_POINT ( 'NONE',  ( -0.1070741851644056997, 0.3996062992125986035, -0.4790026246719158998 ) ) ;
#74399 = AXIS2_PLACEMENT_3D ( 'NONE', #56478, #69941, #82181 ) ;
#74400 = CARTESIAN_POINT ( 'NONE',  ( 0.2891555358219910499, -0.2891555358219909944, 0.05905511811023616414 ) ) ;
#74401 = CARTESIAN_POINT ( 'NONE',  ( 0.02963302784745480353, -0.3970677821444032474, -8.612909436665150641E-17 ) ) ;
#74402 = CARTESIAN_POINT ( 'NONE',  ( 1.233595800524935227, -0.5023911411419708095, 0.1820866141732285504 ) ) ;
#74403 = CARTESIAN_POINT ( 'NONE',  ( 0.9711286089238851948, 0.2306618581243848609, 0.2411417322834645549 ) ) ;
#74404 = CARTESIAN_POINT ( 'NONE',  ( -9.787531504996567848E-17, 0.3996062992125986035, -1.920830620545185230E-17 ) ) ;
#74405 = CARTESIAN_POINT ( 'NONE',  ( 0.7611548556430451917, -0.6046776061558807314, 0.2411417322834647770 ) ) ;
#74406 = CARTESIAN_POINT ( 'NONE',  ( 0.3420746716998660508, 0.1974969037888705814, -0.9954068241469814504 ) ) ;
#74407 = CARTESIAN_POINT ( 'NONE',  ( 1.312335958005250269, -0.5023911411419708095, 0.1820866141732285504 ) ) ;
#74408 = CARTESIAN_POINT ( 'NONE',  ( 0.08530183727034192087, -0.05778040916215522460, 0.4822834645669289988 ) ) ;
#74409 = CARTESIAN_POINT ( 'NONE',  ( -0.9973753280839886548, 0.2306618581243848609, 0.2411417322834645549 ) ) ;
#74410 = CARTESIAN_POINT ( 'NONE',  ( 1.391076115485564868, 0.2306618581243847221, -0.2411417322834647770 ) ) ;
#74411 = CARTESIAN_POINT ( 'NONE',  ( -0.4724409448818895907, -0.1265901696524993070, -0.9908136482939633449 ) ) ;
#74412 = CARTESIAN_POINT ( 'NONE',  ( -0.3460692066303960868, 0.1998031496062990242, -2.230971128608923770 ) ) ;
#74413 = CARTESIAN_POINT ( 'NONE',  ( 0.3083989501312343062, -0.2845877964562159024, 0.3641732283464567677 ) ) ;
#74414 = ORIENTED_EDGE ( 'NONE', *, *, #16758, .F. ) ;
#74415 = CARTESIAN_POINT ( 'NONE',  ( 0.3392501089628018884, -0.1958661417322833942, -0.8891269273303956666 ) ) ;
#74416 = ORIENTED_EDGE ( 'NONE', *, *, #18267, .T. ) ;
#74417 = CARTESIAN_POINT ( 'NONE',  ( -0.7677165354330699465, 0.1660481256975885056, 0.3530559997133364547 ) ) ;
#74418 = CARTESIAN_POINT ( 'NONE',  ( -0.1246719160104980823, -0.6692913385826773087, -0.1292274648535924053 ) ) ;
#74419 = CARTESIAN_POINT ( 'NONE',  ( -0.3018372703412066094, -0.4281496062992127816, -0.4176697321401328100 ) ) ;
#74420 = CARTESIAN_POINT ( 'NONE',  ( 0.7217847769028878924, 0.05413385826771666132, 0.4176697321401328100 ) ) ;
#74421 = CARTESIAN_POINT ( 'NONE',  ( -0.9776902887139098386, 0.2952755905511810774, -0.1292274648535930714 ) ) ;
#74422 = CARTESIAN_POINT ( 'NONE',  ( -0.1902887139107604098, -0.6692913385826771977, 0.1292274648535927661 ) ) ;
#74423 = CARTESIAN_POINT ( 'NONE',  ( 1.364829396325459854, -0.6046776061558809534, -0.2411417322834644161 ) ) ;
#74424 = CARTESIAN_POINT ( 'NONE',  ( 0.6430446194225728496, 0.05413385826771666132, 0.4176697321401328100 ) ) ;
#74425 = CARTESIAN_POINT ( 'NONE',  ( 0.7414698162729663755, 0.2952755905511811885, 0.1292274648535926551 ) ) ;
#74426 = CARTESIAN_POINT ( 'NONE',  ( 0.1049643490035303689, 0.3917322834645670104, -1.087926509186351476 ) ) ;
#74427 = CARTESIAN_POINT ( 'NONE',  ( -0.3215223097112853146, -0.08942795157528024563, -0.3641732283464568787 ) ) ;
#74428 = EDGE_LOOP ( 'NONE', ( #71910, #81894, #19128, #42398 ) ) ;
#74429 = CARTESIAN_POINT ( 'NONE',  ( 0.3420746716998659953, 0.1974969037888705536, -1.391076115485564424 ) ) ;
#74430 = VERTEX_POINT ( 'NONE', #13296 ) ;
#74431 = CARTESIAN_POINT ( 'NONE',  ( -0.8923884514435688198, 0.1283753931104746893, -0.1820866141732285504 ) ) ;
#74432 = CARTESIAN_POINT ( 'NONE',  ( -0.4658792650918627265, -0.3162353388693409650, -0.4822834645669289433 ) ) ;
#74433 = CARTESIAN_POINT ( 'NONE',  ( -1.559171609364246924, 0.000000000000000000, 0.7327394035119333404 ) ) ;
#74434 = CARTESIAN_POINT ( 'NONE',  ( -0.7217847769028863381, 0.05413385826771626580, -0.4176697321401330321 ) ) ;
#74435 = CARTESIAN_POINT ( 'NONE',  ( -1.036745406824146176, 0.05413385826771626580, -0.4176697321401330321 ) ) ;
#74436 = CARTESIAN_POINT ( 'NONE',  ( -1.351706036745406347, -0.4281496062992124485, 0.4176697321401328655 ) ) ;
#74437 = ADVANCED_FACE ( 'NONE', ( #57467 ), #12877, .T. ) ;
#74438 = CARTESIAN_POINT ( 'NONE',  ( -1.489501312335957062, -0.3162353388693409650, -0.4822834645669289433 ) ) ;
#74439 = CARTESIAN_POINT ( 'NONE',  ( 0.9711286089238851948, -0.5023911411419708095, -0.1820866141732282451 ) ) ;
#74440 = DIRECTION ( 'NONE',  ( 0.000000000000000000, 1.000000000000000000, -0.000000000000000000 ) ) ;
#74441 = CARTESIAN_POINT ( 'NONE',  ( 0.3149606299212184268, 2.559055118110236560, 3.937007874015792552 ) ) ;
#74442 = CARTESIAN_POINT ( 'NONE',  ( 0.2493438320209980519, -0.3690944881889765550, -0.3153832671262227771 ) ) ;
#74443 = AXIS2_PLACEMENT_3D ( 'NONE', #29842, #36570, #61838 ) ;
#74444 = CARTESIAN_POINT ( 'NONE',  ( 0.04593175853018440641, -0.6692913385826771977, 0.1292274648535927661 ) ) ;
#74445 = CARTESIAN_POINT ( 'NONE',  ( -0.1706036745406816491, 0.05413385826771626580, -0.4176697321401330321 ) ) ;
#74446 = ORIENTED_EDGE ( 'NONE', *, *, #1221, .T. ) ;
#74447 = CARTESIAN_POINT ( 'NONE',  ( 0.3996062992125986590, -0.1070741851644053111, -1.843832020997375309 ) ) ;
#74448 = CARTESIAN_POINT ( 'NONE',  ( 0.5314960629920995050, 2.729661064330338061, 2.530077726415326023 ) ) ;
#74449 = VERTEX_POINT ( 'NONE', #76029 ) ;
#74450 = CARTESIAN_POINT ( 'NONE',  ( -0.3996062992125984925, -0.1070741851644056858, -1.067585301837270517 ) ) ;
#74451 = CARTESIAN_POINT ( 'NONE',  ( 1.601049868766404982, 0.2306618581243848609, 0.2411417322834645549 ) ) ;
#74452 = CARTESIAN_POINT ( 'NONE',  ( -0.6824146981627291497, -0.5023911411419708095, -0.1820866141732282451 ) ) ;
#74453 = CARTESIAN_POINT ( 'NONE',  ( -1.049868766404198794, 0.2306618581243847221, -0.2411417322834647770 ) ) ;
#74454 = CARTESIAN_POINT ( 'NONE',  ( 0.4724409448818897572, -0.1265901696524988906, -0.4265091863517060933 ) ) ;
#74455 = LINE ( 'NONE', #34597, #10218 ) ;
#74456 = CARTESIAN_POINT ( 'NONE',  ( -0.1958661417322834220, -0.3392501089628018884, -2.354986876640420057 ) ) ;
#74457 = CARTESIAN_POINT ( 'NONE',  ( -1.607611548556429737, 0.1771653543307087075, -0.09757992244046823083 ) ) ;
#74458 = CARTESIAN_POINT ( 'NONE',  ( 0.5971128608923890191, -0.6692913385826771977, 0.1292274648535927661 ) ) ;
#74459 = CARTESIAN_POINT ( 'NONE',  ( 0.5314960629921267055, -0.5400638737290844871, 0.3530559997133364547 ) ) ;
#74460 = CARTESIAN_POINT ( 'NONE',  ( -0.6167979002624665030, -0.3690944881889765550, -0.3153832671262227771 ) ) ;
#74461 = CARTESIAN_POINT ( 'NONE',  ( -0.06561679790026180015, -0.4281496062992127816, -0.4176697321401328100 ) ) ;
#74462 = CARTESIAN_POINT ( 'NONE',  ( 0.4724409448818896462, 0.1265901696524990294, -2.406167979002624246 ) ) ;
#74463 = CARTESIAN_POINT ( 'NONE',  ( -0.6102362204724400829, 0.1660481256975885056, 0.3530559997133364547 ) ) ;
#74464 = AXIS2_PLACEMENT_3D ( 'NONE', #39188, #5955, #64451 ) ;
#74465 = CARTESIAN_POINT ( 'NONE',  ( 0.2891555358219910499, 0.2891555358219910499, -1.946850393700787496 ) ) ;
#74466 = CARTESIAN_POINT ( 'NONE',  ( 1.292650918635171564, 0.1771653543307087630, 0.09757992244046791164 ) ) ;
#74467 = CARTESIAN_POINT ( 'NONE',  ( 0.2952755905511816326, -0.4536011799217367080, 0.2665933059059888421 ) ) ;
#74468 = CARTESIAN_POINT ( 'NONE',  ( 1.227034120734908917, 0.1771653543307087075, -0.09757992244046823083 ) ) ;
#74469 = CARTESIAN_POINT ( 'NONE',  ( -1.220472440944881054, 0.2952755905511811885, 0.000000000000000000 ) ) ;
#74470 = CARTESIAN_POINT ( 'NONE',  ( -1.167979002624671470, -0.004921259842519576551, 0.3153832671262227771 ) ) ;
#74471 = CARTESIAN_POINT ( 'NONE',  ( -0.5314960629921123836, 2.677165354330708791, -3.900966923095591454 ) ) ;
#74472 = CARTESIAN_POINT ( 'NONE',  ( -1.030183727034119867, -0.05778040916215560624, -0.4822834645669293319 ) ) ;
#74473 = CARTESIAN_POINT ( 'NONE',  ( -0.2493438320209966919, -0.4281496062992124485, 0.4176697321401328655 ) ) ;
#74474 = CARTESIAN_POINT ( 'NONE',  ( 0.4461942257217856311, 0.2306618581243847221, -0.2411417322834647770 ) ) ;
#74475 = CARTESIAN_POINT ( 'NONE',  ( 0.1049643490035303689, 0.3917322834645668994, -2.593156537236534387 ) ) ;
#74476 = CARTESIAN_POINT ( 'NONE',  ( -2.139067083128550983, 1.422987107291908249, 0.4606739315415592229 ) ) ;
#74477 = CARTESIAN_POINT ( 'NONE',  ( 0.5118110236220480003, -0.5511811023622047445, 6.969142054262312111E-17 ) ) ;
#74478 = CARTESIAN_POINT ( 'NONE',  ( 1.102362204724410155, -0.1870078740157479769, 0.4822834645669291653 ) ) ;
#74479 = CARTESIAN_POINT ( 'NONE',  ( -1.686351706036744558, 0.1771653543307087075, -0.09757992244046823083 ) ) ;
#74480 = CARTESIAN_POINT ( 'NONE',  ( 0.9120734908136490793, 0.2952755905511810774, -0.1292274648535930714 ) ) ;
#74481 = CARTESIAN_POINT ( 'NONE',  ( -1.725721784776902190, -0.08942795157527998196, 0.3641732283464567121 ) ) ;
#74482 = CARTESIAN_POINT ( 'NONE',  ( -1.502624671916009680, -0.05778040916215560624, -0.4822834645669293319 ) ) ;
#74483 = CARTESIAN_POINT ( 'NONE',  ( -0.7939632545931754048, -0.3162353388693405765, 0.4822834645669290543 ) ) ;
#74484 = CARTESIAN_POINT ( 'NONE',  ( -0.3018372703412066094, -0.3690944881889765550, -0.3153832671262227771 ) ) ;
#74485 = CARTESIAN_POINT ( 'NONE',  ( 0.000000000000000000, 2.185039370078740273, 0.000000000000000000 ) ) ;
#74486 = CARTESIAN_POINT ( 'NONE',  ( 0.6364829396325465405, -0.08942795157527998196, 0.3641732283464567121 ) ) ;
#74487 = B_SPLINE_CURVE_WITH_KNOTS ( 'NONE', 3,
 ( #43255, #10483, #36136, #4149, #82010, #29814, #5388, #23919, #61809, #75280, #68543, #49169, #31049, #56719, #10884, #11302, #62638, #42850, #4982, #82416, #6622, #64704, #45745, #63867, #39445, #26817 ),
 .UNSPECIFIED., .F., .F.,
 ( 4, 2, 2, 2, 2, 2, 2, 2, 2, 2, 2, 2, 4 ),
 ( 0.01885842312717905811, 0.02003652323609797156, 0.02121462334501688501, 0.02357082356285470845, 0.02474892367177362190, 0.02592702378069253535, 0.02828322399853035532, 0.03063942421636817875, 0.03181752432528708874, 0.03299562443420599872, 0.03535182465204379787, 0.03652992476096270091, 0.03770802486988160396 ),
 .UNSPECIFIED. ) ;
#74488 = CARTESIAN_POINT ( 'NONE',  ( -0.09186351706036663400, -0.4281496062992124485, 0.4176697321401328655 ) ) ;
#74489 = CARTESIAN_POINT ( 'NONE',  ( -0.3996062992125985480, -7.340648628747423112E-17, -0.4311023622047244208 ) ) ;
#74490 = CARTESIAN_POINT ( 'NONE',  ( -1.036745406824146176, 0.05413385826771626580, -0.4176697321401330321 ) ) ;
#74491 = CARTESIAN_POINT ( 'NONE',  ( -0.1958661417322834220, -0.3392501089628018884, -1.882545931758530244 ) ) ;
#74492 = CARTESIAN_POINT ( 'NONE',  ( 0.8727034120734912248, -0.2845877964562161244, -0.3641732283464567121 ) ) ;
#74493 = CARTESIAN_POINT ( 'NONE',  ( -0.1574803149606292529, -0.1870078740157480879, -0.4822834645669291653 ) ) ;
#74494 = CARTESIAN_POINT ( 'NONE',  ( -0.4658792650918627265, -0.3162353388693409650, -0.4822834645669289433 ) ) ;
#74495 = CARTESIAN_POINT ( 'NONE',  ( -0.4527559055118102749, -0.4536011799217368745, -0.2665933059059886201 ) ) ;
#74496 = FACE_OUTER_BOUND ( 'NONE', #3209, .T. ) ;
#74497 = CARTESIAN_POINT ( 'NONE',  ( -0.3083989501312330295, -0.2845877964562161244, -0.3641732283464567121 ) ) ;
#74498 = CARTESIAN_POINT ( 'NONE',  ( 0.5446194225721792126, -0.3162353388693405765, 0.4822834645669290543 ) ) ;
#74499 = CARTESIAN_POINT ( 'NONE',  ( -1.030183727034119867, -0.08942795157528024563, -0.3641732283464568787 ) ) ;
#74500 = CARTESIAN_POINT ( 'NONE',  ( -0.3996062992125985480, -7.340648628747423112E-17, -1.375984251968504157 ) ) ;
#74501 = CARTESIAN_POINT ( 'NONE',  ( 1.528871391076116026, -0.6692913385826773087, -0.1292274648535924053 ) ) ;
#74502 = DIRECTION ( 'NONE',  ( -3.096699300667737957E-16, 1.000000000000000000, -0.000000000000000000 ) ) ;
#74503 = VERTEX_POINT ( 'NONE', #30977 ) ;
#74504 = AXIS2_PLACEMENT_3D ( 'NONE', #28044, #27627, #15860 ) ;
#74505 = CARTESIAN_POINT ( 'NONE',  ( -1.417322834645668772, -0.1870078740157479769, 0.3641732283464567677 ) ) ;
#74506 = CARTESIAN_POINT ( 'NONE',  ( -0.3805774278215216522, -0.4281496062992127816, -0.4176697321401328100 ) ) ;
#74507 = CARTESIAN_POINT ( 'NONE',  ( -1.167979002624671470, 0.05413385826771666132, 0.4176697321401328100 ) ) ;
#74508 = CARTESIAN_POINT ( 'NONE',  ( 0.1958661417322836440, -0.3392501089628017219, -1.751312335958005395 ) ) ;
#74509 = CARTESIAN_POINT ( 'NONE',  ( 0.4724409448818898682, 2.892866454678787531E-17, -2.165354330708661568 ) ) ;
#74510 = CARTESIAN_POINT ( 'NONE',  ( 1.345144356955381593, -0.05778040916215522460, 0.4822834645669289988 ) ) ;
#74511 = CARTESIAN_POINT ( 'NONE',  ( 0.5052493438320218022, -0.6692913385826773087, -0.1292274648535924053 ) ) ;
#74512 = CARTESIAN_POINT ( 'NONE',  ( 4.797336870675656522E-17, -0.3917322834645670104, -2.748031496062991685 ) ) ;
#74513 = CARTESIAN_POINT ( 'NONE',  ( 0.1998031496062992463, 0.3460692066303959202, -2.425853018372703396 ) ) ;
#74514 = CARTESIAN_POINT ( 'NONE',  ( 1.607611548556431069, 0.1771653543307087630, 0.09757992244046791164 ) ) ;
#74515 = CARTESIAN_POINT ( 'NONE',  ( -0.3460692066303958092, -0.1998031496062994683, -0.8398950131233595684 ) ) ;
#74516 = ORIENTED_EDGE ( 'NONE', *, *, #74315, .T. ) ;
#74517 = CARTESIAN_POINT ( 'NONE',  ( -0.8398950131233585692, 0.1283753931104748280, 0.1820866141732283561 ) ) ;
#74519 = CARTESIAN_POINT ( 'NONE',  ( -0.1049643490035307020, 0.3917322834645669549, -2.833333333333333037 ) ) ;
#74518 = VECTOR ( 'NONE', #81239, 39.37007874015748143 ) ;
#74520 = ORIENTED_EDGE ( 'NONE', *, *, #17653, .T. ) ;
#74521 = CARTESIAN_POINT ( 'NONE',  ( 0.6955380577427828781, 0.05413385826771626580, -0.4176697321401330321 ) ) ;
#74522 = CARTESIAN_POINT ( 'NONE',  ( -0.2559055118110230564, 0.1660481256975883668, -0.3530559997133364547 ) ) ;
#74523 = APPLICATION_CONTEXT ( 'automotive_design' ) ;
#74524 = CARTESIAN_POINT ( 'NONE',  ( -1.128608923884513837, 0.2306618581243847221, -0.2411417322834647770 ) ) ;
#74525 = CARTESIAN_POINT ( 'NONE',  ( 1.043307086614173818, 0.1660481256975885056, 0.3530559997133364547 ) ) ;
#74526 = CARTESIAN_POINT ( 'NONE',  ( -1.397637795275589623, -0.4536011799217368745, -0.2665933059059886201 ) ) ;
#74527 = PLANE ( 'NONE',  #72259 ) ;
#74528 = CARTESIAN_POINT ( 'NONE',  ( 0.1574803149606306130, -0.1870078740157480879, -0.4822834645669291653 ) ) ;
#74529 = CARTESIAN_POINT ( 'NONE',  ( -0.9317585301837263412, -0.4281496062992127816, -0.4176697321401328100 ) ) ;
#74530 = CARTESIAN_POINT ( 'NONE',  ( -0.1049643490035301746, -0.3917322834645670659, -1.569534489992439497 ) ) ;
#74531 = CARTESIAN_POINT ( 'NONE',  ( 1.555118110236221041, -0.5400638737290844871, 0.3530559997133364547 ) ) ;
#74532 = LINE ( 'NONE', #61471, #61370 ) ;
#74533 = CARTESIAN_POINT ( 'NONE',  ( 0.9317585301837276734, 0.05413385826771626580, -0.4176697321401330321 ) ) ;
#74534 = CARTESIAN_POINT ( 'NONE',  ( -0.3917322834645671215, 0.1049643490035301469, -2.794619422572177658 ) ) ;
#74535 = CARTESIAN_POINT ( 'NONE',  ( 1.351706036745407680, -0.004921259842519576551, 0.3153832671262227771 ) ) ;
#74536 = ORIENTED_EDGE ( 'NONE', *, *, #30658, .F. ) ;
#74537 = CARTESIAN_POINT ( 'NONE',  ( 0.3917322834645670104, 0.1049643490035304660, -2.798575746228034067 ) ) ;
#74538 = CARTESIAN_POINT ( 'NONE',  ( -0.2230971128608915943, 0.05413385826771666132, 0.4176697321401328100 ) ) ;
#74539 = ORIENTED_EDGE ( 'NONE', *, *, #30503, .F. ) ;
#74540 = CARTESIAN_POINT ( 'NONE',  ( 0.5511811023622054106, -0.1870078740157480601, -0.3641732283464567677 ) ) ;
#74541 = CARTESIAN_POINT ( 'NONE',  ( -1.502624671916009680, -0.05778040916215560624, -0.4822834645669293319 ) ) ;
#74542 = CARTESIAN_POINT ( 'NONE',  ( 0.5314960629921264834, 0.1660481256975883668, -0.3530559997133364547 ) ) ;
#74543 = CARTESIAN_POINT ( 'NONE',  ( 0.7086614173228352742, -0.1870078740157480879, -0.4822834645669291653 ) ) ;
#74544 = EDGE_CURVE ( 'NONE', #51716, #37370, #3118, .T. ) ;
#74545 = CARTESIAN_POINT ( 'NONE',  ( -0.1181102362204717315, 0.2952755905511811885, 0.000000000000000000 ) ) ;
#74546 = CARTESIAN_POINT ( 'NONE',  ( -0.3917322834645670104, -0.1049643490035307020, -1.459993069062679005 ) ) ;
#74547 = CARTESIAN_POINT ( 'NONE',  ( -0.6233595800524928121, -0.3162353388693409650, -0.4822834645669289433 ) ) ;
#74548 = CARTESIAN_POINT ( 'NONE',  ( -0.1958661417322834220, -0.3392501089628018884, -2.040026246719160330 ) ) ;
#74549 = CARTESIAN_POINT ( 'NONE',  ( -1.640419947506561060, -0.4281496062992127816, -0.4176697321401328100 ) ) ;
#74550 = CARTESIAN_POINT ( 'NONE',  ( -1.128608923884513837, 0.2306618581243847221, -0.2411417322834647770 ) ) ;
#74551 = CARTESIAN_POINT ( 'NONE',  ( 1.463254593175853824, -0.6692913385826771977, 0.1292274648535927661 ) ) ;
#74552 = CARTESIAN_POINT ( 'NONE',  ( 1.246719160104987623, 0.05413385826771626580, -0.4176697321401330321 ) ) ;
#74553 = CARTESIAN_POINT ( 'NONE',  ( 0.2925321140481932369, 0.2925321140481932369, -0.6102362204724409711 ) ) ;
#74554 = CARTESIAN_POINT ( 'NONE',  ( -1.135170603674539924, -0.6692913385826771977, 0.1292274648535927661 ) ) ;
#74555 = CARTESIAN_POINT ( 'NONE',  ( 0.3996062992125985480, 2.446882876249141654E-17, -0.03740157480314962313 ) ) ;
#74556 = CARTESIAN_POINT ( 'NONE',  ( 0.1181102362204730916, -0.6692913385826771977, 8.415575281601705876E-17 ) ) ;
#74557 = CARTESIAN_POINT ( 'NONE',  ( -0.2925321140481930704, -0.2925321140481933480, -2.263779527559055094 ) ) ;
#74558 = CARTESIAN_POINT ( 'NONE',  ( -0.5052493438320203589, 0.2952755905511810774, -0.1292274648535930714 ) ) ;
#74559 = CARTESIAN_POINT ( 'NONE',  ( 1.633858267716535639, -0.5400638737290844871, 0.3530559997133364547 ) ) ;
#74560 = CARTESIAN_POINT ( 'NONE',  ( 0.7677165354330716118, 0.07958543189024071263, -0.2665933059059888421 ) ) ;
#74561 = CARTESIAN_POINT ( 'NONE',  ( 1.259842519685040019, -0.1870078740157479769, 0.4822834645669291653 ) ) ;
#74562 = CARTESIAN_POINT ( 'NONE',  ( -0.4724409448818899238, 0.1265901696524986686, -1.054461942257217899 ) ) ;
#74563 = CARTESIAN_POINT ( 'NONE',  ( 0.6758530183727039509, -0.5511811023622046335, 0.09757992244046803654 ) ) ;
#74564 = CARTESIAN_POINT ( 'NONE',  ( 0.9908136482939640111, 0.2952755905511810774, -0.1292274648535930714 ) ) ;
#74565 = CARTESIAN_POINT ( 'NONE',  ( 0.3949938075777409963, 2.418639510665530743E-17, -0.6673228346456693272 ) ) ;
#74566 = CARTESIAN_POINT ( 'NONE',  ( -0.7283464566929126471, 0.1660481256975883668, -0.3530559997133364547 ) ) ;
#74567 = DIRECTION ( 'NONE',  ( 1.000000000000000000, 0.000000000000000000, 1.047444401652940007E-14 ) ) ;
#74568 = VECTOR ( 'NONE', #79438, 39.37007874015748143 ) ;
#74569 = CARTESIAN_POINT ( 'NONE',  ( 1.161417322834646271, 0.07958543189024071263, -0.2665933059059888421 ) ) ;
#74570 = CARTESIAN_POINT ( 'NONE',  ( -0.3740157480314953431, -0.5400638737290845981, -0.3530559997133363437 ) ) ;
#74571 = CARTESIAN_POINT ( 'NONE',  ( 0.09842519685039434474, -0.5400638737290845981, -0.3530559997133363437 ) ) ;
#74572 = CARTESIAN_POINT ( 'NONE',  ( 0.09115970038225353067, 3.421639014772782816E-16, 0.3464511005275203726 ) ) ;
#74573 = CARTESIAN_POINT ( 'NONE',  ( -0.09186351706036689768, 0.05413385826771626580, -0.4176697321401330321 ) ) ;
#74574 = CARTESIAN_POINT ( 'NONE',  ( 0.7283464566929143125, 0.07958543189024085140, 0.2665933059059887866 ) ) ;
#74575 = CARTESIAN_POINT ( 'NONE',  ( -2.557140022784271327, 1.502969453419624513, 0.4732359647714760587 ) ) ;
#74576 = CARTESIAN_POINT ( 'NONE',  ( -0.01968503937007793844, 0.07958543189024071263, -0.2665933059059888421 ) ) ;
#74577 = CARTESIAN_POINT ( 'NONE',  ( 0.9120734908136489683, -0.5511811023622046335, 0.09757992244046803654 ) ) ;
#74578 = DIRECTION ( 'NONE',  ( -3.096699300667737957E-16, 1.000000000000000000, -0.000000000000000000 ) ) ;
#74579 = CARTESIAN_POINT ( 'NONE',  ( 0.3460692066303958092, 0.1998031496062993018, -1.940288713910761409 ) ) ;
#74580 = CARTESIAN_POINT ( 'NONE',  ( 0.4396325459317593221, 0.2952755905511810774, -0.1292274648535930714 ) ) ;
#74581 = CARTESIAN_POINT ( 'NONE',  ( 0.2867679344610365999, 0.2867679344610365999, -1.232283464566929387 ) ) ;
#74582 = CARTESIAN_POINT ( 'NONE',  ( 1.423884514435696413, -0.2845877964562161244, -0.3641732283464567121 ) ) ;
#74583 = CARTESIAN_POINT ( 'NONE',  ( -0.3165741174739065689, -0.2316922116739008053, -4.446769521226833214E-17 ) ) ;
#74584 = CARTESIAN_POINT ( 'NONE',  ( -0.3871391076115479057, -0.2845877964562161244, -0.3641732283464567121 ) ) ;
#74585 = CIRCLE ( 'NONE', #32857, 3.937007874015748143 ) ;
#74586 = CARTESIAN_POINT ( 'NONE',  ( -0.01312335958005186876, 0.05413385826771626580, -0.4176697321401330321 ) ) ;
#74587 = CARTESIAN_POINT ( 'NONE',  ( 1.240157480314961314, 0.07958543189024071263, -0.2665933059059888421 ) ) ;
#74588 = CARTESIAN_POINT ( 'NONE',  ( -1.423884514435694859, -0.2845877964562159024, 0.3641732283464567677 ) ) ;
#74589 = CARTESIAN_POINT ( 'NONE',  ( -1.338582677165353729, -0.1870078740157480879, -0.4822834645669291653 ) ) ;
#74590 = CARTESIAN_POINT ( 'NONE',  ( 0.2559055118110243332, 0.1660481256975885056, 0.3530559997133364547 ) ) ;
#74591 = CARTESIAN_POINT ( 'NONE',  ( 1.023622047244095334, -0.1870078740157479769, 0.4822834645669291653 ) ) ;
#74592 = CARTESIAN_POINT ( 'NONE',  ( -0.03443470937339819515, 1.064243487142144673, -1.633358474390059989 ) ) ;
#74593 = CARTESIAN_POINT ( 'NONE',  ( 0.3280839895013130669, 0.05413385826771666132, 0.4176697321401328100 ) ) ;
#74594 = CARTESIAN_POINT ( 'NONE',  ( 1.154855643044620184, -0.6046776061558807314, 0.2411417322834647770 ) ) ;
#74595 = B_SPLINE_CURVE_WITH_KNOTS ( 'NONE', 3,
 ( #64441, #38349, #6364, #26132 ),
 .UNSPECIFIED., .F., .F.,
 ( 4, 4 ),
 ( 9.341771812940338307E-18, 0.001494448006632299744 ),
 .UNSPECIFIED. ) ;
#74596 = CARTESIAN_POINT ( 'NONE',  ( 0.7939632545931766261, -0.3162353388693409650, -0.4822834645669289433 ) ) ;
#74597 = CARTESIAN_POINT ( 'NONE',  ( 0.4091458600556404646, -0.2362204724409448231, -0.3392388451443569819 ) ) ;
#74598 = CARTESIAN_POINT ( 'NONE',  ( 0.8792650918635177559, -0.004921259842519576551, 0.3153832671262227771 ) ) ;
#74599 = CARTESIAN_POINT ( 'NONE',  ( -1.587926509186350810, -0.004921259842519870586, -0.3153832671262229437 ) ) ;
#74600 = CARTESIAN_POINT ( 'NONE',  ( -0.05905511811023545637, -0.4536011799217368745, -0.2665933059059886201 ) ) ;
#74601 = CARTESIAN_POINT ( 'NONE',  ( -0.1312335958005241554, -0.6046776061558809534, -0.2411417322834644161 ) ) ;
#74602 = CARTESIAN_POINT ( 'NONE',  ( 0.5971128608923890191, -0.6692913385826771977, 0.1292274648535927661 ) ) ;
#74603 = CARTESIAN_POINT ( 'NONE',  ( -0.2887139107611542133, -0.6046776061558809534, -0.2411417322834644161 ) ) ;
#74604 = CARTESIAN_POINT ( 'NONE',  ( -0.2867679344610367109, 0.2867679344610365444, -2.221147924705723753 ) ) ;
#74605 = CARTESIAN_POINT ( 'NONE',  ( -0.1377952755905504645, 0.07958543189024085140, 0.2665933059059887866 ) ) ;
#74606 = CARTESIAN_POINT ( 'NONE',  ( 0.8792650918635177559, -0.4281496062992127816, -0.4176697321401328100 ) ) ;
#74607 = CARTESIAN_POINT ( 'NONE',  ( 0.9186351706036752773, 0.1283753931104746893, -0.1820866141732285504 ) ) ;
#74608 = CARTESIAN_POINT ( 'NONE',  ( 1.141392835773559211, 1.299212598425196985, 1.141392835773562764 ) ) ;
#74610 = CARTESIAN_POINT ( 'NONE',  ( 1.011202504342157527, 9.477779430591278127E-17, -0.3464511005275205946 ) ) ;
#74609 = CARTESIAN_POINT ( 'NONE',  ( -0.6299212598425059095, 1.724409448818897905, -3.937007874015764131 ) ) ;
#74611 = CARTESIAN_POINT ( 'NONE',  ( -0.1455973158445646731, 1.053234027224559943, 0.2773552301749948046 ) ) ;
#74612 = CARTESIAN_POINT ( 'NONE',  ( -1.233595800524933894, -0.6046776061558809534, -0.2411417322834644161 ) ) ;
#74613 = CARTESIAN_POINT ( 'NONE',  ( -0.3871391076115479057, -0.3162353388693409650, -0.4822834645669289433 ) ) ;
#74614 =( BOUNDED_CURVE ( )  B_SPLINE_CURVE ( 2, ( #12701, #38777, #6375, #57706, #77088, #71610, #64454, #26985, #13963, #69, #25723, #51383, #58124 ),
 .UNSPECIFIED., .F., .F. ) 
 B_SPLINE_CURVE_WITH_KNOTS ( ( 3, 2, 2, 2, 2, 2, 3 ),
 ( 0.3551492764529827206, 0.3560606060606060774, 0.3598484848484848619, 0.3636363636363636465, 0.3674242424242424310, 0.3712121212121212155, 0.3721234508197446278 ),
 .UNSPECIFIED. ) 
 CURVE ( )  GEOMETRIC_REPRESENTATION_ITEM ( )  RATIONAL_B_SPLINE_CURVE ( ( 0.9875488213027530104, 0.9918020599134685922, 1.000000000000000000, 0.9659258262890683122, 1.000000000000000000, 0.9659258262890683122, 1.000000000000000000, 0.9659258262890683122, 1.000000000000000000, 0.9659258262890683122, 1.000000000000000000, 0.9918020599134680371, 0.9875488213027523443 ) ) 
 REPRESENTATION_ITEM ( '' )  );
#74615 = CARTESIAN_POINT ( 'NONE',  ( -0.1265901696524986964, -0.4724409448818899238, 0.08530183727034119923 ) ) ;
#74616 = CARTESIAN_POINT ( 'NONE',  ( 0.3420746716998660508, -0.1974969037888703871, -2.152230971128608950 ) ) ;
#74617 = VERTEX_POINT ( 'NONE', #20018 ) ;
#74618 = CARTESIAN_POINT ( 'NONE',  ( 0.3937007874015754361, -0.1870078740157479769, 0.3641732283464567677 ) ) ;
#74619 = CARTESIAN_POINT ( 'NONE',  ( -0.1049643490035302024, -0.3917322834645671215, -0.8517060367454066805 ) ) ;
#74620 = CARTESIAN_POINT ( 'NONE',  ( 1.108923884514436242, -0.05778040916215522460, 0.4822834645669289988 ) ) ;
#74621 = CARTESIAN_POINT ( 'NONE',  ( -0.4724409448818898682, -8.678599364036362592E-17, -2.559055118110236560 ) ) ;
#74622 = CARTESIAN_POINT ( 'NONE',  ( 2.142213561789872767, 0.02617651024168201127, 0.4623158380715620130 ) ) ;
#74623 = CARTESIAN_POINT ( 'NONE',  ( -1.692913385826770645, 0.1771653543307087630, 0.000000000000000000 ) ) ;
#74624 = CARTESIAN_POINT ( 'NONE',  ( 1.666666666666667185, 0.05413385826771666132, 0.4176697321401328100 ) ) ;
#74625 = CARTESIAN_POINT ( 'NONE',  ( 1.482939632545932307, -0.004921259842519870586, -0.3153832671262229437 ) ) ;
#74626 = CARTESIAN_POINT ( 'NONE',  ( 0.5905511811023629321, 0.2952755905511811885, 0.000000000000000000 ) ) ;
#74627 = CARTESIAN_POINT ( 'NONE',  ( -0.1049643490035301746, -0.3917322834645670659, -0.3096919703073997554 ) ) ;
#74628 = CARTESIAN_POINT ( 'NONE',  ( -0.03937007874015669567, 0.2952755905511811885, 0.000000000000000000 ) ) ;
#74629 = CARTESIAN_POINT ( 'NONE',  ( -0.8136482939632537770, -0.5023911411419708095, 0.1820866141732285504 ) ) ;
#74631 = EDGE_CURVE ( 'NONE', #59707, #80266, #70268, .T. ) ;
#74630 = CARTESIAN_POINT ( 'NONE',  ( 0.4133858267716541968, -0.5400638737290845981, -0.3530559997133363437 ) ) ;
#74632 = CARTESIAN_POINT ( 'NONE',  ( -0.006561679790025524116, -0.3162353388693405765, 0.4822834645669290543 ) ) ;
#74633 = CARTESIAN_POINT ( 'NONE',  ( -1.603475055217291612, 2.094628720676861011, 0.04573490813648255215 ) ) ;
#74634 = CARTESIAN_POINT ( 'NONE',  ( -0.1070741851644051862, -0.3996062992125987146, -2.906824146981627610 ) ) ;
#74635 = CARTESIAN_POINT ( 'NONE',  ( -0.1958661417322836995, 0.3392501089628017219, -1.742145300033807631 ) ) ;
#74636 = CARTESIAN_POINT ( 'NONE',  ( 1.017060367454068803, -0.3162353388693405765, 0.4822834645669290543 ) ) ;
#74637 = CARTESIAN_POINT ( 'NONE',  ( -0.3346456692913377662, -0.5400638737290844871, 0.3530559997133364547 ) ) ;
#74638 = CARTESIAN_POINT ( 'NONE',  ( -1.502624671916009680, -0.3162353388693405765, 0.4822834645669290543 ) ) ;
#74640 = CARTESIAN_POINT ( 'NONE',  ( 1.003937007874016185, 0.1660481256975883668, -0.3530559997133364547 ) ) ;
#74639 = VECTOR ( 'NONE', #34692, 39.37007874015748143 ) ;
#74641 = CARTESIAN_POINT ( 'NONE',  ( 0.5249343832021005074, -0.6046776061558807314, 0.2411417322834647770 ) ) ;
#74642 = CARTESIAN_POINT ( 'NONE',  ( 0.3917322834645670104, 2.398668435337828261E-17, -1.147637795275590733 ) ) ;
#74643 = CARTESIAN_POINT ( 'NONE',  ( -0.3740157480314953431, -0.5400638737290845981, -0.3530559997133363437 ) ) ;
#74644 = CARTESIAN_POINT ( 'NONE',  ( 0.1377952755905518800, 0.1660481256975883668, -0.3530559997133364547 ) ) ;
#74645 = CARTESIAN_POINT ( 'NONE',  ( -0.6233595800524928121, -0.3162353388693409650, -0.4822834645669289433 ) ) ;
#74646 = CARTESIAN_POINT ( 'NONE',  ( 0.1443569553805781891, -0.004921259842519870586, -0.3153832671262229437 ) ) ;
#74647 = CARTESIAN_POINT ( 'NONE',  ( -1.640419947506561060, -0.4281496062992127816, -0.4176697321401328100 ) ) ;
#74648 = DIRECTION ( 'NONE',  ( 0.000000000000000000, 0.000000000000000000, -1.000000000000000000 ) ) ;
#74649 = CARTESIAN_POINT ( 'NONE',  ( 0.1902887139107617975, 0.2952755905511811885, 0.1292274648535926551 ) ) ;
#74650 = FACE_OUTER_BOUND ( 'NONE', #2045, .T. ) ;
#74651 = CARTESIAN_POINT ( 'NONE',  ( 1.502624671916010790, -0.3162353388693409650, -0.4822834645669289433 ) ) ;
#74652 = CARTESIAN_POINT ( 'NONE',  ( -0.2867679344610365999, 0.2867679344610364889, -2.374015748031496287 ) ) ;
#74653 = VERTEX_POINT ( 'NONE', #27156 ) ;
#74654 = ORIENTED_EDGE ( 'NONE', *, *, #29199, .F. ) ;
#74655 = CARTESIAN_POINT ( 'NONE',  ( 0.6496062992125991586, -0.5400638737290845981, -0.3530559997133363437 ) ) ;
#74656 = CARTESIAN_POINT ( 'NONE',  ( 0.03937007874015806264, 0.1771653543307087630, 0.000000000000000000 ) ) ;
#74658 = DIRECTION ( 'NONE',  ( 1.000000000000000000, 0.000000000000000000, -0.000000000000000000 ) ) ;
#74657 = CARTESIAN_POINT ( 'NONE',  ( 1.666666666666667185, -0.004921259842519576551, 0.3153832671262227771 ) ) ;
#74659 = CARTESIAN_POINT ( 'NONE',  ( 0.3917322834645670104, 2.398668435337828261E-17, -0.8326771653543307838 ) ) ;
#74660 = CARTESIAN_POINT ( 'NONE',  ( 0.4724409448818897572, -0.1265901696524988906, -0.03083989501312336262 ) ) ;
#74661 = CARTESIAN_POINT ( 'NONE',  ( 0.3034644639079869255, -3.790565315793794774E-16, -0.3791475997938105191 ) ) ;
#74662 = CARTESIAN_POINT ( 'NONE',  ( 0.2925321140481932369, 0.2925321140481932369, -2.261811023622047223 ) ) ;
#74663 = CARTESIAN_POINT ( 'NONE',  ( 1.043307086614173818, -0.5400638737290845981, -0.3530559997133363437 ) ) ;
#74664 = CARTESIAN_POINT ( 'NONE',  ( -0.7874015748031489847, -0.1870078740157480879, -0.4822834645669291653 ) ) ;
#74665 = CARTESIAN_POINT ( 'NONE',  ( -0.6824146981627291497, -0.6046776061558809534, -0.2411417322834644161 ) ) ;
#74666 = CARTESIAN_POINT ( 'NONE',  ( 0.7217847769028878924, -0.4281496062992127816, -0.4176697321401328100 ) ) ;
#74667 = CARTESIAN_POINT ( 'NONE',  ( 1.200787401574803681, -0.5400638737290845981, -0.3530559997133363437 ) ) ;
#74668 = CARTESIAN_POINT ( 'NONE',  ( 1.640419947506562393, -0.3690944881889763329, 0.3153832671262228327 ) ) ;
#74669 = PRODUCT_CONTEXT ( 'NONE', #32577, 'mechanical' ) ;
#74670 = CARTESIAN_POINT ( 'NONE',  ( 1.200787401574803681, 0.07958543189024085140, 0.2665933059059887866 ) ) ;
#74671 = DIRECTION ( 'NONE',  ( 0.000000000000000000, -1.000000000000000000, -1.734723475976808327E-16 ) ) ;
#74672 = CARTESIAN_POINT ( 'NONE',  ( -1.200787401574802349, -0.4536011799217367080, 0.2665933059059888421 ) ) ;
#74673 = CARTESIAN_POINT ( 'NONE',  ( 0.3083989501312343062, -0.05778040916215560624, -0.4822834645669293319 ) ) ;
#74675 = DIRECTION ( 'NONE',  ( 0.000000000000000000, -1.000000000000000000, 0.000000000000000000 ) ) ;
#74674 = CARTESIAN_POINT ( 'NONE',  ( 1.056430446194226658, 0.2952755905511811885, 0.1292274648535926551 ) ) ;
#74676 = CARTESIAN_POINT ( 'NONE',  ( -1.364829396325458521, 0.1283753931104746893, -0.1820866141732285504 ) ) ;
#74677 = CARTESIAN_POINT ( 'NONE',  ( 0.2559055118110243332, 0.1660481256975885056, 0.3530559997133364547 ) ) ;
#74678 = CARTESIAN_POINT ( 'NONE',  ( 1.443569553805774897, 0.1283753931104748280, 0.1820866141732283561 ) ) ;
#74679 = CARTESIAN_POINT ( 'NONE',  ( 0.1049643490035303689, 0.3917322834645668994, -1.805754962433383737 ) ) ;
#74680 = CARTESIAN_POINT ( 'NONE',  ( -1.318897637795274802, -0.4536011799217368745, -0.2665933059059886201 ) ) ;
#74681 = CARTESIAN_POINT ( 'NONE',  ( 1.541994750656168645, 0.2952755905511810774, -0.1292274648535930714 ) ) ;
#74682 = CARTESIAN_POINT ( 'NONE',  ( 0.3006637500733741475, 1.776489521407567551, 0.08741570540071638695 ) ) ;
#74683 = CARTESIAN_POINT ( 'NONE',  ( 0.08530183727034192087, -0.2845877964562161244, -0.3641732283464567121 ) ) ;
#74684 = CARTESIAN_POINT ( 'NONE',  ( -0.1640419947506555343, -0.3162353388693405765, 0.4822834645669290543 ) ) ;
#74685 = CARTESIAN_POINT ( 'NONE',  ( -1.266404199475064773, -0.08942795157528024563, -0.3641732283464568787 ) ) ;
#74686 = CARTESIAN_POINT ( 'NONE',  ( -0.8005249343832013809, -0.4281496062992124485, 0.4176697321401328655 ) ) ;
#74687 = CARTESIAN_POINT ( 'NONE',  ( 1.515748031496063408, 0.1660481256975885056, 0.3530559997133364547 ) ) ;
#74688 = CARTESIAN_POINT ( 'NONE',  ( 0.1958661417322836718, -0.3392501089628017219, -0.4035626228684533467 ) ) ;
#74689 = FACE_OUTER_BOUND ( 'NONE', #39614, .T. ) ;
#74690 = CARTESIAN_POINT ( 'NONE',  ( 1.272965879265092637, 0.05413385826771666132, 0.4176697321401328100 ) ) ;
#74691 = CARTESIAN_POINT ( 'NONE',  ( -0.4091458600556402980, -0.2362204724409451284, -2.176509186351706315 ) ) ;
#74692 = AXIS2_PLACEMENT_3D ( 'NONE', #74441, #53405, #61796 ) ;
#74693 = CARTESIAN_POINT ( 'NONE',  ( -1.128608923884513837, -0.6046776061558807314, 0.2411417322834647770 ) ) ;
#74694 = CARTESIAN_POINT ( 'NONE',  ( -1.174540682414697335, -0.08942795157527998196, 0.3641732283464567121 ) ) ;
#74695 = CARTESIAN_POINT ( 'NONE',  ( -0.6824146981627291497, -0.5023911411419708095, -0.1820866141732282451 ) ) ;
#74696 = CARTESIAN_POINT ( 'NONE',  ( -1.220472440944882386, -0.1870078740157480046, 1.254653134982923898E-17 ) ) ;
#74697 = CARTESIAN_POINT ( 'NONE',  ( -0.09186351706036663400, -0.4281496062992124485, 0.4176697321401328655 ) ) ;
#74698 = CARTESIAN_POINT ( 'NONE',  ( 0.1771653543307093182, -0.4536011799217368745, -0.2665933059059886201 ) ) ;
#74699 = CARTESIAN_POINT ( 'NONE',  ( -0.9383202099737524282, -0.08942795157527998196, 0.3641732283464567121 ) ) ;
#74700 = CARTESIAN_POINT ( 'NONE',  ( -1.646981627296586703, -0.3162353388693409650, -0.4822834645669289433 ) ) ;
#74701 = CARTESIAN_POINT ( 'NONE',  ( 1.535433070866142335, -0.5511811023622047445, 6.969142054262312111E-17 ) ) ;
#74702 = CARTESIAN_POINT ( 'NONE',  ( 1.443569553805774897, -0.6046776061558809534, -0.2411417322834644161 ) ) ;
#74703 = CARTESIAN_POINT ( 'NONE',  ( 0.3013144171194340193, 1.169708940200703040, 1.947449872764505541 ) ) ;
#74704 = CARTESIAN_POINT ( 'NONE',  ( 0.4986876640419954376, -0.5023911411419708095, -0.1820866141732282451 ) ) ;
#74705 = CARTESIAN_POINT ( 'NONE',  ( 0.9580052493438327987, -0.4281496062992127816, -0.4176697321401328100 ) ) ;
#74706 = CARTESIAN_POINT ( 'NONE',  ( 1.154855643044620184, 0.1283753931104746893, -0.1820866141732285504 ) ) ;
#74707 = ORIENTED_EDGE ( 'NONE', *, *, #302, .F. ) ;
#74708 = CARTESIAN_POINT ( 'NONE',  ( -1.384514435695537005, -0.6692913385826773087, -0.1292274648535924053 ) ) ;
#74709 = CARTESIAN_POINT ( 'NONE',  ( -1.030183727034119867, -0.3162353388693405765, 0.4822834645669290543 ) ) ;
#74710 = CARTESIAN_POINT ( 'NONE',  ( -0.04593175853018302557, -0.6692913385826773087, -0.1292274648535924053 ) ) ;
#74711 = CARTESIAN_POINT ( 'NONE',  ( 0.5392480709929744487, -4.069555009745408348E-17, -0.3627989612356148363 ) ) ;
#74712 = CARTESIAN_POINT ( 'NONE',  ( 0.1998031496062992463, 0.3460692066303959202, -2.110892388451443669 ) ) ;
#74713 = CARTESIAN_POINT ( 'NONE',  ( 0.7611548556430451917, -0.6046776061558807314, 0.2411417322834647770 ) ) ;
#74714 = CARTESIAN_POINT ( 'NONE',  ( 1.397637795275591177, -0.4536011799217367080, 0.2665933059059888421 ) ) ;
#74715 = CARTESIAN_POINT ( 'NONE',  ( 0.2034120734908144990, -0.6692913385826771977, 0.1292274648535927661 ) ) ;
#74716 = CARTESIAN_POINT ( 'NONE',  ( 0.6824146981627303710, 0.2306618581243847221, -0.2411417322834647770 ) ) ;
#74717 = CARTESIAN_POINT ( 'NONE',  ( 0.3996062992125986035, 2.446882876249141962E-17, -1.850393700787401619 ) ) ;
#74718 = CARTESIAN_POINT ( 'NONE',  ( 0.2891555358219910499, 0.2891555358219910499, -1.082677165354330784 ) ) ;
#74719 = CARTESIAN_POINT ( 'NONE',  ( -0.3460692066303960868, 0.1998031496062990242, -2.545931758530183497 ) ) ;
#74720 = CARTESIAN_POINT ( 'NONE',  ( -0.7478466213799872531, 1.968503937007873850, -0.5309055118110235227 ) ) ;
#74721 = CARTESIAN_POINT ( 'NONE',  ( 0.1958661417322834775, 0.3392501089628018884, -0.4514435695538057125 ) ) ;
#74722 = CARTESIAN_POINT ( 'NONE',  ( -0.5708661417322828946, 0.07958543189024071263, -0.2665933059059888421 ) ) ;
#74723 = CARTESIAN_POINT ( 'NONE',  ( -0.5708661417322828946, 0.1660481256975883668, -0.3530559997133364547 ) ) ;
#74724 = CARTESIAN_POINT ( 'NONE',  ( 0.2624671916010504757, -0.6046776061558809534, -0.2411417322834644161 ) ) ;
#74725 = CARTESIAN_POINT ( 'NONE',  ( -0.1058382717557497660, -0.3949938075777411073, -2.353674540682414218 ) ) ;
#74726 = CARTESIAN_POINT ( 'NONE',  ( -1.555118110236219930, -0.5400638737290845981, -0.3530559997133363437 ) ) ;
#74727 = CARTESIAN_POINT ( 'NONE',  ( 0.9908136482939640111, 0.2952755905511810774, -0.1292274648535930714 ) ) ;
#74728 = CARTESIAN_POINT ( 'NONE',  ( -0.1265901696524986964, -0.4724409448818899238, -2.434383202099737353 ) ) ;
#74729 = CARTESIAN_POINT ( 'NONE',  ( 0.1998031496062994405, -0.3460692066303958092, -1.824146981627296604 ) ) ;
#74730 = CARTESIAN_POINT ( 'NONE',  ( 1.135170603674541256, 0.2952755905511811885, 0.1292274648535926551 ) ) ;
#74731 = CIRCLE ( 'NONE', #80151, 0.3149606299212597826 ) ;
#74732 = CARTESIAN_POINT ( 'NONE',  ( 1.030183727034121421, -0.3162353388693409650, -0.4822834645669289433 ) ) ;
#74733 = CARTESIAN_POINT ( 'NONE',  ( 1.154855643044620184, 0.1283753931104746893, -0.1820866141732285504 ) ) ;
#74735 = CARTESIAN_POINT ( 'NONE',  ( -1.535433070866141225, -0.6692913385826771977, 8.415575281601705876E-17 ) ) ;
#74734 = CARTESIAN_POINT ( 'NONE',  ( -1.640419947506561060, -0.004921259842519576551, 0.3153832671262227771 ) ) ;
#74736 = CARTESIAN_POINT ( 'NONE',  ( -9.594673741351310580E-17, 0.3917322834645669549, -2.757198531987190115 ) ) ;
#74737 = FILL_AREA_STYLE_COLOUR ( '', #21132 ) ;
#74738 = CARTESIAN_POINT ( 'NONE',  ( 0.8792650918635177559, 0.05413385826771666132, 0.4176697321401328100 ) ) ;
#74739 = CARTESIAN_POINT ( 'NONE',  ( 1.358267716535433323, 0.07958543189024085140, 0.2665933059059887866 ) ) ;
#74740 = CARTESIAN_POINT ( 'NONE',  ( -0.6627296587926503335, -0.6692913385826771977, 0.1292274648535927661 ) ) ;
#74741 = CARTESIAN_POINT ( 'NONE',  ( -0.4396325459317579898, 0.2952755905511811885, 0.1292274648535926551 ) ) ;
#74742 = CARTESIAN_POINT ( 'NONE',  ( -1.587926509186350810, 0.05413385826771626580, -0.4176697321401330321 ) ) ;
#74743 = CARTESIAN_POINT ( 'NONE',  ( 0.1049643490035304938, -0.3917322834645669549, -0.1699475065616798397 ) ) ;
#74744 = CARTESIAN_POINT ( 'NONE',  ( 0.2755905511811031494, -0.6692913385826771977, 8.415575281601705876E-17 ) ) ;
#74745 =( BOUNDED_CURVE ( )  B_SPLINE_CURVE ( 2, ( #82157, #56042, #49730, #31611, #25289, #18985, #24877, #50139, #75429, #69515, #11864, #5532, #18583 ),
 .UNSPECIFIED., .F., .F. ) 
 B_SPLINE_CURVE_WITH_KNOTS ( ( 3, 2, 2, 2, 2, 2, 3 ),
 ( 0.2125000000000000222, 0.2166666666666667018, 0.2208333333333333537, 0.2250000000000000333, 0.2291666666666666852, 0.2333333333333333648, 0.2375000000000000167 ),
 .UNSPECIFIED. ) 
 CURVE ( )  GEOMETRIC_REPRESENTATION_ITEM ( )  RATIONAL_B_SPLINE_CURVE ( ( 0.9999999999999997780, 0.9659258262890685343, 1.000000000000000000, 0.9659258262890683122, 1.000000000000000000, 0.9659258262890683122, 1.000000000000000000, 0.9659258262890683122, 1.000000000000000000, 0.9659258262890683122, 1.000000000000000000, 0.9659258262890680902, 1.000000000000000222 ) ) 
 REPRESENTATION_ITEM ( '' )  );
#74746 = CARTESIAN_POINT ( 'NONE',  ( -9.594673741351313045E-17, 0.3917322834645670104, -2.196850393700787496 ) ) ;
#74747 = CARTESIAN_POINT ( 'NONE',  ( 1.620734908136483465, -0.6692913385826771977, 0.1292274648535927661 ) ) ;
#74748 = VERTEX_POINT ( 'NONE', #21679 ) ;
#74749 = CARTESIAN_POINT ( 'NONE',  ( 4.837279021331060870E-17, -0.3949938075777409963, -2.598425196850393970 ) ) ;
#74750 = EDGE_LOOP ( 'NONE', ( #10052, #80161, #22676, #73922 ) ) ;
#74751 = DIRECTION ( 'NONE',  ( -0.000000000000000000, -1.000000000000000000, -0.000000000000000000 ) ) ;
#74752 = AXIS2_PLACEMENT_3D ( 'NONE', #50700, #38494, #1046 ) ;
#74753 = CARTESIAN_POINT ( 'NONE',  ( 1.614173228346457378, 0.1771653543307087630, 0.000000000000000000 ) ) ;
#74754 = CARTESIAN_POINT ( 'NONE',  ( -0.3996062992125986035, -7.340648628747425578E-17, -1.141732283464566899 ) ) ;
#74755 = CARTESIAN_POINT ( 'NONE',  ( 1.581364829396326277, -0.2845877964562161244, -0.3641732283464567121 ) ) ;
#74756 = CARTESIAN_POINT ( 'NONE',  ( -0.1447075906223733999, 0.004960608223778823628, 0.3437734562760190182 ) ) ;
#74757 = CARTESIAN_POINT ( 'NONE',  ( 0.1273213304869930951, 0.2755905511811023723, -1.680969278250197707 ) ) ;
#74758 = CARTESIAN_POINT ( 'NONE',  ( -0.07815110806776767727, 1.950626090833269766, 0.3034832608173697599 ) ) ;
#74759 = CARTESIAN_POINT ( 'NONE',  ( 0.3917322834645669549, 0.1049643490035304660, -0.5242782152230972548 ) ) ;
#74760 = CARTESIAN_POINT ( 'NONE',  ( -0.2559055118110227234, -0.4536011799217367080, 0.2665933059059888421 ) ) ;
#74761 = CARTESIAN_POINT ( 'NONE',  ( -1.292650918635170010, -0.5511811023622046335, 0.09757992244046803654 ) ) ;
#74762 = CARTESIAN_POINT ( 'NONE',  ( 1.502624671916010790, -0.3162353388693409650, -0.4822834645669289433 ) ) ;
#74763 = CARTESIAN_POINT ( 'NONE',  ( 0.3740157480314966754, 0.1660481256975883668, -0.3530559997133364547 ) ) ;
#74764 = CARTESIAN_POINT ( 'NONE',  ( -1.456692913385826182, 0.2952755905511811885, 0.000000000000000000 ) ) ;
#74765 = CARTESIAN_POINT ( 'NONE',  ( 0.3917322834645670104, -0.1049643490035303411, -0.1036745406824146343 ) ) ;
#74766 = ORIENTED_EDGE ( 'NONE', *, *, #57094, .F. ) ;
#74767 = ADVANCED_FACE ( 'NONE', ( #1915 ), #78107, .T. ) ;
#74768 = CARTESIAN_POINT ( 'NONE',  ( 1.423884514435696191, -0.05778040916215522460, 0.4822834645669289988 ) ) ;
#74769 = CARTESIAN_POINT ( 'NONE',  ( 0.4177787735907000366, 1.299212598425196985, -1.559171609364239375 ) ) ;
#74770 = CARTESIAN_POINT ( 'NONE',  ( -0.2362204724409447953, -0.4091458600556404646, -1.482939632545931863 ) ) ;
#74771 = CARTESIAN_POINT ( 'NONE',  ( -1.646051170424378096, 0.4405861044731112508, -0.5309055118110234117 ) ) ;
#74772 = EDGE_CURVE ( 'NONE', #83292, #47997, #39368, .T. ) ;
#74773 = PLANE ( 'NONE',  #11695 ) ;
#74774 = CARTESIAN_POINT ( 'NONE',  ( -0.6036745406824141069, -0.6046776061558809534, -0.2411417322834644161 ) ) ;
#74775 = CARTESIAN_POINT ( 'NONE',  ( 1.568241469816273659, -0.05778040916215560624, -0.4822834645669293319 ) ) ;
#74777 = CARTESIAN_POINT ( 'NONE',  ( 0.6426939841807760567, 0.004960608223778823628, 0.3437734562760190182 ) ) ;
#74776 = CARTESIAN_POINT ( 'NONE',  ( -0.3458507752293906723, -0.3458507752293910609, -2.263779527559055094 ) ) ;
#74778 = CARTESIAN_POINT ( 'NONE',  ( 1.541994750656168645, 0.2952755905511810774, -0.1292274648535930714 ) ) ;
#74779 = CARTESIAN_POINT ( 'NONE',  ( -0.7808398950131225646, -0.05778040916215522460, 0.4822834645669289988 ) ) ;
#74780 = CARTESIAN_POINT ( 'NONE',  ( 0.1049643490035303689, 0.3917322834645668994, -0.2309518128270847681 ) ) ;
#74781 = CARTESIAN_POINT ( 'NONE',  ( -0.05249343832020938322, -0.5023911411419708095, -0.1820866141732282451 ) ) ;
#74782 = CARTESIAN_POINT ( 'NONE',  ( 4.797336870675656522E-17, -0.3917322834645670104, -0.3208661417322835607 ) ) ;
#74783 = CARTESIAN_POINT ( 'NONE',  ( 0.03937007874015833325, -0.5511811023622047445, 6.969142054262312111E-17 ) ) ;
#74784 = CARTESIAN_POINT ( 'NONE',  ( 0.5511811023622054106, -0.1870078740157480601, -0.3641732283464567677 ) ) ;
#74785 = CARTESIAN_POINT ( 'NONE',  ( 0.7152230971128614723, -0.3162353388693409650, -0.4822834645669289433 ) ) ;
#74786 = CARTESIAN_POINT ( 'NONE',  ( -0.2887139107611542133, -0.5023911411419708095, -0.1820866141732282451 ) ) ;
#74787 = CARTESIAN_POINT ( 'NONE',  ( -0.1958661417322836718, 0.3392501089628017219, -2.524934383202099397 ) ) ;
#74788 = CARTESIAN_POINT ( 'NONE',  ( 1.456692913385827515, 0.2952755905511811885, 0.000000000000000000 ) ) ;
#74789 = EDGE_CURVE ( 'NONE', #66895, #77098, #46092, .T. ) ;
#74790 = CARTESIAN_POINT ( 'NONE',  ( -1.213910761154854745, -0.6692913385826771977, 0.1292274648535927661 ) ) ;
#74791 = VECTOR ( 'NONE', #67664, 39.37007874015748143 ) ;
#74792 = CARTESIAN_POINT ( 'NONE',  ( 0.4724409448818897572, -0.1265901696524988906, -0.6607611548556431291 ) ) ;
#74793 = AXIS2_PLACEMENT_3D ( 'NONE', #41828, #79327, #74671 ) ;
#74794 = CARTESIAN_POINT ( 'NONE',  ( 5.463695987328526437E-16, -0.1870078740157479769, 0.4822834645669291653 ) ) ;
#74795 = ADVANCED_FACE ( 'NONE', ( #1092 ), #33484, .F. ) ;
#74796 = CARTESIAN_POINT ( 'NONE',  ( -0.3083989501312330295, -0.3162353388693409650, -0.4822834645669289433 ) ) ;
#74797 = CARTESIAN_POINT ( 'NONE',  ( 1.646981627296588035, -0.2845877964562159024, 0.3641732283464567677 ) ) ;
#74798 = CARTESIAN_POINT ( 'NONE',  ( 0.1509186351706042484, -0.2845877964562159024, 0.3641732283464567677 ) ) ;
#74799 = CARTESIAN_POINT ( 'NONE',  ( -0.3674540682414692561, -0.6046776061558809534, -0.2411417322834644161 ) ) ;
#74800 = CARTESIAN_POINT ( 'NONE',  ( -0.8202099737532799750, 0.2952755905511810774, -0.1292274648535930714 ) ) ;
#74801 = CARTESIAN_POINT ( 'NONE',  ( -3.881246834694716874, 2.729333734409945755, 0.5314960629921260393 ) ) ;
#74802 = CARTESIAN_POINT ( 'NONE',  ( 1.509186351706037543, -0.004921259842519576551, 0.3153832671262227771 ) ) ;
#74803 = CARTESIAN_POINT ( 'NONE',  ( 0.3412073490813655186, -0.6046776061558809534, -0.2411417322834644161 ) ) ;
#74804 = ORIENTED_EDGE ( 'NONE', *, *, #40435, .F. ) ;
#74805 = CARTESIAN_POINT ( 'NONE',  ( -0.3460692066303957537, -0.1998031496062994405, -1.861548556430446144 ) ) ;
#74806 = CARTESIAN_POINT ( 'NONE',  ( 1.148293963254593653, 0.2952755905511810774, -0.1292274648535930714 ) ) ;
#74807 = B_SPLINE_CURVE_WITH_KNOTS ( 'NONE', 3,
 ( #72501, #14850, #66191, #8527 ),
 .UNSPECIFIED., .F., .F.,
 ( 4, 4 ),
 ( 2.857347768991906607E-07, 0.001436604392377180406 ),
 .UNSPECIFIED. ) ;
#74808 = CARTESIAN_POINT ( 'NONE',  ( -0.6824146981627291497, -0.5023911411419708095, -0.1820866141732282451 ) ) ;
#74809 = CONICAL_SURFACE ( 'NONE', #54595, 3.543307086614174484, 0.7853981633974447263 ) ;
#74810 = CARTESIAN_POINT ( 'NONE',  ( -0.4265091863517051496, 0.2952755905511810774, -0.1292274648535930714 ) ) ;
#74811 = CARTESIAN_POINT ( 'NONE',  ( 1.476377952755906442, -0.5400638737290844871, 0.3530559997133364547 ) ) ;
#74812 = CARTESIAN_POINT ( 'NONE',  ( 0.9186351706036752773, 0.2306618581243847221, -0.2411417322834647770 ) ) ;
#74813 = FACE_OUTER_BOUND ( 'NONE', #46143, .T. ) ;
#74814 = CARTESIAN_POINT ( 'NONE',  ( -1.102362204724408601, -0.1870078740157479769, 0.3641732283464567677 ) ) ;
#74815 = CARTESIAN_POINT ( 'NONE',  ( -0.3996062992125984925, -0.1070741851644056719, -0.1227034120734908362 ) ) ;
#74816 = CARTESIAN_POINT ( 'NONE',  ( -0.1070741851644056997, 0.3996062992125986035, -0.6364829396325458744 ) ) ;
#74817 = CARTESIAN_POINT ( 'NONE',  ( -0.3917322834645670104, -0.1049643490035307020, -2.877315903708348444 ) ) ;
#74818 = CARTESIAN_POINT ( 'NONE',  ( 1.640419947506562393, -0.3690944881889763329, 0.3153832671262228327 ) ) ;
#74819 = CARTESIAN_POINT ( 'NONE',  ( 1.023622047244095112, -0.1870078740157480601, -0.3641732283464567677 ) ) ;
#74820 = CARTESIAN_POINT ( 'NONE',  ( 0.6430446194225728496, 0.05413385826771666132, 0.4176697321401328100 ) ) ;
#74821 = CARTESIAN_POINT ( 'NONE',  ( -1.561679790026246017, 0.05413385826771666132, 0.4176697321401328100 ) ) ;
#74822 = B_SPLINE_CURVE_WITH_KNOTS ( 'NONE', 3,
 ( #60728, #22843, #54827, #48502, #28744, #14887, #46845, #53990, #53574, #34235, #8566, #47261, #53153, #40547 ),
 .UNSPECIFIED., .F., .F.,
 ( 4, 2, 2, 2, 2, 2, 4 ),
 ( 0.000000000000000000, 0.0003923887041693346835, 0.0007847774083386693670, 0.001177166112508004105, 0.001569554816677338734, 0.002354332225016037266, 0.003139109633354736015 ),
 .UNSPECIFIED. ) ;
#74823 = CARTESIAN_POINT ( 'NONE',  ( 0.3420746716998660508, 0.1974969037888705814, -0.8379265091863515869 ) ) ;
#74824 = CARTESIAN_POINT ( 'NONE',  ( 0.9120734908136490793, 0.1771653543307087075, -0.09757992244046823083 ) ) ;
#74825 = CARTESIAN_POINT ( 'NONE',  ( -0.2427821522309703550, -0.3162353388693405765, 0.4822834645669290543 ) ) ;
#74826 = CARTESIAN_POINT ( 'NONE',  ( -0.6430446194225712953, 0.05413385826771626580, -0.4176697321401330321 ) ) ;
#74827 = CARTESIAN_POINT ( 'NONE',  ( 1.299212598425197429, -0.6692913385826771977, 8.415575281601705876E-17 ) ) ;
#74828 = CARTESIAN_POINT ( 'NONE',  ( -0.3458507752293906723, -0.3458507752293910609, -1.003937007874015741 ) ) ;
#74829 = CARTESIAN_POINT ( 'NONE',  ( 0.1070741851644053666, 0.3996062992125986035, -2.198162729658792447 ) ) ;
#74830 = CARTESIAN_POINT ( 'NONE',  ( -0.09842519685039295696, 0.07958543189024071263, -0.2665933059059888421 ) ) ;
#74831 = ADVANCED_FACE ( 'NONE', ( #72617 ), #71784, .F. ) ;
#74832 = ORIENTED_EDGE ( 'NONE', *, *, #55159, .F. ) ;
#74833 = CARTESIAN_POINT ( 'NONE',  ( 4.797336870675656522E-17, -0.3917322834645670659, -0.7053998932096606778 ) ) ;
#74834 = EDGE_LOOP ( 'NONE', ( #55863, #19753, #16036, #33702 ) ) ;
#74835 = CARTESIAN_POINT ( 'NONE',  ( -0.7217847769028863381, 0.05413385826771626580, -0.4176697321401330321 ) ) ;
#74836 = CARTESIAN_POINT ( 'NONE',  ( -0.01312335958005186876, 0.05413385826771626580, -0.4176697321401330321 ) ) ;
#74837 = CARTESIAN_POINT ( 'NONE',  ( -0.3083989501312330295, -0.3162353388693409650, -0.4822834645669289433 ) ) ;
#74838 = CARTESIAN_POINT ( 'NONE',  ( 0.9448818897637802916, -0.1870078740157480879, -0.4822834645669291653 ) ) ;
#74839 = CARTESIAN_POINT ( 'NONE',  ( -0.4921259842519677963, 0.1660481256975883668, -0.3530559997133364547 ) ) ;
#74840 = CARTESIAN_POINT ( 'NONE',  ( -1.286089238845143479, 0.2306618581243847221, -0.2411417322834647770 ) ) ;
#74841 = CARTESIAN_POINT ( 'NONE',  ( -0.5118110236220466680, -0.6692913385826771977, 8.415575281601705876E-17 ) ) ;
#74842 = CARTESIAN_POINT ( 'NONE',  ( 0.8070866141732288002, 0.1660481256975885056, 0.3530559997133364547 ) ) ;
#74843 = CARTESIAN_POINT ( 'NONE',  ( 0.6364829396325465405, -0.05778040916215522460, 0.4822834645669289988 ) ) ;
#74844 = EDGE_CURVE ( 'NONE', #48126, #65535, #59977, .T. ) ;
#74845 = CARTESIAN_POINT ( 'NONE',  ( 0.1958661417322834775, 0.3392501089628018884, -1.238845144356955252 ) ) ;
#74846 = CARTESIAN_POINT ( 'NONE',  ( -0.3149606299212590610, -0.1870078740157480601, -0.3641732283464567677 ) ) ;
#74847 = ORIENTED_EDGE ( 'NONE', *, *, #33021, .F. ) ;
#74848 = CARTESIAN_POINT ( 'NONE',  ( 4.837279021331060870E-17, -0.3949938075777409963, -1.653543307086614123 ) ) ;
#74849 = ORIENTED_EDGE ( 'NONE', *, *, #13007, .T. ) ;
#74850 = CARTESIAN_POINT ( 'NONE',  ( -1.469816272965878357, -0.5023911411419708095, -0.1820866141732282451 ) ) ;
#74851 = AXIS2_PLACEMENT_3D ( 'NONE', #15486, #66833, #66409 ) ;
#74852 = AXIS2_PLACEMENT_3D ( 'NONE', #75273, #5785, #4551 ) ;
#74853 = CARTESIAN_POINT ( 'NONE',  ( -0.6036745406824141069, -0.6046776061558809534, -0.2411417322834644161 ) ) ;
#74854 = CARTESIAN_POINT ( 'NONE',  ( 0.7086614173228347191, 0.000000000000000000, 0.09842519685039344268 ) ) ;
#74855 = CARTESIAN_POINT ( 'NONE',  ( -0.7283464566929126471, 0.1660481256975883668, -0.3530559997133364547 ) ) ;
#74856 = CARTESIAN_POINT ( 'NONE',  ( -0.6692913385826764205, -0.6692913385826771977, 8.415575281601705876E-17 ) ) ;
#74857 = CARTESIAN_POINT ( 'NONE',  ( -1.213910761154854745, -0.6692913385826771977, 0.1292274648535927661 ) ) ;
#74858 = CARTESIAN_POINT ( 'NONE',  ( -1.732283464566928277, -0.1870078740157479769, 0.4822834645669291653 ) ) ;
#74859 = CARTESIAN_POINT ( 'NONE',  ( 1.023622047244095334, -0.1870078740157479769, 0.3641732283464567677 ) ) ;
#74860 = CARTESIAN_POINT ( 'NONE',  ( 0.4735861421683033035, 1.569672585540540899, 1.017206702362611903 ) ) ;
#74861 = CARTESIAN_POINT ( 'NONE',  ( -0.3392501089628019995, 0.1958661417322832277, 0.2040682414698161695 ) ) ;
#74862 = CARTESIAN_POINT ( 'NONE',  ( 0.02624671916010564918, 0.1283753931104748280, 0.1820866141732283561 ) ) ;
#74863 = CARTESIAN_POINT ( 'NONE',  ( -0.3871391076115476282, -0.05778040916215522460, 0.4822834645669289988 ) ) ;
#74864 = CARTESIAN_POINT ( 'NONE',  ( -0.1509186351706028884, -0.3162353388693409650, -0.4822834645669289433 ) ) ;
#74865 = VERTEX_POINT ( 'NONE', #52820 ) ;
#74866 = CARTESIAN_POINT ( 'NONE',  ( 0.3460692066303959757, -0.1998031496062991907, -1.994750656167979086 ) ) ;
#74867 = CARTESIAN_POINT ( 'NONE',  ( 0.2465595919007004533, 6.148515279637353769E-16, 0.4281993546915524584 ) ) ;
#74868 = ORIENTED_EDGE ( 'NONE', *, *, #68011, .T. ) ;
#74869 = CARTESIAN_POINT ( 'NONE',  ( 4.893765752498283308E-17, -0.3996062992125985480, -1.572834645669291431 ) ) ;
#74870 = CARTESIAN_POINT ( 'NONE',  ( -0.1502491711592395529, 0.2549859370038549122, 0.1564451348283543985 ) ) ;
#74871 = CARTESIAN_POINT ( 'NONE',  ( -0.5839895013123351797, 0.1771653543307087075, -0.09757992244046823083 ) ) ;
#74872 = CARTESIAN_POINT ( 'NONE',  ( -0.9186351706036736120, 0.2306618581243848609, 0.2411417322834645549 ) ) ;
#74873 = CARTESIAN_POINT ( 'NONE',  ( 0.4724409448818896462, 0.1265901696524990294, -0.5971128608923884640 ) ) ;
#74874 = FACE_OUTER_BOUND ( 'NONE', #12612, .T. ) ;
#74875 = CARTESIAN_POINT ( 'NONE',  ( 0.3917322834645670104, -0.1049643490035303411, -2.400918635170603554 ) ) ;
#74876 = CARTESIAN_POINT ( 'NONE',  ( 1.246719160104987623, 0.05413385826771626580, -0.4176697321401330321 ) ) ;
#74877 = CARTESIAN_POINT ( 'NONE',  ( 0.6430446194225728496, 0.05413385826771666132, 0.4176697321401328100 ) ) ;
#74878 = CARTESIAN_POINT ( 'NONE',  ( 0.5183727034120741983, -0.6692913385826771977, 0.1292274648535927661 ) ) ;
#74879 = CARTESIAN_POINT ( 'NONE',  ( -0.4527559055118102749, -0.4536011799217368745, -0.2665933059059886201 ) ) ;
#74880 = CARTESIAN_POINT ( 'NONE',  ( -0.5052493438320203589, -0.6692913385826771977, 0.1292274648535927661 ) ) ;
#74881 = CARTESIAN_POINT ( 'NONE',  ( -0.1265901696524993347, 0.4724409448818895907, -2.288057742782152015 ) ) ;
#74882 = CARTESIAN_POINT ( 'NONE',  ( -0.2952755905511804668, 0.1660481256975885056, 0.3530559997133364547 ) ) ;
#74883 = CARTESIAN_POINT ( 'NONE',  ( -0.1058382717557503072, 0.3949938075777408852, -2.130577427821521930 ) ) ;
#74884 = CARTESIAN_POINT ( 'NONE',  ( 1.443569553805774897, 0.1283753931104748280, 0.1820866141732283561 ) ) ;
#74885 = CARTESIAN_POINT ( 'NONE',  ( -0.3215223097112853146, -0.2845877964562159024, 0.3641732283464567677 ) ) ;
#74886 = CARTESIAN_POINT ( 'NONE',  ( 1.259842519685040019, -0.1870078740157480601, -0.3641732283464567677 ) ) ;
#74887 = CARTESIAN_POINT ( 'NONE',  ( -1.528871391076114250, 0.2952755905511810774, -0.1292274648535930714 ) ) ;
#74888 = CARTESIAN_POINT ( 'NONE',  ( -1.003937007874014853, 0.07958543189024085140, 0.2665933059059887866 ) ) ;
#74889 = CARTESIAN_POINT ( 'NONE',  ( 1.614173228346457378, 0.2952755905511811885, 0.000000000000000000 ) ) ;
#74890 = CARTESIAN_POINT ( 'NONE',  ( -1.305774278215222184, -0.6692913385826773087, -0.1292274648535924053 ) ) ;
#74891 = CARTESIAN_POINT ( 'NONE',  ( -0.4002624671916004129, -0.3162353388693405765, 0.4822834645669290543 ) ) ;
#74892 = CARTESIAN_POINT ( 'NONE',  ( -2.058019426306472166, 1.301092492065855089, 0.4123476441529934644 ) ) ;
#74893 = CARTESIAN_POINT ( 'NONE',  ( 0.3871391076115493490, -0.2845877964562159024, 0.3641732283464567677 ) ) ;
#74894 = CARTESIAN_POINT ( 'NONE',  ( -1.502624671916009680, -0.08942795157528024563, -0.3641732283464568787 ) ) ;
#74895 = CARTESIAN_POINT ( 'NONE',  ( 0.6233595800524942554, -0.05778040916215560624, -0.4822834645669293319 ) ) ;
#74896 = CARTESIAN_POINT ( 'NONE',  ( -1.699475065616797398, 0.1771653543307087630, 0.09757992244046791164 ) ) ;
#74897 = CARTESIAN_POINT ( 'NONE',  ( 1.377952755905512472, -0.5511811023622047445, 6.969142054262312111E-17 ) ) ;
#74898 = CARTESIAN_POINT ( 'NONE',  ( -1.082677165354329896, 0.1660481256975885056, 0.3530559997133364547 ) ) ;
#74899 = CARTESIAN_POINT ( 'NONE',  ( -0.4790026246719152336, -0.08942795157528024563, -0.3641732283464568787 ) ) ;
#74900 = CARTESIAN_POINT ( 'NONE',  ( 0.1181102362204724254, 8.537024980200824098E-18, 0.000000000000000000 ) ) ;
#74901 = CARTESIAN_POINT ( 'NONE',  ( 0.2887139107611556010, -0.5023911411419708095, 0.1820866141732285504 ) ) ;
#74902 = CARTESIAN_POINT ( 'NONE',  ( -0.09842519685039295696, -0.5400638737290844871, 0.3530559997133364547 ) ) ;
#74903 = CARTESIAN_POINT ( 'NONE',  ( 0.1070741851644053388, 0.3996062992125986035, -0.8576115485564304031 ) ) ;
#74904 = AXIS2_PLACEMENT_3D ( 'NONE', #56421, #25256, #24436 ) ;
#74905 = CARTESIAN_POINT ( 'NONE',  ( 0.1049643490035303689, 0.3917322834645670104, -1.967847769028871374 ) ) ;
#74906 = CARTESIAN_POINT ( 'NONE',  ( 0.7414698162729663755, -0.5511811023622048555, -0.09757992244046775898 ) ) ;
#74908 = VECTOR ( 'NONE', #41312, 39.37007874015748143 ) ;
#74907 = CARTESIAN_POINT ( 'NONE',  ( 0.08530183727034192087, -0.05778040916215522460, 0.4822834645669289988 ) ) ;
#74909 = VECTOR ( 'NONE', #13476, 39.37007874015748143 ) ;
#74910 = CARTESIAN_POINT ( 'NONE',  ( -0.7742782152230962556, -0.4281496062992127816, -0.4176697321401328100 ) ) ;
#74911 = CARTESIAN_POINT ( 'NONE',  ( -0.8005249343832011588, -0.004921259842519870586, -0.3153832671262229437 ) ) ;
#74912 = DIRECTION ( 'NONE',  ( 0.000000000000000000, 1.000000000000000000, 0.000000000000000000 ) ) ;
#74913 = CARTESIAN_POINT ( 'NONE',  ( -0.4658792650918627265, -0.2845877964562161244, -0.3641732283464567121 ) ) ;
#74914 = CARTESIAN_POINT ( 'NONE',  ( -0.1574803149606292529, -0.1870078740157480879, -0.4822834645669291653 ) ) ;
#74915 = EDGE_CURVE ( 'NONE', #44566, #13764, #5097, .T. ) ;
#74916 = CARTESIAN_POINT ( 'NONE',  ( -1.174540682414697335, -0.2845877964562161244, -0.3641732283464567121 ) ) ;
#74917 = CARTESIAN_POINT ( 'NONE',  ( 0.2925321140481932369, 0.2925321140481932369, -1.474409448818897905 ) ) ;
#74918 = CARTESIAN_POINT ( 'NONE',  ( -1.601049868766403650, 0.2306618581243847221, -0.2411417322834647770 ) ) ;
#74919 = CARTESIAN_POINT ( 'NONE',  ( 0.4621018179204952614, 1.702998256715020864E-15, -0.4281989832122452544 ) ) ;
#74920 = ORIENTED_EDGE ( 'NONE', *, *, #69249, .T. ) ;
#74921 = ADVANCED_FACE ( 'NONE', ( #27992 ), #28407, .F. ) ;
#74922 = CARTESIAN_POINT ( 'NONE',  ( -1.489501312335957062, -0.2845877964562161244, -0.3641732283464567121 ) ) ;
#74923 = CARTESIAN_POINT ( 'NONE',  ( -0.3280839895013117347, -0.4281496062992124485, 0.4176697321401328655 ) ) ;
#74924 = CARTESIAN_POINT ( 'NONE',  ( -1.023622047244093558, -0.1870078740157479769, 0.4822834645669291653 ) ) ;
#74925 = CARTESIAN_POINT ( 'NONE',  ( -0.3917322834645671215, 0.1049643490035301469, -1.692257217847769057 ) ) ;
#74926 = CARTESIAN_POINT ( 'NONE',  ( 0.000000000000000000, 2.755905511811024056, 0.000000000000000000 ) ) ;
#74927 = CARTESIAN_POINT ( 'NONE',  ( 1.194225721784777594, 0.05413385826771666132, 0.4176697321401328100 ) ) ;
#74928 = CARTESIAN_POINT ( 'NONE',  ( 0.4133858267716541968, 0.1660481256975885056, 0.3530559997133364547 ) ) ;
#74929 = FACE_BOUND ( 'NONE', #80561, .T. ) ;
#74930 = CARTESIAN_POINT ( 'NONE',  ( 0.3460692066303958092, 0.1998031496062993018, -2.255249343832021136 ) ) ;
#74931 = CARTESIAN_POINT ( 'NONE',  ( 1.515748031496063186, -0.4536011799217368745, -0.2665933059059886201 ) ) ;
#74932 = CARTESIAN_POINT ( 'NONE',  ( 0.2925321140481932369, 0.2925321140481932369, -0.7677165354330709457 ) ) ;
#74933 = ORIENTED_EDGE ( 'NONE', *, *, #32543, .T. ) ;
#74934 = CARTESIAN_POINT ( 'NONE',  ( -0.7545931758530176614, -0.5511811023622048555, -0.09757992244046775898 ) ) ;
#74935 = CARTESIAN_POINT ( 'NONE',  ( -0.3917322834645671215, 0.1049643490035301469, -2.544619422572177658 ) ) ;
#74936 = ORIENTED_EDGE ( 'NONE', *, *, #2885, .F. ) ;
#74937 = CARTESIAN_POINT ( 'NONE',  ( 0.5380577427821529035, 0.05413385826771626580, -0.4176697321401330321 ) ) ;
#74938 = CARTESIAN_POINT ( 'NONE',  ( -0.5708661417322828946, 0.1660481256975883668, -0.3530559997133364547 ) ) ;
#74939 = CARTESIAN_POINT ( 'NONE',  ( -1.200787401574802349, -0.5400638737290844871, 0.3530559997133364547 ) ) ;
#74940 = CARTESIAN_POINT ( 'NONE',  ( 0.8595800524934390507, -0.3162353388693405765, 0.4822834645669290543 ) ) ;
#74941 = CARTESIAN_POINT ( 'NONE',  ( -1.423884514435694859, -0.08942795157528024563, -0.3641732283464568787 ) ) ;
#74942 = DIRECTION ( 'NONE',  ( -0.000000000000000000, -1.000000000000000000, -0.000000000000000000 ) ) ;
#74943 = CARTESIAN_POINT ( 'NONE',  ( -0.04593175853018302557, 0.2952755905511811885, 0.1292274648535926551 ) ) ;
#74944 = CARTESIAN_POINT ( 'NONE',  ( -1.286089238845143479, 0.2306618581243847221, -0.2411417322834647770 ) ) ;
#74945 = CARTESIAN_POINT ( 'NONE',  ( 0.1049643490035303689, 0.3917322834645668994, -1.805754962433383737 ) ) ;
#74946 = CARTESIAN_POINT ( 'NONE',  ( -1.620734908136482577, 0.2952755905511811885, 0.1292274648535926551 ) ) ;
#74947 = CARTESIAN_POINT ( 'NONE',  ( 0.1181102362204724532, 0.09842519685039372024, 0.000000000000000000 ) ) ;
#74948 = CARTESIAN_POINT ( 'NONE',  ( -0.1049643490035302024, -0.3917322834645671215, 0.09317585301837273681 ) ) ;
#74949 = CARTESIAN_POINT ( 'NONE',  ( 0.9186351706036752773, 0.1283753931104746893, -0.1820866141732285504 ) ) ;
#74950 = ORIENTED_EDGE ( 'NONE', *, *, #16635, .F. ) ;
#74951 = CARTESIAN_POINT ( 'NONE',  ( -0.1058382717557503211, 0.3949938075777409408, -0.1640419947506562559 ) ) ;
#74952 = CARTESIAN_POINT ( 'NONE',  ( -0.9908136482939626788, 0.2952755905511811885, 0.1292274648535926551 ) ) ;
#74953 = ORIENTED_EDGE ( 'NONE', *, *, #35152, .T. ) ;
#74954 = CARTESIAN_POINT ( 'NONE',  ( -0.1115485564304456306, 0.1771653543307087075, -0.09757992244046823083 ) ) ;
#74955 = CARTESIAN_POINT ( 'NONE',  ( -1.594488188976377563, -0.5400638737290844871, 0.3530559997133364547 ) ) ;
#74956 = CARTESIAN_POINT ( 'NONE',  ( 0.4724409448818904789, -0.1870078740157479769, 0.4822834645669291653 ) ) ;
#74957 = CARTESIAN_POINT ( 'NONE',  ( 0.3018372703412079971, -0.4281496062992124485, 0.4176697321401328655 ) ) ;
#74958 = CARTESIAN_POINT ( 'NONE',  ( -0.2821522309711278487, 0.2952755905511811885, 0.1292274648535926551 ) ) ;
#74959 = CARTESIAN_POINT ( 'NONE',  ( 0.1049643490035303967, 0.3917322834645670659, -1.407499630742469199 ) ) ;
#74960 = CARTESIAN_POINT ( 'NONE',  ( -0.6364829396325453192, -0.05778040916215560624, -0.4822834645669293319 ) ) ;
#74961 = CARTESIAN_POINT ( 'NONE',  ( 0.1958661417322836440, -0.3392501089628017219, -2.853674540682414662 ) ) ;
#74962 = CARTESIAN_POINT ( 'NONE',  ( 1.522309711286089939, -0.5023911411419708095, -0.1820866141732282451 ) ) ;
#74963 = CARTESIAN_POINT ( 'NONE',  ( -1.062992125984250968, -0.6692913385826771977, 8.415575281601705876E-17 ) ) ;
#74964 = CARTESIAN_POINT ( 'NONE',  ( 0.8727034120734913358, -0.05778040916215522460, 0.4822834645669289988 ) ) ;
#74965 = CARTESIAN_POINT ( 'NONE',  ( 1.299212598425197429, -0.6692913385826771977, 8.415575281601705876E-17 ) ) ;
#74966 = CARTESIAN_POINT ( 'NONE',  ( 0.2925321140481932369, -0.2925321140481932369, -0.8858267716535430658 ) ) ;
#74967 = CARTESIAN_POINT ( 'NONE',  ( -0.8989501312335946848, 0.2952755905511810774, -0.1292274648535930714 ) ) ;
#74968 = CARTESIAN_POINT ( 'NONE',  ( -0.3996062992125985480, -7.340648628747423112E-17, -0.1161417322834645827 ) ) ;
#74969 = CARTESIAN_POINT ( 'NONE',  ( 0.2624671916010504757, -0.6046776061558809534, -0.2411417322834644161 ) ) ;
#74970 = CARTESIAN_POINT ( 'NONE',  ( -0.1070741851644056997, 0.3996062992125986035, -2.368766404199475151 ) ) ;
#74971 = CARTESIAN_POINT ( 'NONE',  ( -0.6561679790026240244, 0.2306618581243847221, -0.2411417322834647770 ) ) ;
#74972 = CIRCLE ( 'NONE', #58784, 0.1771653543307085410 ) ;
#74973 = CARTESIAN_POINT ( 'NONE',  ( -1.535433070866141225, -0.5511811023622047445, 6.969142054262312111E-17 ) ) ;
#74974 = CARTESIAN_POINT ( 'NONE',  ( 0.5446194225721792126, -0.2845877964562159024, 0.3641732283464567677 ) ) ;
#74975 = CARTESIAN_POINT ( 'NONE',  ( 1.266404199475066328, -0.05778040916215522460, 0.4822834645669289988 ) ) ;
#74976 = CARTESIAN_POINT ( 'NONE',  ( -0.2362204724409447953, -0.4091458600556404646, -1.244750656167979086 ) ) ;
#74977 = CARTESIAN_POINT ( 'NONE',  ( 0.9055118110236227702, 0.1771653543307087630, 0.000000000000000000 ) ) ;
#74978 = CARTESIAN_POINT ( 'NONE',  ( 0.8464566929133865436, 0.1660481256975883668, -0.3530559997133364547 ) ) ;
#74979 = CARTESIAN_POINT ( 'NONE',  ( 0.3949938075777409408, -0.1058382717557499186, -0.6607611548556431291 ) ) ;
#74980 = CARTESIAN_POINT ( 'NONE',  ( -0.6627296587926503335, -0.6692913385826771977, 0.1292274648535927661 ) ) ;
#74981 = LINE ( 'NONE', #24021, #12288 ) ;
#74982 = CARTESIAN_POINT ( 'NONE',  ( 0.8267716535433077274, 0.1771653543307087630, 0.000000000000000000 ) ) ;
#74983 = CARTESIAN_POINT ( 'NONE',  ( -0.6102362204724400829, 0.1660481256975885056, 0.3530559997133364547 ) ) ;
#74984 = CARTESIAN_POINT ( 'NONE',  ( -0.07217847769028813698, -0.3162353388693409650, -0.4822834645669289433 ) ) ;
#74985 = CARTESIAN_POINT ( 'NONE',  ( 0.4581426849250296862, 1.664615899758173034, -1.024278008493450409 ) ) ;
#74986 = CARTESIAN_POINT ( 'NONE',  ( 0.03937007874015806264, 0.2952755905511811885, 0.000000000000000000 ) ) ;
#74987 = CARTESIAN_POINT ( 'NONE',  ( 0.1443569553805781891, -0.004921259842519870586, -0.3153832671262229437 ) ) ;
#74988 = CARTESIAN_POINT ( 'NONE',  ( -2.704370107879186413, 1.253873987468420603, 0.3814095263789963330 ) ) ;
#74989 = CARTESIAN_POINT ( 'NONE',  ( 0.1902887139107617975, -0.5511811023622048555, -0.09757992244046775898 ) ) ;
#74990 = CARTESIAN_POINT ( 'NONE',  ( 0.5446194225721792126, -0.08942795157528024563, -0.3641732283464568787 ) ) ;
#74991 = DIRECTION ( 'NONE',  ( 0.000000000000000000, 1.000000000000000000, 0.000000000000000000 ) ) ;
#74992 = CARTESIAN_POINT ( 'NONE',  ( -0.1070741851644056997, 0.3996062992125984925, -1.658136482939632339 ) ) ;
#74993 = CARTESIAN_POINT ( 'NONE',  ( 0.3871391076115493490, -0.3162353388693405765, 0.4822834645669290543 ) ) ;
#74994 = CARTESIAN_POINT ( 'NONE',  ( -0.3917322834645669549, -0.1049643490035306603, -1.455380577427821676 ) ) ;
#74995 = CARTESIAN_POINT ( 'NONE',  ( 0.2247243262887798632, -4.135162568743707313E-16, -0.3791483426435169890 ) ) ;
#74996 = CARTESIAN_POINT ( 'NONE',  ( -0.1906283239483360925, -0.3428707098288028554, -2.110585413283057979E-17 ) ) ;
#74997 = CARTESIAN_POINT ( 'NONE',  ( -0.3477690288713905509, -0.5511811023622046335, 0.09757992244046803654 ) ) ;
#74998 = CARTESIAN_POINT ( 'NONE',  ( -0.2559055118110227234, -0.5400638737290844871, 0.3530559997133364547 ) ) ;
#74999 = CARTESIAN_POINT ( 'NONE',  ( 1.030183727034121421, -0.08942795157527998196, 0.3641732283464567121 ) ) ;
#75000 = CARTESIAN_POINT ( 'NONE',  ( 0.4620341399816233485, 1.428627056473853241, -1.022509594724332116 ) ) ;
#75001 = CARTESIAN_POINT ( 'NONE',  ( -1.397637795275589623, 0.1660481256975885056, 0.3530559997133364547 ) ) ;
#75002 = CARTESIAN_POINT ( 'NONE',  ( 0.2230971128608932319, -0.4281496062992124485, 0.4176697321401328655 ) ) ;
#75003 = CARTESIAN_POINT ( 'NONE',  ( 1.364829396325460076, 0.2306618581243848609, 0.2411417322834645549 ) ) ;
#75004 = CARTESIAN_POINT ( 'NONE',  ( 0.08529443231574072859, 1.070420337342308459, -1.857273270772795026 ) ) ;
#75005 = CARTESIAN_POINT ( 'NONE',  ( 0.2230971128608929543, 0.05413385826771626580, -0.4176697321401330321 ) ) ;
#75006 = CARTESIAN_POINT ( 'NONE',  ( 1.515748031496063408, 0.1660481256975885056, 0.3530559997133364547 ) ) ;
#75007 = CARTESIAN_POINT ( 'NONE',  ( 0.3477690288713918276, -0.6692913385826773087, -0.1292274648535924053 ) ) ;
#75008 = CARTESIAN_POINT ( 'NONE',  ( -1.603475055217291612, 1.330568129716839909, 0.04573490813648253134 ) ) ;
#75009 = CARTESIAN_POINT ( 'NONE',  ( 0.8333333333333340365, -0.5511811023622046335, 0.09757992244046803654 ) ) ;
#75010 = CARTESIAN_POINT ( 'NONE',  ( 1.404199475065617708, 0.05413385826771626580, -0.4176697321401330321 ) ) ;
#75011 = EDGE_CURVE ( 'NONE', #3706, #36535, #80340, .T. ) ;
#75012 = CARTESIAN_POINT ( 'NONE',  ( 0.1640419947506569498, -0.08942795157527998196, 0.3641732283464567121 ) ) ;
#75013 = CARTESIAN_POINT ( 'NONE',  ( -0.4133858267716528645, -0.5400638737290844871, 0.3530559997133364547 ) ) ;
#75014 = CARTESIAN_POINT ( 'NONE',  ( 0.4921259842519691285, 0.1660481256975885056, 0.3530559997133364547 ) ) ;
#75015 = CARTESIAN_POINT ( 'NONE',  ( -0.2165354330708654795, 0.1660481256975885056, 0.3530559997133364547 ) ) ;
#75016 = CARTESIAN_POINT ( 'NONE',  ( 0.1958661417322834775, 0.3392501089628018884, -2.030859210794962344 ) ) ;
#75017 = CARTESIAN_POINT ( 'NONE',  ( -0.4068241469816267775, -0.004921259842519870586, -0.3153832671262229437 ) ) ;
#75018 = CARTESIAN_POINT ( 'NONE',  ( 0.8923884514435701520, -0.6046776061558809534, -0.2411417322834644161 ) ) ;
#75019 = CARTESIAN_POINT ( 'NONE',  ( 0.9908136482939640111, -0.5511811023622046335, 0.09757992244046803654 ) ) ;
#75020 = CARTESIAN_POINT ( 'NONE',  ( 0.04593175853018440641, -0.6692913385826771977, 0.1292274648535927661 ) ) ;
#75021 = CARTESIAN_POINT ( 'NONE',  ( -1.661807552036326463, 1.149545036241496510, 0.2732228506959576420 ) ) ;
#75023 = CARTESIAN_POINT ( 'NONE',  ( 1.594488188976378673, 0.1660481256975885056, 0.3530559997133364547 ) ) ;
#75022 = CARTESIAN_POINT ( 'NONE',  ( -0.5314960629921349211, 2.729656497683583538, 2.556891340746902053 ) ) ;
#75024 = CARTESIAN_POINT ( 'NONE',  ( -0.3917322834645670104, -7.196005306013484475E-17, -2.078740157480314821 ) ) ;
#75025 = AXIS2_PLACEMENT_3D ( 'NONE', #7615, #58948, #1306 ) ;
#75026 = CARTESIAN_POINT ( 'NONE',  ( -1.325459317585300889, 0.05413385826771666132, 0.4176697321401328100 ) ) ;
#75027 = CARTESIAN_POINT ( 'NONE',  ( -0.5774278215223089816, 0.2306618581243847221, -0.2411417322834647770 ) ) ;
#75028 = CARTESIAN_POINT ( 'NONE',  ( -0.1265901696524993347, 0.4724409448818895907, -0.1640419947506561726 ) ) ;
#75029 = CARTESIAN_POINT ( 'NONE',  ( -0.1974969037888706647, 0.3420746716998658843, -2.847769028871391495 ) ) ;
#75030 = ORIENTED_EDGE ( 'NONE', *, *, #12573, .F. ) ;
#75031 = CARTESIAN_POINT ( 'NONE',  ( 0.4790026246719168435, -0.2845877964562161244, -0.3641732283464567121 ) ) ;
#75032 = CARTESIAN_POINT ( 'NONE',  ( -0.2867679344610364334, -0.2867679344610367109, -1.468503937007874294 ) ) ;
#75033 = CARTESIAN_POINT ( 'NONE',  ( 0.7677165354330716118, -0.5400638737290844871, 0.3530559997133364547 ) ) ;
#75034 = CARTESIAN_POINT ( 'NONE',  ( -0.3458507752293906723, -0.3458507752293910609, -2.578740157480315265 ) ) ;
#75035 = DIRECTION ( 'NONE',  ( -1.000000000000000000, -8.673617379884021667E-16, 0.000000000000000000 ) ) ;
#75036 = CARTESIAN_POINT ( 'NONE',  ( 1.174540682414699111, -0.3162353388693405765, 0.4822834645669290543 ) ) ;
#75037 = CARTESIAN_POINT ( 'NONE',  ( 1.167979002624672580, -0.004921259842519870586, -0.3153832671262229437 ) ) ;
#75038 = CARTESIAN_POINT ( 'NONE',  ( 0.4396325459317593221, 0.2952755905511810774, -0.1292274648535930714 ) ) ;
#75039 = CARTESIAN_POINT ( 'NONE',  ( -0.1958661417322834497, -0.3392501089628018884, -0.9330515503598931781 ) ) ;
#75040 = CARTESIAN_POINT ( 'NONE',  ( -0.3280839895013117347, 0.05413385826771626580, -0.4176697321401330321 ) ) ;
#75041 = CARTESIAN_POINT ( 'NONE',  ( -0.9383202099737524282, -0.08942795157527998196, 0.3641732283464567121 ) ) ;
#75042 = CARTESIAN_POINT ( 'NONE',  ( 0.2624671916010504757, -0.6046776061558809534, -0.2411417322834644161 ) ) ;
#75043 = CARTESIAN_POINT ( 'NONE',  ( 0.05905511811023681640, 0.1660481256975883668, -0.3530559997133364547 ) ) ;
#75044 = FACE_OUTER_BOUND ( 'NONE', #6282, .T. ) ;
#75045 = PLANE ( 'NONE',  #58391 ) ;
#75046 = CARTESIAN_POINT ( 'NONE',  ( -0.1049643490035302301, -0.3917322834645671770, -2.116161048065303696 ) ) ;
#75047 = CARTESIAN_POINT ( 'NONE',  ( 1.010498687664042716, -0.4281496062992124485, 0.4176697321401328655 ) ) ;
#75048 = CARTESIAN_POINT ( 'NONE',  ( -0.2821522309711278487, 0.2952755905511811885, 0.1292274648535926551 ) ) ;
#75049 = CARTESIAN_POINT ( 'NONE',  ( -1.397637795275589623, -0.5400638737290845981, -0.3530559997133363437 ) ) ;
#75050 = CARTESIAN_POINT ( 'NONE',  ( 1.299212598425197429, 0.2952755905511811885, 0.000000000000000000 ) ) ;
#75051 = CARTESIAN_POINT ( 'NONE',  ( 0.3280839895013130669, -0.4281496062992127816, -0.4176697321401328100 ) ) ;
#75052 = CARTESIAN_POINT ( 'NONE',  ( 0.3392501089628018329, 0.1958661417322835607, -0.8458005249343831800 ) ) ;
#75053 = CARTESIAN_POINT ( 'NONE',  ( -0.8727034120734901146, -0.05778040916215560624, -0.4822834645669293319 ) ) ;
#75054 = CARTESIAN_POINT ( 'NONE',  ( 0.05905511811023709395, -0.5400638737290844871, 0.3530559997133364547 ) ) ;
#75055 = CARTESIAN_POINT ( 'NONE',  ( -0.5183727034120726440, 0.2952755905511811885, 0.1292274648535926551 ) ) ;
#75056 = CARTESIAN_POINT ( 'NONE',  ( 0.3412073490813655186, -0.5023911411419708095, -0.1820866141732282451 ) ) ;
#75057 = CARTESIAN_POINT ( 'NONE',  ( -1.725721784776902190, -0.05778040916215522460, 0.4822834645669289988 ) ) ;
#75058 = CARTESIAN_POINT ( 'NONE',  ( -1.692913385826770645, 0.2952755905511811885, 0.000000000000000000 ) ) ;
#75059 = CARTESIAN_POINT ( 'NONE',  ( 0.3018372703412079971, -0.4281496062992124485, 0.4176697321401328655 ) ) ;
#75060 = CARTESIAN_POINT ( 'NONE',  ( 1.423884514435696191, -0.05778040916215522460, 0.4822834645669289988 ) ) ;
#75061 = CARTESIAN_POINT ( 'NONE',  ( 0.3392501089628018884, -0.1958661417322834220, -2.774278215223096922 ) ) ;
#75062 = ORIENTED_EDGE ( 'NONE', *, *, #51779, .F. ) ;
#75063 = VERTEX_POINT ( 'NONE', #46924 ) ;
#75064 = CARTESIAN_POINT ( 'NONE',  ( 0.8661417322834653598, -0.1870078740157479769, 0.4822834645669291653 ) ) ;
#75065 = CARTESIAN_POINT ( 'NONE',  ( 0.01968503937007930540, 0.07958543189024085140, 0.2665933059059887866 ) ) ;
#75067 = DIRECTION ( 'NONE',  ( 0.000000000000000000, -1.408710688920637755E-15, -1.000000000000000000 ) ) ;
#75066 = PLANE ( 'NONE',  #8192 ) ;
#75068 = CARTESIAN_POINT ( 'NONE',  ( 0.3917322834645670104, 2.398668435337828261E-17, -0.9901574803149607584 ) ) ;
#75069 = CARTESIAN_POINT ( 'NONE',  ( -0.4724409448818899238, 0.1265901696524986686, 0.2053805774278214813 ) ) ;
#75070 = LENGTH_MEASURE_WITH_UNIT ( LENGTH_MEASURE( 0.02539999999999999897 ), #62419 );
#75071 = CARTESIAN_POINT ( 'NONE',  ( 0.3996062992125986035, -0.1070741851644052972, -2.235564304461942431 ) ) ;
#75072 = CARTESIAN_POINT ( 'NONE',  ( 0.6299212598425204535, -0.1870078740157479769, 0.4822834645669291653 ) ) ;
#75073 = CARTESIAN_POINT ( 'NONE',  ( -0.6102362204724400829, -0.5400638737290845981, -0.3530559997133363437 ) ) ;
#75074 = CARTESIAN_POINT ( 'NONE',  ( -0.9251968503937002541, 0.1660481256975885056, 0.3530559997133364547 ) ) ;
#75075 = CARTESIAN_POINT ( 'NONE',  ( 0.6430446194225728496, 0.05413385826771666132, 0.4176697321401328100 ) ) ;
#75076 = CARTESIAN_POINT ( 'NONE',  ( 1.496062992125984703, -0.1870078740157480879, -0.4822834645669291653 ) ) ;
#75077 = CARTESIAN_POINT ( 'NONE',  ( 1.181102362204725198, -0.1870078740157479769, 0.3641732283464567677 ) ) ;
#75078 = CARTESIAN_POINT ( 'NONE',  ( 1.227034120734908917, 0.1771653543307087075, -0.09757992244046823083 ) ) ;
#75079 = CARTESIAN_POINT ( 'NONE',  ( -0.8989501312335946848, -0.6692913385826771977, 0.1292274648535927661 ) ) ;
#75080 = CARTESIAN_POINT ( 'NONE',  ( -0.2925321140481930149, -0.2925321140481933480, -0.2933070866141732069 ) ) ;
#75081 = CARTESIAN_POINT ( 'NONE',  ( -1.561679790026246017, -0.3690944881889765550, -0.3153832671262227771 ) ) ;
#75082 = CARTESIAN_POINT ( 'NONE',  ( -0.1958661417322834220, -0.3392501089628018884, -0.05774278215223092176 ) ) ;
#75083 = CARTESIAN_POINT ( 'NONE',  ( -0.3477690288713902178, 0.2952755905511810774, -0.1292274648535930714 ) ) ;
#75085 = CARTESIAN_POINT ( 'NONE',  ( -0.7080320533160967544, 1.900312960331933976, 0.5309055118110236338 ) ) ;
#75084 = CARTESIAN_POINT ( 'NONE',  ( 1.017060367454068803, -0.3162353388693405765, 0.4822834645669290543 ) ) ;
#75086 = CARTESIAN_POINT ( 'NONE',  ( -1.253280839895012377, -0.08942795157527998196, 0.3641732283464567121 ) ) ;
#75087 = CARTESIAN_POINT ( 'NONE',  ( 0.4855643044619430415, -0.4281496062992127816, -0.4176697321401328100 ) ) ;
#75088 = CARTESIAN_POINT ( 'NONE',  ( 0.9514435695538062676, -0.08942795157527998196, 0.3641732283464567121 ) ) ;
#75089 = CARTESIAN_POINT ( 'NONE',  ( 0.3917322834645669549, 2.398668435337827645E-17, -1.615466248522622550 ) ) ;
#75090 = CARTESIAN_POINT ( 'NONE',  ( -1.404199475065615932, -0.004921259842519576551, 0.3153832671262227771 ) ) ;
#75091 = CARTESIAN_POINT ( 'NONE',  ( 1.286089238845145033, -0.6046776061558809534, -0.2411417322834644161 ) ) ;
#75092 = DIRECTION ( 'NONE',  ( 0.000000000000000000, 1.000000000000000000, -0.000000000000000000 ) ) ;
#75093 = CARTESIAN_POINT ( 'NONE',  ( -0.6627296587926503335, -0.5511811023622046335, 0.09757992244046803654 ) ) ;
#75094 = CARTESIAN_POINT ( 'NONE',  ( -0.1246719160104980823, 0.2952755905511811885, 0.1292274648535926551 ) ) ;
#75095 = CARTESIAN_POINT ( 'NONE',  ( -1.463254593175852492, 0.1771653543307087630, 0.09757992244046791164 ) ) ;
#75096 = CARTESIAN_POINT ( 'NONE',  ( -0.6233595800524928121, -0.05778040916215522460, 0.4822834645669289988 ) ) ;
#75097 = CARTESIAN_POINT ( 'NONE',  ( 1.233595800524935227, 0.2306618581243847221, -0.2411417322834647770 ) ) ;
#75098 = CARTESIAN_POINT ( 'NONE',  ( 0.1049643490035304799, -0.3917322834645670104, -0.3970009430784271487 ) ) ;
#75099 = CARTESIAN_POINT ( 'NONE',  ( -0.8464566929133852113, 0.07958543189024085140, 0.2665933059059887866 ) ) ;
#75100 = ADVANCED_FACE ( 'NONE', ( #8644 ), #62232, .F. ) ;
#75101 = DIRECTION ( 'NONE',  ( 0.000000000000000000, 1.000000000000000000, 0.000000000000000000 ) ) ;
#75102 = CARTESIAN_POINT ( 'NONE',  ( 1.548556430446194954, -0.6046776061558807314, 0.2411417322834647770 ) ) ;
#75103 = CARTESIAN_POINT ( 'NONE',  ( -0.4091458600556405756, 0.2362204724409446288, -1.992782152230971437 ) ) ;
#75104 = CARTESIAN_POINT ( 'NONE',  ( -1.227034120734907585, 0.2952755905511811885, 0.1292274648535926551 ) ) ;
#75105 = CARTESIAN_POINT ( 'NONE',  ( -1.286089238845143479, 0.1283753931104746893, -0.1820866141732285504 ) ) ;
#75106 = CARTESIAN_POINT ( 'NONE',  ( -0.7152230971128602510, -0.08942795157528024563, -0.3641732283464568787 ) ) ;
#75108 = CARTESIAN_POINT ( 'NONE',  ( -1.594488188976377119, 0.1660481256975883668, -0.3530559997133364547 ) ) ;
#75107 =( BOUNDED_CURVE ( )  B_SPLINE_CURVE ( 2, ( #65434, #1449, #65843, #27106, #21626, #51931, #79308, #72976, #27941, #47287, #78894, #7336, #39738 ),
 .UNSPECIFIED., .F., .F. ) 
 B_SPLINE_CURVE_WITH_KNOTS ( ( 3, 2, 2, 2, 2, 2, 3 ),
 ( 0.2375000000000000167, 0.2416666666666666963, 0.2458333333333333204, 0.2500000000000000000, 0.2541666666666666519, 0.2583333333333333037, 0.2624999999999999556 ),
 .UNSPECIFIED. ) 
 CURVE ( )  GEOMETRIC_REPRESENTATION_ITEM ( )  RATIONAL_B_SPLINE_CURVE ( ( 0.9999999999999997780, 0.9659258262890685343, 1.000000000000000000, 0.9659258262890683122, 1.000000000000000000, 0.9659258262890683122, 1.000000000000000000, 0.9659258262890683122, 1.000000000000000000, 0.9659258262890683122, 1.000000000000000000, 0.9659258262890687563, 0.9999999999999995559 ) ) 
 REPRESENTATION_ITEM ( '' )  );
#75109 = CARTESIAN_POINT ( 'NONE',  ( 0.05249343832021075018, -0.6046776061558807314, 0.2411417322834647770 ) ) ;
#75110 = CARTESIAN_POINT ( 'NONE',  ( -0.2099737532808391705, 0.1283753931104748280, 0.1820866141732283561 ) ) ;
#75111 = CARTESIAN_POINT ( 'NONE',  ( -1.345144356955379816, -0.08942795157528024563, -0.3641732283464568787 ) ) ;
#75112 = CARTESIAN_POINT ( 'NONE',  ( -1.535433070866141225, 0.2952755905511811885, 0.000000000000000000 ) ) ;
#75113 = CARTESIAN_POINT ( 'NONE',  ( 1.528871391076116026, -0.5511811023622048555, -0.09757992244046775898 ) ) ;
#75114 = EDGE_CURVE ( 'NONE', #54535, #7865, #67539, .T. ) ;
#75115 = CARTESIAN_POINT ( 'NONE',  ( 1.062992125984252745, 0.2952755905511811885, 0.000000000000000000 ) ) ;
#75116 = CARTESIAN_POINT ( 'NONE',  ( 0.1340670299283531486, 1.082026165109806648, 1.867989472054414346 ) ) ;
#75117 = CARTESIAN_POINT ( 'NONE',  ( 0.5183727034120741983, -0.5511811023622046335, 0.09757992244046803654 ) ) ;
#75118 = CARTESIAN_POINT ( 'NONE',  ( 0.7414698162729663755, 0.2952755905511811885, 0.1292274648535926551 ) ) ;
#75119 = CARTESIAN_POINT ( 'NONE',  ( 1.115485564304462551, -0.004921259842519576551, 0.3153832671262227771 ) ) ;
#75120 = EDGE_LOOP ( 'NONE', ( #54954, #40036, #4143, #44461 ) ) ;
#75121 = CARTESIAN_POINT ( 'NONE',  ( -1.299212598425196097, 0.2952755905511811885, 0.000000000000000000 ) ) ;
#75122 = CARTESIAN_POINT ( 'NONE',  ( -0.9383202099737524282, -0.3162353388693409650, -0.4822834645669289433 ) ) ;
#75123 = CARTESIAN_POINT ( 'NONE',  ( 0.06561679790026316017, 0.05413385826771626580, -0.4176697321401330321 ) ) ;
#75124 = DIRECTION ( 'NONE',  ( 0.000000000000000000, 1.000000000000000000, 0.000000000000000000 ) ) ;
#75125 = CARTESIAN_POINT ( 'NONE',  ( 0.2925321140481932369, 0.2925321140481932369, -2.261811023622047223 ) ) ;
#75126 = CARTESIAN_POINT ( 'NONE',  ( 0.3674540682414705883, 0.2306618581243847221, -0.2411417322834647770 ) ) ;
#75127 = CARTESIAN_POINT ( 'NONE',  ( -1.673228346456691717, 0.1660481256975883668, -0.3530559997133364547 ) ) ;
#75128 = CARTESIAN_POINT ( 'NONE',  ( 0.1049868766404206816, 0.2306618581243848609, 0.2411417322834645549 ) ) ;
#75129 = CARTESIAN_POINT ( 'NONE',  ( 0.7086614173228352742, -0.1870078740157480879, -0.4822834645669291653 ) ) ;
#75130 = CARTESIAN_POINT ( 'NONE',  ( 0.3460692066303959757, -0.1998031496062991907, -1.837270341207349000 ) ) ;
#75131 = CARTESIAN_POINT ( 'NONE',  ( 0.2891555358219910499, 0.2891555358219910499, -1.712598425196850682 ) ) ;
#75132 = CARTESIAN_POINT ( 'NONE',  ( -0.4713486786305523535, 1.475001655854108584, 1.018266755655268474 ) ) ;
#75133 = CARTESIAN_POINT ( 'NONE',  ( -1.586052503253849055, 0.4724409448818907564, -0.1653254495020551051 ) ) ;
#75134 = CARTESIAN_POINT ( 'NONE',  ( -0.3392501089628019995, 0.1958661417322832277, -0.6482939632545930975 ) ) ;
#75135 = CARTESIAN_POINT ( 'NONE',  ( -0.6233595800524928121, -0.08942795157527998196, 0.3641732283464567121 ) ) ;
#75136 = CARTESIAN_POINT ( 'NONE',  ( -0.8661417322834640276, -0.1870078740157480879, -0.4822834645669291653 ) ) ;
#75137 = CARTESIAN_POINT ( 'NONE',  ( 0.6102362204724416372, -0.5400638737290844871, 0.3530559997133364547 ) ) ;
#75138 = CARTESIAN_POINT ( 'NONE',  ( -0.3949938075777411073, 0.1058382717557497660, -1.999343832020997747 ) ) ;
#75139 = CARTESIAN_POINT ( 'NONE',  ( 1.030183727034121421, -0.05778040916215522460, 0.4822834645669289988 ) ) ;
#75140 = CARTESIAN_POINT ( 'NONE',  ( 1.528871391076116026, -0.6692913385826773087, -0.1292274648535924053 ) ) ;
#75141 = CARTESIAN_POINT ( 'NONE',  ( 1.272965879265092637, 0.05413385826771666132, 0.4176697321401328100 ) ) ;
#75142 = CARTESIAN_POINT ( 'NONE',  ( -0.4724409448818899238, 0.1265901696524986686, -2.395013123359580387 ) ) ;
#75143 = CARTESIAN_POINT ( 'NONE',  ( -9.787531504996567848E-17, 0.3996062992125986035, -1.732283464566929165 ) ) ;
#75144 = CARTESIAN_POINT ( 'NONE',  ( 0.4724409448818897017, 0.1265901696524990294, -2.721128608923884862 ) ) ;
#75145 = CARTESIAN_POINT ( 'NONE',  ( 1.095800524934383846, -0.3162353388693405765, 0.4822834645669290543 ) ) ;
#75146 = CARTESIAN_POINT ( 'NONE',  ( 0.5971128608923890191, -0.6692913385826771977, 0.1292274648535927661 ) ) ;
#75147 = CARTESIAN_POINT ( 'NONE',  ( 1.338582677165355062, -0.1870078740157480601, -0.3641732283464567677 ) ) ;
#75149 = CARTESIAN_POINT ( 'NONE',  ( 1.568241469816273437, -0.3162353388693405765, 0.4822834645669290543 ) ) ;
#75148 = CARTESIAN_POINT ( 'NONE',  ( 1.686351706036745890, 0.2952755905511811885, 0.1292274648535926551 ) ) ;
#75150 = CARTESIAN_POINT ( 'NONE',  ( 0.2867679344610365999, -0.2867679344610365999, -2.855623728837584085 ) ) ;
#75151 = CARTESIAN_POINT ( 'NONE',  ( -1.595398199321656607, 1.288687073698533414, 0.1559797534342480252 ) ) ;
#75152 = CARTESIAN_POINT ( 'NONE',  ( 0.8136482939632553313, -0.6046776061558809534, -0.2411417322834644161 ) ) ;
#75153 = FACE_OUTER_BOUND ( 'NONE', #22973, .T. ) ;
#75154 = CARTESIAN_POINT ( 'NONE',  ( -0.4133858267716528645, 0.1660481256975883668, -0.3530559997133364547 ) ) ;
#75155 = CARTESIAN_POINT ( 'NONE',  ( -0.7020997375328076329, -0.3162353388693409650, -0.4822834645669289433 ) ) ;
#75156 = CARTESIAN_POINT ( 'NONE',  ( 1.594488188976378673, 0.1660481256975885056, 0.3530559997133364547 ) ) ;
#75157 = CARTESIAN_POINT ( 'NONE',  ( -0.3392501089628019995, 0.1958661417322832277, -0.2683727034120735877 ) ) ;
#75158 = CARTESIAN_POINT ( 'NONE',  ( 5.463695987328526437E-16, -0.1870078740157479769, 0.4822834645669291653 ) ) ;
#75159 = CARTESIAN_POINT ( 'NONE',  ( 4.797336870675656522E-17, -0.3917322834645670104, -2.118110236220472675 ) ) ;
#75160 = CARTESIAN_POINT ( 'NONE',  ( -1.646981627296586703, -0.08942795157527998196, 0.3641732283464567121 ) ) ;
#75161 = VERTEX_POINT ( 'NONE', #35143 ) ;
#75162 = CARTESIAN_POINT ( 'NONE',  ( -0.3949938075777411628, 0.1058382717557497937, -2.709973753280840114 ) ) ;
#75163 = VERTEX_POINT ( 'NONE', #42271 ) ;
#75164 = CARTESIAN_POINT ( 'NONE',  ( 0.2460629921259843422, 0.000000000000000000, 0.1181102362204723977 ) ) ;
#75165 = CARTESIAN_POINT ( 'NONE',  ( 1.496062992125984703, -0.1870078740157480601, -0.3641732283464567677 ) ) ;
#75166 = CARTESIAN_POINT ( 'NONE',  ( 0.3996062992125986035, 2.446882876249141962E-17, -1.220472440944881942 ) ) ;
#75167 = DIRECTION ( 'NONE',  ( 0.000000000000000000, 0.000000000000000000, -1.000000000000000000 ) ) ;
#75168 = CARTESIAN_POINT ( 'NONE',  ( 0.3458507752293908943, -0.3458507752293908943, -0.8051181102362204856 ) ) ;
#75169 = CARTESIAN_POINT ( 'NONE',  ( 0.000000000000000000, 2.755905511811024056, -3.937007874015748143 ) ) ;
#75170 = DIRECTION ( 'NONE',  ( -3.491481338843132961E-15, 0.000000000000000000, 1.000000000000000000 ) ) ;
#75171 = CARTESIAN_POINT ( 'NONE',  ( 0.1958661417322836440, -0.3392501089628017219, -0.4914698162729659869 ) ) ;
#75172 = CARTESIAN_POINT ( 'NONE',  ( -0.7939632545931750718, -0.08942795157528024563, -0.3641732283464568787 ) ) ;
#75173 = CARTESIAN_POINT ( 'NONE',  ( -1.154855643044618851, -0.5023911411419708095, -0.1820866141732282451 ) ) ;
#75174 = CARTESIAN_POINT ( 'NONE',  ( -1.535433070866141225, -0.6692913385826771977, 8.415575281601705876E-17 ) ) ;
#75175 = CARTESIAN_POINT ( 'NONE',  ( 0.5905511811023629321, -0.6692913385826771977, 8.415575281601705876E-17 ) ) ;
#75176 = CARTESIAN_POINT ( 'NONE',  ( -1.233595800524933894, -0.6046776061558809534, -0.2411417322834644161 ) ) ;
#75177 = CARTESIAN_POINT ( 'NONE',  ( 0.2867679344610365999, -0.2867679344610365444, -0.09055118110236216877 ) ) ;
#75178 = ORIENTED_EDGE ( 'NONE', *, *, #37233, .T. ) ;
#75179 = CARTESIAN_POINT ( 'NONE',  ( 1.496062992125984703, -0.1870078740157480879, -0.4822834645669291653 ) ) ;
#75180 = CARTESIAN_POINT ( 'NONE',  ( 1.403614904275686858E-14, 1.537401574803149984, -3.937007874015761910 ) ) ;
#75181 = CARTESIAN_POINT ( 'NONE',  ( -0.2362204724409451284, 0.4091458600556402425, -1.745406824146981561 ) ) ;
#75182 = CARTESIAN_POINT ( 'NONE',  ( 0.1500752278769513226, 0.2544983382031791308, 0.1555222293686583102 ) ) ;
#75183 = CARTESIAN_POINT ( 'NONE',  ( 0.2362204724409449064, 0.4091458600556404646, -0.9317585301837270073 ) ) ;
#75184 = CARTESIAN_POINT ( 'NONE',  ( -0.7874015748031489847, -0.1870078740157480879, -0.4822834645669291653 ) ) ;
#75185 = CARTESIAN_POINT ( 'NONE',  ( 1.030183727034121421, -0.05778040916215522460, 0.4822834645669289988 ) ) ;
#75187 = CARTESIAN_POINT ( 'NONE',  ( -0.3458507752293906723, -0.3458507752293910609, -1.948818897637795144 ) ) ;
#75186 = DIRECTION ( 'NONE',  ( 0.000000000000000000, 1.000000000000000000, 0.000000000000000000 ) ) ;
#75188 = AXIS2_PLACEMENT_3D ( 'NONE', #58362, #25958, #40269 ) ;
#75189 = CARTESIAN_POINT ( 'NONE',  ( 1.476377952755906442, -0.5400638737290844871, 0.3530559997133364547 ) ) ;
#75190 = CARTESIAN_POINT ( 'NONE',  ( -1.318897637795274802, -0.5400638737290845981, -0.3530559997133363437 ) ) ;
#75191 = CARTESIAN_POINT ( 'NONE',  ( 0.3917322834645668994, 0.1049643490035304522, -0.5196657235882398140 ) ) ;
#75192 = CARTESIAN_POINT ( 'NONE',  ( 0.09842519685039434474, -0.4536011799217368745, -0.2665933059059886201 ) ) ;
#75193 = CARTESIAN_POINT ( 'NONE',  ( 0.2867679344610366554, 0.2867679344610366554, -0.5374015748031496509 ) ) ;
#75194 = CARTESIAN_POINT ( 'NONE',  ( -0.2427821522309703550, -0.2845877964562159024, 0.3641732283464567677 ) ) ;
#75195 = CARTESIAN_POINT ( 'NONE',  ( 0.6627296587926515548, 0.1771653543307087630, 0.09757992244046791164 ) ) ;
#75196 = CARTESIAN_POINT ( 'NONE',  ( 0.4133858267716541968, -0.5400638737290845981, -0.3530559997133363437 ) ) ;
#75197 = CARTESIAN_POINT ( 'NONE',  ( -0.5183727034120726440, 0.1771653543307087630, 0.09757992244046791164 ) ) ;
#75198 = CARTESIAN_POINT ( 'NONE',  ( 0.3917322834645670104, -0.1049643490035303411, -2.308398950131233640 ) ) ;
#75199 = CARTESIAN_POINT ( 'NONE',  ( -1.548556430446193399, -0.6046776061558809534, -0.2411417322834644161 ) ) ;
#75200 = CARTESIAN_POINT ( 'NONE',  ( -1.154855643044618851, 0.2306618581243848609, 0.2411417322834645549 ) ) ;
#75201 = CARTESIAN_POINT ( 'NONE',  ( -0.4091458600556405756, 0.2362204724409446288, -0.8904199475065617264 ) ) ;
#75202 = CARTESIAN_POINT ( 'NONE',  ( 0.1181102362204730916, -0.6692913385826771977, 8.415575281601705876E-17 ) ) ;
#75203 = CARTESIAN_POINT ( 'NONE',  ( -0.6889763779527552368, 0.1660481256975885056, 0.3530559997133364547 ) ) ;
#75204 = CARTESIAN_POINT ( 'NONE',  ( 1.187664041994751285, -0.08942795157527998196, 0.3641732283464567121 ) ) ;
#75205 = CARTESIAN_POINT ( 'NONE',  ( 0.3018372703412079971, -0.3690944881889763329, 0.3153832671262228327 ) ) ;
#75206 = CARTESIAN_POINT ( 'NONE',  ( -0.2099737532808391705, -0.6046776061558809534, -0.2411417322834644161 ) ) ;
#75207 = CARTESIAN_POINT ( 'NONE',  ( -0.9448818897637790704, -0.1870078740157480879, -0.4822834645669291653 ) ) ;
#75208 = LINE ( 'NONE', #43184, #76157 ) ;
#75209 = CARTESIAN_POINT ( 'NONE',  ( -0.4724409448818898682, -8.678599364036362592E-17, -0.3543307086614173040 ) ) ;
#75210 = CARTESIAN_POINT ( 'NONE',  ( 0.02624671916010564918, -0.6046776061558809534, -0.2411417322834644161 ) ) ;
#75211 = ORIENTED_EDGE ( 'NONE', *, *, #47963, .F. ) ;
#75212 = CARTESIAN_POINT ( 'NONE',  ( 0.3996062992125984925, 0.1070741851644054637, -1.776246719160104570 ) ) ;
#75213 = CARTESIAN_POINT ( 'NONE',  ( 0.9973753280839902091, 0.2306618581243847221, -0.2411417322834647770 ) ) ;
#75214 = CARTESIAN_POINT ( 'NONE',  ( -0.7874015748031489847, -0.1870078740157479769, 0.3641732283464567677 ) ) ;
#75215 = CARTESIAN_POINT ( 'NONE',  ( -0.5577427821522301654, -0.05778040916215560624, -0.4822834645669293319 ) ) ;
#75216 = CARTESIAN_POINT ( 'NONE',  ( 1.338582677165355062, -0.1870078740157479769, 0.4822834645669291653 ) ) ;
#75217 = CARTESIAN_POINT ( 'NONE',  ( 0.9383202099737538715, -0.05778040916215560624, -0.4822834645669293319 ) ) ;
#75218 = CARTESIAN_POINT ( 'NONE',  ( -1.502624671916009680, -0.3162353388693405765, 0.4822834645669290543 ) ) ;
#75219 = CARTESIAN_POINT ( 'NONE',  ( -1.266404199475064773, -0.2845877964562159024, 0.3641732283464567677 ) ) ;
#75220 = CARTESIAN_POINT ( 'NONE',  ( -0.2925321140481930149, -0.2925321140481933480, -0.4507874015748031815 ) ) ;
#75221 = CARTESIAN_POINT ( 'NONE',  ( -0.3460692066303958092, -0.1998031496062994683, -0.6824146981627295938 ) ) ;
#75222 = CARTESIAN_POINT ( 'NONE',  ( 0.2891555358219910499, 0.2891555358219910499, -0.2952755905511811885 ) ) ;
#75223 = CARTESIAN_POINT ( 'NONE',  ( 1.653543307086614789, -0.1870078740157479769, 0.3641732283464567677 ) ) ;
#75224 = EDGE_CURVE ( 'NONE', #33617, #41461, #54210, .T. ) ;
#75225 = CARTESIAN_POINT ( 'NONE',  ( 0.8989501312335963501, -0.5511811023622048555, -0.09757992244046775898 ) ) ;
#75226 = CARTESIAN_POINT ( 'NONE',  ( 0.4265091863517067039, -0.6692913385826773087, -0.1292274648535924053 ) ) ;
#75227 = CARTESIAN_POINT ( 'NONE',  ( 1.535433070866142335, -0.6692913385826771977, 8.415575281601705876E-17 ) ) ;
#75228 = CARTESIAN_POINT ( 'NONE',  ( -9.674558042662122972E-17, 0.3949938075777409963, -0.8641732283464566011 ) ) ;
#75229 = CARTESIAN_POINT ( 'NONE',  ( 0.7808398950131241190, -0.08942795157528024563, -0.3641732283464568787 ) ) ;
#75230 =( BOUNDED_CURVE ( )  B_SPLINE_CURVE ( 2, ( #45990, #79681, #47658, #14038, #59465, #1406, #2232, #78432, #8961, #39695, #53968, #65386, #1816 ),
 .UNSPECIFIED., .F., .F. ) 
 B_SPLINE_CURVE_WITH_KNOTS ( ( 3, 2, 2, 2, 2, 2, 3 ),
 ( 0.6875000000000000000, 0.6916666666666666519, 0.6958333333333333037, 0.6999999999999999556, 0.7041666666666666075, 0.7083333333333332593, 0.7124999999999999112 ),
 .UNSPECIFIED. ) 
 CURVE ( )  GEOMETRIC_REPRESENTATION_ITEM ( )  RATIONAL_B_SPLINE_CURVE ( ( 1.000000000000000000, 0.9659258262890683122, 1.000000000000000000, 0.9659258262890683122, 1.000000000000000000, 0.9659258262890683122, 1.000000000000000000, 0.9659258262890683122, 1.000000000000000000, 0.9659258262890683122, 1.000000000000000000, 0.9659258262890692004, 0.9999999999999991118 ) ) 
 REPRESENTATION_ITEM ( '' )  );
#75231 = CARTESIAN_POINT ( 'NONE',  ( -0.2624671916010490880, -0.6046776061558807314, 0.2411417322834647770 ) ) ;
#75232 = CARTESIAN_POINT ( 'NONE',  ( -0.6692913385826764205, 0.2952755905511811885, 0.000000000000000000 ) ) ;
#75233 = CARTESIAN_POINT ( 'NONE',  ( 1.108923884514436686, -0.3162353388693409650, -0.4822834645669289433 ) ) ;
#75234 = CARTESIAN_POINT ( 'NONE',  ( 0.3458507752293908943, -0.3458507752293908943, -1.358267716535433101 ) ) ;
#75235 = CARTESIAN_POINT ( 'NONE',  ( -0.3996062992125986035, -7.340648628747425578E-17, -2.401574803149606474 ) ) ;
#75236 = CARTESIAN_POINT ( 'NONE',  ( -0.2296587926509179312, -0.2845877964562161244, -0.3641732283464567121 ) ) ;
#75237 = ORIENTED_EDGE ( 'NONE', *, *, #71143, .F. ) ;
#75238 = CARTESIAN_POINT ( 'NONE',  ( 0.1049643490035303967, 0.3917322834645670659, -0.7775783708999494115 ) ) ;
#75239 = ORIENTED_EDGE ( 'NONE', *, *, #14066, .T. ) ;
#75240 = CARTESIAN_POINT ( 'NONE',  ( -1.043307086614172707, 0.1660481256975883668, -0.3530559997133364547 ) ) ;
#75241 = CARTESIAN_POINT ( 'NONE',  ( -0.04593175853018302557, 0.2952755905511811885, 0.1292274648535926551 ) ) ;
#75242 = CARTESIAN_POINT ( 'NONE',  ( -0.2755905511811015396, -0.6692913385826771977, 8.415575281601705876E-17 ) ) ;
#75243 = CARTESIAN_POINT ( 'NONE',  ( 0.3412073490813655186, -0.6046776061558809534, -0.2411417322834644161 ) ) ;
#75244 = CARTESIAN_POINT ( 'NONE',  ( -0.6430446194225712953, 0.05413385826771626580, -0.4176697321401330321 ) ) ;
#75245 = CARTESIAN_POINT ( 'NONE',  ( -1.463254593175852492, 0.2952755905511811885, 0.1292274648535926551 ) ) ;
#75246 = CARTESIAN_POINT ( 'NONE',  ( -0.8727034120734901146, -0.05778040916215560624, -0.4822834645669293319 ) ) ;
#75247 = CARTESIAN_POINT ( 'NONE',  ( 0.9645669291338588858, 0.1660481256975885056, 0.3530559997133364547 ) ) ;
#75248 = CARTESIAN_POINT ( 'NONE',  ( 0.6758530183727039509, 0.2952755905511810774, -0.1292274648535930714 ) ) ;
#75249 = EDGE_CURVE ( 'NONE', #62570, #63201, #59290, .T. ) ;
#75250 = CARTESIAN_POINT ( 'NONE',  ( -0.1958661417322834220, -0.3392501089628018884, -1.160104986876640210 ) ) ;
#75251 = CARTESIAN_POINT ( 'NONE',  ( -0.4199475065616791736, -0.5023911411419708095, 0.1820866141732285504 ) ) ;
#75252 = ORIENTED_EDGE ( 'NONE', *, *, #33485, .F. ) ;
#75253 = CARTESIAN_POINT ( 'NONE',  ( -0.1974969037888703871, -0.3420746716998661063, -1.482939632545931863 ) ) ;
#75254 = ORIENTED_EDGE ( 'NONE', *, *, #19393, .T. ) ;
#75255 = CARTESIAN_POINT ( 'NONE',  ( -1.305774278215222184, -0.5511811023622048555, -0.09757992244046775898 ) ) ;
#75256 = CARTESIAN_POINT ( 'NONE',  ( -0.9120734908136475250, -0.6692913385826773087, -0.1292274648535924053 ) ) ;
#75257 = CARTESIAN_POINT ( 'NONE',  ( -0.2559055118110227234, -0.5400638737290844871, 0.3530559997133364547 ) ) ;
#75258 = CARTESIAN_POINT ( 'NONE',  ( -0.1998031496062991907, -0.3460692066303959757, 0.09186351706036742504 ) ) ;
#75259 = CARTESIAN_POINT ( 'NONE',  ( -0.7939632545931754048, -0.3162353388693405765, 0.4822834645669290543 ) ) ;
#75260 = CARTESIAN_POINT ( 'NONE',  ( -0.8792650918635160906, 0.05413385826771626580, -0.4176697321401330321 ) ) ;
#75261 = DIRECTION ( 'NONE',  ( 0.000000000000000000, 0.000000000000000000, -1.000000000000000000 ) ) ;
#75262 = LINE ( 'NONE', #55459, #71147 ) ;
#75263 = B_SPLINE_CURVE_WITH_KNOTS ( 'NONE', 3,
 ( #19298, #50858, #18886, #26450 ),
 .UNSPECIFIED., .F., .F.,
 ( 4, 4 ),
 ( 0.06769753431378609798, 0.06787032835250683682 ),
 .UNSPECIFIED. ) ;
#75264 = CARTESIAN_POINT ( 'NONE',  ( 0.9973753280839902091, -0.5023911411419708095, 0.1820866141732285504 ) ) ;
#75265 = DIRECTION ( 'NONE',  ( -0.000000000000000000, -1.000000000000000000, -0.000000000000000000 ) ) ;
#75266 = CARTESIAN_POINT ( 'NONE',  ( 0.2867679344610365999, -0.2867679344610365444, 0.1318897637795274913 ) ) ;
#75267 = CARTESIAN_POINT ( 'NONE',  ( 0.03280839895013198948, 0.1771653543307087630, 0.09757992244046791164 ) ) ;
#75268 = CARTESIAN_POINT ( 'NONE',  ( -0.5708661417322825615, -0.5400638737290844871, 0.3530559997133364547 ) ) ;
#75269 = CARTESIAN_POINT ( 'NONE',  ( 1.614173228346457156, 1.496062992125984037, -0.5309055118110239668 ) ) ;
#75270 = CARTESIAN_POINT ( 'NONE',  ( 0.09186351706036827158, 0.05413385826771666132, 0.4176697321401328100 ) ) ;
#75271 = ORIENTED_EDGE ( 'NONE', *, *, #39342, .T. ) ;
#75272 = CARTESIAN_POINT ( 'NONE',  ( -0.1070741851644051862, -0.3996062992125987146, -2.119422572178477626 ) ) ;
#75273 = CARTESIAN_POINT ( 'NONE',  ( 0.7086614173228347191, 0.000000000000000000, 0.000000000000000000 ) ) ;
#75274 = ORIENTED_EDGE ( 'NONE', *, *, #76979, .T. ) ;
#75275 = CARTESIAN_POINT ( 'NONE',  ( 0.1998031496062992463, 0.3460692066303959202, -1.480971128608923548 ) ) ;
#75276 = FACE_OUTER_BOUND ( 'NONE', #59724, .T. ) ;
#75277 = CARTESIAN_POINT ( 'NONE',  ( -0.6299212598425188991, -0.1870078740157479769, 0.3641732283464567677 ) ) ;
#75278 = CARTESIAN_POINT ( 'NONE',  ( -0.9055118110236215490, 0.2952755905511811885, 0.000000000000000000 ) ) ;
#75279 = CARTESIAN_POINT ( 'NONE',  ( 0.4091458600556403535, 0.2362204724409449896, -0.6036745406824146620 ) ) ;
#75280 = CARTESIAN_POINT ( 'NONE',  ( -0.2376021588233629689, 1.126485847204533597, 3.929855605829966514 ) ) ;
#75281 = CARTESIAN_POINT ( 'NONE',  ( 0.3392501089628018884, -0.1958661417322834220, -2.866797900262466836 ) ) ;
#75282 = CARTESIAN_POINT ( 'NONE',  ( 1.358267716535433323, 0.1660481256975885056, 0.3530559997133364547 ) ) ;
#75283 = CARTESIAN_POINT ( 'NONE',  ( 0.2690288713910767848, -0.6692913385826773087, -0.1292274648535924053 ) ) ;
#75284 = CARTESIAN_POINT ( 'NONE',  ( 0.4068241469816281097, 0.05413385826771666132, 0.4176697321401328100 ) ) ;
#75285 = CARTESIAN_POINT ( 'NONE',  ( -0.7939632545931750718, -0.08942795157528024563, -0.3641732283464568787 ) ) ;
#75286 = CARTESIAN_POINT ( 'NONE',  ( -0.2230971128608915943, -0.4281496062992127816, -0.4176697321401328100 ) ) ;
#75287 = CARTESIAN_POINT ( 'NONE',  ( 0.1265901696524990294, -0.4724409448818896462, -2.366797900262467280 ) ) ;
#75288 = CARTESIAN_POINT ( 'NONE',  ( -0.9711286089238838626, -0.6046776061558807314, 0.2411417322834647770 ) ) ;
#75289 = CARTESIAN_POINT ( 'NONE',  ( -0.3949938075777408852, -0.1058382717557502933, -2.169947506561679784 ) ) ;
#75290 = CARTESIAN_POINT ( 'NONE',  ( 1.345144356955381593, -0.2845877964562161244, -0.3641732283464567121 ) ) ;
#75291 = CARTESIAN_POINT ( 'NONE',  ( -0.4527559055118102749, 0.07958543189024085140, 0.2665933059059887866 ) ) ;
#75292 = CARTESIAN_POINT ( 'NONE',  ( 1.253280839895013710, -0.08942795157528024563, -0.3641732283464568787 ) ) ;
#75293 = CARTESIAN_POINT ( 'NONE',  ( -1.515748031496062076, 0.1660481256975883668, -0.3530559997133364547 ) ) ;
#75294 = CARTESIAN_POINT ( 'NONE',  ( -0.9711286089238838626, 0.1283753931104746893, -0.1820866141732285504 ) ) ;
#75295 = CARTESIAN_POINT ( 'NONE',  ( -0.2362204724409447953, -0.4091458600556404646, -2.189632545931758489 ) ) ;
#75296 = CARTESIAN_POINT ( 'NONE',  ( 0.6036745406824154392, 0.1283753931104746893, -0.1820866141732285504 ) ) ;
#75297 = CARTESIAN_POINT ( 'NONE',  ( -0.4790026246719152336, -0.05778040916215560624, -0.4822834645669293319 ) ) ;
#75298 = CARTESIAN_POINT ( 'NONE',  ( 0.2478063387913472249, 0.02791078216816225699, 0.4328096321851905293 ) ) ;
#75299 = CARTESIAN_POINT ( 'NONE',  ( 0.1181102362204730916, 0.1771653543307087630, 0.000000000000000000 ) ) ;
#75300 = CARTESIAN_POINT ( 'NONE',  ( -1.640419947506561060, -0.3690944881889765550, -0.3153832671262227771 ) ) ;
#75301 = CARTESIAN_POINT ( 'NONE',  ( 0.7677165354330716118, 0.1660481256975883668, -0.3530559997133364547 ) ) ;
#75302 = CARTESIAN_POINT ( 'NONE',  ( 0.2229926280064457034, 0.1936066689571366295, 0.1399704324547694778 ) ) ;
#75303 = CARTESIAN_POINT ( 'NONE',  ( 1.272965879265092637, -0.004921259842519576551, 0.3153832671262227771 ) ) ;
#75304 = CARTESIAN_POINT ( 'NONE',  ( -0.9514435695538050464, -0.3162353388693405765, 0.4822834645669290543 ) ) ;
#75305 = CARTESIAN_POINT ( 'NONE',  ( -0.2887139107611542133, -0.5023911411419708095, -0.1820866141732282451 ) ) ;
#75306 = CARTESIAN_POINT ( 'NONE',  ( -1.603475055217291612, 0.9922665159524542977, 0.04573490813648251746 ) ) ;
#75307 = CARTESIAN_POINT ( 'NONE',  ( 0.3412073490813655186, 0.1283753931104748280, 0.1820866141732283561 ) ) ;
#75308 = CARTESIAN_POINT ( 'NONE',  ( -0.7086614173228339419, -0.1870078740157479769, 0.4822834645669291653 ) ) ;
#75309 = CARTESIAN_POINT ( 'NONE',  ( -0.2925321140481932369, 0.2925321140481931259, -0.7263779527559056648 ) ) ;
#75310 = CARTESIAN_POINT ( 'NONE',  ( -0.3917322834645669549, -0.1049643490035306603, -2.335301837270341352 ) ) ;
#75311 = CARTESIAN_POINT ( 'NONE',  ( 0.4724409448818904789, -0.1870078740157479769, 0.3641732283464567677 ) ) ;
#75312 = CARTESIAN_POINT ( 'NONE',  ( -0.3608923884514428360, 0.2952755905511811885, 0.1292274648535926551 ) ) ;
#75313 = CARTESIAN_POINT ( 'NONE',  ( -0.8989501312335946848, -0.6692913385826771977, 0.1292274648535927661 ) ) ;
#75314 = CARTESIAN_POINT ( 'NONE',  ( -0.8661417322834640276, -0.1870078740157479769, 0.3641732283464567677 ) ) ;
#75315 = CARTESIAN_POINT ( 'NONE',  ( -3.923617024849349377, 1.191103570792281241, 0.3246236190342044470 ) ) ;
#75316 = CARTESIAN_POINT ( 'NONE',  ( -0.07217847769028787330, -0.05778040916215522460, 0.4822834645669289988 ) ) ;
#75317 = CARTESIAN_POINT ( 'NONE',  ( -1.167979002624671470, -0.3690944881889765550, -0.3153832671262227771 ) ) ;
#75318 = CARTESIAN_POINT ( 'NONE',  ( -1.391076115485563314, -0.6046776061558809534, -0.2411417322834644161 ) ) ;
#75319 = CARTESIAN_POINT ( 'NONE',  ( 0.2165354330708668951, 0.1012011053420775880, -0.2882089793578257453 ) ) ;
#75320 = ORIENTED_EDGE ( 'NONE', *, *, #81028, .F. ) ;
#75321 = EDGE_CURVE ( 'NONE', #32589, #19658, #67140, .T. ) ;
#75322 = CARTESIAN_POINT ( 'NONE',  ( -1.627296587926508442, -0.5023911411419708095, -0.1820866141732282451 ) ) ;
#75323 = CARTESIAN_POINT ( 'NONE',  ( -1.167979002624671470, -0.4281496062992127816, -0.4176697321401328100 ) ) ;
#75324 = CARTESIAN_POINT ( 'NONE',  ( -0.8727034120734901146, -0.05778040916215560624, -0.4822834645669293319 ) ) ;
#75325 = CARTESIAN_POINT ( 'NONE',  ( 1.581364829396326277, -0.05778040916215522460, 0.4822834645669289988 ) ) ;
#75326 = CARTESIAN_POINT ( 'NONE',  ( 0.1958661417322836440, -0.3392501089628017219, -1.436351706036745446 ) ) ;
#75327 = CARTESIAN_POINT ( 'NONE',  ( -0.06766049032609942893, 0.3859888145977988794, -1.220472440944881498 ) ) ;
#75328 = CARTESIAN_POINT ( 'NONE',  ( 1.010498687664042716, -0.4281496062992124485, 0.4176697321401328655 ) ) ;
#75329 = CARTESIAN_POINT ( 'NONE',  ( 0.6167979002624679463, 0.05413385826771626580, -0.4176697321401330321 ) ) ;
#75330 = CARTESIAN_POINT ( 'NONE',  ( -0.2362204724409451284, 0.4091458600556402425, -0.4855643044619422644 ) ) ;
#75331 = CARTESIAN_POINT ( 'NONE',  ( -0.1998031496062991630, -0.3460692066303959202, -2.189632545931758489 ) ) ;
#75332 = CARTESIAN_POINT ( 'NONE',  ( 1.364829396325459854, -0.5023911411419708095, -0.1820866141732282451 ) ) ;
#75333 = CARTESIAN_POINT ( 'NONE',  ( -0.1070741851644051862, -0.3996062992125987146, -1.017060367454067915 ) ) ;
#75334 = ORIENTED_EDGE ( 'NONE', *, *, #66845, .T. ) ;
#75335 = CARTESIAN_POINT ( 'NONE',  ( -0.8005249343832011588, -0.004921259842519870586, -0.3153832671262229437 ) ) ;
#75336 = CARTESIAN_POINT ( 'NONE',  ( 0.1049643490035304938, -0.3917322834645669549, -2.754593175853017328 ) ) ;
#75337 = ORIENTED_EDGE ( 'NONE', *, *, #79988, .F. ) ;
#75338 = CARTESIAN_POINT ( 'NONE',  ( 0.5774278215223103139, -0.6046776061558809534, -0.2411417322834644161 ) ) ;
#75339 = CARTESIAN_POINT ( 'NONE',  ( -0.2165354330708654795, -0.5400638737290845981, -0.3530559997133363437 ) ) ;
#75340 = CARTESIAN_POINT ( 'NONE',  ( -1.292650918635170010, 0.2952755905511810774, -0.1292274648535930714 ) ) ;
#75341 = CARTESIAN_POINT ( 'NONE',  ( 1.017060367454068803, -0.3162353388693405765, 0.4822834645669290543 ) ) ;
#75342 = CARTESIAN_POINT ( 'NONE',  ( 1.528871391076116026, 0.2952755905511811885, 0.1292274648535926551 ) ) ;
#75343 = CYLINDRICAL_SURFACE ( 'NONE', #19797, 0.1574803149606299746 ) ;
#75344 = CARTESIAN_POINT ( 'NONE',  ( -0.1443569553805765515, -0.4281496062992127816, -0.4176697321401328100 ) ) ;
#75345 = CARTESIAN_POINT ( 'NONE',  ( -1.299212598425196097, 0.2952755905511811885, 0.000000000000000000 ) ) ;
#75346 = CARTESIAN_POINT ( 'NONE',  ( -1.640419947506561060, 0.05413385826771666132, 0.4176697321401328100 ) ) ;
#75347 = CARTESIAN_POINT ( 'NONE',  ( 0.4477342634306737956, 1.379855024864605539, -2.610352282803159785 ) ) ;
#75348 = CARTESIAN_POINT ( 'NONE',  ( 0.2867679344610365999, -0.2867679344610365444, -2.702755905511810663 ) ) ;
#75349 = CARTESIAN_POINT ( 'NONE',  ( 0.6955380577427828781, -0.3690944881889763329, 0.3153832671262228327 ) ) ;
#75350 = ORIENTED_EDGE ( 'NONE', *, *, #14488, .F. ) ;
#75351 = CARTESIAN_POINT ( 'NONE',  ( -9.674558042662121740E-17, 0.3949938075777409963, -0.1574803149606300023 ) ) ;
#75352 = CARTESIAN_POINT ( 'NONE',  ( -0.7545931758530176614, -0.6692913385826773087, -0.1292274648535924053 ) ) ;
#75353 = ORIENTED_EDGE ( 'NONE', *, *, #56823, .T. ) ;
#75354 = CARTESIAN_POINT ( 'NONE',  ( 0.1574803149606306130, -0.1870078740157479769, 0.3641732283464567677 ) ) ;
#75355 = CARTESIAN_POINT ( 'NONE',  ( -1.640419947506561060, -0.4281496062992127816, -0.4176697321401328100 ) ) ;
#75356 = CARTESIAN_POINT ( 'NONE',  ( 0.6758530183727039509, 0.2952755905511810774, -0.1292274648535930714 ) ) ;
#75357 = CARTESIAN_POINT ( 'NONE',  ( 0.4921259842519691285, 0.1660481256975885056, 0.3530559997133364547 ) ) ;
#75358 = CARTESIAN_POINT ( 'NONE',  ( -0.6889763779527552368, -0.5400638737290845981, -0.3530559997133363437 ) ) ;
#75359 = CARTESIAN_POINT ( 'NONE',  ( -0.1958661417322836995, 0.3392501089628017219, -1.269704355151917818 ) ) ;
#75360 = CARTESIAN_POINT ( 'NONE',  ( -0.9186351706036736120, -0.6046776061558809534, -0.2411417322834644161 ) ) ;
#75361 = CARTESIAN_POINT ( 'NONE',  ( -0.1049643490035302024, -0.3917322834645671215, -2.676509186351705871 ) ) ;
#75362 = CARTESIAN_POINT ( 'NONE',  ( 1.115485564304462551, -0.004921259842519576551, 0.3153832671262227771 ) ) ;
#75363 = CARTESIAN_POINT ( 'NONE',  ( -0.8202099737532799750, 0.2952755905511810774, -0.1292274648535930714 ) ) ;
#75364 = CARTESIAN_POINT ( 'NONE',  ( 0.7349081364829403995, 0.2306618581243848609, 0.2411417322834645549 ) ) ;
#75365 = CARTESIAN_POINT ( 'NONE',  ( 1.122047244094488860, -0.5400638737290845981, -0.3530559997133363437 ) ) ;
#75366 = VECTOR ( 'NONE', #42017, 39.37007874015748143 ) ;
#75367 = CARTESIAN_POINT ( 'NONE',  ( -0.3460692066303960868, 0.1998031496062990242, -0.6561679790026246906 ) ) ;
#75368 = CARTESIAN_POINT ( 'NONE',  ( -1.515748031496062076, 0.1660481256975883668, -0.3530559997133364547 ) ) ;
#75369 = CARTESIAN_POINT ( 'NONE',  ( -0.3996062992125984925, -0.1070741851644056858, -0.1227034120734908362 ) ) ;
#75370 = B_SPLINE_CURVE_WITH_KNOTS ( 'NONE', 3,
 ( #3314, #55461, #74860, #29800, #23074, #80760, #15543, #17202, #66890, #23488 ),
 .UNSPECIFIED., .F., .F.,
 ( 4, 2, 2, 2, 4 ),
 ( 0.01907194592498655597, 0.02029034601373087832, 0.02150874610247520413, 0.02272714619121952648, 0.02394554627996384882 ),
 .UNSPECIFIED. ) ;
#75371 = CARTESIAN_POINT ( 'NONE',  ( 0.3412073490813655186, 0.2306618581243848609, 0.2411417322834645549 ) ) ;
#75372 = CARTESIAN_POINT ( 'NONE',  ( -0.1998031496062991907, -0.3460692066303959757, -2.112860892388451539 ) ) ;
#75373 = CARTESIAN_POINT ( 'NONE',  ( -1.489501312335957062, -0.08942795157527998196, 0.3641732283464567121 ) ) ;
#75374 = CARTESIAN_POINT ( 'NONE',  ( 0.4330708661417329575, 0.1771653543307087630, 0.000000000000000000 ) ) ;
#75375 = CARTESIAN_POINT ( 'NONE',  ( 0.9448818897637802916, -0.1870078740157479769, 0.4822834645669291653 ) ) ;
#75376 = CARTESIAN_POINT ( 'NONE',  ( -0.4724409448818895907, -0.1265901696524993070, -1.067585301837270517 ) ) ;
#75377 = CARTESIAN_POINT ( 'NONE',  ( 0.6364829396325465405, -0.2845877964562161244, -0.3641732283464567121 ) ) ;
#75378 = ADVANCED_FACE ( 'NONE', ( #62466 ), #9469, .T. ) ;
#75379 = CARTESIAN_POINT ( 'NONE',  ( 0.4658792650918640033, -0.3162353388693405765, 0.4822834645669290543 ) ) ;
#75380 = CARTESIAN_POINT ( 'NONE',  ( -0.2891555358219909388, -0.2891555358219912164, -0.9232283464566930498 ) ) ;
#75381 = CARTESIAN_POINT ( 'NONE',  ( -0.9448818897637790704, -0.1870078740157479769, 0.4822834645669291653 ) ) ;
#75382 = CARTESIAN_POINT ( 'NONE',  ( -0.2362204724409447953, -0.4091458600556404646, -1.087270341207349000 ) ) ;
#75383 = CARTESIAN_POINT ( 'NONE',  ( 1.095800524934383846, -0.2845877964562159024, 0.3641732283464567677 ) ) ;
#75384 = EDGE_CURVE ( 'NONE', #32899, #52886, #48588, .T. ) ;
#75385 = CARTESIAN_POINT ( 'NONE',  ( -0.1443569553805768291, 0.05413385826771666132, 0.4176697321401328100 ) ) ;
#75386 = AXIS2_PLACEMENT_3D ( 'NONE', #16856, #42491, #66955 ) ;
#75387 = CARTESIAN_POINT ( 'NONE',  ( 0.4359958488159758616, 1.724409448818897905, -1.033875059083675163 ) ) ;
#75388 = CARTESIAN_POINT ( 'NONE',  ( -0.5183727034120726440, -0.6692913385826773087, -0.1292274648535924053 ) ) ;
#75389 = CARTESIAN_POINT ( 'NONE',  ( 8.195543980992789655E-16, -0.1870078740157480601, -0.3641732283464567677 ) ) ;
#75390 = CARTESIAN_POINT ( 'NONE',  ( -2.619510771202522292, 1.365902157108380477, -0.4425616331406683202 ) ) ;
#75391 = CARTESIAN_POINT ( 'NONE',  ( -0.4527559055118102749, 0.1660481256975885056, 0.3530559997133364547 ) ) ;
#75392 = CARTESIAN_POINT ( 'NONE',  ( -0.08530183727034056085, -0.2845877964562159024, 0.3641732283464567677 ) ) ;
#75393 = CARTESIAN_POINT ( 'NONE',  ( 0.5839895013123367340, -0.5511811023622048555, -0.09757992244046775898 ) ) ;
#75394 = DIRECTION ( 'NONE',  ( 0.000000000000000000, 0.000000000000000000, 1.000000000000000000 ) ) ;
#75395 = CARTESIAN_POINT ( 'NONE',  ( -0.3460692066303960313, 0.1998031496062989965, -1.677821522309711488 ) ) ;
#75396 = CARTESIAN_POINT ( 'NONE',  ( 0.3280839895013130669, -0.4281496062992127816, -0.4176697321401328100 ) ) ;
#75397 = CARTESIAN_POINT ( 'NONE',  ( 0.2867679344610365999, 0.2867679344610365999, -1.547244094488189115 ) ) ;
#75398 = CARTESIAN_POINT ( 'NONE',  ( 1.076115485564305141, 0.1283753931104746893, -0.1820866141732285504 ) ) ;
#75399 = DIRECTION ( 'NONE',  ( 0.000000000000000000, 1.000000000000000000, 0.000000000000000000 ) ) ;
#75400 = CARTESIAN_POINT ( 'NONE',  ( -0.4658792650918627265, -0.08942795157527998196, 0.3641732283464567121 ) ) ;
#75401 = CARTESIAN_POINT ( 'NONE',  ( -0.7677165354330699465, 0.07958543189024085140, 0.2665933059059887866 ) ) ;
#75402 = CARTESIAN_POINT ( 'NONE',  ( -0.4527559055118102749, -0.5400638737290845981, -0.3530559997133363437 ) ) ;
#75403 = CARTESIAN_POINT ( 'NONE',  ( 1.154855643044620184, -0.5023911411419708095, 0.1820866141732285504 ) ) ;
#75404 = CARTESIAN_POINT ( 'NONE',  ( -1.633858267716534529, -0.4536011799217368745, -0.2665933059059886201 ) ) ;
#75405 = CARTESIAN_POINT ( 'NONE',  ( 1.594488188976378673, 0.07958543189024085140, 0.2665933059059887866 ) ) ;
#75406 = CARTESIAN_POINT ( 'NONE',  ( 0.2493438320209980519, 0.05413385826771666132, 0.4176697321401328100 ) ) ;
#75407 = EDGE_CURVE ( 'NONE', #35363, #74087, #75704, .T. ) ;
#75408 = B_SPLINE_CURVE_WITH_KNOTS ( 'NONE', 3,
 ( #4628, #16878, #22348, #9720, #61056, #9309, #3406, #34979, #60643, #35391, #48008, #29069, #80445, #22755, #48416, #63120, #57615, #63531, #5862, #43323, #69023, #11374, #75347, #25216, #50470, #37446, #38682, #17695, #37031, #62713 ),
 .UNSPECIFIED., .F., .F.,
 ( 4, 2, 2, 2, 2, 2, 2, 2, 2, 2, 2, 2, 2, 2, 4 ),
 ( 0.02630788966047398897, 0.02761938857346088114, 0.02893088748644776984, 0.03024238639943466200, 0.03155388531242155070, 0.03417688313839533504, 0.03548838205138224455, 0.03679988096436914713, 0.03942287879034296616, 0.04073437770332988261, 0.04204587661631679907, 0.04335737552930371552, 0.04466887444229063198, 0.04598037335527754843, 0.04729187226826446488 ),
 .UNSPECIFIED. ) ;
#75409 = CARTESIAN_POINT ( 'NONE',  ( 0.9645669291338591078, -0.5400638737290845981, -0.3530559997133363437 ) ) ;
#75410 = CARTESIAN_POINT ( 'NONE',  ( 0.2087913723976025926, -0.2087913723976025926, 0.1248231986745540617 ) ) ;
#75411 = CARTESIAN_POINT ( 'NONE',  ( 0.1771653543307093182, 0.1660481256975885056, 0.3530559997133364547 ) ) ;
#75412 = CARTESIAN_POINT ( 'NONE',  ( 0.3392501089628018329, 0.1958661417322835607, -1.160761154855643129 ) ) ;
#75413 = CARTESIAN_POINT ( 'NONE',  ( 0.7086614173228353852, -0.1870078740157479769, 0.4822834645669291653 ) ) ;
#75414 = CARTESIAN_POINT ( 'NONE',  ( 0.5511811023622055217, -0.1870078740157479769, 0.4822834645669291653 ) ) ;
#75415 = CARTESIAN_POINT ( 'NONE',  ( 1.895394334970792016, 2.755905511811024056, -0.5314960629921260393 ) ) ;
#75416 = CARTESIAN_POINT ( 'NONE',  ( 0.7611548556430454138, 0.1283753931104746893, -0.1820866141732285504 ) ) ;
#75417 = CARTESIAN_POINT ( 'NONE',  ( 1.384514435695538559, 0.2952755905511810774, -0.1292274648535930714 ) ) ;
#75418 = ADVANCED_FACE ( 'NONE', ( #36382 ), #20605, .F. ) ;
#75419 = CARTESIAN_POINT ( 'NONE',  ( 0.1246719160104994284, -0.5511811023622046335, 0.09757992244046803654 ) ) ;
#75420 = CARTESIAN_POINT ( 'NONE',  ( -0.4461942257217840213, -0.6046776061558809534, -0.2411417322834644161 ) ) ;
#75421 = CARTESIAN_POINT ( 'NONE',  ( 0.4396325459317590445, -0.6692913385826771977, 0.1292274648535927661 ) ) ;
#75422 = CARTESIAN_POINT ( 'NONE',  ( -0.6955380577427815458, 0.05413385826771666132, 0.4176697321401328100 ) ) ;
#75423 = CARTESIAN_POINT ( 'NONE',  ( -0.3871391076115479057, -0.2845877964562161244, -0.3641732283464567121 ) ) ;
#75424 = VECTOR ( 'NONE', #64753, 39.37007874015748143 ) ;
#75425 = CARTESIAN_POINT ( 'NONE',  ( 0.9448818897637802916, -0.1870078740157479769, 0.4822834645669291653 ) ) ;
#75426 = CARTESIAN_POINT ( 'NONE',  ( 1.095800524934383846, -0.08942795157528024563, -0.3641732283464568787 ) ) ;
#75427 = CARTESIAN_POINT ( 'NONE',  ( 0.2230971128608932319, -0.4281496062992124485, 0.4176697321401328655 ) ) ;
#75428 = EDGE_CURVE ( 'NONE', #44792, #10316, #17905, .T. ) ;
#75429 = CARTESIAN_POINT ( 'NONE',  ( 0.2362204724409451007, -0.4091458600556402980, -0.5643044619422572516 ) ) ;
#75431 = CARTESIAN_POINT ( 'NONE',  ( 0.2925321140481932369, -0.2925321140481931814, -1.200787401574802793 ) ) ;
#75430 = CARTESIAN_POINT ( 'NONE',  ( -1.646051170424378096, -0.1870078740157480046, 1.254653134982923898E-17 ) ) ;
#75432 = CARTESIAN_POINT ( 'NONE',  ( -0.1474713956048439301, -2.191421614605370878E-15, 0.4445507791589071167 ) ) ;
#75433 = CARTESIAN_POINT ( 'NONE',  ( -0.1049643490035301885, -0.3917322834645671215, -2.111548556430446144 ) ) ;
#75434 = CARTESIAN_POINT ( 'NONE',  ( -1.115485564304461219, 0.05413385826771626580, -0.4176697321401330321 ) ) ;
#75435 = CARTESIAN_POINT ( 'NONE',  ( -0.7742782152230965886, 0.05413385826771666132, 0.4176697321401328100 ) ) ;
#75436 = B_SPLINE_CURVE_WITH_KNOTS ( 'NONE', 3,
 ( #23403, #48657, #61289, #73941 ),
 .UNSPECIFIED., .F., .F.,
 ( 4, 4 ),
 ( 3.210432057660995322E-07, 0.001287787053612127848 ),
 .UNSPECIFIED. ) ;
#75437 = CARTESIAN_POINT ( 'NONE',  ( 5.785732909357575061E-17, -0.4724409448818898682, -0.2362204724409449064 ) ) ;
#75438 = CARTESIAN_POINT ( 'NONE',  ( -0.1058382717557497937, -0.3949938075777411628, -2.749343832020997969 ) ) ;
#75439 = ORIENTED_EDGE ( 'NONE', *, *, #6477, .T. ) ;
#75440 = CARTESIAN_POINT ( 'NONE',  ( 0.4199475065616805614, 0.1283753931104748280, 0.1820866141732283561 ) ) ;
#75441 = CARTESIAN_POINT ( 'NONE',  ( 0.3392501089628018884, -0.1958661417322834220, -1.199475065616797842 ) ) ;
#75442 = CARTESIAN_POINT ( 'NONE',  ( 0.8858267716535438430, -0.5400638737290845981, -0.3530559997133363437 ) ) ;
#75443 = CARTESIAN_POINT ( 'NONE',  ( 0.2362204724409449064, 0.4091458600556404646, -2.664041994750656173 ) ) ;
#75444 = CARTESIAN_POINT ( 'NONE',  ( -0.9881811337016640495, 2.755905511811024056, 0.5314960629921260393 ) ) ;
#75446 = VECTOR ( 'NONE', #48450, 39.37007874015748143 ) ;
#75445 = CARTESIAN_POINT ( 'NONE',  ( -1.627296587926508442, -0.5023911411419708095, -0.1820866141732282451 ) ) ;
#75447 = CARTESIAN_POINT ( 'NONE',  ( 1.364829396325460076, 0.2306618581243848609, 0.2411417322834645549 ) ) ;
#75448 = CARTESIAN_POINT ( 'NONE',  ( 1.207349081364829990, -0.5023911411419708095, -0.1820866141732282451 ) ) ;
#75449 = CARTESIAN_POINT ( 'NONE',  ( -0.07217847769028787330, -0.05778040916215522460, 0.4822834645669289988 ) ) ;
#75450 = CARTESIAN_POINT ( 'NONE',  ( -0.3917322834645668994, -0.1049643490035306742, -0.7558861960291846094 ) ) ;
#75451 = CARTESIAN_POINT ( 'NONE',  ( -0.2165354330708654795, 0.1660481256975885056, 0.3530559997133364547 ) ) ;
#75452 = CARTESIAN_POINT ( 'NONE',  ( -0.7152230971128602510, -0.08942795157528024563, -0.3641732283464568787 ) ) ;
#75453 = CARTESIAN_POINT ( 'NONE',  ( 0.5052493438320215802, 0.2952755905511811885, 0.1292274648535926551 ) ) ;
#75454 = CARTESIAN_POINT ( 'NONE',  ( -0.5380577427821514602, -0.4281496062992127816, -0.4176697321401328100 ) ) ;
#75455 = CARTESIAN_POINT ( 'NONE',  ( -3.937007874015748143, 1.724409448818897905, -0.4359958488159722534 ) ) ;
#75456 = DIRECTION ( 'NONE',  ( 0.000000000000000000, 1.000000000000000000, 0.000000000000000000 ) ) ;
#75457 = ORIENTED_EDGE ( 'NONE', *, *, #69293, .T. ) ;
#75458 = CARTESIAN_POINT ( 'NONE',  ( 0.3392501089628018329, 0.1958661417322835607, -1.860255536254279862 ) ) ;
#75459 = CARTESIAN_POINT ( 'NONE',  ( 0.5971128608923891301, 0.2952755905511810774, -0.1292274648535930714 ) ) ;
#75460 = CARTESIAN_POINT ( 'NONE',  ( -0.4724409448818890911, -0.1870078740157479769, 0.4822834645669291653 ) ) ;
#75461 = CARTESIAN_POINT ( 'NONE',  ( -1.620734908136482577, 0.2952755905511811885, 0.1292274648535926551 ) ) ;
#75462 = CARTESIAN_POINT ( 'NONE',  ( 0.7020997375328090762, -0.05778040916215560624, -0.4822834645669293319 ) ) ;
#75463 = CARTESIAN_POINT ( 'NONE',  ( 0.3215223097112867578, -0.3162353388693409650, -0.4822834645669289433 ) ) ;
#75464 = CARTESIAN_POINT ( 'NONE',  ( 0.3917322834645670104, 2.398668435337828261E-17, -1.462598425196850460 ) ) ;
#75465 = CARTESIAN_POINT ( 'NONE',  ( -0.6299212598425188991, -0.1870078740157479769, 0.4822834645669291653 ) ) ;
#75466 = CARTESIAN_POINT ( 'NONE',  ( 0.3871391076115493490, -0.3162353388693405765, 0.4822834645669290543 ) ) ;
#75467 = CARTESIAN_POINT ( 'NONE',  ( -0.4330708661417315697, -0.6692913385826771977, 8.415575281601705876E-17 ) ) ;
#75468 = CARTESIAN_POINT ( 'NONE',  ( 0.3674540682414705883, -0.5023911411419708095, 0.1820866141732285504 ) ) ;
#75469 = CARTESIAN_POINT ( 'NONE',  ( -1.706036745406823485, 0.2306618581243848609, 0.2411417322834645549 ) ) ;
#75470 = CARTESIAN_POINT ( 'NONE',  ( -0.2952755905511810774, -0.01196537350834416848, 5.524802951929911110 ) ) ;
#75471 = CARTESIAN_POINT ( 'NONE',  ( -0.2427821522309703550, -0.05778040916215560624, -0.4822834645669293319 ) ) ;
#75472 = CYLINDRICAL_SURFACE ( 'NONE', #46643, 1.181102362204724310 ) ;
#75473 = CARTESIAN_POINT ( 'NONE',  ( 1.535433070866142335, -0.6692913385826771977, 8.415575281601705876E-17 ) ) ;
#75474 = CARTESIAN_POINT ( 'NONE',  ( -0.3917322834645670104, -7.196005306013484475E-17, -2.708661417322834275 ) ) ;
#75475 = ORIENTED_EDGE ( 'NONE', *, *, #3774, .T. ) ;
#75476 = EDGE_LOOP ( 'NONE', ( #36538, #6250, #12909, #33490, #35789, #24399, #74290, #79510, #13428, #15640, #55438, #5632, #56070, #58353, #38996, #52205, #18005, #15517, #38251, #72257, #12003, #44660, #53781, #73402, #4111, #50788, #80451, #46990, #65125, #16961, #68034, #79000, #53181, #10256, #7791, #15096 ) ) ;
#75477 = CARTESIAN_POINT ( 'NONE',  ( 0.5643044619422579178, 0.05413385826771666132, 0.4176697321401328100 ) ) ;
#75478 = CARTESIAN_POINT ( 'NONE',  ( 0.1443569553805781891, -0.3690944881889763329, 0.3153832671262228327 ) ) ;
#75480 = CARTESIAN_POINT ( 'NONE',  ( -1.036041590146031366, -2.613618158232546091E-15, -0.3464511005275220379 ) ) ;
#75479 = CARTESIAN_POINT ( 'NONE',  ( -2.543486866223389153, 2.716535433070866645, -0.5314960629921260393 ) ) ;
#75481 = CARTESIAN_POINT ( 'NONE',  ( -0.1958661417322836718, 0.3392501089628017219, -0.7276902887139108378 ) ) ;
#75482 = CARTESIAN_POINT ( 'NONE',  ( 0.4724409448818896462, 0.1265901696524990294, 0.1135170603674540563 ) ) ;
#75483 = DIRECTION ( 'NONE',  ( 0.000000000000000000, 0.000000000000000000, 1.000000000000000000 ) ) ;
#75484 = ADVANCED_FACE ( 'NONE', ( #38440 ), #77168, .T. ) ;
#75485 = CARTESIAN_POINT ( 'NONE',  ( -0.3996062992125984925, -0.1070741851644056858, -2.799868766404198794 ) ) ;
#75486 = CARTESIAN_POINT ( 'NONE',  ( 0.4593175853018379162, -0.4281496062992124485, 0.4176697321401328655 ) ) ;
#75487 = CARTESIAN_POINT ( 'NONE',  ( -1.410761154855641575, -0.3162353388693409650, -0.4822834645669289433 ) ) ;
#75488 = CARTESIAN_POINT ( 'NONE',  ( -1.194225721784776262, 0.05413385826771626580, -0.4176697321401330321 ) ) ;
#75489 = CARTESIAN_POINT ( 'NONE',  ( 0.7939632545931766261, -0.05778040916215522460, 0.4822834645669289988 ) ) ;
#75490 = AXIS2_PLACEMENT_3D ( 'NONE', #17005, #26183, #19884 ) ;
#75491 = CARTESIAN_POINT ( 'NONE',  ( 0.7480314960629927956, -0.6692913385826771977, 8.415575281601705876E-17 ) ) ;
#75492 = CARTESIAN_POINT ( 'NONE',  ( 1.292650918635171564, -0.5511811023622048555, -0.09757992244046775898 ) ) ;
#75493 = CARTESIAN_POINT ( 'NONE',  ( 1.043307086614173818, 0.07958543189024085140, 0.2665933059059887866 ) ) ;
#75494 = CARTESIAN_POINT ( 'NONE',  ( -0.7545931758530176614, -0.6692913385826773087, -0.1292274648535924053 ) ) ;
#75495 = CARTESIAN_POINT ( 'NONE',  ( 0.3996062992125986035, -0.1070741851644052972, -0.3458005249343831244 ) ) ;
#75496 = CARTESIAN_POINT ( 'NONE',  ( -1.607611548556429737, 0.1771653543307087075, -0.09757992244046823083 ) ) ;
#75497 = CARTESIAN_POINT ( 'NONE',  ( 0.1958661417322834775, 0.3392501089628018884, -0.1364829396325459021 ) ) ;
#75498 = CARTESIAN_POINT ( 'NONE',  ( -0.4396325459317577122, -0.6692913385826773087, -0.1292274648535924053 ) ) ;
#75500 = FACE_OUTER_BOUND ( 'NONE', #38254, .T. ) ;
#75499 = CARTESIAN_POINT ( 'NONE',  ( 1.227034120734908917, 0.2952755905511810774, -0.1292274648535930714 ) ) ;
#75501 = CARTESIAN_POINT ( 'NONE',  ( -1.417322834645668772, -0.1870078740157479769, 0.3641732283464567677 ) ) ;
#75502 = CARTESIAN_POINT ( 'NONE',  ( 0.4658792650918641698, -0.05778040916215560624, -0.4822834645669293319 ) ) ;
#75503 = CARTESIAN_POINT ( 'NONE',  ( 0.8464566929133865436, 0.07958543189024071263, -0.2665933059059888421 ) ) ;
#75504 = CARTESIAN_POINT ( 'NONE',  ( -0.1049643490035306742, 0.3917322834645668994, -1.661398007052806269 ) ) ;
#75505 = CARTESIAN_POINT ( 'NONE',  ( -1.213910761154854745, 0.1771653543307087075, -0.09757992244046823083 ) ) ;
#75506 = CARTESIAN_POINT ( 'NONE',  ( 0.9251968503937015864, 0.1660481256975883668, -0.3530559997133364547 ) ) ;
#75507 = CARTESIAN_POINT ( 'NONE',  ( -0.5183727034120726440, 0.2952755905511811885, 0.1292274648535926551 ) ) ;
#75508 = CARTESIAN_POINT ( 'NONE',  ( -0.4461942257217840213, 0.1283753931104748280, 0.1820866141732283561 ) ) ;
#75509 = CARTESIAN_POINT ( 'NONE',  ( -0.4527559055118102749, 0.1660481256975885056, 0.3530559997133364547 ) ) ;
#75510 = CARTESIAN_POINT ( 'NONE',  ( 1.496062992125985147, -0.1870078740157479769, 0.4822834645669291653 ) ) ;
#75511 = CARTESIAN_POINT ( 'NONE',  ( -0.6824146981627291497, -0.6046776061558809534, -0.2411417322834644161 ) ) ;
#75512 = CARTESIAN_POINT ( 'NONE',  ( 1.581364829396326277, -0.3162353388693409650, -0.4822834645669289433 ) ) ;
#75513 = CARTESIAN_POINT ( 'NONE',  ( 0.2867679344610366554, -0.2867679344610365999, -0.8825652475403695796 ) ) ;
#75514 = CARTESIAN_POINT ( 'NONE',  ( -0.8530183727034112984, -0.004921259842519576551, 0.3153832671262227771 ) ) ;
#75515 = CARTESIAN_POINT ( 'NONE',  ( 2.565964038698667515, 1.605872332714551876, 0.4695140184743388789 ) ) ;
#75516 = CARTESIAN_POINT ( 'NONE',  ( 1.253280839895013710, -0.3162353388693405765, 0.4822834645669290543 ) ) ;
#75517 = CARTESIAN_POINT ( 'NONE',  ( 0.4091458600556404646, -0.2362204724409448231, -2.071522309711285814 ) ) ;
#75518 = CARTESIAN_POINT ( 'NONE',  ( -1.318897637795274802, -0.5400638737290845981, -0.3530559997133363437 ) ) ;
#75519 = CARTESIAN_POINT ( 'NONE',  ( -1.515748031496062076, -0.4536011799217367080, 0.2665933059059888421 ) ) ;
#75520 = CARTESIAN_POINT ( 'NONE',  ( -0.4658792650918627265, -0.08942795157527998196, 0.3641732283464567121 ) ) ;
#75521 = CARTESIAN_POINT ( 'NONE',  ( 3.833048052449394218E-17, 2.145669291338582418, 0.3129921259842520787 ) ) ;
#75522 = CARTESIAN_POINT ( 'NONE',  ( -0.4921259842519677963, 0.1660481256975883668, -0.3530559997133364547 ) ) ;
#75523 = CARTESIAN_POINT ( 'NONE',  ( -0.006561679790025524116, -0.08942795157528024563, -0.3641732283464568787 ) ) ;
#75524 = CARTESIAN_POINT ( 'NONE',  ( -1.043307086614172707, 0.07958543189024071263, -0.2665933059059888421 ) ) ;
#75525 = CARTESIAN_POINT ( 'NONE',  ( 1.397637795275591177, -0.4536011799217367080, 0.2665933059059888421 ) ) ;
#75526 = CARTESIAN_POINT ( 'NONE',  ( 0.9251968503937015864, 0.1660481256975883668, -0.3530559997133364547 ) ) ;
#75527 = DIRECTION ( 'NONE',  ( 1.000000000000000000, -0.000000000000000000, -0.000000000000000000 ) ) ;
#75528 = CARTESIAN_POINT ( 'NONE',  ( 0.5839895013123367340, 0.1771653543307087630, 0.09757992244046791164 ) ) ;
#75529 = CARTESIAN_POINT ( 'NONE',  ( 0.2755905511811031494, 0.2952755905511811885, 0.000000000000000000 ) ) ;
#75530 = CARTESIAN_POINT ( 'NONE',  ( 0.8202099737532813073, 0.1771653543307087630, 0.09757992244046791164 ) ) ;
#75531 = ORIENTED_EDGE ( 'NONE', *, *, #15762, .F. ) ;
#75532 = CARTESIAN_POINT ( 'NONE',  ( -1.030183727034119867, -0.3162353388693405765, 0.4822834645669290543 ) ) ;
#75533 = CARTESIAN_POINT ( 'NONE',  ( -0.9776902887139098386, 0.2952755905511810774, -0.1292274648535930714 ) ) ;
#75534 = CARTESIAN_POINT ( 'NONE',  ( -0.2887139107611542133, 0.2306618581243848609, 0.2411417322834645549 ) ) ;
#75535 = CARTESIAN_POINT ( 'NONE',  ( 0.2925321140481932369, -0.2925321140481931814, -0.09842519685039372024 ) ) ;
#75536 = CARTESIAN_POINT ( 'NONE',  ( 0.1070741851644053388, 0.3996062992125986035, -2.432414698162729039 ) ) ;
#75537 = CARTESIAN_POINT ( 'NONE',  ( 0.5380577427821529035, 0.05413385826771626580, -0.4176697321401330321 ) ) ;
#75538 = CARTESIAN_POINT ( 'NONE',  ( 1.509186351706037543, -0.3690944881889765550, -0.3153832671262227771 ) ) ;
#75539 = CARTESIAN_POINT ( 'NONE',  ( -0.1312335958005241554, -0.6046776061558809534, -0.2411417322834644161 ) ) ;
#75540 = CARTESIAN_POINT ( 'NONE',  ( 0.9776902887139113929, 0.2952755905511811885, 0.1292274648535926551 ) ) ;
#75541 = CARTESIAN_POINT ( 'NONE',  ( 0.3460692066303959757, -0.1998031496062991907, -2.309711286089239035 ) ) ;
#75542 = CARTESIAN_POINT ( 'NONE',  ( -0.3949938075777411628, 0.1058382717557497937, -1.607611548556430847 ) ) ;
#75543 = CARTESIAN_POINT ( 'NONE',  ( 0.000000000000000000, 1.929133858267716661, 1.850393700787401619 ) ) ;
#75544 = CARTESIAN_POINT ( 'NONE',  ( -1.813482582612293559, 2.755905511811024056, -0.5314960629921260393 ) ) ;
#75545 = CARTESIAN_POINT ( 'NONE',  ( 0.2867679344610366554, 0.2867679344610366554, -0.6023622047244093780 ) ) ;
#75546 = CARTESIAN_POINT ( 'NONE',  ( -0.7217847769028863381, -0.004921259842519870586, -0.3153832671262229437 ) ) ;
#75547 = CARTESIAN_POINT ( 'NONE',  ( -0.7020997375328076329, -0.3162353388693409650, -0.4822834645669289433 ) ) ;
#75548 = CARTESIAN_POINT ( 'NONE',  ( 0.3215223097112867578, -0.05778040916215522460, 0.4822834645669289988 ) ) ;
#75549 = AXIS2_PLACEMENT_3D ( 'NONE', #49703, #75399, #37491 ) ;
#75550 = CARTESIAN_POINT ( 'NONE',  ( 0.1974969037888706092, -0.3420746716998660508, -2.688320209973753094 ) ) ;
#75551 = CARTESIAN_POINT ( 'NONE',  ( 1.003937007874016407, -0.5400638737290844871, 0.3530559997133364547 ) ) ;
#75552 = CARTESIAN_POINT ( 'NONE',  ( 1.574803149606299746, -0.1870078740157479769, 0.4822834645669291653 ) ) ;
#75553 = CARTESIAN_POINT ( 'NONE',  ( 0.8398950131233602345, 0.2306618581243847221, -0.2411417322834647770 ) ) ;
#75554 = CARTESIAN_POINT ( 'NONE',  ( 0.3458507752293908943, -0.3458507752293908943, -2.933070866141732402 ) ) ;
#75555 = CARTESIAN_POINT ( 'NONE',  ( -0.3460692066303960868, 0.1998031496062990242, -2.230971128608923770 ) ) ;
#75556 = CARTESIAN_POINT ( 'NONE',  ( 1.489501312335958172, -0.3162353388693405765, 0.4822834645669290543 ) ) ;
#75557 = CARTESIAN_POINT ( 'NONE',  ( 0.7480314960629927956, -0.6692913385826771977, 8.415575281601705876E-17 ) ) ;
#75558 = CARTESIAN_POINT ( 'NONE',  ( 0.7217847769028878924, -0.4281496062992127816, -0.4176697321401328100 ) ) ;
#75559 = CARTESIAN_POINT ( 'NONE',  ( 1.371391076115485719, -0.5511811023622048555, -0.09757992244046775898 ) ) ;
#75561 = CARTESIAN_POINT ( 'NONE',  ( 1.561679790026247350, -0.4281496062992124485, 0.4176697321401328655 ) ) ;
#75560 = CARTESIAN_POINT ( 'NONE',  ( -1.476377952755905110, 0.07958543189024085140, 0.2665933059059887866 ) ) ;
#75562 = CARTESIAN_POINT ( 'NONE',  ( -0.3392501089628017219, -0.1958661417322836718, -0.1371391076115486551 ) ) ;
#75563 = CARTESIAN_POINT ( 'NONE',  ( 2.170146923806634653, 1.537401574803149984, -0.4744094488188970171 ) ) ;
#75564 = CARTESIAN_POINT ( 'NONE',  ( 0.9973753280839902091, -0.6046776061558807314, 0.2411417322834647770 ) ) ;
#75565 = CARTESIAN_POINT ( 'NONE',  ( 1.391076115485564868, 0.1283753931104746893, -0.1820866141732285504 ) ) ;
#75566 = CARTESIAN_POINT ( 'NONE',  ( -0.4855643044619415427, -0.4281496062992124485, 0.4176697321401328655 ) ) ;
#75567 = CARTESIAN_POINT ( 'NONE',  ( -0.7939632545931754048, -0.3162353388693405765, 0.4822834645669290543 ) ) ;
#75568 = CARTESIAN_POINT ( 'NONE',  ( 1.587926509186352142, 0.05413385826771666132, 0.4176697321401328100 ) ) ;
#75569 = CARTESIAN_POINT ( 'NONE',  ( 0.1049643490035303689, 0.3917322834645670104, -0.3930446194225722945 ) ) ;
#75570 = B_SPLINE_CURVE_WITH_KNOTS ( 'NONE', 3,
 ( #73541, #60061, #28072, #16293 ),
 .UNSPECIFIED., .F., .F.,
 ( 4, 4 ),
 ( 0.07239528109754654606, 0.07258229963060973400 ),
 .UNSPECIFIED. ) ;
#75571 = CARTESIAN_POINT ( 'NONE',  ( 0.2867679344610365999, -0.2867679344610365444, -1.507874015748031260 ) ) ;
#75572 = CARTESIAN_POINT ( 'NONE',  ( -0.1958661417322834220, -0.3392501089628018884, -2.577427821522309426 ) ) ;
#75573 = CARTESIAN_POINT ( 'NONE',  ( 1.673228346456693494, 0.1660481256975885056, 0.3530559997133364547 ) ) ;
#75574 = ORIENTED_EDGE ( 'NONE', *, *, #48087, .F. ) ;
#75575 = CARTESIAN_POINT ( 'NONE',  ( 0.2891555358219910499, -0.2891555358219909944, -2.618110236220472675 ) ) ;
#75576 = ORIENTED_EDGE ( 'NONE', *, *, #6890, .F. ) ;
#75577 = CARTESIAN_POINT ( 'NONE',  ( -1.604771003085130099, 1.595806277125122241, -0.1466069496707745334 ) ) ;
#75578 = CARTESIAN_POINT ( 'NONE',  ( 1.299212598425197429, 0.1771653543307087630, 0.000000000000000000 ) ) ;
#75579 = CARTESIAN_POINT ( 'NONE',  ( -0.3996062992125986035, -0.1070741851644056997, -1.305774278215223072 ) ) ;
#75580 = DIRECTION ( 'NONE',  ( -0.000000000000000000, -1.000000000000000000, -0.000000000000000000 ) ) ;
#75581 = DIRECTION ( 'NONE',  ( 0.000000000000000000, 0.000000000000000000, 1.000000000000000000 ) ) ;
#75582 = CARTESIAN_POINT ( 'NONE',  ( 0.4177787735907000366, 0.3937007874015747699, -1.559171609364239375 ) ) ;
#75583 = CARTESIAN_POINT ( 'NONE',  ( -0.3129921259842521342, 1.527825669364019756, 5.602422643256820041E-18 ) ) ;
#75584 = CARTESIAN_POINT ( 'NONE',  ( -0.1049643490035302024, -0.3917322834645671215, -0.3143044619422573072 ) ) ;
#75585 = EDGE_CURVE ( 'NONE', #82661, #36021, #43501, .T. ) ;
#75586 = CARTESIAN_POINT ( 'NONE',  ( -0.8333333333333323711, 0.1771653543307087630, 0.09757992244046791164 ) ) ;
#75587 = CARTESIAN_POINT ( 'NONE',  ( -1.056430446194224881, 0.1771653543307087075, -0.09757992244046823083 ) ) ;
#75588 = CARTESIAN_POINT ( 'NONE',  ( -1.207349081364828436, -0.6046776061558807314, 0.2411417322834647770 ) ) ;
#75589 = CARTESIAN_POINT ( 'NONE',  ( -0.01312335958005186876, -0.4281496062992124485, 0.4176697321401328655 ) ) ;
#75590 = CARTESIAN_POINT ( 'NONE',  ( -1.338582677165353729, -0.1870078740157479769, 0.4822834645669291653 ) ) ;
#75591 = ORIENTED_EDGE ( 'NONE', *, *, #65602, .F. ) ;
#75592 = CARTESIAN_POINT ( 'NONE',  ( 1.522309711286089939, -0.6046776061558809534, -0.2411417322834644161 ) ) ;
#75593 = CARTESIAN_POINT ( 'NONE',  ( -1.611562765098779382, 0.2819705615091875339, 0.1148851572488242823 ) ) ;
#75594 = CARTESIAN_POINT ( 'NONE',  ( 0.2362204724409451007, -0.4091458600556402980, -1.824146981627296604 ) ) ;
#75595 = DIRECTION ( 'NONE',  ( 1.000000000000000000, -0.000000000000000000, -0.000000000000000000 ) ) ;
#75596 = CARTESIAN_POINT ( 'NONE',  ( -0.3477690288713902178, 0.1771653543307087075, -0.09757992244046823083 ) ) ;
#75597 = CARTESIAN_POINT ( 'NONE',  ( -1.023622047244093558, -0.1870078740157479769, 0.4822834645669291653 ) ) ;
#75598 = CARTESIAN_POINT ( 'NONE',  ( 0.9514435695538062676, -0.3162353388693409650, -0.4822834645669289433 ) ) ;
#75599 = ORIENTED_EDGE ( 'NONE', *, *, #36496, .T. ) ;
#75601 = PLANE ( 'NONE',  #82822 ) ;
#75600 = CARTESIAN_POINT ( 'NONE',  ( 0.7480314960629927956, 0.2952755905511811885, 0.000000000000000000 ) ) ;
#75602 = CARTESIAN_POINT ( 'NONE',  ( 1.692913385826772421, 0.2952755905511811885, 0.000000000000000000 ) ) ;
#75603 = CARTESIAN_POINT ( 'NONE',  ( -1.384514435695537005, 0.2952755905511811885, 0.1292274648535926551 ) ) ;
#75604 = CARTESIAN_POINT ( 'NONE',  ( -0.2867679344610366554, 0.2867679344610365444, -0.4146788469478197015 ) ) ;
#75605 = CARTESIAN_POINT ( 'NONE',  ( 0.1509186351706042484, -0.2845877964562159024, 0.3641732283464567677 ) ) ;
#75606 = CARTESIAN_POINT ( 'NONE',  ( 0.1958661417322836440, -0.3392501089628017219, -0.8064304461942258806 ) ) ;
#75607 = CARTESIAN_POINT ( 'NONE',  ( -0.2099737532808391705, 0.1283753931104748280, 0.1820866141732283561 ) ) ;
#75608 = CARTESIAN_POINT ( 'NONE',  ( 0.3740157480314966754, 0.07958543189024071263, -0.2665933059059888421 ) ) ;
#75609 = CARTESIAN_POINT ( 'NONE',  ( 0.7349081364829402885, -0.6046776061558809534, -0.2411417322834644161 ) ) ;
#75610 = AXIS2_PLACEMENT_3D ( 'NONE', #32968, #21588, #26658 ) ;
#75611 = CARTESIAN_POINT ( 'NONE',  ( -0.7283464566929126471, -0.4536011799217367080, 0.2665933059059888421 ) ) ;
#75612 = CARTESIAN_POINT ( 'NONE',  ( 4.797336870675656522E-17, -0.3917322834645670104, -2.748031496062991685 ) ) ;
#75613 = CARTESIAN_POINT ( 'NONE',  ( 1.076115485564305141, -0.6046776061558807314, 0.2411417322834647770 ) ) ;
#75614 = CARTESIAN_POINT ( 'NONE',  ( -0.9317585301837263412, -0.4281496062992127816, -0.4176697321401328100 ) ) ;
#75615 = CARTESIAN_POINT ( 'NONE',  ( 0.3458507752293908943, 0.3458507752293908943, -0.8444881889763780070 ) ) ;
#75616 = CARTESIAN_POINT ( 'NONE',  ( -0.01312335958005186876, -0.4281496062992124485, 0.4176697321401328655 ) ) ;
#75617 = CARTESIAN_POINT ( 'NONE',  ( -0.4002624671916004129, -0.3162353388693405765, 0.4822834645669290543 ) ) ;
#75618 = CARTESIAN_POINT ( 'NONE',  ( 1.345144356955381593, -0.08942795157527998196, 0.3641732283464567121 ) ) ;
#75619 = CARTESIAN_POINT ( 'NONE',  ( 0.1640419947506569498, -0.08942795157527998196, 0.3641732283464567121 ) ) ;
#75620 = CARTESIAN_POINT ( 'NONE',  ( -0.07874015748031421014, -0.1870078740157480879, -0.4822834645669291653 ) ) ;
#75621 = CARTESIAN_POINT ( 'NONE',  ( -0.9580052493438311334, 0.05413385826771626580, -0.4176697321401330321 ) ) ;
#75622 = FACE_OUTER_BOUND ( 'NONE', #65943, .T. ) ;
#75623 = CARTESIAN_POINT ( 'NONE',  ( 1.587926509186352586, -0.3690944881889765550, -0.3153832671262227771 ) ) ;
#75624 = APPLICATION_CONTEXT ( 'automotive_design' ) ;
#75625 = CARTESIAN_POINT ( 'NONE',  ( -0.2690288713910754526, -0.6692913385826771977, 0.1292274648535927661 ) ) ;
#75626 = ORIENTED_EDGE ( 'NONE', *, *, #34718, .F. ) ;
#75627 = CARTESIAN_POINT ( 'NONE',  ( -0.2925321140481932369, 0.2925321140481931259, -1.986220472440944906 ) ) ;
#75628 = CARTESIAN_POINT ( 'NONE',  ( 1.095800524934383846, -0.3162353388693405765, 0.4822834645669290543 ) ) ;
#75629 = CARTESIAN_POINT ( 'NONE',  ( -0.6561679790026240244, -0.5023911411419708095, 0.1820866141732285504 ) ) ;
#75630 = CARTESIAN_POINT ( 'NONE',  ( -0.4068241469816267775, 0.05413385826771626580, -0.4176697321401330321 ) ) ;
#75631 = CARTESIAN_POINT ( 'NONE',  ( 1.397637795275591177, 0.1660481256975883668, -0.3530559997133364547 ) ) ;
#75632 = CARTESIAN_POINT ( 'NONE',  ( 1.003937007874016407, -0.5400638737290844871, 0.3530559997133364547 ) ) ;
#75633 = CARTESIAN_POINT ( 'NONE',  ( -0.3307086614173228023, 0.3647102339900947787, 0.000000000000000000 ) ) ;
#75634 = CARTESIAN_POINT ( 'NONE',  ( -1.253280839895012377, -0.08942795157527998196, 0.3641732283464567121 ) ) ;
#75635 = CARTESIAN_POINT ( 'NONE',  ( 0.1070741851644053527, 0.3996062992125985480, -0.8576115485564304031 ) ) ;
#75636 = CARTESIAN_POINT ( 'NONE',  ( 0.1998031496062994405, -0.3460692066303958092, -1.036745406824147064 ) ) ;
#75637 = CARTESIAN_POINT ( 'NONE',  ( -0.3949938075777409963, -7.255918531996591613E-17, -0.03937007874015754222 ) ) ;
#75638 = CARTESIAN_POINT ( 'NONE',  ( 0.2423360639762433821, 1.129538687396121954, -1.530894784087906357 ) ) ;
#75639 = CARTESIAN_POINT ( 'NONE',  ( 1.240157480314961314, 0.07958543189024071263, -0.2665933059059888421 ) ) ;
#75640 = CARTESIAN_POINT ( 'NONE',  ( 0.8267716535433077274, 0.1771653543307087630, 0.000000000000000000 ) ) ;
#75641 = CARTESIAN_POINT ( 'NONE',  ( 0.6627296587926515548, 0.2952755905511811885, 0.1292274648535926551 ) ) ;
#75642 = LINE ( 'NONE', #49533, #78935 ) ;
#75643 = CARTESIAN_POINT ( 'NONE',  ( -0.1974969037888704149, -0.3420746716998661063, -1.402230971128609172 ) ) ;
#75644 = CARTESIAN_POINT ( 'NONE',  ( 0.7939632545931766261, -0.2845877964562161244, -0.3641732283464567121 ) ) ;
#75645 = CARTESIAN_POINT ( 'NONE',  ( -0.2296587926509179312, -0.05778040916215522460, 0.4822834645669289988 ) ) ;
#75646 = CARTESIAN_POINT ( 'NONE',  ( -0.8989501312335946848, -0.6692913385826771977, 0.1292274648535927661 ) ) ;
#75647 = CARTESIAN_POINT ( 'NONE',  ( 1.305774278215223960, -0.6692913385826771977, 0.1292274648535927661 ) ) ;
#75648 = CARTESIAN_POINT ( 'NONE',  ( -0.2362204724409447953, -0.4091458600556404646, -1.167979002624671914 ) ) ;
#75649 = CARTESIAN_POINT ( 'NONE',  ( -0.3996062992125986590, 0.1070741851644051862, -2.709973753280840114 ) ) ;
#75650 = CARTESIAN_POINT ( 'NONE',  ( -0.1706036745406816491, -0.3690944881889763329, 0.3153832671262228327 ) ) ;
#75651 = ORIENTED_EDGE ( 'NONE', *, *, #9813, .F. ) ;
#75652 = CARTESIAN_POINT ( 'NONE',  ( -9.594673741351313045E-17, 0.3917322834645670659, -0.9416203656506056952 ) ) ;
#75653 = ORIENTED_EDGE ( 'NONE', *, *, #82446, .T. ) ;
#75654 = CARTESIAN_POINT ( 'NONE',  ( -0.8595800524934373854, -0.3162353388693409650, -0.4822834645669289433 ) ) ;
#75655 = CARTESIAN_POINT ( 'NONE',  ( -0.1771653543307080136, 0.1660481256975883668, -0.3530559997133364547 ) ) ;
#75656 = CARTESIAN_POINT ( 'NONE',  ( -0.2952755905511803003, -0.5400638737290845981, -0.3530559997133363437 ) ) ;
#75657 = CARTESIAN_POINT ( 'NONE',  ( 0.2952755905511819101, 0.1660481256975883668, -0.3530559997133364547 ) ) ;
#75658 = CARTESIAN_POINT ( 'NONE',  ( -0.4790026246719152336, -0.05778040916215560624, -0.4822834645669293319 ) ) ;
#75659 = CARTESIAN_POINT ( 'NONE',  ( -1.482939632545930975, 0.05413385826771666132, 0.4176697321401328100 ) ) ;
#75660 = CARTESIAN_POINT ( 'NONE',  ( -0.7152230971128602510, -0.05778040916215560624, -0.4822834645669293319 ) ) ;
#75661 = CARTESIAN_POINT ( 'NONE',  ( 0.5774278215223103139, -0.6046776061558809534, -0.2411417322834644161 ) ) ;
#75662 = ADVANCED_FACE ( 'NONE', ( #18274 ), #31712, .F. ) ;
#75663 = CARTESIAN_POINT ( 'NONE',  ( -0.1049643490035302024, -0.3917322834645671215, -1.009186351706036433 ) ) ;
#75664 = CARTESIAN_POINT ( 'NONE',  ( -0.3018372703412066094, -0.3690944881889765550, -0.3153832671262227771 ) ) ;
#75665 = VERTEX_POINT ( 'NONE', #82656 ) ;
#75666 = CARTESIAN_POINT ( 'NONE',  ( -0.3949938075777409408, -0.1058382717557502933, -1.620734908136483243 ) ) ;
#75667 = ORIENTED_EDGE ( 'NONE', *, *, #18320, .T. ) ;
#75668 = CARTESIAN_POINT ( 'NONE',  ( -1.115485564304461219, -0.3690944881889763329, 0.3153832671262228327 ) ) ;
#75669 = CARTESIAN_POINT ( 'NONE',  ( -1.108923884514435132, -0.05778040916215560624, -0.4822834645669293319 ) ) ;
#75670 = CARTESIAN_POINT ( 'NONE',  ( -0.8661417322834640276, -0.1870078740157479769, 0.4822834645669291653 ) ) ;
#75671 = CARTESIAN_POINT ( 'NONE',  ( -0.3460692066303960868, 0.1998031496062990242, -0.02624671916010499692 ) ) ;
#75672 = CARTESIAN_POINT ( 'NONE',  ( -0.6758530183727028406, -0.6692913385826773087, -0.1292274648535924053 ) ) ;
#75673 = CARTESIAN_POINT ( 'NONE',  ( -0.8661417322834640276, -0.1870078740157480879, -0.4822834645669291653 ) ) ;
#75674 = CARTESIAN_POINT ( 'NONE',  ( 0.3996062992125986035, 2.446882876249141962E-17, -1.220472440944881942 ) ) ;
#75675 = CARTESIAN_POINT ( 'NONE',  ( -0.2755905511811031494, 0.000000000000000000, 6.062992125984251857 ) ) ;
#75676 = CARTESIAN_POINT ( 'NONE',  ( 0.4921259842519691285, -0.4536011799217368745, -0.2665933059059886201 ) ) ;
#75677 = LINE ( 'NONE', #4966, #44434 ) ;
#75678 = CARTESIAN_POINT ( 'NONE',  ( -0.2867679344610364334, -0.2867679344610367109, -0.1437007874015748810 ) ) ;
#75679 = CARTESIAN_POINT ( 'NONE',  ( -0.09842519685039295696, 0.07958543189024071263, -0.2665933059059888421 ) ) ;
#75680 = CARTESIAN_POINT ( 'NONE',  ( -0.1640419947506553400, -0.05778040916215560624, -0.4822834645669293319 ) ) ;
#75681 = CARTESIAN_POINT ( 'NONE',  ( 1.604771003085129433, 1.044625174762918496, 0.1466069496707750885 ) ) ;
#75682 = CARTESIAN_POINT ( 'NONE',  ( -0.03280839895013062252, 0.2952755905511810774, -0.1292274648535930714 ) ) ;
#75683 = ORIENTED_EDGE ( 'NONE', *, *, #58402, .F. ) ;
#75684 = CARTESIAN_POINT ( 'NONE',  ( -0.3460692066303960868, 0.1998031496062990242, -2.230971128608923770 ) ) ;
#75685 = CARTESIAN_POINT ( 'NONE',  ( 0.2477166185931112263, 2.056812631849083806E-16, 0.3791483426435167670 ) ) ;
#75686 = ORIENTED_EDGE ( 'NONE', *, *, #41641, .F. ) ;
#75687 = CARTESIAN_POINT ( 'NONE',  ( 0.3460692066303958092, 0.1998031496062993018, -1.782808398950131101 ) ) ;
#75688 = CARTESIAN_POINT ( 'NONE',  ( -0.03143970413924313673, 0.3977953519386766557, -2.755905511811078679 ) ) ;
#75689 = CARTESIAN_POINT ( 'NONE',  ( -1.299212598425196097, -0.5511811023622047445, 6.969142054262312111E-17 ) ) ;
#75690 = CARTESIAN_POINT ( 'NONE',  ( -1.535433070866141225, 0.2952755905511811885, 0.000000000000000000 ) ) ;
#75691 = CARTESIAN_POINT ( 'NONE',  ( -0.4091458600556405756, 0.2362204724409446288, -0.3412073490813647969 ) ) ;
#75692 = CARTESIAN_POINT ( 'NONE',  ( 0.5314960629920921775, 2.716535433070866645, 3.224202737261820939 ) ) ;
#75693 = CARTESIAN_POINT ( 'NONE',  ( 0.1958661417322836440, -0.3392501089628017219, -2.853674540682414662 ) ) ;
#75694 = CARTESIAN_POINT ( 'NONE',  ( 1.286089238845145033, -0.6046776061558809534, -0.2411417322834644161 ) ) ;
#75695 = CARTESIAN_POINT ( 'NONE',  ( 0.4724409448818904789, -0.1870078740157479769, 0.4822834645669291653 ) ) ;
#75696 = CARTESIAN_POINT ( 'NONE',  ( -0.1049868766404193215, -0.6046776061558807314, 0.2411417322834647770 ) ) ;
#75697 = CARTESIAN_POINT ( 'NONE',  ( -1.030183727034119867, -0.2845877964562159024, 0.3641732283464567677 ) ) ;
#75698 = CARTESIAN_POINT ( 'NONE',  ( -0.5643044619422565855, 0.05413385826771626580, -0.4176697321401330321 ) ) ;
#75699 = CARTESIAN_POINT ( 'NONE',  ( 0.4091458600556403535, 0.2362204724409449896, -2.255249343832020692 ) ) ;
#75700 = CARTESIAN_POINT ( 'NONE',  ( -0.9317585301837263412, 0.05413385826771666132, 0.4176697321401328100 ) ) ;
#75701 = CARTESIAN_POINT ( 'NONE',  ( -0.1058382717557503072, 0.3949938075777408852, -2.288057742782152459 ) ) ;
#75702 = CARTESIAN_POINT ( 'NONE',  ( 1.253280839895013710, -0.2845877964562159024, 0.3641732283464567677 ) ) ;
#75703 = CARTESIAN_POINT ( 'NONE',  ( -0.5314960629921254842, -0.4536011799217368745, -0.2665933059059886201 ) ) ;
#75704 = CIRCLE ( 'NONE', #8471, 2.401574803149606474 ) ;
#75705 = CARTESIAN_POINT ( 'NONE',  ( 1.181102362204725198, -0.1870078740157479769, 0.3641732283464567677 ) ) ;
#75706 = CARTESIAN_POINT ( 'NONE',  ( -1.548556430446193399, 0.2306618581243848609, 0.2411417322834645549 ) ) ;
#75707 = CARTESIAN_POINT ( 'NONE',  ( -0.9776902887139098386, 0.1771653543307087075, -0.09757992244046823083 ) ) ;
#75708 = CARTESIAN_POINT ( 'NONE',  ( 0.4724409448818898682, 2.892866454678787531E-17, -2.242125984251968518 ) ) ;
#75709 = CARTESIAN_POINT ( 'NONE',  ( 0.5118110236220480003, -0.5511811023622047445, 6.969142054262312111E-17 ) ) ;
#75710 = CARTESIAN_POINT ( 'NONE',  ( -0.5052493438320203589, 0.2952755905511810774, -0.1292274648535930714 ) ) ;
#75711 = CARTESIAN_POINT ( 'NONE',  ( 0.3033747635708586854, 0.02791078216816508459, -0.4328096321851889194 ) ) ;
#75712 = CARTESIAN_POINT ( 'NONE',  ( 0.07217847769028949700, -0.2845877964562159024, 0.3641732283464567677 ) ) ;
#75713 = CARTESIAN_POINT ( 'NONE',  ( -1.157146581871515012E-16, 0.4724409448818898682, -1.021653543307086576 ) ) ;
#75714 = CARTESIAN_POINT ( 'NONE',  ( 0.8661417322834653598, -0.1870078740157479769, 0.4822834645669291653 ) ) ;
#75715 = CARTESIAN_POINT ( 'NONE',  ( 0.2114133405073579941, 0.2061694042878472466, 0.1284558427095351951 ) ) ;
#75716 = AXIS2_PLACEMENT_3D ( 'NONE', #1095, #26746, #27582 ) ;
#75717 = CARTESIAN_POINT ( 'NONE',  ( 1.371391076115485719, -0.5511811023622048555, -0.09757992244046775898 ) ) ;
#75718 = CARTESIAN_POINT ( 'NONE',  ( -0.8005249343832013809, -0.4281496062992124485, 0.4176697321401328655 ) ) ;
#75719 = CARTESIAN_POINT ( 'NONE',  ( -0.3149606299212590610, -0.1870078740157480601, -0.3641732283464567677 ) ) ;
#75720 = CARTESIAN_POINT ( 'NONE',  ( 0.1181102362204724532, -0.04921259842519688094, 0.08523872084492505052 ) ) ;
#75721 = CARTESIAN_POINT ( 'NONE',  ( 0.2034120734908142214, 0.1771653543307087075, -0.09757992244046823083 ) ) ;
#75722 = CARTESIAN_POINT ( 'NONE',  ( -1.207349081364828880, 0.2306618581243847221, -0.2411417322834647770 ) ) ;
#75723 = CARTESIAN_POINT ( 'NONE',  ( -0.5314960629921250401, 0.1660481256975885056, 0.3530559997133364547 ) ) ;
#75724 = CARTESIAN_POINT ( 'NONE',  ( -0.3460692066303957537, -0.1998031496062994405, -0.7591863517060367661 ) ) ;
#75725 = CARTESIAN_POINT ( 'NONE',  ( 0.1958661417322834775, 0.3392501089628018884, -2.433727034120734878 ) ) ;
#75726 = CARTESIAN_POINT ( 'NONE',  ( 0.5839895013123367340, -0.5511811023622048555, -0.09757992244046775898 ) ) ;
#75727 = CARTESIAN_POINT ( 'NONE',  ( -0.3083989501312330295, -0.3162353388693409650, -0.4822834645669289433 ) ) ;
#75728 = CARTESIAN_POINT ( 'NONE',  ( -0.5577427821522301654, -0.3162353388693405765, 0.4822834645669290543 ) ) ;
#75729 = CARTESIAN_POINT ( 'NONE',  ( -0.9711286089238838626, 0.1283753931104746893, -0.1820866141732285504 ) ) ;
#75730 = CARTESIAN_POINT ( 'NONE',  ( 0.4177787735907000366, 0.3937007874015747699, -1.361336963694947944 ) ) ;
#75731 = CARTESIAN_POINT ( 'NONE',  ( -0.1706036745406816491, 0.05413385826771626580, -0.4176697321401330321 ) ) ;
#75732 = CARTESIAN_POINT ( 'NONE',  ( -1.246719160104986512, -0.004921259842519576551, 0.3153832671262227771 ) ) ;
#75733 = CARTESIAN_POINT ( 'NONE',  ( -1.371391076115484609, -0.6692913385826771977, 0.1292274648535927661 ) ) ;
#75734 = CARTESIAN_POINT ( 'NONE',  ( -1.157146581871515012E-16, 0.4724409448818898682, -2.204724409448818978 ) ) ;
#75735 = ORIENTED_EDGE ( 'NONE', *, *, #69293, .F. ) ;
#75736 = CARTESIAN_POINT ( 'NONE',  ( -1.482939632545930975, -0.3690944881889765550, -0.3153832671262227771 ) ) ;
#75737 = CARTESIAN_POINT ( 'NONE',  ( -1.174540682414697335, -0.3162353388693409650, -0.4822834645669289433 ) ) ;
#75738 = CARTESIAN_POINT ( 'NONE',  ( -0.7283464566929126471, 0.1660481256975883668, -0.3530559997133364547 ) ) ;
#75739 = CARTESIAN_POINT ( 'NONE',  ( -1.423884514435694859, -0.05778040916215560624, -0.4822834645669293319 ) ) ;
#75740 = CARTESIAN_POINT ( 'NONE',  ( -0.3917322834645671215, 0.1049643490035301469, -1.377296587926508664 ) ) ;
#75741 = FACE_OUTER_BOUND ( 'NONE', #28773, .T. ) ;
#75742 = CARTESIAN_POINT ( 'NONE',  ( 1.089238845144357759, 0.05413385826771626580, -0.4176697321401330321 ) ) ;
#75743 = CARTESIAN_POINT ( 'NONE',  ( 0.5971128608923891301, 0.2952755905511810774, -0.1292274648535930714 ) ) ;
#75744 = DIRECTION ( 'NONE',  ( -0.000000000000000000, -0.000000000000000000, 1.000000000000000000 ) ) ;
#75745 = CARTESIAN_POINT ( 'NONE',  ( 0.1998031496062994128, -0.3460692066303957537, -2.373359580052493367 ) ) ;
#75746 = CARTESIAN_POINT ( 'NONE',  ( 1.259842519685040019, -0.1870078740157479769, 0.3641732283464567677 ) ) ;
#75747 = B_SPLINE_CURVE_WITH_KNOTS ( 'NONE', 3,
 ( #18461, #5813, #48777, #16823, #68159, #10503, #55912 ),
 .UNSPECIFIED., .F., .F.,
 ( 4, 3, 4 ),
 ( 3.469446951953614189E-18, 0.001246230184515571522, 0.002492489877932649398 ),
 .UNSPECIFIED. ) ;
#75748 = CARTESIAN_POINT ( 'NONE',  ( 0.1998031496062994405, -0.3460692066303958092, -1.036745406824147064 ) ) ;
#75749 = VERTEX_POINT ( 'NONE', #30884 ) ;
#75750 = CARTESIAN_POINT ( 'NONE',  ( -0.1958661417322836718, 0.3392501089628017219, -2.524934383202099397 ) ) ;
#75751 = VERTEX_POINT ( 'NONE', #69199 ) ;
#75752 = CARTESIAN_POINT ( 'NONE',  ( 0.4330708661417329575, -0.6692913385826771977, 8.415575281601705876E-17 ) ) ;
#75753 = CARTESIAN_POINT ( 'NONE',  ( -0.6627296587926503335, -0.6692913385826771977, 0.1292274648535927661 ) ) ;
#75754 = CARTESIAN_POINT ( 'NONE',  ( 1.561679790026247350, -0.4281496062992124485, 0.4176697321401328655 ) ) ;
#75755 = CARTESIAN_POINT ( 'NONE',  ( 0.9973753280839902091, -0.6046776061558807314, 0.2411417322834647770 ) ) ;
#75756 = CARTESIAN_POINT ( 'NONE',  ( -1.653543307086613234, -0.1870078740157479769, 0.3641732283464567677 ) ) ;
#75757 = DIRECTION ( 'NONE',  ( 0.7071067811865489050, 2.189697074797801291E-16, -0.7071067811865460184 ) ) ;
#75758 = CARTESIAN_POINT ( 'NONE',  ( -0.1706036745406816491, 0.05413385826771626580, -0.4176697321401330321 ) ) ;
#75759 = CARTESIAN_POINT ( 'NONE',  ( -1.423884514435694859, -0.05778040916215560624, -0.4822834645669293319 ) ) ;
#75760 = CARTESIAN_POINT ( 'NONE',  ( -1.502624671916009680, -0.3162353388693405765, 0.4822834645669290543 ) ) ;
#75761 = CARTESIAN_POINT ( 'NONE',  ( 1.417322834645670104, -0.1870078740157480879, -0.4822834645669291653 ) ) ;
#75762 = CARTESIAN_POINT ( 'NONE',  ( 0.2867679344610365999, 0.2867679344610365999, -2.742125984251967630 ) ) ;
#75763 = CARTESIAN_POINT ( 'NONE',  ( 0.6496062992125991586, -0.4536011799217368745, -0.2665933059059886201 ) ) ;
#75764 = ORIENTED_EDGE ( 'NONE', *, *, #8497, .T. ) ;
#75765 = CARTESIAN_POINT ( 'NONE',  ( 4.837279021331060870E-17, -0.3949938075777409963, -0.07874015748031501505 ) ) ;
#75766 = ORIENTED_EDGE ( 'NONE', *, *, #57587, .F. ) ;
#75767 = CARTESIAN_POINT ( 'NONE',  ( 0.07217847769028949700, -0.08942795157528024563, -0.3641732283464568787 ) ) ;
#75768 = CARTESIAN_POINT ( 'NONE',  ( -1.541994750656167090, 0.2952755905511811885, 0.1292274648535926551 ) ) ;
#75769 = CARTESIAN_POINT ( 'NONE',  ( 0.3674540682414705883, 0.2306618581243847221, -0.2411417322834647770 ) ) ;
#75770 = CARTESIAN_POINT ( 'NONE',  ( 0.3149606299212603933, -0.1870078740157479769, 0.4822834645669291653 ) ) ;
#75771 = CARTESIAN_POINT ( 'NONE',  ( -0.6955380577427815458, -0.4281496062992127816, -0.4176697321401328100 ) ) ;
#75772 = AXIS2_PLACEMENT_3D ( 'NONE', #4536, #55455, #61789 ) ;
#75773 = CARTESIAN_POINT ( 'NONE',  ( -0.3917322834645671770, 0.1049643490035302024, -1.604350024443256695 ) ) ;
#75774 = CARTESIAN_POINT ( 'NONE',  ( -1.108923884514435132, -0.05778040916215560624, -0.4822834645669293319 ) ) ;
#75775 = CARTESIAN_POINT ( 'NONE',  ( -0.3392501089628019995, 0.1958661417322832277, -2.630577427821522374 ) ) ;
#75776 = CARTESIAN_POINT ( 'NONE',  ( 1.502624671916010790, -0.2845877964562161244, -0.3641732283464567121 ) ) ;
#75777 = CARTESIAN_POINT ( 'NONE',  ( -0.8398950131233585692, 0.2306618581243848609, 0.2411417322834645549 ) ) ;
#75778 = CARTESIAN_POINT ( 'NONE',  ( 0.6955380577427828781, -0.4281496062992124485, 0.4176697321401328655 ) ) ;
#75779 = CARTESIAN_POINT ( 'NONE',  ( 1.233595800524935227, 0.2306618581243847221, -0.2411417322834647770 ) ) ;
#75780 = CARTESIAN_POINT ( 'NONE',  ( 0.1070741851644053527, 0.3996062992125986590, -0.9383202099737533164 ) ) ;
#75781 = CARTESIAN_POINT ( 'NONE',  ( -1.555118110236219930, 0.1660481256975885056, 0.3530559997133364547 ) ) ;
#75782 = CARTESIAN_POINT ( 'NONE',  ( -0.3996062992125986590, 0.1070741851644051723, -0.2670603674540683037 ) ) ;
#75783 = CARTESIAN_POINT ( 'NONE',  ( 0.1837270341207354329, 0.2306618581243848609, 0.2411417322834645549 ) ) ;
#75784 = CARTESIAN_POINT ( 'NONE',  ( 4.893765752498283924E-17, -0.3996062992125986035, -2.440944881889763884 ) ) ;
#75785 = CARTESIAN_POINT ( 'NONE',  ( 0.3392501089628018884, -0.1958661417322834220, -1.764435695538057791 ) ) ;
#75786 = CARTESIAN_POINT ( 'NONE',  ( 1.627296587926509996, -0.6046776061558807314, 0.2411417322834647770 ) ) ;
#75787 = CARTESIAN_POINT ( 'NONE',  ( 0.1115485564304470323, 0.1771653543307087630, 0.09757992244046791164 ) ) ;
#75788 = CARTESIAN_POINT ( 'NONE',  ( 0.8333333333333340365, 0.2952755905511810774, -0.1292274648535930714 ) ) ;
#75789 = CARTESIAN_POINT ( 'NONE',  ( 0.4091458600556404646, -0.2362204724409448231, -1.126640419947506633 ) ) ;
#75790 = CARTESIAN_POINT ( 'NONE',  ( 0.8267716535433078384, -0.5511811023622047445, 6.969142054262312111E-17 ) ) ;
#75791 = CARTESIAN_POINT ( 'NONE',  ( 0.5380577427821529035, 0.05413385826771626580, -0.4176697321401330321 ) ) ;
#75792 = CARTESIAN_POINT ( 'NONE',  ( 0.1974969037888706092, -0.3420746716998660508, -1.113517060367454015 ) ) ;
#75793 = CARTESIAN_POINT ( 'NONE',  ( -0.7480314960629914633, 0.2952755905511811885, 0.000000000000000000 ) ) ;
#75794 = DIRECTION ( 'NONE',  ( 0.000000000000000000, 1.000000000000000000, -0.000000000000000000 ) ) ;
#75795 = CARTESIAN_POINT ( 'NONE',  ( 0.7939632545931766261, -0.08942795157527998196, 0.3641732283464567121 ) ) ;
#75796 = DIRECTION ( 'NONE',  ( 1.000000000000000000, -0.000000000000000000, -0.000000000000000000 ) ) ;
#75798 = ADVANCED_FACE ( 'NONE', ( #43915 ), #44385, .F. ) ;
#75797 = CARTESIAN_POINT ( 'NONE',  ( -0.3412073490813641308, -0.6046776061558807314, 0.2411417322834647770 ) ) ;
#75799 = CARTESIAN_POINT ( 'NONE',  ( 0.3215223097112867578, -0.2845877964562161244, -0.3641732283464567121 ) ) ;
#75800 = CARTESIAN_POINT ( 'NONE',  ( -2.750540364621139933, 1.199841186584425845, 0.3336616047370347671 ) ) ;
#75801 = CARTESIAN_POINT ( 'NONE',  ( -0.2427821522309703550, -0.05778040916215560624, -0.4822834645669293319 ) ) ;
#75802 = CARTESIAN_POINT ( 'NONE',  ( 0.7086614173228352742, -0.1870078740157480601, -0.3641732283464567677 ) ) ;
#75803 = CARTESIAN_POINT ( 'NONE',  ( -1.114295247146195988, 1.305470409705170549E-15, -0.3627985898453510161 ) ) ;
#75804 = CARTESIAN_POINT ( 'NONE',  ( -0.3996062992125986590, 0.1070741851644051723, -1.684383202099737575 ) ) ;
#75805 = CARTESIAN_POINT ( 'NONE',  ( 0.2427821522309719648, -0.05778040916215522460, 0.4822834645669289988 ) ) ;
#75806 = EDGE_CURVE ( 'NONE', #41865, #29189, #53159, .T. ) ;
#75807 = CARTESIAN_POINT ( 'NONE',  ( 1.259842519685040019, -0.1870078740157480601, -0.3641732283464567677 ) ) ;
#75808 = CARTESIAN_POINT ( 'NONE',  ( 2.362204724409448620, 1.724409448818900570, -0.5118110236220390075 ) ) ;
#75809 = CARTESIAN_POINT ( 'NONE',  ( -0.4724409448818890911, -0.1870078740157479769, 0.3641732283464567677 ) ) ;
#75810 = CARTESIAN_POINT ( 'NONE',  ( -0.6233595800524928121, -0.08942795157527998196, 0.3641732283464567121 ) ) ;
#75811 = CARTESIAN_POINT ( 'NONE',  ( -0.5118110236220466680, 0.2952755905511811885, 0.000000000000000000 ) ) ;
#75812 = CARTESIAN_POINT ( 'NONE',  ( 0.4461942257217855201, -0.6046776061558807314, 0.2411417322834647770 ) ) ;
#75813 = CARTESIAN_POINT ( 'NONE',  ( 0.9645669291338591078, -0.4536011799217368745, -0.2665933059059886201 ) ) ;
#75814 = CARTESIAN_POINT ( 'NONE',  ( 0.4111343648323678157, 1.298683528505548468, -1.044172509125263160 ) ) ;
#75815 = CARTESIAN_POINT ( 'NONE',  ( 1.496062992125984703, -0.1870078740157480601, -0.3641732283464567677 ) ) ;
#75816 = VECTOR ( 'NONE', #30112, 39.37007874015748143 ) ;
#75817 = CARTESIAN_POINT ( 'NONE',  ( 0.9055118110236227702, 0.2952755905511811885, 0.000000000000000000 ) ) ;
#75818 = EDGE_CURVE ( 'NONE', #11040, #80330, #66265, .T. ) ;
#75819 = CARTESIAN_POINT ( 'NONE',  ( 0.4698482617964849783, 1.469690627553814410, -2.159191069290731679 ) ) ;
#75820 = CARTESIAN_POINT ( 'NONE',  ( -0.2296587926509179312, -0.3162353388693409650, -0.4822834645669289433 ) ) ;
#75821 = CARTESIAN_POINT ( 'NONE',  ( -0.1958661417322836718, 0.3392501089628017219, -0.8851706036745407014 ) ) ;
#75822 = CARTESIAN_POINT ( 'NONE',  ( 0.9383202099737538715, -0.05778040916215560624, -0.4822834645669293319 ) ) ;
#75823 = CARTESIAN_POINT ( 'NONE',  ( 0.4724409448818904789, -0.1870078740157480879, -0.4822834645669291653 ) ) ;
#75824 = ADVANCED_FACE ( 'NONE', ( #56839 ), #11009, .F. ) ;
#75825 = CARTESIAN_POINT ( 'NONE',  ( -0.1232682223025967638, 1.078237662714072176, -3.935195272298547042 ) ) ;
#75826 = CARTESIAN_POINT ( 'NONE',  ( 0.2493438320209980519, -0.004921259842519576551, 0.3153832671262227771 ) ) ;
#75827 = CARTESIAN_POINT ( 'NONE',  ( 1.017060367454068803, -0.3162353388693405765, 0.4822834645669290543 ) ) ;
#75828 = CARTESIAN_POINT ( 'NONE',  ( 0.1377952755905518800, -0.4536011799217367080, 0.2665933059059888421 ) ) ;
#75829 = CARTESIAN_POINT ( 'NONE',  ( -0.3937007874015740483, -0.1870078740157479769, 0.4822834645669291653 ) ) ;
#75830 = CARTESIAN_POINT ( 'NONE',  ( -1.840814964558169287, 2.729664688135040596, 0.5314960629921260393 ) ) ;
#75831 = CARTESIAN_POINT ( 'NONE',  ( 0.1181102362204730916, -0.6692913385826771977, 8.415575281601705876E-17 ) ) ;
#75832 = CARTESIAN_POINT ( 'NONE',  ( -0.8005249343832011588, 0.05413385826771626580, -0.4176697321401330321 ) ) ;
#75833 = CARTESIAN_POINT ( 'NONE',  ( -0.1640419947506555343, -0.2845877964562159024, 0.3641732283464567677 ) ) ;
#75834 = CARTESIAN_POINT ( 'NONE',  ( 0.3543307086614179147, 0.2952755905511811885, 0.000000000000000000 ) ) ;
#75835 = CARTESIAN_POINT ( 'NONE',  ( 0.8136482939632553313, -0.5023911411419708095, -0.1820866141732282451 ) ) ;
#75836 = CARTESIAN_POINT ( 'NONE',  ( -0.3937007874015740483, -0.1870078740157479769, 0.4822834645669291653 ) ) ;
#75838 = CARTESIAN_POINT ( 'NONE',  ( 1.286089238845145033, 0.2306618581243848609, 0.2411417322834645549 ) ) ;
#75837 = CARTESIAN_POINT ( 'NONE',  ( 0.4177787735907000366, 0.4110443821404751730, -1.736336963694947944 ) ) ;
#75839 = CARTESIAN_POINT ( 'NONE',  ( 1.574803149606299746, -0.1870078740157480879, -0.4822834645669291653 ) ) ;
#75840 = CARTESIAN_POINT ( 'NONE',  ( 0.3392501089628018329, 0.1958661417322835607, -2.013123359580052618 ) ) ;
#75841 = CARTESIAN_POINT ( 'NONE',  ( -1.286089238845143479, 0.2306618581243847221, -0.2411417322834647770 ) ) ;
#75842 = CARTESIAN_POINT ( 'NONE',  ( -0.8792650918635160906, 0.05413385826771626580, -0.4176697321401330321 ) ) ;
#75843 = CARTESIAN_POINT ( 'NONE',  ( -0.4091458600556405756, 0.2362204724409446288, -0.4986876640419947715 ) ) ;
#75844 = CARTESIAN_POINT ( 'NONE',  ( -0.1058382717557503211, 0.3949938075777409408, -2.841207349081365408 ) ) ;
#75845 = VERTEX_POINT ( 'NONE', #70307 ) ;
#75846 = CARTESIAN_POINT ( 'NONE',  ( 0.3740157480314966754, -0.4536011799217367080, 0.2665933059059888421 ) ) ;
#75847 = CARTESIAN_POINT ( 'NONE',  ( -0.3917322834645670104, -7.196005306013484475E-17, -1.291338582677165503 ) ) ;
#75848 = CARTESIAN_POINT ( 'NONE',  ( 0.8267716535433077274, 0.2952755905511811885, 0.000000000000000000 ) ) ;
#75849 = CARTESIAN_POINT ( 'NONE',  ( 0.1265901696524990294, -0.4724409448818896462, -2.290026246719159442 ) ) ;
#75850 = CARTESIAN_POINT ( 'NONE',  ( 0.9908136482939640111, 0.2952755905511810219, -0.1292274648535930437 ) ) ;
#75851 = CARTESIAN_POINT ( 'NONE',  ( -0.3871391076115476282, -0.08942795157527998196, 0.3641732283464567121 ) ) ;
#75852 = CARTESIAN_POINT ( 'NONE',  ( 0.4849061582275024929, 1.805669738366188382, -0.4921425059946357150 ) ) ;
#75853 = CARTESIAN_POINT ( 'NONE',  ( 1.017060367454068803, -0.3162353388693405765, 0.4822834645669290543 ) ) ;
#75854 = CARTESIAN_POINT ( 'NONE',  ( 1.364829396325459854, -0.5023911411419708095, -0.1820866141732282451 ) ) ;
#75855 = CARTESIAN_POINT ( 'NONE',  ( -0.1181102362204717315, -0.6692913385826771977, 8.415575281601705876E-17 ) ) ;
#75856 = CARTESIAN_POINT ( 'NONE',  ( 0.3392501089628018329, 0.1958661417322835052, -0.8411880332995258502 ) ) ;
#75857 = CARTESIAN_POINT ( 'NONE',  ( -0.4527559055118102749, -0.5400638737290845981, -0.3530559997133363437 ) ) ;
#75858 = CARTESIAN_POINT ( 'NONE',  ( -1.469816272965878357, -0.5023911411419708095, -0.1820866141732282451 ) ) ;
#75859 = CARTESIAN_POINT ( 'NONE',  ( -0.3805774278215216522, -0.4281496062992127816, -0.4176697321401328100 ) ) ;
#75860 = CARTESIAN_POINT ( 'NONE',  ( 1.646981627296588035, -0.3162353388693405765, 0.4822834645669290543 ) ) ;
#75861 = CARTESIAN_POINT ( 'NONE',  ( -0.3230088838496750214, 1.189621120221113770, -1.964944096575241828 ) ) ;
#75862 = ORIENTED_EDGE ( 'NONE', *, *, #50024, .F. ) ;
#75863 = CARTESIAN_POINT ( 'NONE',  ( 0.3917322834645670659, 2.398668435337828261E-17, -2.162092806595487637 ) ) ;
#75864 = CARTESIAN_POINT ( 'NONE',  ( 0.4724409448818904789, -0.1870078740157480879, -0.4822834645669291653 ) ) ;
#75865 = ORIENTED_EDGE ( 'NONE', *, *, #13485, .F. ) ;
#75866 = CARTESIAN_POINT ( 'NONE',  ( -0.2099737532808391705, -0.6046776061558809534, -0.2411417322834644161 ) ) ;
#75867 = CARTESIAN_POINT ( 'NONE',  ( -1.423884514435694859, -0.05778040916215560624, -0.4822834645669293319 ) ) ;
#75868 = CARTESIAN_POINT ( 'NONE',  ( 0.6036745406824153282, -0.6046776061558807314, 0.2411417322834647770 ) ) ;
#75869 = CARTESIAN_POINT ( 'NONE',  ( -0.1115485564304453947, -0.6692913385826771977, 0.1292274648535927661 ) ) ;
#75870 = CARTESIAN_POINT ( 'NONE',  ( -0.3392501089628019995, 0.1958661417322832277, -1.528215223097112885 ) ) ;
#75871 = CARTESIAN_POINT ( 'NONE',  ( -0.8923884514435688198, 0.2306618581243847221, -0.2411417322834647770 ) ) ;
#75872 = CARTESIAN_POINT ( 'NONE',  ( 0.4265091863517067594, 0.2952755905511811885, 0.1292274648535926551 ) ) ;
#75873 = CARTESIAN_POINT ( 'NONE',  ( -0.6036745406824141069, -0.6046776061558809534, -0.2411417322834644161 ) ) ;
#75874 =( GEOMETRIC_REPRESENTATION_CONTEXT ( 3 ) GLOBAL_UNCERTAINTY_ASSIGNED_CONTEXT ( ( #71458 ) ) GLOBAL_UNIT_ASSIGNED_CONTEXT ( ( #23816, #60877, #42753 ) ) REPRESENTATION_CONTEXT ( 'NONE', 'WORKASPACE' ) );
#75875 = CARTESIAN_POINT ( 'NONE',  ( 0.2821522309711292364, 0.1771653543307087075, -0.09757992244046823083 ) ) ;
#75876 = CARTESIAN_POINT ( 'NONE',  ( -0.2710828156362889985, -0.1173918767474883551, 5.835147349599719035 ) ) ;
#75877 = CARTESIAN_POINT ( 'NONE',  ( 0.07874015748031558404, -0.1870078740157480879, -0.4822834645669291653 ) ) ;
#75878 = CARTESIAN_POINT ( 'NONE',  ( 0.3025410870193226964, 2.784432375088962958E-17, -0.3464511005275205946 ) ) ;
#75879 = EDGE_CURVE ( 'NONE', #52953, #23282, #34101, .T. ) ;
#75880 = CARTESIAN_POINT ( 'NONE',  ( -1.633858267716534529, 0.1660481256975885056, 0.3530559997133364547 ) ) ;
#75881 = CARTESIAN_POINT ( 'NONE',  ( 0.3917322834645670104, -0.1049643490035303411, -2.780839895013122565 ) ) ;
#75882 = ORIENTED_EDGE ( 'NONE', *, *, #15723, .F. ) ;
#75883 = ORIENTED_EDGE ( 'NONE', *, *, #27454, .F. ) ;
#75884 = CARTESIAN_POINT ( 'NONE',  ( 0.6955380577427828781, -0.4281496062992124485, 0.4176697321401328655 ) ) ;
#75885 = CARTESIAN_POINT ( 'NONE',  ( 0.1837270341207354329, 0.1283753931104748280, 0.1820866141732283561 ) ) ;
#75887 = FACE_OUTER_BOUND ( 'NONE', #24789, .T. ) ;
#75886 = CARTESIAN_POINT ( 'NONE',  ( 0.9559795740584967616, -8.614921172258640174E-17, 0.3954974714151467396 ) ) ;
#75888 = CARTESIAN_POINT ( 'NONE',  ( 0.1049643490035303689, 0.3917322834645670104, -1.337926509186352142 ) ) ;
#75889 = CARTESIAN_POINT ( 'NONE',  ( 5.785732909357575061E-17, -0.4724409448818898682, 0.1594488188976377896 ) ) ;
#75890 = DIRECTION ( 'NONE',  ( 0.000000000000000000, 0.000000000000000000, 1.000000000000000000 ) ) ;
#75891 = CIRCLE ( 'NONE', #39591, 3.543307086614173596 ) ;
#75892 = CARTESIAN_POINT ( 'NONE',  ( 0.3996062992125986035, -0.1070741851644052972, -2.865485564304462329 ) ) ;
#75893 = CARTESIAN_POINT ( 'NONE',  ( 0.2755905511811031494, -0.6692913385826771977, 8.415575281601705876E-17 ) ) ;
#75894 = CARTESIAN_POINT ( 'NONE',  ( -1.305774278215222184, 0.2952755905511811885, 0.1292274648535926551 ) ) ;
#75895 = CARTESIAN_POINT ( 'NONE',  ( -1.259842519685038686, -0.1870078740157479769, 0.4822834645669291653 ) ) ;
#75896 = CARTESIAN_POINT ( 'NONE',  ( 0.4396325459317590445, -0.6692913385826771977, 0.1292274648535927661 ) ) ;
#75897 = CARTESIAN_POINT ( 'NONE',  ( 0.9186351706036751663, -0.6046776061558807314, 0.2411417322834647770 ) ) ;
#75898 = CARTESIAN_POINT ( 'NONE',  ( 1.541994750656168645, 0.1771653543307087075, -0.09757992244046823083 ) ) ;
#75899 = CARTESIAN_POINT ( 'NONE',  ( 1.167979002624672580, -0.3690944881889763329, 0.3153832671262228327 ) ) ;
#75900 = CARTESIAN_POINT ( 'NONE',  ( -0.8333333333333323711, 0.2952755905511811885, 0.1292274648535926551 ) ) ;
#75901 = CARTESIAN_POINT ( 'NONE',  ( 0.1070741851644054776, -0.3996062992125984925, -0.6345144356955381149 ) ) ;
#75902 = CARTESIAN_POINT ( 'NONE',  ( 1.535433070866142558, 0.2952755905511811885, 0.000000000000000000 ) ) ;
#75903 = EDGE_CURVE ( 'NONE', #66338, #26273, #33277, .T. ) ;
#75904 = CARTESIAN_POINT ( 'NONE',  ( 0.1049643490035304938, -0.3917322834645669549, -0.3923884514435695414 ) ) ;
#75905 = CARTESIAN_POINT ( 'NONE',  ( -0.07874015748031421014, -0.1870078740157479769, 0.4822834645669291653 ) ) ;
#75907 = CARTESIAN_POINT ( 'NONE',  ( -0.2885979965725595231, 1.160566086728933133, 1.939267709711407717 ) ) ;
#75906 = CARTESIAN_POINT ( 'NONE',  ( 1.082677165354331228, 0.1660481256975883668, -0.3530559997133364547 ) ) ;
#75908 = CARTESIAN_POINT ( 'NONE',  ( -1.489501312335957062, -0.2845877964562161244, -0.3641732283464567121 ) ) ;
#75909 = CARTESIAN_POINT ( 'NONE',  ( 0.1377952755905518800, 0.1660481256975883668, -0.3530559997133364547 ) ) ;
#75910 = CARTESIAN_POINT ( 'NONE',  ( 0.7611548556430451917, -0.5023911411419708095, 0.1820866141732285504 ) ) ;
#75911 = CARTESIAN_POINT ( 'NONE',  ( -1.568241469816272105, -0.08942795157527998196, 0.3641732283464567121 ) ) ;
#75912 = CARTESIAN_POINT ( 'NONE',  ( 1.095800524934383846, -0.05778040916215560624, -0.4822834645669293319 ) ) ;
#75913 = CARTESIAN_POINT ( 'NONE',  ( 0.000000000000000000, 2.755905511811024056, 0.000000000000000000 ) ) ;
#75914 = CARTESIAN_POINT ( 'NONE',  ( -0.6036745406824141069, 0.1283753931104748280, 0.1820866141732283561 ) ) ;
#75915 = CARTESIAN_POINT ( 'NONE',  ( -0.7086614173228339419, -0.1870078740157480879, -0.4822834645669291653 ) ) ;
#75916 = CARTESIAN_POINT ( 'NONE',  ( 1.581364829396326277, -0.3162353388693409650, -0.4822834645669289433 ) ) ;
#75917 = CARTESIAN_POINT ( 'NONE',  ( -1.017060367454067249, -0.3162353388693409650, -0.4822834645669289433 ) ) ;
#75918 = CARTESIAN_POINT ( 'NONE',  ( 1.227034120734908917, 0.2952755905511810774, -0.1292274648535930714 ) ) ;
#75919 = CARTESIAN_POINT ( 'NONE',  ( -0.3917322834645670104, -0.1049643490035307020, -0.8300718092201594400 ) ) ;
#75920 = CARTESIAN_POINT ( 'NONE',  ( -1.371391076115484609, -0.5511811023622046335, 0.09757992244046803654 ) ) ;
#75921 = CARTESIAN_POINT ( 'NONE',  ( 1.016821367227983552, 1.537401574803149984, 0.4744094488188975722 ) ) ;
#75922 = CARTESIAN_POINT ( 'NONE',  ( 1.332020997375328974, -0.05778040916215560624, -0.4822834645669293319 ) ) ;
#75923 = CARTESIAN_POINT ( 'NONE',  ( 0.4724409448818896462, 0.1265901696524990294, -2.563648293963254776 ) ) ;
#75924 = CARTESIAN_POINT ( 'NONE',  ( -1.463254593175852492, -0.6692913385826773087, -0.1292274648535924053 ) ) ;
#75925 = CARTESIAN_POINT ( 'NONE',  ( -1.404199475065615932, -0.3690944881889765550, -0.3153832671262227771 ) ) ;
#75926 = CARTESIAN_POINT ( 'NONE',  ( -0.9514435695538050464, -0.2845877964562159024, 0.3641732283464567677 ) ) ;
#75927 = FACE_OUTER_BOUND ( 'NONE', #40729, .T. ) ;
#75928 = CARTESIAN_POINT ( 'NONE',  ( -0.2034120734908128059, 0.2952755905511811885, 0.1292274648535926551 ) ) ;
#75929 = CARTESIAN_POINT ( 'NONE',  ( 8.195543980992789655E-16, -0.1870078740157480601, -0.3641732283464567677 ) ) ;
#75930 = CARTESIAN_POINT ( 'NONE',  ( -1.102362204724408601, -0.1870078740157479769, 0.3641732283464567677 ) ) ;
#75931 = CARTESIAN_POINT ( 'NONE',  ( 1.358267716535433323, -0.4536011799217368745, -0.2665933059059886201 ) ) ;
#75932 = CARTESIAN_POINT ( 'NONE',  ( 0.8070866141732289112, -0.5400638737290845981, -0.3530559997133363437 ) ) ;
#75933 = CARTESIAN_POINT ( 'NONE',  ( 1.437007874015748810, 0.1660481256975885056, 0.3530559997133364547 ) ) ;
#75934 = CARTESIAN_POINT ( 'NONE',  ( 0.5774278215223104249, 0.1283753931104748280, 0.1820866141732283561 ) ) ;
#75935 = AXIS2_PLACEMENT_3D ( 'NONE', #62952, #43982, #36861 ) ;
#75936 = CARTESIAN_POINT ( 'NONE',  ( 0.4002624671916016896, -0.05778040916215522460, 0.4822834645669289988 ) ) ;
#75937 = CARTESIAN_POINT ( 'NONE',  ( 1.003937007874016185, 0.07958543189024071263, -0.2665933059059888421 ) ) ;
#75938 = EDGE_LOOP ( 'NONE', ( #58678, #20904, #54116, #67091 ) ) ;
#75939 = CARTESIAN_POINT ( 'NONE',  ( 1.496062992125984703, -0.1870078740157480879, -0.4822834645669291653 ) ) ;
#75940 = CARTESIAN_POINT ( 'NONE',  ( -1.213910761154854745, -0.6692913385826771977, 0.1292274648535927661 ) ) ;
#75941 = CARTESIAN_POINT ( 'NONE',  ( -0.05249343832020938322, -0.6046776061558809534, -0.2411417322834644161 ) ) ;
#75942 = CARTESIAN_POINT ( 'NONE',  ( -2.170146923806554273, 1.537401574803149984, -0.4744094488188975722 ) ) ;
#75943 = CARTESIAN_POINT ( 'NONE',  ( 0.1070741851644053388, 0.3996062992125986035, -2.589895013123359568 ) ) ;
#75944 = CARTESIAN_POINT ( 'NONE',  ( 0.3346456692913390985, 0.1660481256975885056, 0.3530559997133364547 ) ) ;
#75945 = CARTESIAN_POINT ( 'NONE',  ( 1.200787401574803681, -0.4536011799217368745, -0.2665933059059886201 ) ) ;
#75946 = CARTESIAN_POINT ( 'NONE',  ( 0.2165354330708668673, -0.5400638737290844871, 0.3530559997133364547 ) ) ;
#75947 = CARTESIAN_POINT ( 'NONE',  ( 0.1902887139107617975, 0.2952755905511811885, 0.1292274648535926551 ) ) ;
#75948 = EDGE_CURVE ( 'NONE', #39954, #49578, #16589, .T. ) ;
#75949 = CARTESIAN_POINT ( 'NONE',  ( 0.3996062992125986035, 0.1070741851644054776, -2.329396325459317296 ) ) ;
#75950 = VECTOR ( 'NONE', #205, 39.37007874015748143 ) ;
#75951 = CARTESIAN_POINT ( 'NONE',  ( -0.1974969037888706647, 0.3420746716998658843, -1.587926509186351920 ) ) ;
#75952 = CARTESIAN_POINT ( 'NONE',  ( -0.3247161055182421485, 1.191192147208269159, 1.074094784059450802 ) ) ;
#75953 = CARTESIAN_POINT ( 'NONE',  ( -0.3458507752293909498, 0.3458507752293908388, -2.539370078740157410 ) ) ;
#75954 = CARTESIAN_POINT ( 'NONE',  ( -0.3917322834645671215, 0.1049643490035301469, -0.4973753280839894875 ) ) ;
#75955 = EDGE_CURVE ( 'NONE', #22261, #47474, #70731, .T. ) ;
#75956 = CARTESIAN_POINT ( 'NONE',  ( -0.4396325459317579898, 0.1771653543307087630, 0.09757992244046791164 ) ) ;
#75957 = CARTESIAN_POINT ( 'NONE',  ( -0.8923884514435688198, 0.2306618581243847221, -0.2411417322834647770 ) ) ;
#75958 = CARTESIAN_POINT ( 'NONE',  ( 0.5839895013123367340, -0.6692913385826773087, -0.1292274648535924053 ) ) ;
#75959 = CARTESIAN_POINT ( 'NONE',  ( -0.3420746716998662729, 0.1974969037888702206, -2.465223097112861250 ) ) ;
#75960 = CARTESIAN_POINT ( 'NONE',  ( 0.7414698162729663755, 0.2952755905511811885, 0.1292274648535926551 ) ) ;
#75961 = CARTESIAN_POINT ( 'NONE',  ( -1.377952755905511140, -0.6692913385826771977, 8.415575281601705876E-17 ) ) ;
#75962 = CARTESIAN_POINT ( 'NONE',  ( 0.6299212598425204535, -0.1870078740157479769, 0.4822834645669291653 ) ) ;
#75963 = CARTESIAN_POINT ( 'NONE',  ( -0.6184250938292459310, -3.724876541855331158E-15, 0.3791475997938233422 ) ) ;
#75964 = CARTESIAN_POINT ( 'NONE',  ( -0.3460692066303960868, 0.1998031496062990242, -2.073490813648294129 ) ) ;
#75965 = CARTESIAN_POINT ( 'NONE',  ( 1.561679790026247350, 0.05413385826771626580, -0.4176697321401330321 ) ) ;
#75966 = CARTESIAN_POINT ( 'NONE',  ( 0.7677165354330716118, -0.5400638737290844871, 0.3530559997133364547 ) ) ;
#75967 = CARTESIAN_POINT ( 'NONE',  ( 0.3871391076115492380, -0.05778040916215560624, -0.4822834645669293319 ) ) ;
#75968 = CARTESIAN_POINT ( 'NONE',  ( 1.423884514435696191, -0.08942795157527998196, 0.3641732283464567121 ) ) ;
#75969 = CARTESIAN_POINT ( 'NONE',  ( 1.410761154855643795, -0.05778040916215560624, -0.4822834645669293319 ) ) ;
#75970 = CARTESIAN_POINT ( 'NONE',  ( -0.3392501089628019995, 0.1958661417322832277, -0.1108923884514436548 ) ) ;
#75971 = PLANE ( 'NONE',  #54700 ) ;
#75972 = CARTESIAN_POINT ( 'NONE',  ( 0.9580052493438327987, -0.4281496062992127816, -0.4176697321401328100 ) ) ;
#75973 = CARTESIAN_POINT ( 'NONE',  ( 1.594488188976378673, -0.4536011799217368745, -0.2665933059059886201 ) ) ;
#75974 = CARTESIAN_POINT ( 'NONE',  ( -0.3477690288713905509, -0.6692913385826771977, 0.1292274648535927661 ) ) ;
#75975 = CARTESIAN_POINT ( 'NONE',  ( -1.095800524934382292, -0.05778040916215522460, 0.4822834645669289988 ) ) ;
#75976 = CARTESIAN_POINT ( 'NONE',  ( 0.9842519685039375910, 0.2952755905511811885, 0.000000000000000000 ) ) ;
#75977 = CARTESIAN_POINT ( 'NONE',  ( 0.1958661417322836440, -0.3392501089628017219, -0.6489501312335959060 ) ) ;
#75978 = CARTESIAN_POINT ( 'NONE',  ( -0.1958661417322834220, -0.3392501089628018884, -1.632545931758530244 ) ) ;
#75979 = CARTESIAN_POINT ( 'NONE',  ( -0.1958661417322836718, 0.3392501089628017219, -2.524934383202099397 ) ) ;
#75980 = CARTESIAN_POINT ( 'NONE',  ( 1.522309711286089939, 0.2306618581243848609, 0.2411417322834645549 ) ) ;
#75981 = ORIENTED_EDGE ( 'NONE', *, *, #16494, .F. ) ;
#75982 = CARTESIAN_POINT ( 'NONE',  ( 0.1974969037888704704, 0.3420746716998660508, -2.506561679790026087 ) ) ;
#75983 = ORIENTED_EDGE ( 'NONE', *, *, #68146, .F. ) ;
#75984 = DIRECTION ( 'NONE',  ( 0.000000000000000000, 0.000000000000000000, -1.000000000000000000 ) ) ;
#75985 = CARTESIAN_POINT ( 'NONE',  ( 1.561679790026247350, -0.3690944881889763329, 0.3153832671262228327 ) ) ;
#75986 = CARTESIAN_POINT ( 'NONE',  ( -0.2925321140481930704, -0.2925321140481933480, -1.476377952755905554 ) ) ;
#75987 = CARTESIAN_POINT ( 'NONE',  ( 1.450131233595801428, -0.5511811023622048555, -0.09757992244046775898 ) ) ;
#75988 = CARTESIAN_POINT ( 'NONE',  ( -3.821484228344193657, 2.755905511811024056, -0.5314960629921260393 ) ) ;
#75989 = CARTESIAN_POINT ( 'NONE',  ( 0.000000000000000000, 1.724409448818897905, -2.362204724409448620 ) ) ;
#75990 = CARTESIAN_POINT ( 'NONE',  ( 0.8537221893815273299, 2.409604939980833412E-17, -0.3464511005275205946 ) ) ;
#75991 = CARTESIAN_POINT ( 'NONE',  ( 0.1049643490035303689, 0.3917322834645670104, -0.3930446194225722945 ) ) ;
#75992 = CARTESIAN_POINT ( 'NONE',  ( -0.5380577427821514602, -0.004921259842519576551, 0.3153832671262227771 ) ) ;
#75993 = CARTESIAN_POINT ( 'NONE',  ( -1.102362204724408601, -0.1870078740157479769, 0.3641732283464567677 ) ) ;
#75994 = CARTESIAN_POINT ( 'NONE',  ( -1.430446194225720724, 0.05413385826771626580, -0.4176697321401330321 ) ) ;
#75995 = CARTESIAN_POINT ( 'NONE',  ( 0.1115485564304467270, -0.6692913385826773087, -0.1292274648535924053 ) ) ;
#75996 = CARTESIAN_POINT ( 'NONE',  ( -1.620734908136482577, 0.2952755905511811885, 0.1292274648535926551 ) ) ;
#75997 = ORIENTED_EDGE ( 'NONE', *, *, #66513, .T. ) ;
#75998 = CARTESIAN_POINT ( 'NONE',  ( -1.614173228346455824, 0.2952755905511811885, 0.000000000000000000 ) ) ;
#75999 = CARTESIAN_POINT ( 'NONE',  ( -1.013613127888308485, -2.191421614605370878E-15, 0.4445507791589071167 ) ) ;
#76000 =( LENGTH_UNIT ( ) NAMED_UNIT ( * ) SI_UNIT ( $, .METRE. ) );
#76001 = CARTESIAN_POINT ( 'NONE',  ( -0.3458507752293906723, -0.3458507752293910609, -1.948818897637795144 ) ) ;
#76002 = CARTESIAN_POINT ( 'NONE',  ( 2.795275590551181466, 2.793565526369266916, 0.000000000000000000 ) ) ;
#76003 = CARTESIAN_POINT ( 'NONE',  ( -0.4265091863517051496, -0.5511811023622046335, 0.09757992244046803654 ) ) ;
#76004 = CARTESIAN_POINT ( 'NONE',  ( -1.351706036745406347, -0.4281496062992124485, 0.4176697321401328655 ) ) ;
#76005 = CARTESIAN_POINT ( 'NONE',  ( 1.095800524934383846, -0.05778040916215560624, -0.4822834645669293319 ) ) ;
#76006 = EDGE_LOOP ( 'NONE', ( #34554, #56499, #53682, #62632 ) ) ;
#76008 = DIRECTION ( 'NONE',  ( 0.000000000000000000, 0.000000000000000000, 1.000000000000000000 ) ) ;
#76007 = CARTESIAN_POINT ( 'NONE',  ( 5.785732909357575061E-17, -0.4724409448818898682, -2.283464566929133799 ) ) ;
#76009 = CARTESIAN_POINT ( 'NONE',  ( 1.555118110236221041, 0.1660481256975883668, -0.3530559997133364547 ) ) ;
#76010 = CARTESIAN_POINT ( 'NONE',  ( -1.286089238845143479, -0.6046776061558807314, 0.2411417322834647770 ) ) ;
#76011 = CARTESIAN_POINT ( 'NONE',  ( -0.3917322834645668994, -0.1049643490035306742, -0.5984058810685547458 ) ) ;
#76012 = CARTESIAN_POINT ( 'NONE',  ( -0.1968503937007867743, -0.5511811023622047445, 6.969142054262312111E-17 ) ) ;
#76013 = CARTESIAN_POINT ( 'NONE',  ( 0.2867679344610366554, -0.2867679344610365444, -0.8129921259842519676 ) ) ;
#76014 = CARTESIAN_POINT ( 'NONE',  ( -0.4396325459317577122, -0.5511811023622048555, -0.09757992244046775898 ) ) ;
#76015 = CARTESIAN_POINT ( 'NONE',  ( 0.6758530183727039509, 0.1771653543307087075, -0.09757992244046823083 ) ) ;
#76016 = CARTESIAN_POINT ( 'NONE',  ( 0.09186351706036799403, -0.4281496062992127816, -0.4176697321401328100 ) ) ;
#76017 = CARTESIAN_POINT ( 'NONE',  ( -0.5971128608923877978, -0.5511811023622048555, -0.09757992244046775898 ) ) ;
#76018 = CARTESIAN_POINT ( 'NONE',  ( 0.2867679344610365999, 0.2867679344610365999, -2.649606299212598604 ) ) ;
#76019 = CARTESIAN_POINT ( 'NONE',  ( 1.246719160104987623, -0.4281496062992124485, 0.4176697321401328655 ) ) ;
#76020 = B_SPLINE_CURVE_WITH_KNOTS ( 'NONE', 3,
 ( #25276, #44214, #43390, #75415 ),
 .UNSPECIFIED., .F., .F.,
 ( 4, 4 ),
 ( 0.08702371034448001808, 0.08847090869701748628 ),
 .UNSPECIFIED. ) ;
#76021 = CARTESIAN_POINT ( 'NONE',  ( -1.207349081364828436, -0.6046776061558807314, 0.2411417322834647770 ) ) ;
#76022 = CARTESIAN_POINT ( 'NONE',  ( 0.4091458600556403535, 0.2362204724409449896, -0.8379265091863516979 ) ) ;
#76023 = CARTESIAN_POINT ( 'NONE',  ( -0.5249343832020990641, -0.6046776061558809534, -0.2411417322834644161 ) ) ;
#76024 = CARTESIAN_POINT ( 'NONE',  ( -0.7677165354330699465, -0.5400638737290845981, -0.3530559997133363437 ) ) ;
#76025 = CARTESIAN_POINT ( 'NONE',  ( 1.417322834645670104, -0.1870078740157480601, -0.3641732283464567677 ) ) ;
#76026 = CARTESIAN_POINT ( 'NONE',  ( 0.2362204724409456558, -0.1870078740157480601, -0.3641732283464567677 ) ) ;
#76027 = CARTESIAN_POINT ( 'NONE',  ( -0.3740157480314953431, -0.5400638737290845981, -0.3530559997133363437 ) ) ;
#76028 = CARTESIAN_POINT ( 'NONE',  ( -1.023622047244093558, -0.1870078740157479769, 0.4822834645669291653 ) ) ;
#76029 = CARTESIAN_POINT ( 'NONE',  ( -0.8785612751854012803, -2.613618158232546091E-15, -0.3464511005275220379 ) ) ;
#76030 = CARTESIAN_POINT ( 'NONE',  ( 0.1181102362204724532, 0.04921259842519689481, 0.08523872084492503665 ) ) ;
#76031 = CARTESIAN_POINT ( 'NONE',  ( -0.3477690288713902178, 0.2952755905511810774, -0.1292274648535930714 ) ) ;
#76032 = CARTESIAN_POINT ( 'NONE',  ( -0.9973753280839886548, -0.6046776061558809534, -0.2411417322834644161 ) ) ;
#76033 = ORIENTED_EDGE ( 'NONE', *, *, #10993, .T. ) ;
#76034 = CARTESIAN_POINT ( 'NONE',  ( -0.3996062992125985480, -7.340648628747423112E-17, -2.163385826771653697 ) ) ;
#76035 = CARTESIAN_POINT ( 'NONE',  ( 1.253280839895013710, -0.3162353388693405765, 0.4822834645669290543 ) ) ;
#76036 = CARTESIAN_POINT ( 'NONE',  ( -0.7611548556430438595, 0.1283753931104748280, 0.1820866141732283561 ) ) ;
#76037 = CARTESIAN_POINT ( 'NONE',  ( -0.9776902887139098386, -0.6692913385826771977, 0.1292274648535927661 ) ) ;
#76038 = CARTESIAN_POINT ( 'NONE',  ( 1.122047244094488860, -0.5400638737290845981, -0.3530559997133363437 ) ) ;
#76039 = CARTESIAN_POINT ( 'NONE',  ( 0.7545931758530189937, 0.2952755905511810774, -0.1292274648535930714 ) ) ;
#76040 = CARTESIAN_POINT ( 'NONE',  ( 0.1265901696524990572, -0.4724409448818897017, -0.08530183727034119923 ) ) ;
#76041 = CARTESIAN_POINT ( 'NONE',  ( -1.161417322834644716, -0.4536011799217368745, -0.2665933059059886201 ) ) ;
#76043 = ADVANCED_FACE ( 'NONE', ( #6750 ), #26535, .T. ) ;
#76042 = CARTESIAN_POINT ( 'NONE',  ( 0.1998031496062992463, 0.3460692066303959202, -0.5360892388451443669 ) ) ;
#76044 = CARTESIAN_POINT ( 'NONE',  ( -0.3460692066303958092, -0.1998031496062994683, -0.9973753280839895430 ) ) ;
#76045 = CARTESIAN_POINT ( 'NONE',  ( -0.3420746716998659953, -0.1974969037888706647, -0.05249343832021002854 ) ) ;
#76046 = CARTESIAN_POINT ( 'NONE',  ( 0.4425803288943399583, 1.365943002350758384, 2.619481425262184526 ) ) ;
#76047 = CARTESIAN_POINT ( 'NONE',  ( 1.371391076115485941, 0.1771653543307087630, 0.09757992244046791164 ) ) ;
#76048 = CARTESIAN_POINT ( 'NONE',  ( 0.8333333333333340365, 0.1771653543307087075, -0.09757992244046823083 ) ) ;
#76049 = CARTESIAN_POINT ( 'NONE',  ( 0.4461942257217855201, -0.6046776061558807314, 0.2411417322834647770 ) ) ;
#76050 = CARTESIAN_POINT ( 'NONE',  ( 1.076935383196057305, 5.463695987328539379E-17, 0.3149606299212603933 ) ) ;
#76051 = CARTESIAN_POINT ( 'NONE',  ( -0.1058382717557497660, -0.3949938075777411073, -1.408792650918635259 ) ) ;
#76052 = CARTESIAN_POINT ( 'NONE',  ( 0.9645669291338591078, -0.4536011799217368745, -0.2665933059059886201 ) ) ;
#76053 = CARTESIAN_POINT ( 'NONE',  ( -0.1377952755905504645, -0.5400638737290845981, -0.3530559997133363437 ) ) ;
#76054 = CARTESIAN_POINT ( 'NONE',  ( -1.154855643044618851, 0.2306618581243848609, 0.2411417322834645549 ) ) ;
#76055 = CARTESIAN_POINT ( 'NONE',  ( 1.069553805774278832, 0.2952755905511810774, -0.1292274648535930714 ) ) ;
#76056 = CARTESIAN_POINT ( 'NONE',  ( 5.785732909357575061E-17, -0.4724409448818898682, -1.811023622047244208 ) ) ;
#76057 = CARTESIAN_POINT ( 'NONE',  ( 0.1998031496062992740, 0.3460692066303959757, -2.664041994750656173 ) ) ;
#76058 = AXIS2_PLACEMENT_3D ( 'NONE', #5175, #3528, #35931 ) ;
#76059 = CARTESIAN_POINT ( 'NONE',  ( -0.1377952755905504645, 0.07958543189024085140, 0.2665933059059887866 ) ) ;
#76060 = ORIENTED_EDGE ( 'NONE', *, *, #28501, .F. ) ;
#76061 = ORIENTED_EDGE ( 'NONE', *, *, #67561, .T. ) ;
#76062 = CARTESIAN_POINT ( 'NONE',  ( -0.9645669291338575535, -0.5400638737290844871, 0.3530559997133364547 ) ) ;
#76063 = CARTESIAN_POINT ( 'NONE',  ( -0.5577427821522301654, -0.3162353388693405765, 0.4822834645669290543 ) ) ;
#76064 = CARTESIAN_POINT ( 'NONE',  ( -0.5577427821522301654, -0.3162353388693405765, 0.4822834645669290543 ) ) ;
#76065 = DIMENSIONAL_EXPONENTS ( 1.000000000000000000, 0.000000000000000000, 0.000000000000000000, 0.000000000000000000, 0.000000000000000000, 0.000000000000000000, 0.000000000000000000 ) ;
#76066 = CARTESIAN_POINT ( 'NONE',  ( 0.4396325459317593221, 0.2952755905511810774, -0.1292274648535930714 ) ) ;
#76067 = CARTESIAN_POINT ( 'NONE',  ( -0.4658792650918627265, -0.3162353388693409650, -0.4822834645669289433 ) ) ;
#76068 = CARTESIAN_POINT ( 'NONE',  ( -1.528871391076114250, -0.6692913385826771977, 0.1292274648535927661 ) ) ;
#76069 = CARTESIAN_POINT ( 'NONE',  ( -1.003937007874015297, -0.5400638737290845981, -0.3530559997133363437 ) ) ;
#76070 = CARTESIAN_POINT ( 'NONE',  ( 0.7217847769028878924, -0.4281496062992127816, -0.4176697321401328100 ) ) ;
#76071 = CARTESIAN_POINT ( 'NONE',  ( 0.3917322834645669549, 0.1049643490035304660, -1.534120734908136052 ) ) ;
#76072 = CARTESIAN_POINT ( 'NONE',  ( -0.4396325459317577122, -0.5511811023622048555, -0.09757992244046775898 ) ) ;
#76073 = ORIENTED_EDGE ( 'NONE', *, *, #80383, .F. ) ;
#76074 = CARTESIAN_POINT ( 'NONE',  ( -0.2891555358219911054, 0.2891555358219909388, -1.594488188976378007 ) ) ;
#76075 = ORIENTED_EDGE ( 'NONE', *, *, #66367, .T. ) ;
#76076 = CARTESIAN_POINT ( 'NONE',  ( -1.391076115485563758, 0.1283753931104748280, 0.1820866141732283561 ) ) ;
#76077 = CARTESIAN_POINT ( 'NONE',  ( -1.161417322834644716, 0.1660481256975885056, 0.3530559997133364547 ) ) ;
#76078 = CARTESIAN_POINT ( 'NONE',  ( -0.8070866141732276899, 0.1660481256975883668, -0.3530559997133364547 ) ) ;
#76079 = CARTESIAN_POINT ( 'NONE',  ( 0.1998031496062992740, 0.3460692066303959757, -0.1443569553805774397 ) ) ;
#76080 = CARTESIAN_POINT ( 'NONE',  ( -1.154855643044618851, -0.6046776061558809534, -0.2411417322834644161 ) ) ;
#76081 = CARTESIAN_POINT ( 'NONE',  ( -0.8530183727034112984, -0.4281496062992127816, -0.4176697321401328100 ) ) ;
#76082 = CARTESIAN_POINT ( 'NONE',  ( -1.535433070866141225, -0.6692913385826771977, 8.415575281601705876E-17 ) ) ;
#76083 = FACE_OUTER_BOUND ( 'NONE', #37775, .T. ) ;
#76084 = CARTESIAN_POINT ( 'NONE',  ( 0.5774278215223104249, 0.1283753931104748280, 0.1820866141732283561 ) ) ;
#76085 = DIRECTION ( 'NONE',  ( -1.000000000000000000, 0.000000000000000000, 0.000000000000000000 ) ) ;
#76086 = CARTESIAN_POINT ( 'NONE',  ( 0.3392501089628018329, 0.1958661417322835607, 0.09908136482939623735 ) ) ;
#76087 = CARTESIAN_POINT ( 'NONE',  ( 0.01312335958005323398, -0.004921259842519576551, 0.3153832671262227771 ) ) ;
#76088 = CARTESIAN_POINT ( 'NONE',  ( -0.5249343832020990641, 0.2306618581243848609, 0.2411417322834645549 ) ) ;
#76089 = CARTESIAN_POINT ( 'NONE',  ( 1.450131233595801428, 0.2952755905511811885, 0.1292274648535926551 ) ) ;
#76090 = CARTESIAN_POINT ( 'NONE',  ( -0.02624671916010428221, 0.2306618581243847221, -0.2411417322834647770 ) ) ;
#76091 = ORIENTED_EDGE ( 'NONE', *, *, #17897, .T. ) ;
#76092 = CARTESIAN_POINT ( 'NONE',  ( -0.3996062992125986035, -7.340648628747425578E-17, -1.929133858267716439 ) ) ;
#76093 = DIRECTION ( 'NONE',  ( 0.000000000000000000, 0.000000000000000000, 1.000000000000000000 ) ) ;
#76094 = ORIENTED_EDGE ( 'NONE', *, *, #82940, .T. ) ;
#76095 = CARTESIAN_POINT ( 'NONE',  ( 0.3460692066303959202, -0.1998031496062991630, -1.756561679790026309 ) ) ;
#76096 = CARTESIAN_POINT ( 'NONE',  ( 1.115485564304462551, 0.05413385826771666132, 0.4176697321401328100 ) ) ;
#76097 = CARTESIAN_POINT ( 'NONE',  ( -1.135170603674539924, -0.5511811023622046335, 0.09757992244046803654 ) ) ;
#76098 = CARTESIAN_POINT ( 'NONE',  ( -1.318897637795274802, -0.5400638737290845981, -0.3530559997133363437 ) ) ;
#76099 = CARTESIAN_POINT ( 'NONE',  ( 0.4724409448818897572, -0.1265901696524988906, -0.8989501312335956840 ) ) ;
#76100 = DIRECTION ( 'NONE',  ( -3.491481338843132961E-15, -0.000000000000000000, 1.000000000000000000 ) ) ;
#76101 = CARTESIAN_POINT ( 'NONE',  ( 0.1049643490035303689, 0.3917322834645670104, -2.755249343832020248 ) ) ;
#76102 = CARTESIAN_POINT ( 'NONE',  ( 1.141732283464567788, -0.6692913385826771977, 8.415575281601705876E-17 ) ) ;
#76103 = CONICAL_SURFACE ( 'NONE', #881, 0.3129921259842520787, 0.7853981633974533860 ) ;
#76104 = CARTESIAN_POINT ( 'NONE',  ( 0.3917322834645670104, -0.1049643490035303273, -2.085958005249343827 ) ) ;
#76105 = CARTESIAN_POINT ( 'NONE',  ( 0.1509186351706045259, -0.05778040916215560624, -0.4822834645669293319 ) ) ;
#76106 = CARTESIAN_POINT ( 'NONE',  ( -1.108923884514435132, -0.08942795157528024563, -0.3641732283464568787 ) ) ;
#76107 = CIRCLE ( 'NONE', #23697, 0.3149606299212597826 ) ;
#76108 = CIRCLE ( 'NONE', #63949, 0.5118110236220472231 ) ;
#76109 = CARTESIAN_POINT ( 'NONE',  ( -0.5446194225721777693, -0.3162353388693409650, -0.4822834645669289433 ) ) ;
#76110 = CARTESIAN_POINT ( 'NONE',  ( 0.1998031496062994128, -0.3460692066303957537, 0.1463254593175852825 ) ) ;
#76111 = CARTESIAN_POINT ( 'NONE',  ( -1.082677165354329896, 0.1660481256975885056, 0.3530559997133364547 ) ) ;
#76112 = CARTESIAN_POINT ( 'NONE',  ( -0.2891555358219909388, -0.2891555358219912164, -2.183070866141731958 ) ) ;
#76113 = CARTESIAN_POINT ( 'NONE',  ( 1.115485564304462551, -0.004921259842519576551, 0.3153832671262227771 ) ) ;
#76114 = CARTESIAN_POINT ( 'NONE',  ( -0.1968503937007867743, -0.5511811023622047445, 6.969142054262312111E-17 ) ) ;
#76115 = CARTESIAN_POINT ( 'NONE',  ( 0.8595800524934390507, -0.2845877964562159024, 0.3641732283464567677 ) ) ;
#76116 = CARTESIAN_POINT ( 'NONE',  ( -1.410761154855642463, -0.05778040916215522460, 0.4822834645669289988 ) ) ;
#76117 = CARTESIAN_POINT ( 'NONE',  ( -0.4724409448818880364, -0.1265901696525023323, -2.169947506561679784 ) ) ;
#76118 = CARTESIAN_POINT ( 'NONE',  ( 0.6758530183727039509, -0.5511811023622046335, 0.09757992244046803654 ) ) ;
#76119 = CARTESIAN_POINT ( 'NONE',  ( -0.7939632545931750718, -0.05778040916215560624, -0.4822834645669293319 ) ) ;
#76120 = VECTOR ( 'NONE', #59216, 39.37007874015748143 ) ;
#76121 = CARTESIAN_POINT ( 'NONE',  ( 0.02624671916010564918, -0.5023911411419708095, -0.1820866141732282451 ) ) ;
#76122 = CARTESIAN_POINT ( 'NONE',  ( -1.607611548556429737, -0.5511811023622046335, 0.09757992244046803654 ) ) ;
#76123 = CARTESIAN_POINT ( 'NONE',  ( 0.8202099737532814183, -0.6692913385826773087, -0.1292274648535924053 ) ) ;
#76124 = CARTESIAN_POINT ( 'NONE',  ( 0.6561679790026253567, 0.2306618581243848609, 0.2411417322834645549 ) ) ;
#76125 = CARTESIAN_POINT ( 'NONE',  ( 1.351706036745407458, -0.3690944881889765550, -0.3153832671262227771 ) ) ;
#76126 = CARTESIAN_POINT ( 'NONE',  ( -1.391076115485563758, 0.2306618581243848609, 0.2411417322834645549 ) ) ;
#76127 = CARTESIAN_POINT ( 'NONE',  ( -0.2755905511811015396, -0.5511811023622047445, 6.969142054262312111E-17 ) ) ;
#76128 = CARTESIAN_POINT ( 'NONE',  ( 2.795275590551181910, 1.900312960331935086, 0.000000000000000000 ) ) ;
#76129 = CARTESIAN_POINT ( 'NONE',  ( 0.04593175853018440641, 0.1771653543307087075, -0.09757992244046823083 ) ) ;
#76130 = CARTESIAN_POINT ( 'NONE',  ( -1.358267716535432434, 0.1660481256975883668, -0.3530559997133364547 ) ) ;
#76131 = CARTESIAN_POINT ( 'NONE',  ( -0.5118110236220466680, 0.2952755905511811885, 0.000000000000000000 ) ) ;
#76132 = SHAPE_REPRESENTATION ( 'Spindle Dowel Pin', ( #22098 ), #75874 ) ;
#76133 = CARTESIAN_POINT ( 'NONE',  ( 0.3996062992125984925, 0.1070741851644054637, -0.5164041994750655507 ) ) ;
#76134 = EDGE_CURVE ( 'NONE', #6583, #50887, #47615, .T. ) ;
#76135 = CARTESIAN_POINT ( 'NONE',  ( 0.3917322834645670104, -0.1049643490035303411, -2.400918635170603554 ) ) ;
#76136 = CARTESIAN_POINT ( 'NONE',  ( 0.4265091863517067039, -0.5511811023622048555, -0.09757992244046775898 ) ) ;
#76137 = CARTESIAN_POINT ( 'NONE',  ( -0.5052493438320203589, 0.2952755905511810774, -0.1292274648535930714 ) ) ;
#76138 = CARTESIAN_POINT ( 'NONE',  ( -0.7480314960629914633, -0.6692913385826771977, 8.415575281601705876E-17 ) ) ;
#76139 = CARTESIAN_POINT ( 'NONE',  ( -0.9120734908136475250, -0.5511811023622048555, -0.09757992244046775898 ) ) ;
#76140 = CARTESIAN_POINT ( 'NONE',  ( -3.924565315667062126, 1.180549598472639961, -0.3129926727910089523 ) ) ;
#76141 = CARTESIAN_POINT ( 'NONE',  ( -0.2559055118110227234, -0.5400638737290844871, 0.3530559997133364547 ) ) ;
#76142 = CARTESIAN_POINT ( 'NONE',  ( -1.404199475065615932, -0.004921259842519576551, 0.3153832671262227771 ) ) ;
#76143 = CARTESIAN_POINT ( 'NONE',  ( 1.594488188976378673, 0.1660481256975885056, 0.3530559997133364547 ) ) ;
#76144 = CARTESIAN_POINT ( 'NONE',  ( -0.4724409448818898682, -8.678599364036362592E-17, -0.6692913385826770867 ) ) ;
#76145 = EDGE_CURVE ( 'NONE', #67389, #51195, #51448, .T. ) ;
#76146 = VERTEX_POINT ( 'NONE', #34098 ) ;
#76147 = CARTESIAN_POINT ( 'NONE',  ( 0.000000000000000000, 2.559055118110236560, 0.000000000000000000 ) ) ;
#76148 = CARTESIAN_POINT ( 'NONE',  ( -1.318897637795274802, -0.5400638737290845981, -0.3530559997133363437 ) ) ;
#76149 = CARTESIAN_POINT ( 'NONE',  ( -0.7874015748031489847, -0.1870078740157479769, 0.4822834645669291653 ) ) ;
#76150 = CARTESIAN_POINT ( 'NONE',  ( 1.601049868766404982, 0.2306618581243848609, 0.2411417322834645549 ) ) ;
#76151 = CARTESIAN_POINT ( 'NONE',  ( -0.2867679344610364334, -0.2867679344610367109, -1.875984251968503935 ) ) ;
#76152 = CARTESIAN_POINT ( 'NONE',  ( 0.02733964191757773388, 0.3913445824879502322, -1.220472440944881498 ) ) ;
#76153 = CARTESIAN_POINT ( 'NONE',  ( 0.9317585301837276734, 0.05413385826771626580, -0.4176697321401330321 ) ) ;
#76154 = CARTESIAN_POINT ( 'NONE',  ( 0.2296587926509192634, -0.3162353388693405765, 0.4822834645669290543 ) ) ;
#76155 = CARTESIAN_POINT ( 'NONE',  ( 0.4091458600556403535, 0.2362204724409449896, -0.4461942257217847430 ) ) ;
#76156 = AXIS2_PLACEMENT_3D ( 'NONE', #33369, #64932, #7270 ) ;
#76157 = VECTOR ( 'NONE', #29338, 39.37007874015748854 ) ;
#76159 = AXIS2_PLACEMENT_3D ( 'NONE', #33453, #1472, #65863 ) ;
#76158 = CARTESIAN_POINT ( 'NONE',  ( -0.01591673448991381273, 0.3996062992125985480, -2.754912411187758536 ) ) ;
#76160 = CARTESIAN_POINT ( 'NONE',  ( 1.391076115485564868, -0.5023911411419708095, 0.1820866141732285504 ) ) ;
#76161 = CARTESIAN_POINT ( 'NONE',  ( 0.1070741851644053527, 0.3996062992125986590, -1.095800524934382958 ) ) ;
#76162 = ORIENTED_EDGE ( 'NONE', *, *, #28583, .F. ) ;
#76163 = CARTESIAN_POINT ( 'NONE',  ( 0.1958661417322834775, 0.3392501089628018884, -2.813648293963254776 ) ) ;
#76164 = ORIENTED_EDGE ( 'NONE', *, *, #15715, .T. ) ;
#76165 = CARTESIAN_POINT ( 'NONE',  ( 0.5052493438320215802, 0.2952755905511811885, 0.1292274648535926551 ) ) ;
#76166 = CARTESIAN_POINT ( 'NONE',  ( -0.7742782152230965886, 0.05413385826771666132, 0.4176697321401328100 ) ) ;
#76167 = CARTESIAN_POINT ( 'NONE',  ( 1.614173228346457378, 0.2952755905511811885, 0.000000000000000000 ) ) ;
#76168 = CARTESIAN_POINT ( 'NONE',  ( 0.8070866141732289112, -0.5400638737290845981, -0.3530559997133363437 ) ) ;
#76169 = CARTESIAN_POINT ( 'NONE',  ( 1.476377952755906442, -0.5400638737290844871, 0.3530559997133364547 ) ) ;
#76170 = CARTESIAN_POINT ( 'NONE',  ( 1.246719160104987623, -0.4281496062992124485, 0.4176697321401328655 ) ) ;
#76171 = CARTESIAN_POINT ( 'NONE',  ( 0.03937007874015833325, -0.6692913385826771977, 8.415575281601705876E-17 ) ) ;
#76172 = CARTESIAN_POINT ( 'NONE',  ( -1.148293963254592542, 0.2952755905511811885, 0.1292274648535926551 ) ) ;
#76173 = DIRECTION ( 'NONE',  ( 0.7071067811865472397, -0.000000000000000000, 0.7071067811865476838 ) ) ;
#76174 = CARTESIAN_POINT ( 'NONE',  ( 1.686351706036745890, 0.2952755905511811885, 0.1292274648535926551 ) ) ;
#76175 = CARTESIAN_POINT ( 'NONE',  ( -0.1049643490035302024, -0.3917322834645671215, -0.2217847769028870319 ) ) ;
#76176 = CARTESIAN_POINT ( 'NONE',  ( 1.036745406824147731, -0.004921259842519576551, 0.3153832671262227771 ) ) ;
#76177 = EDGE_LOOP ( 'NONE', ( #58761, #20593, #25072, #61803 ) ) ;
#76178 = CARTESIAN_POINT ( 'NONE',  ( 0.1058382717557499880, 0.3949938075777411073, 0.006561679790026190250 ) ) ;
#76179 = EDGE_LOOP ( 'NONE', ( #43314, #45407, #5765, #77503 ) ) ;
#76180 = CARTESIAN_POINT ( 'NONE',  ( -0.05905511811023545637, -0.4536011799217368745, -0.2665933059059886201 ) ) ;
#76181 = CARTESIAN_POINT ( 'NONE',  ( 2.571327113428977018, 1.453547212638085950, -0.4672029448317638889 ) ) ;
#76182 = CARTESIAN_POINT ( 'NONE',  ( 0.4593175853018379162, -0.4281496062992124485, 0.4176697321401328655 ) ) ;
#76183 = CARTESIAN_POINT ( 'NONE',  ( 0.2296587926509192634, -0.05778040916215560624, -0.4822834645669293319 ) ) ;
#76184 = CARTESIAN_POINT ( 'NONE',  ( -0.5380577427821514602, -0.4281496062992127816, -0.4176697321401328100 ) ) ;
#76185 = CARTESIAN_POINT ( 'NONE',  ( -0.1958661417322836995, 0.3392501089628017219, -1.742145300033807631 ) ) ;
#76186 = CARTESIAN_POINT ( 'NONE',  ( -1.102362204724408601, -0.1870078740157480879, -0.4822834645669291653 ) ) ;
#76187 = CARTESIAN_POINT ( 'NONE',  ( -9.594673741351313045E-17, 0.3917322834645670104, -2.604330708661416693 ) ) ;
#76188 = CARTESIAN_POINT ( 'NONE',  ( 1.135170603674541256, 0.1771653543307087630, 0.09757992244046791164 ) ) ;
#76189 = CARTESIAN_POINT ( 'NONE',  ( -1.568241469816272105, -0.3162353388693409650, -0.4822834645669289433 ) ) ;
#76190 = CARTESIAN_POINT ( 'NONE',  ( 0.7808398950131241190, -0.05778040916215560624, -0.4822834645669293319 ) ) ;
#76191 = CARTESIAN_POINT ( 'NONE',  ( 1.272965879265092637, -0.4281496062992127816, -0.4176697321401328100 ) ) ;
#76192 = CARTESIAN_POINT ( 'NONE',  ( -0.2925321140481932924, 0.2925321140481931814, -0.6496062992125984925 ) ) ;
#76193 = CARTESIAN_POINT ( 'NONE',  ( -1.364829396325458521, 0.2306618581243847221, -0.2411417322834647770 ) ) ;
#76194 = CARTESIAN_POINT ( 'NONE',  ( 0.2925321140481932369, 0.2925321140481932369, -0.2145669291338583029 ) ) ;
#76195 = CARTESIAN_POINT ( 'NONE',  ( 0.02624671916010564918, 0.2306618581243848609, 0.2411417322834645549 ) ) ;
#76196 = CARTESIAN_POINT ( 'NONE',  ( 0.3996062992125986035, 0.1070741851644054776, -2.486876640419947382 ) ) ;
#76197 = CARTESIAN_POINT ( 'NONE',  ( -0.3917322834645669549, -0.1049643490035306603, -1.862860892388451761 ) ) ;
#76198 = B_SPLINE_CURVE_WITH_KNOTS ( 'NONE', 3,
 ( #10775, #16686, #43557, #4040 ),
 .UNSPECIFIED., .F., .F.,
 ( 4, 4 ),
 ( 0.1183700917297995092, 0.1198164042326150397 ),
 .UNSPECIFIED. ) ;
#76199 = CARTESIAN_POINT ( 'NONE',  ( 1.272965879265092637, -0.4281496062992127816, -0.4176697321401328100 ) ) ;
#76200 = CARTESIAN_POINT ( 'NONE',  ( 0.04593175853018440641, -0.5511811023622046335, 0.09757992244046803654 ) ) ;
#76201 = CARTESIAN_POINT ( 'NONE',  ( 0.7414698162729663755, -0.6692913385826773087, -0.1292274648535924053 ) ) ;
#76202 = CARTESIAN_POINT ( 'NONE',  ( -0.4091458600556405756, 0.2362204724409446288, -1.677821522309711266 ) ) ;
#76203 = CARTESIAN_POINT ( 'NONE',  ( 0.1706036745406830368, -0.3690944881889765550, -0.3153832671262227771 ) ) ;
#76204 = CARTESIAN_POINT ( 'NONE',  ( 0.4527559055118117182, -0.5400638737290844871, 0.3530559997133364547 ) ) ;
#76205 = CARTESIAN_POINT ( 'NONE',  ( -0.1058382717557497660, -0.3949938075777411073, -0.7788713910761156933 ) ) ;
#76206 = EDGE_CURVE ( 'NONE', #27710, #39595, #61422, .T. ) ;
#76207 = CARTESIAN_POINT ( 'NONE',  ( -0.7742782152230965886, 0.05413385826771666132, 0.4176697321401328100 ) ) ;
#76208 = CARTESIAN_POINT ( 'NONE',  ( -0.4724409448818888135, -0.1265901696525008335, -1.067585301837270517 ) ) ;
#76209 = CARTESIAN_POINT ( 'NONE',  ( 0.7480314960629927956, -0.5511811023622047445, 6.969142054262312111E-17 ) ) ;
#76210 = CARTESIAN_POINT ( 'NONE',  ( 0.1450607720586929161, 2.784432375088962958E-17, -0.3464511005275205946 ) ) ;
#76211 = CARTESIAN_POINT ( 'NONE',  ( -0.2690288713910754526, 0.2952755905511810774, -0.1292274648535930714 ) ) ;
#76212 = CARTESIAN_POINT ( 'NONE',  ( 0.2887139107611556010, 0.1283753931104746893, -0.1820866141732285504 ) ) ;
#76213 = CARTESIAN_POINT ( 'NONE',  ( -2.666386537446475913, 1.301102360844756722, 0.4123394245947728520 ) ) ;
#76214 = CARTESIAN_POINT ( 'NONE',  ( -0.1443569553805768291, 0.05413385826771666132, 0.4176697321401328100 ) ) ;
#76215 = CARTESIAN_POINT ( 'NONE',  ( 0.3412073490813655186, 0.1283753931104748280, 0.1820866141732283561 ) ) ;
#76216 = CIRCLE ( 'NONE', #3643, 1.122047244094488194 ) ;
#76217 = CARTESIAN_POINT ( 'NONE',  ( -0.1070741851644051862, -0.3996062992125986590, -1.881233595800524849 ) ) ;
#76218 = CARTESIAN_POINT ( 'NONE',  ( 0.3608923884514443348, -0.6692913385826771977, 0.1292274648535927661 ) ) ;
#76219 =( BOUNDED_CURVE ( )  B_SPLINE_CURVE ( 2, ( #20498, #57526, #39004, #7452, #1150, #27216, #12934, #46152, #52878, #64271, #45312, #51616, #77746 ),
 .UNSPECIFIED., .F., .F. ) 
 B_SPLINE_CURVE_WITH_KNOTS ( ( 3, 2, 2, 2, 2, 2, 3 ),
 ( 0.7187856400893463116, 0.7196969696969697239, 0.7234848484848485084, 0.7272727272727272929, 0.7310606060606060774, 0.7348484848484848619, 0.7357598144561083853 ),
 .UNSPECIFIED. ) 
 CURVE ( )  GEOMETRIC_REPRESENTATION_ITEM ( )  RATIONAL_B_SPLINE_CURVE ( ( 0.9875488213027523443, 0.9918020599134680371, 1.000000000000000000, 0.9659258262890683122, 1.000000000000000000, 0.9659258262890683122, 1.000000000000000000, 0.9659258262890683122, 1.000000000000000000, 0.9659258262890683122, 1.000000000000000000, 0.9918020599134671489, 0.9875488213027514561 ) ) 
 REPRESENTATION_ITEM ( '' )  );
#76220 = AXIS2_PLACEMENT_3D ( 'NONE', #54781, #48050, #73751 ) ;
#76221 = AXIS2_PLACEMENT_3D ( 'NONE', #63234, #69959, #31240 ) ;
#76222 = VECTOR ( 'NONE', #37631, 39.37007874015748143 ) ;
#76223 = CARTESIAN_POINT ( 'NONE',  ( 0.9908136482939640111, -0.5511811023622046335, 0.09757992244046803654 ) ) ;
#76224 = CARTESIAN_POINT ( 'NONE',  ( -0.4199475065616791736, 0.1283753931104746893, -0.1820866141732285504 ) ) ;
#76225 = CARTESIAN_POINT ( 'NONE',  ( -0.5511811023622041894, -0.1870078740157480601, -0.3641732283464567677 ) ) ;
#76226 = CARTESIAN_POINT ( 'NONE',  ( -0.4724409448818890911, -0.1870078740157480879, -0.4822834645669291653 ) ) ;
#76227 = CARTESIAN_POINT ( 'NONE',  ( 0.3083989501312343062, -0.3162353388693405765, 0.4822834645669290543 ) ) ;
#76228 = CARTESIAN_POINT ( 'NONE',  ( 1.167979002624672580, -0.3690944881889763329, 0.3153832671262228327 ) ) ;
#76229 = CARTESIAN_POINT ( 'NONE',  ( -1.607611548556429737, -0.5511811023622046335, 0.09757992244046803654 ) ) ;
#76230 = CARTESIAN_POINT ( 'NONE',  ( 1.410761154855643795, -0.2845877964562159024, 0.3641732283464567677 ) ) ;
#76231 = CARTESIAN_POINT ( 'NONE',  ( 0.9120734908136490793, 0.2952755905511810774, -0.1292274648535930714 ) ) ;
#76232 = FACE_OUTER_BOUND ( 'NONE', #25191, .T. ) ;
#76233 = CARTESIAN_POINT ( 'NONE',  ( -0.1443569553805768291, 0.05413385826771666132, 0.4176697321401328100 ) ) ;
#76234 = CARTESIAN_POINT ( 'NONE',  ( 0.1049643490035304938, -0.3917322834645669549, -0.9573490813648293241 ) ) ;
#76235 = CARTESIAN_POINT ( 'NONE',  ( 0.7020997375328090762, -0.3162353388693405765, 0.4822834645669290543 ) ) ;
#76236 = CARTESIAN_POINT ( 'NONE',  ( 0.6364829396325465405, -0.3162353388693409650, -0.4822834645669289433 ) ) ;
#76237 = FACE_OUTER_BOUND ( 'NONE', #29398, .T. ) ;
#76238 = CARTESIAN_POINT ( 'NONE',  ( 0.3280839895013130669, -0.3690944881889765550, -0.3153832671262227771 ) ) ;
#76239 = CARTESIAN_POINT ( 'NONE',  ( 1.043307086614173818, 0.1660481256975885056, 0.3530559997133364547 ) ) ;
#76240 = CARTESIAN_POINT ( 'NONE',  ( -0.3674540682414692561, -0.5023911411419708095, -0.1820866141732282451 ) ) ;
#76241 = CARTESIAN_POINT ( 'NONE',  ( -0.4986876640419939388, 0.2306618581243847221, -0.2411417322834647770 ) ) ;
#76242 = LINE ( 'NONE', #64430, #20623 ) ;
#76243 = CARTESIAN_POINT ( 'NONE',  ( 0.2296587926509192634, -0.05778040916215560624, -0.4822834645669293319 ) ) ;
#76244 = CARTESIAN_POINT ( 'NONE',  ( -0.6692913385826764205, 0.2952755905511811885, 0.000000000000000000 ) ) ;
#76245 = CARTESIAN_POINT ( 'NONE',  ( -0.5511811023622041894, -0.1870078740157480601, -0.3641732283464567677 ) ) ;
#76246 = CARTESIAN_POINT ( 'NONE',  ( 0.4658792650918640033, -0.3162353388693405765, 0.4822834645669290543 ) ) ;
#76247 = CARTESIAN_POINT ( 'NONE',  ( -1.259842519685038686, -0.1870078740157479769, 0.4822834645669291653 ) ) ;
#76248 = CARTESIAN_POINT ( 'NONE',  ( -0.5249343832020990641, 0.2306618581243848609, 0.2411417322834645549 ) ) ;
#76249 = CARTESIAN_POINT ( 'NONE',  ( -0.4709442531824371558, -0.03757601356356778805, -1.220472440944882164 ) ) ;
#76251 = CARTESIAN_POINT ( 'NONE',  ( 1.332020997375328974, -0.05778040916215560624, -0.4822834645669293319 ) ) ;
#76250 = CARTESIAN_POINT ( 'NONE',  ( -0.9348729704079935532, -2.191421614605370878E-15, 0.4445507791589071167 ) ) ;
#76252 = CARTESIAN_POINT ( 'NONE',  ( 1.522309711286089939, 0.2306618581243848609, 0.2411417322834645549 ) ) ;
#76253 = CARTESIAN_POINT ( 'NONE',  ( 0.3917322834645670104, 2.398668435337828261E-17, -2.000000000000000000 ) ) ;
#76254 = CARTESIAN_POINT ( 'NONE',  ( -1.450131233595799651, 0.2952755905511810774, -0.1292274648535930714 ) ) ;
#76255 = CARTESIAN_POINT ( 'NONE',  ( -0.8267716535433065062, -0.6692913385826771977, 8.415575281601705876E-17 ) ) ;
#76256 = CARTESIAN_POINT ( 'NONE',  ( 0.2362204724409449064, 0.4091458600556404646, -0.1443569553805774397 ) ) ;
#76257 = CARTESIAN_POINT ( 'NONE',  ( -0.3949938075777411628, 0.1058382717557497937, -2.709973753280840114 ) ) ;
#76258 = ORIENTED_EDGE ( 'NONE', *, *, #8336, .F. ) ;
#76259 = CARTESIAN_POINT ( 'NONE',  ( 0.1574803149606306130, -0.1870078740157480601, -0.3641732283464567677 ) ) ;
#76260 = CARTESIAN_POINT ( 'NONE',  ( -0.3917322834645671215, 0.1049643490035301469, -1.442257217847769057 ) ) ;
#76261 = CARTESIAN_POINT ( 'NONE',  ( 0.5446194225721792126, -0.05778040916215560624, -0.4822834645669293319 ) ) ;
#76262 = CARTESIAN_POINT ( 'NONE',  ( -0.3458507752293906723, -0.3458507752293910609, -2.736220472440944018 ) ) ;
#76263 = CARTESIAN_POINT ( 'NONE',  ( 4.821444091131311894E-16, 2.755905511811024056, 3.937007874015748143 ) ) ;
#76264 = CARTESIAN_POINT ( 'NONE',  ( -0.6299212598425188991, -0.1870078740157480601, -0.3641732283464567677 ) ) ;
#76265 = CARTESIAN_POINT ( 'NONE',  ( -0.2493438320209966919, 0.05413385826771626580, -0.4176697321401330321 ) ) ;
#76266 = CARTESIAN_POINT ( 'NONE',  ( 1.128608923884515169, -0.6046776061558809534, -0.2411417322834644161 ) ) ;
#76267 = ADVANCED_FACE ( 'NONE', ( #3772 ), #67757, .F. ) ;
#76268 = CARTESIAN_POINT ( 'NONE',  ( 1.095800524934383846, -0.2845877964562159024, 0.3641732283464567677 ) ) ;
#76269 = CARTESIAN_POINT ( 'NONE',  ( -0.1640419947506553400, -0.05778040916215560624, -0.4822834645669293319 ) ) ;
#76270 = CARTESIAN_POINT ( 'NONE',  ( -0.3917322834645668994, -0.1049643490035306742, -0.9133665109898146950 ) ) ;
#76271 = CARTESIAN_POINT ( 'NONE',  ( -0.6102362204724400829, -0.5400638737290845981, -0.3530559997133363437 ) ) ;
#76272 = CARTESIAN_POINT ( 'NONE',  ( -1.364829396325458521, 0.1283753931104746893, -0.1820866141732285504 ) ) ;
#76274 = EDGE_CURVE ( 'NONE', #23151, #59949, #30397, .T. ) ;
#76273 = CARTESIAN_POINT ( 'NONE',  ( -0.2755905511811018171, 0.2952755905511811885, 0.000000000000000000 ) ) ;
#76275 = DIRECTION ( 'NONE',  ( 0.000000000000000000, 0.000000000000000000, -1.000000000000000000 ) ) ;
#76276 = AXIS2_PLACEMENT_3D ( 'NONE', #31282, #70000, #37601 ) ;
#76277 = CARTESIAN_POINT ( 'NONE',  ( -0.4724409448818898682, -8.678599364036362592E-17, -1.141732283464566899 ) ) ;
#76278 = ORIENTED_EDGE ( 'NONE', *, *, #41310, .F. ) ;
#76279 = CARTESIAN_POINT ( 'NONE',  ( 4.797336870675656522E-17, -0.3917322834645670659, -1.965242412894699919 ) ) ;
#76280 = CARTESIAN_POINT ( 'NONE',  ( 0.3280839895013130669, -0.4281496062992127816, -0.4176697321401328100 ) ) ;
#76281 = ORIENTED_EDGE ( 'NONE', *, *, #39057, .F. ) ;
#76282 = AXIS2_PLACEMENT_3D ( 'NONE', #47447, #3679, #54593 ) ;
#76283 = CARTESIAN_POINT ( 'NONE',  ( -0.9317585301837263412, 0.05413385826771666132, 0.4176697321401328100 ) ) ;
#76284 = CARTESIAN_POINT ( 'NONE',  ( -1.456692913385826182, 0.2952755905511811885, 0.000000000000000000 ) ) ;
#76285 = CARTESIAN_POINT ( 'NONE',  ( 0.5577427821522314977, -0.3162353388693409650, -0.4822834645669289433 ) ) ;
#76286 = CARTESIAN_POINT ( 'NONE',  ( -0.01312335958005186876, 0.05413385826771626580, -0.4176697321401330321 ) ) ;
#76287 = CARTESIAN_POINT ( 'NONE',  ( -0.3917322834645669549, -0.1049643490035306603, -1.547900262467191590 ) ) ;
#76288 = CARTESIAN_POINT ( 'NONE',  ( -0.8333333333333323711, -0.6692913385826773087, -0.1292274648535924053 ) ) ;
#76289 = CARTESIAN_POINT ( 'NONE',  ( -0.2559055118110227234, -0.5400638737290844871, 0.3530559997133364547 ) ) ;
#76290 = CARTESIAN_POINT ( 'NONE',  ( -1.010498687664041384, 0.05413385826771666132, 0.4176697321401328100 ) ) ;
#76291 = CARTESIAN_POINT ( 'NONE',  ( 0.4790026246719168435, -0.2845877964562161244, -0.3641732283464567121 ) ) ;
#76292 = CARTESIAN_POINT ( 'NONE',  ( -0.0008564280371856086574, 0.3986795681651738033, 7.618016766297077184E-18 ) ) ;
#76293 = CARTESIAN_POINT ( 'NONE',  ( 0.09842519685039434474, -0.5400638737290845981, -0.3530559997133363437 ) ) ;
#76294 = CARTESIAN_POINT ( 'NONE',  ( 0.2460629921259843422, 1.506701278478534659E-17, -0.1181102362204724116 ) ) ;
#76295 = EDGE_CURVE ( 'NONE', #22229, #23692, #40413, .T. ) ;
#76296 = CARTESIAN_POINT ( 'NONE',  ( 1.108923884514436242, -0.05778040916215522460, 0.4822834645669289988 ) ) ;
#76297 = CARTESIAN_POINT ( 'NONE',  ( 0.1049643490035303689, 0.3917322834645670104, -2.662729658792650778 ) ) ;
#76298 = ORIENTED_EDGE ( 'NONE', *, *, #26365, .F. ) ;
#76299 = EDGE_CURVE ( 'NONE', #71856, #59949, #47219, .T. ) ;
#76300 = EDGE_LOOP ( 'NONE', ( #64364, #35148, #50872, #8806 ) ) ;
#76301 = CARTESIAN_POINT ( 'NONE',  ( 0.2230971128608932319, -0.4281496062992124485, 0.4176697321401328655 ) ) ;
#76302 = CARTESIAN_POINT ( 'NONE',  ( -0.07874015748031421014, -0.1870078740157480601, -0.3641732283464567677 ) ) ;
#76304 = CARTESIAN_POINT ( 'NONE',  ( 0.5314960629921325896, 2.755905511811024056, -1.895394334970790018 ) ) ;
#76303 = CARTESIAN_POINT ( 'NONE',  ( 1.548556430446194954, 0.1283753931104746893, -0.1820866141732285504 ) ) ;
#76305 = CARTESIAN_POINT ( 'NONE',  ( 4.797336870675656522E-17, -0.3917322834645670104, -1.108267716535433101 ) ) ;
#76306 = CARTESIAN_POINT ( 'NONE',  ( -0.4091458600556402980, -0.2362204724409451284, 0.02821522309711285356 ) ) ;
#76307 = CARTESIAN_POINT ( 'NONE',  ( -0.1070741851644051862, -0.3996062992125986590, -2.668635170603674833 ) ) ;
#76308 = CARTESIAN_POINT ( 'NONE',  ( 0.6102362204724416372, -0.5400638737290844871, 0.3530559997133364547 ) ) ;
#76309 = CARTESIAN_POINT ( 'NONE',  ( -1.240157480314959759, -0.5400638737290845981, -0.3530559997133363437 ) ) ;
#76310 = CARTESIAN_POINT ( 'NONE',  ( -0.9842519685039365918, -0.6692913385826771977, 8.415575281601705876E-17 ) ) ;
#76311 = CARTESIAN_POINT ( 'NONE',  ( 0.4265091863517067039, -0.6692913385826773087, -0.1292274648535924053 ) ) ;
#76312 = CARTESIAN_POINT ( 'NONE',  ( 0.8070866141732288002, 0.1660481256975885056, 0.3530559997133364547 ) ) ;
#76313 = CARTESIAN_POINT ( 'NONE',  ( 1.364829396325460076, 0.1283753931104748280, 0.1820866141732283561 ) ) ;
#76314 = CONTEXT_DEPENDENT_SHAPE_REPRESENTATION ( #71304, #960 ) ;
#76315 = CARTESIAN_POINT ( 'NONE',  ( 0.9120734908136490793, 0.1771653543307087075, -0.09757992244046823083 ) ) ;
#76316 = CARTESIAN_POINT ( 'NONE',  ( -0.8136482939632537770, 0.2306618581243847221, -0.2411417322834647770 ) ) ;
#76317 = CARTESIAN_POINT ( 'NONE',  ( 0.3996062992125986035, -0.1070741851644052972, -0.6607611548556431291 ) ) ;
#76318 = CARTESIAN_POINT ( 'NONE',  ( 1.679790026246720025, 0.2306618581243848609, 0.2411417322834645549 ) ) ;
#76319 = CARTESIAN_POINT ( 'NONE',  ( 0.3917322834645670104, 2.398668435337828261E-17, -0.2677165354330708347 ) ) ;
#76321 = CARTESIAN_POINT ( 'NONE',  ( 1.595398199321655275, 0.7585570207896586981, -0.1559797534342493852 ) ) ;
#76320 = CARTESIAN_POINT ( 'NONE',  ( 1.286089238845145033, -0.6046776061558809534, -0.2411417322834644161 ) ) ;
#76322 = CARTESIAN_POINT ( 'NONE',  ( -1.535433070866141225, 0.1771653543307087630, 0.000000000000000000 ) ) ;
#76323 = CARTESIAN_POINT ( 'NONE',  ( -0.02624671916010428221, 0.2306618581243847221, -0.2411417322834647770 ) ) ;
#76324 = CARTESIAN_POINT ( 'NONE',  ( 0.6889763779527563470, 0.07958543189024071263, -0.2665933059059888421 ) ) ;
#76325 = CARTESIAN_POINT ( 'NONE',  ( -1.712598425196849572, 0.07958543189024085140, 0.2665933059059887866 ) ) ;
#76326 = CARTESIAN_POINT ( 'NONE',  ( 0.9383202099737538715, -0.05778040916215560624, -0.4822834645669293319 ) ) ;
#76327 = CARTESIAN_POINT ( 'NONE',  ( -0.3149606299212459048, 2.559055118110236560, -3.937007874015763242 ) ) ;
#76328 = CARTESIAN_POINT ( 'NONE',  ( -0.4790026246719154557, -0.2845877964562159024, 0.3641732283464567677 ) ) ;
#76329 = CARTESIAN_POINT ( 'NONE',  ( -0.4461942257217840213, 0.2306618581243848609, 0.2411417322834645549 ) ) ;
#76330 = CARTESIAN_POINT ( 'NONE',  ( 1.391076115485564868, 0.2306618581243847221, -0.2411417322834647770 ) ) ;
#76331 = CARTESIAN_POINT ( 'NONE',  ( -0.9776902887139098386, -0.6692913385826771977, 0.1292274648535927661 ) ) ;
#76332 = CARTESIAN_POINT ( 'NONE',  ( 1.259842519685040019, -0.1870078740157480879, -0.4822834645669291653 ) ) ;
#76333 = CARTESIAN_POINT ( 'NONE',  ( 0.3392501089628018884, -0.1958661417322833942, -1.046607242291025752 ) ) ;
#76334 = CARTESIAN_POINT ( 'NONE',  ( -1.318897637795274802, 0.07958543189024085140, 0.2665933059059887866 ) ) ;
#76335 = CARTESIAN_POINT ( 'NONE',  ( -0.7426113562969628434, 2.209901789876557832, 0.5309055118110236338 ) ) ;
#76336 = CARTESIAN_POINT ( 'NONE',  ( 0.9908136482939640111, 0.2952755905511810774, -0.1292274648535930714 ) ) ;
#76337 = CARTESIAN_POINT ( 'NONE',  ( -0.2362204724409451284, 0.4091458600556402425, -2.452099737532808188 ) ) ;
#76338 = CARTESIAN_POINT ( 'NONE',  ( -1.679790026246718693, 0.2306618581243847221, -0.2411417322834647770 ) ) ;
#76339 = CARTESIAN_POINT ( 'NONE',  ( -1.377952755905511140, -0.5511811023622047445, 6.969142054262312111E-17 ) ) ;
#76340 = CARTESIAN_POINT ( 'NONE',  ( -0.8530183727034112984, -0.3690944881889765550, -0.3153832671262227771 ) ) ;
#76341 = CARTESIAN_POINT ( 'NONE',  ( 1.437007874015748810, -0.4536011799217368745, -0.2665933059059886201 ) ) ;
#76342 = CARTESIAN_POINT ( 'NONE',  ( -0.4133858267716528645, -0.5400638737290844871, 0.3530559997133364547 ) ) ;
#76343 = CARTESIAN_POINT ( 'NONE',  ( -0.1181102362204717315, -0.5511811023622047445, 6.969142054262312111E-17 ) ) ;
#76344 = CARTESIAN_POINT ( 'NONE',  ( -1.509186351706035767, -0.004921259842519870586, -0.3153832671262229437 ) ) ;
#76345 = CARTESIAN_POINT ( 'NONE',  ( 1.062992125984252745, -0.5511811023622047445, 6.969142054262312111E-17 ) ) ;
#76346 = CARTESIAN_POINT ( 'NONE',  ( 0.8858267716535438430, 0.1660481256975885056, 0.3530559997133364547 ) ) ;
#76347 = DIRECTION ( 'NONE',  ( 1.047444401652940007E-14, -0.000000000000000000, -1.000000000000000000 ) ) ;
#76348 = CARTESIAN_POINT ( 'NONE',  ( -0.07217847769028787330, -0.08942795157527998196, 0.3641732283464567121 ) ) ;
#76349 = CARTESIAN_POINT ( 'NONE',  ( 0.3740157480314966754, -0.5400638737290844871, 0.3530559997133364547 ) ) ;
#76350 = CARTESIAN_POINT ( 'NONE',  ( 0.4068241469816279987, -0.3690944881889765550, -0.3153832671262227771 ) ) ;
#76351 = ORIENTED_EDGE ( 'NONE', *, *, #50027, .T. ) ;
#76352 = CARTESIAN_POINT ( 'NONE',  ( -1.528871391076114250, -0.6692913385826771977, 0.1292274648535927661 ) ) ;
#76353 = ADVANCED_FACE ( 'NONE', ( #42062 ), #35346, .T. ) ;
#76354 = CARTESIAN_POINT ( 'NONE',  ( -1.108923884514435132, -0.05778040916215560624, -0.4822834645669293319 ) ) ;
#76355 = CARTESIAN_POINT ( 'NONE',  ( 0.09186351706036799403, -0.4281496062992127816, -0.4176697321401328100 ) ) ;
#76356 = CARTESIAN_POINT ( 'NONE',  ( 0.3996062992125986035, -0.1070741851644053111, -0.4265091863517060378 ) ) ;
#76357 = CARTESIAN_POINT ( 'NONE',  ( 0.1070741851644053388, 0.3996062992125986035, -2.747375328083988766 ) ) ;
#76358 = CARTESIAN_POINT ( 'NONE',  ( 0.5118110236220478892, 0.2952755905511811885, 0.000000000000000000 ) ) ;
#76359 = CARTESIAN_POINT ( 'NONE',  ( 1.305774278215223960, 0.1771653543307087075, -0.09757992244046823083 ) ) ;
#76360 = CARTESIAN_POINT ( 'NONE',  ( -0.1968503937007867743, 0.2952755905511811885, 0.000000000000000000 ) ) ;
#76361 = CARTESIAN_POINT ( 'NONE',  ( 0.1968503937007881344, 0.2952755905511811885, 0.000000000000000000 ) ) ;
#76362 = CARTESIAN_POINT ( 'NONE',  ( -0.3996062992125986035, -7.340648628747425578E-17, -2.244094488188976388 ) ) ;
#76363 = CARTESIAN_POINT ( 'NONE',  ( -9.674558042662121740E-17, 0.3949938075777409963, -1.417322834645669216 ) ) ;
#76364 = CARTESIAN_POINT ( 'NONE',  ( -0.1973832605630230219, 1.105719693649961810, 1.104646637927854336 ) ) ;
#76365 = CARTESIAN_POINT ( 'NONE',  ( -1.827151725772330648, 2.742788129994044866, -0.5314960629921260393 ) ) ;
#76366 = CARTESIAN_POINT ( 'NONE',  ( -0.1958661417322834220, -0.3392501089628018884, -0.6876640419947506189 ) ) ;
#76367 = CARTESIAN_POINT ( 'NONE',  ( -0.7152230971128602510, -0.08942795157528024563, -0.3641732283464568787 ) ) ;
#76368 = CARTESIAN_POINT ( 'NONE',  ( -1.023622047244094002, -0.1870078740157480879, -0.4822834645669291653 ) ) ;
#76369 = CARTESIAN_POINT ( 'NONE',  ( 0.3420746716998660508, -0.1974969037888704149, -2.386482939632546429 ) ) ;
#76370 = CARTESIAN_POINT ( 'NONE',  ( 0.6758530183727039509, -0.6692913385826771977, 0.1292274648535927661 ) ) ;
#76371 = CARTESIAN_POINT ( 'NONE',  ( -1.620734908136482577, 0.2952755905511811885, 0.1292274648535926551 ) ) ;
#76372 = CARTESIAN_POINT ( 'NONE',  ( 0.5905511811023629321, -0.6692913385826771977, 8.415575281601705876E-17 ) ) ;
#76373 = CARTESIAN_POINT ( 'NONE',  ( -0.6199123404867337150, -2.191421614605370878E-15, 0.4445507791589071167 ) ) ;
#76374 = CARTESIAN_POINT ( 'NONE',  ( 0.1070741851644054915, -0.3996062992125986035, -1.975065616797900381 ) ) ;
#76375 = CARTESIAN_POINT ( 'NONE',  ( 1.679790026246720025, 0.2306618581243848609, 0.2411417322834645549 ) ) ;
#76376 = CARTESIAN_POINT ( 'NONE',  ( 0.9908136482939640111, 0.2952755905511810774, -0.1292274648535930714 ) ) ;
#76377 = CARTESIAN_POINT ( 'NONE',  ( 0.5577427821522314977, -0.3162353388693409650, -0.4822834645669289433 ) ) ;
#76378 = CARTESIAN_POINT ( 'NONE',  ( 0.7677165354330716118, -0.4536011799217367080, 0.2665933059059888421 ) ) ;
#76379 = CARTESIAN_POINT ( 'NONE',  ( 1.305774278215223960, -0.6692913385826771977, 0.1292274648535927661 ) ) ;
#76380 = CARTESIAN_POINT ( 'NONE',  ( 0.1958661417322834775, 0.3392501089628018884, -0.2290026246719160941 ) ) ;
#76381 = CARTESIAN_POINT ( 'NONE',  ( -1.595398199321655275, 2.115458727241839476, 0.1559797534342494407 ) ) ;
#76382 = CARTESIAN_POINT ( 'NONE',  ( 0.6692913385826778638, -0.6692913385826771977, 8.415575281601705876E-17 ) ) ;
#76383 = CARTESIAN_POINT ( 'NONE',  ( 1.423884514435696413, -0.2845877964562161244, -0.3641732283464567121 ) ) ;
#76384 = CARTESIAN_POINT ( 'NONE',  ( -0.8530183727034112984, -0.4281496062992127816, -0.4176697321401328100 ) ) ;
#76385 = CARTESIAN_POINT ( 'NONE',  ( -1.141732283464566011, -0.6692913385826771977, 8.415575281601705876E-17 ) ) ;
#76386 = CARTESIAN_POINT ( 'NONE',  ( 1.299212598425197429, 0.2952755905511811885, 0.000000000000000000 ) ) ;
#76387 = CARTESIAN_POINT ( 'NONE',  ( -0.3917322834645669549, -0.1049643490035306603, -0.4455380577427821565 ) ) ;
#76388 = CARTESIAN_POINT ( 'NONE',  ( -0.2867679344610364334, -0.2867679344610367109, -1.468503937007874294 ) ) ;
#76389 = CARTESIAN_POINT ( 'NONE',  ( -0.3392501089628019995, 0.1958661417322832277, -2.695538057742782101 ) ) ;
#76390 = ORIENTED_EDGE ( 'NONE', *, *, #25562, .F. ) ;
#76391 = CARTESIAN_POINT ( 'NONE',  ( -0.3996062992125986035, -7.340648628747425578E-17, 0.1181102362204724254 ) ) ;
#76392 = ORIENTED_EDGE ( 'NONE', *, *, #9399, .T. ) ;
#76393 = CARTESIAN_POINT ( 'NONE',  ( 1.620734908136483465, -0.6692913385826771977, 0.1292274648535927661 ) ) ;
#76394 = AXIS2_PLACEMENT_3D ( 'NONE', #14257, #39915, #65604 ) ;
#76395 = CARTESIAN_POINT ( 'NONE',  ( 1.384514435695538337, -0.5511811023622046335, 0.09757992244046803654 ) ) ;
#76396 = CARTESIAN_POINT ( 'NONE',  ( 0.3460692066303959757, -0.1998031496062991907, -1.364829396325459188 ) ) ;
#76397 = CARTESIAN_POINT ( 'NONE',  ( 1.292650918635171564, -0.5511811023622048555, -0.09757992244046775898 ) ) ;
#76398 = CARTESIAN_POINT ( 'NONE',  ( -0.3996062992125986035, -1.273259842764937629E-12, -1.929133858267794599 ) ) ;
#76399 = PLANE ( 'NONE',  #36944 ) ;
#76400 = CARTESIAN_POINT ( 'NONE',  ( 0.1742125984251973736, -0.1742125984251973736, -0.3937007874015748254 ) ) ;
#76401 = CARTESIAN_POINT ( 'NONE',  ( -0.3917322834645670104, -7.196005306013484475E-17, -0.4389763779527560139 ) ) ;
#76402 = CARTESIAN_POINT ( 'NONE',  ( -0.5643044619422565855, -0.3690944881889763329, 0.3153832671262228327 ) ) ;
#76403 = CARTESIAN_POINT ( 'NONE',  ( -1.614173228346456268, -0.5511811023622047445, 6.969142054262312111E-17 ) ) ;
#76404 = EDGE_CURVE ( 'NONE', #77294, #41668, #35756, .T. ) ;
#76405 = CARTESIAN_POINT ( 'NONE',  ( -1.345144356955379816, -0.3162353388693405765, 0.4822834645669290543 ) ) ;
#76406 = CARTESIAN_POINT ( 'NONE',  ( -0.07874015748031421014, -0.1870078740157480879, -0.4822834645669291653 ) ) ;
#76407 = CARTESIAN_POINT ( 'NONE',  ( 1.377952755905512472, -0.6692913385826771977, 8.415575281601705876E-17 ) ) ;
#76408 = ORIENTED_EDGE ( 'NONE', *, *, #82874, .T. ) ;
#76409 = FACE_OUTER_BOUND ( 'NONE', #39339, .T. ) ;
#76410 = B_SPLINE_CURVE_WITH_KNOTS ( 'NONE', 3,
 ( #14830, #66584, #8920, #53930 ),
 .UNSPECIFIED., .F., .F.,
 ( 4, 4 ),
 ( 2.888536477662776634E-07, 0.001436607511248048788 ),
 .UNSPECIFIED. ) ;
#76411 = CARTESIAN_POINT ( 'NONE',  ( 0.4091458600556403535, 0.2362204724409449896, -2.178477690288713742 ) ) ;
#76412 = DIRECTION ( 'NONE',  ( 0.000000000000000000, 1.000000000000000000, 0.000000000000000000 ) ) ;
#76413 = CARTESIAN_POINT ( 'NONE',  ( -0.3280839895013117347, -0.004921259842519870586, -0.3153832671262229437 ) ) ;
#76414 = CARTESIAN_POINT ( 'NONE',  ( -1.154855643044618851, 0.2306618581243848609, 0.2411417322834645549 ) ) ;
#76415 = CARTESIAN_POINT ( 'NONE',  ( 1.154855643044620184, -0.6046776061558807314, 0.2411417322834647770 ) ) ;
#76416 = VERTEX_POINT ( 'NONE', #48370 ) ;
#76418 = CARTESIAN_POINT ( 'NONE',  ( -3.924389226575468737, 2.755905511811024056, -0.3149606299212598381 ) ) ;
#76417 = DIRECTION ( 'NONE',  ( -1.000000000000000000, -0.000000000000000000, -0.000000000000000000 ) ) ;
#76419 = EDGE_CURVE ( 'NONE', #28541, #31638, #54170, .T. ) ;
#76420 = CARTESIAN_POINT ( 'NONE',  ( 1.299212598425197429, -0.6692913385826771977, 8.415575281601705876E-17 ) ) ;
#76421 = CARTESIAN_POINT ( 'NONE',  ( -1.364829396325458521, 0.2306618581243847221, -0.2411417322834647770 ) ) ;
#76422 = CARTESIAN_POINT ( 'NONE',  ( 4.797336870675655290E-17, -0.3917322834645669549, -0.4737339650580559280 ) ) ;
#76423 = CARTESIAN_POINT ( 'NONE',  ( -0.3543307086614165824, -0.5511811023622047445, 6.969142054262312111E-17 ) ) ;
#76424 = CARTESIAN_POINT ( 'NONE',  ( 4.797336870675656522E-17, -0.3917322834645670104, -0.6358267716535433989 ) ) ;
#76425 = EDGE_CURVE ( 'NONE', #42415, #28644, #13702, .T. ) ;
#76426 = CARTESIAN_POINT ( 'NONE',  ( -0.5577427821522301654, -0.2845877964562159024, 0.3641732283464567677 ) ) ;
#76427 = CARTESIAN_POINT ( 'NONE',  ( 0.5774278215223103139, -0.5023911411419708095, -0.1820866141732282451 ) ) ;
#76428 = CARTESIAN_POINT ( 'NONE',  ( 0.2559055118110243332, -0.5400638737290845981, -0.3530559997133363437 ) ) ;
#76429 = CARTESIAN_POINT ( 'NONE',  ( -0.6364829396325453192, -0.08942795157528024563, -0.3641732283464568787 ) ) ;
#76430 = CARTESIAN_POINT ( 'NONE',  ( 0.1049643490035304938, -0.3917322834645669549, -2.597112860892388131 ) ) ;
#76431 = CARTESIAN_POINT ( 'NONE',  ( 1.200787401574803681, -0.5400638737290845981, -0.3530559997133363437 ) ) ;
#76432 = CARTESIAN_POINT ( 'NONE',  ( -1.443569553805773564, 0.2306618581243847221, -0.2411417322834647770 ) ) ;
#76433 = CARTESIAN_POINT ( 'NONE',  ( -0.2362204724409451284, 0.4091458600556402425, -1.192257217847769057 ) ) ;
#76434 = CARTESIAN_POINT ( 'NONE',  ( -0.5577427821522301654, -0.05778040916215560624, -0.4822834645669293319 ) ) ;
#76435 = CARTESIAN_POINT ( 'NONE',  ( -0.9448818897637790704, -0.1870078740157480879, -0.4822834645669291653 ) ) ;
#76436 = CARTESIAN_POINT ( 'NONE',  ( 1.318897637795276356, -0.4536011799217367080, 0.2665933059059888421 ) ) ;
#76437 = CARTESIAN_POINT ( 'NONE',  ( -0.4724409448818890911, -0.1870078740157479769, 0.3641732283464567677 ) ) ;
#76438 = CARTESIAN_POINT ( 'NONE',  ( -0.7086614173228339419, -0.1870078740157480879, -0.4822834645669291653 ) ) ;
#76439 = CARTESIAN_POINT ( 'NONE',  ( -1.286089238845143479, 0.2306618581243847221, -0.2411417322834647770 ) ) ;
#76440 = CARTESIAN_POINT ( 'NONE',  ( 0.000000000000000000, 2.755905511811024056, 0.000000000000000000 ) ) ;
#76441 = CARTESIAN_POINT ( 'NONE',  ( 1.397637795275591177, 0.07958543189024071263, -0.2665933059059888421 ) ) ;
#76442 = CARTESIAN_POINT ( 'NONE',  ( -0.4396325459317577122, -0.6692913385826773087, -0.1292274648535924053 ) ) ;
#76443 = CARTESIAN_POINT ( 'NONE',  ( -1.049868766404198794, 0.2306618581243847221, -0.2411417322834647770 ) ) ;
#76444 = EDGE_LOOP ( 'NONE', ( #24519, #11497, #26057, #1964 ) ) ;
#76445 = EDGE_CURVE ( 'NONE', #42893, #31040, #59579, .T. ) ;
#76446 = CARTESIAN_POINT ( 'NONE',  ( 0.3996062992125985480, 2.446882876249141654E-17, -2.399606299212598604 ) ) ;
#76447 =( BOUNDED_CURVE ( )  B_SPLINE_CURVE ( 2, ( #34399, #15050, #33153, #8729, #59229, #20108, #21763, #27245, #47009, #2421, #33982, #71453, #41126, #28078, #72295, #52904, #14641, #59643, #27662, #73117, #2000, #53328, #79037, #21356, #79444, #15469, #32726, #58394, #26415, #13802, #39459, #58822, #1179, #26830, #47841, #49082, #74368, #41539, #29730, #4473, #17133, #60892, #23832, #42765, #36459, #60480, #54984, #2831, #80692, #35228, #74782, #34822, #73954, #23005, #28492, #62133, #73547, #49500, #9558, #3660, #15890, #30141, #54152, #61302, #42352, #79866, #36054, #16711, #29323, #41943, #22184, #67639, #23415, #67227, #68461, #48671, #3242, #28907, #54570, #55804, #81098, #10799, #68050, #75193, #80284, #22597, #17537, #16300, #48258, #10397, #9971, #81510, #35642, #61726, #66817, #4063, #55392, #9150, #76424, #63777, #19158, #24236, #50315, #51131, #25464, #70089, #17945, #82732, #30962, #62965, #5303, #18753, #57452, #69283, #38519, #49909, #57037, #76825, #11629, #12443, #63367, #43581, #18355, #32206, #75606, #76013, #44808, #70503, #38102, #37290, #25051, #56629, #82330, #24648, #44397, #83145, #43998, #12862, #5701, #6117, #31789, #64202, #6536, #50726, #77246, #57863, #69692, #12035, #231, #25882, #37692, #51543, #31373, #30561, #43169, #68865, #11214, #36873, #62551, #81925, #4887, #56227, #21249, #40604, #66287, #53632, #39771, #13281, #46073, #7369, #8211, #65466, #72183, #7800, #59958, #19576, #8626, #34297, #2313, #33039, #6950, #65034, #78089, #1484, #59127, #32621, #33465, #1073, #20835 ),
 .UNSPECIFIED., .F., .F. ) 
 B_SPLINE_CURVE_WITH_KNOTS ( ( 3, 2, 2, 2, 2, 2, 2, 2, 2, 2, 2, 2, 2, 2, 2, 2, 2, 2, 2, 2, 2, 2, 2, 2, 2, 2, 2, 2, 2, 2, 2, 2, 2, 2, 2, 2, 2, 2, 2, 2, 2, 2, 2, 2, 2, 2, 2, 2, 2, 2, 2, 2, 2, 2, 2, 2, 2, 2, 2, 2, 2, 2, 2, 2, 2, 2, 2, 2, 2, 2, 2, 2, 2, 2, 2, 2, 2, 2, 2, 2, 2, 2, 2, 2, 2, 2, 2, 2, 2, 2, 2, 2, 2, 2, 3 ),
 ( 0.07312148491320361043, 0.07499999999999999722, 0.07916666666666666297, 0.08333333333333332871, 0.08749999999999999445, 0.09166666666666666019, 0.09583333333333333981, 0.1000000000000000056, 0.1041666666666666713, 0.1083333333333333370, 0.1125000000000000028, 0.1166666666666666685, 0.1208333333333333204, 0.1250000000000000000, 0.1291666666666666796, 0.1333333333333333315, 0.1375000000000000111, 0.1416666666666666630, 0.1458333333333333426, 0.1499999999999999944, 0.1541666666666666741, 0.1583333333333333259, 0.1625000000000000056, 0.1666666666666666297, 0.1708333333333333370, 0.1749999999999999889, 0.1791666666666666685, 0.1833333333333333204, 0.1875000000000000000, 0.1916666666666666796, 0.1958333333333333592, 0.2000000000000000111, 0.2041666666666666630, 0.2083333333333333426, 0.2124999999999999944, 0.2166666666666666741, 0.2208333333333333259, 0.2250000000000000056, 0.2291666666666666574, 0.2333333333333333370, 0.2374999999999999889, 0.2416666666666666685, 0.2458333333333332926, 0.2500000000000000000, 0.2541666666666666519, 0.2583333333333333592, 0.2624999999999999556, 0.2666666666666666630, 0.2708333333333333148, 0.2750000000000000222, 0.2791666666666666741, 0.2833333333333333259, 0.2874999999999999778, 0.2916666666666667407, 0.2958333333333333370, 0.2999999999999999889, 0.3041666666666666408, 0.3083333333333333481, 0.3125000000000000000, 0.3166666666666666519, 0.3208333333333334147, 0.3249999999999999556, 0.3291666666666666075, 0.3333333333333332593, 0.3375000000000000222, 0.3416666666666666741, 0.3458333333333333259, 0.3499999999999999778, 0.3541666666666666297, 0.3583333333333332815, 0.3624999999999999334, 0.3666666666666665853, 0.3708333333333333481, 0.3750000000000000000, 0.3791666666666666519, 0.3833333333333333037, 0.3874999999999999556, 0.3916666666666666075, 0.3958333333333332593, 0.4000000000000000222, 0.4041666666666666741, 0.4083333333333333259, 0.4124999999999999778, 0.4166666666666666297, 0.4208333333333333925, 0.4249999999999999334, 0.4291666666666665853, 0.4333333333333333481, 0.4375000000000000000, 0.4416666666666666519, 0.4458333333333333037, 0.4499999999999999556, 0.4541666666666666075, 0.4583333333333333703, 0.4606214849132036493 ),
 .UNSPECIFIED. ) 
 CURVE ( )  GEOMETRIC_REPRESENTATION_ITEM ( )  RATIONAL_B_SPLINE_CURVE ( ( 0.9831275833774530959, 0.9846378761473345564, 1.000000000000000000, 0.9659258262890683122, 1.000000000000000000, 0.9659258262890683122, 1.000000000000000000, 0.9659258262890683122, 1.000000000000000000, 0.9659258262890683122, 1.000000000000000000, 0.9659258262890683122, 1.000000000000000000, 0.9659258262890683122, 1.000000000000000000, 0.9659258262890683122, 1.000000000000000000, 0.9659258262890683122, 1.000000000000000000, 0.9659258262890683122, 1.000000000000000000, 0.9659258262890683122, 1.000000000000000000, 0.9659258262890683122, 1.000000000000000000, 0.9659258262890683122, 1.000000000000000000, 0.9659258262890683122, 1.000000000000000000, 0.9659258262890683122, 1.000000000000000000, 0.9659258262890683122, 1.000000000000000000, 0.9659258262890683122, 1.000000000000000000, 0.9659258262890683122, 1.000000000000000000, 0.9659258262890683122, 1.000000000000000000, 0.9659258262890683122, 1.000000000000000000, 0.9659258262890683122, 1.000000000000000000, 0.9659258262890683122, 1.000000000000000000, 0.9659258262890683122, 1.000000000000000000, 0.9659258262890683122, 1.000000000000000000, 0.9659258262890683122, 1.000000000000000000, 0.9659258262890683122, 1.000000000000000000, 0.9659258262890683122, 1.000000000000000000, 0.9659258262890683122, 1.000000000000000000, 0.9659258262890683122, 1.000000000000000000, 0.9659258262890683122, 1.000000000000000000, 0.9659258262890683122, 1.000000000000000000, 0.9659258262890683122, 1.000000000000000000, 0.9659258262890683122, 1.000000000000000000, 0.9659258262890683122, 1.000000000000000000, 0.9659258262890683122, 1.000000000000000000, 0.9659258262890683122, 1.000000000000000000, 0.9659258262890683122, 1.000000000000000000, 0.9659258262890683122, 1.000000000000000000, 0.9659258262890683122, 1.000000000000000000, 0.9659258262890683122, 1.000000000000000000, 0.9659258262890683122, 1.000000000000000000, 0.9659258262890683122, 1.000000000000000000, 0.9659258262890683122, 1.000000000000000000, 0.9659258262890683122, 1.000000000000000000, 0.9659258262890683122, 1.000000000000000000, 0.9659258262890683122, 1.000000000000000000, 0.9659258262890683122, 1.000000000000000000, 0.9659258262890683122, 1.000000000000000000, 0.9659258262890683122, 1.000000000000000000, 0.9659258262890683122, 1.000000000000000000, 0.9659258262890683122, 1.000000000000000000, 0.9659258262890683122, 1.000000000000000000, 0.9659258262890683122, 1.000000000000000000, 0.9659258262890683122, 1.000000000000000000, 0.9659258262890683122, 1.000000000000000000, 0.9659258262890683122, 1.000000000000000000, 0.9659258262890683122, 1.000000000000000000, 0.9659258262890683122, 1.000000000000000000, 0.9659258262890683122, 1.000000000000000000, 0.9659258262890683122, 1.000000000000000000, 0.9659258262890683122, 1.000000000000000000, 0.9659258262890683122, 1.000000000000000000, 0.9659258262890683122, 1.000000000000000000, 0.9659258262890683122, 1.000000000000000000, 0.9659258262890683122, 1.000000000000000000, 0.9659258262890683122, 1.000000000000000000, 0.9659258262890683122, 1.000000000000000000, 0.9659258262890683122, 1.000000000000000000, 0.9659258262890683122, 1.000000000000000000, 0.9659258262890683122, 1.000000000000000000, 0.9659258262890683122, 1.000000000000000000, 0.9659258262890683122, 1.000000000000000000, 0.9659258262890683122, 1.000000000000000000, 0.9659258262890683122, 1.000000000000000000, 0.9659258262890683122, 1.000000000000000000, 0.9659258262890683122, 1.000000000000000000, 0.9659258262890683122, 1.000000000000000000, 0.9659258262890683122, 1.000000000000000000, 0.9659258262890683122, 1.000000000000000000, 0.9659258262890683122, 1.000000000000000000, 0.9659258262890683122, 1.000000000000000000, 0.9659258262890683122, 1.000000000000000000, 0.9659258262890683122, 1.000000000000000000, 0.9659258262890683122, 1.000000000000000000, 0.9659258262890683122, 1.000000000000000000, 0.9659258262890683122, 1.000000000000000000, 0.9659258262890683122, 1.000000000000000000, 0.9659258262890683122, 1.000000000000000000, 0.9659258262890683122, 1.000000000000000000, 0.9659258262890683122, 1.000000000000000000, 0.9659258262890683122, 1.000000000000000000, 0.9659258262890683122, 1.000000000000000000, 0.9659258262890683122, 1.000000000000000000, 0.9812879501417335337, 0.9831275833774533179 ) ) 
 REPRESENTATION_ITEM ( '' )  );
#76448 = CARTESIAN_POINT ( 'NONE',  ( -0.7611548556430438595, -0.5023911411419708095, -0.1820866141732282451 ) ) ;
#76449 = CARTESIAN_POINT ( 'NONE',  ( 1.292650918635171564, 0.2952755905511811885, 0.1292274648535926551 ) ) ;
#76450 = CARTESIAN_POINT ( 'NONE',  ( -0.9186351706036736120, 0.1283753931104748280, 0.1820866141732283561 ) ) ;
#76451 = CARTESIAN_POINT ( 'NONE',  ( -0.1998031496062994405, 0.3460692066303957537, -1.507217847769029007 ) ) ;
#76452 = CARTESIAN_POINT ( 'NONE',  ( -0.9580052493438311334, -0.4281496062992124485, 0.4176697321401328655 ) ) ;
#76453 = CARTESIAN_POINT ( 'NONE',  ( 1.351706036745407680, 0.05413385826771666132, 0.4176697321401328100 ) ) ;
#76454 = CARTESIAN_POINT ( 'NONE',  ( 0.7020997375328090762, -0.3162353388693405765, 0.4822834645669290543 ) ) ;
#76455 = CARTESIAN_POINT ( 'NONE',  ( 1.548556430446194954, -0.6046776061558807314, 0.2411417322834647770 ) ) ;
#76456 = CARTESIAN_POINT ( 'NONE',  ( -1.587926509186350810, -0.3690944881889763329, 0.3153832671262228327 ) ) ;
#76457 = CARTESIAN_POINT ( 'NONE',  ( 0.3996062992125984925, 0.1070741851644054499, -0.6738845144356955252 ) ) ;
#76459 = EDGE_CURVE ( 'NONE', #1651, #74449, #9071, .T. ) ;
#76458 = CARTESIAN_POINT ( 'NONE',  ( -0.3996062992125987146, 0.1070741851644051862, -1.135170603674540590 ) ) ;
#76460 = CARTESIAN_POINT ( 'NONE',  ( 0.2891555358219910499, 0.2891555358219910499, -0.4527559055118110520 ) ) ;
#76461 = CARTESIAN_POINT ( 'NONE',  ( 0.4102808022082889416, 1.299212598425196985, -1.382164990278189398 ) ) ;
#76462 = CARTESIAN_POINT ( 'NONE',  ( 1.338582677165355062, -0.1870078740157479769, 0.3641732283464567677 ) ) ;
#76463 = CARTESIAN_POINT ( 'NONE',  ( 0.7480314960629927956, -0.5511811023622047445, 6.969142054262312111E-17 ) ) ;
#76464 = CARTESIAN_POINT ( 'NONE',  ( 0.6496062992125991586, 0.1660481256975885056, 0.3530559997133364547 ) ) ;
#76465 = CARTESIAN_POINT ( 'NONE',  ( 1.515748031496063186, -0.5400638737290845981, -0.3530559997133363437 ) ) ;
#76466 = CARTESIAN_POINT ( 'NONE',  ( -0.1974969037888706924, 0.3420746716998658843, -1.507217847769029007 ) ) ;
#76467 = CARTESIAN_POINT ( 'NONE',  ( 0.7874015748031503170, -0.1870078740157480601, -0.3641732283464567677 ) ) ;
#76468 = CARTESIAN_POINT ( 'NONE',  ( -0.3740157480314953431, 0.1660481256975885056, 0.3530559997133364547 ) ) ;
#76469 = CARTESIAN_POINT ( 'NONE',  ( -1.259842519685038686, -0.1870078740157480879, -0.4822834645669291653 ) ) ;
#76470 = CARTESIAN_POINT ( 'NONE',  ( 1.003937007874016407, -0.5400638737290844871, 0.3530559997133364547 ) ) ;
#76471 = CARTESIAN_POINT ( 'NONE',  ( 0.4091458600556403535, 0.2362204724409449896, -1.706036745406824151 ) ) ;
#76472 = CARTESIAN_POINT ( 'NONE',  ( 0.2925321140481932369, 0.2925321140481932369, -2.657480314960630086 ) ) ;
#76473 = ORIENTED_EDGE ( 'NONE', *, *, #65474, .F. ) ;
#76474 = VERTEX_POINT ( 'NONE', #5821 ) ;
#76475 = CARTESIAN_POINT ( 'NONE',  ( -1.122047244094487306, -0.5400638737290844871, 0.3530559997133364547 ) ) ;
#76476 = CARTESIAN_POINT ( 'NONE',  ( -0.6955380577427815458, 0.05413385826771666132, 0.4176697321401328100 ) ) ;
#76478 = CARTESIAN_POINT ( 'NONE',  ( -0.6627296587926501115, 0.2952755905511810774, -0.1292274648535930714 ) ) ;
#76477 = CARTESIAN_POINT ( 'NONE',  ( -0.9711286089238838626, 0.1283753931104746893, -0.1820866141732285504 ) ) ;
#76479 = CARTESIAN_POINT ( 'NONE',  ( -0.1049643490035301746, -0.3917322834645670659, -2.041975434874328865 ) ) ;
#76480 = CARTESIAN_POINT ( 'NONE',  ( 0.2427821522309719648, -0.05778040916215522460, 0.4822834645669289988 ) ) ;
#76481 = CARTESIAN_POINT ( 'NONE',  ( -0.5643044619422565855, -0.4281496062992124485, 0.4176697321401328655 ) ) ;
#76482 = CARTESIAN_POINT ( 'NONE',  ( 1.502624671916010790, -0.3162353388693409650, -0.4822834645669289433 ) ) ;
#76483 = CARTESIAN_POINT ( 'NONE',  ( -0.8858267716535425107, 0.1660481256975883668, -0.3530559997133364547 ) ) ;
#76484 = CARTESIAN_POINT ( 'NONE',  ( 0.6102362204724416372, -0.5400638737290844871, 0.3530559997133364547 ) ) ;
#76485 = CARTESIAN_POINT ( 'NONE',  ( -0.1049643490035302024, -0.3917322834645671215, -1.481627296587926690 ) ) ;
#76486 = CARTESIAN_POINT ( 'NONE',  ( -0.9055118110236215490, -0.5511811023622047445, 6.969142054262312111E-17 ) ) ;
#76487 = ORIENTED_EDGE ( 'NONE', *, *, #58647, .F. ) ;
#76488 = CARTESIAN_POINT ( 'NONE',  ( 0.3949938075777409408, 0.1058382717557500574, -2.014435695538057569 ) ) ;
#76489 = EDGE_LOOP ( 'NONE', ( #56760, #66677, #27308, #31107 ) ) ;
#76490 = CARTESIAN_POINT ( 'NONE',  ( -1.417322834645668772, -0.1870078740157479769, 0.3641732283464567677 ) ) ;
#76491 = CARTESIAN_POINT ( 'NONE',  ( -1.259842519685038686, -0.1870078740157480879, -0.4822834645669291653 ) ) ;
#76492 = CARTESIAN_POINT ( 'NONE',  ( -0.7874015748031489847, -0.1870078740157480879, -0.4822834645669291653 ) ) ;
#76493 = CARTESIAN_POINT ( 'NONE',  ( 0.3996062992125986035, 0.1070741851644054776, -0.1246719160104987068 ) ) ;
#76494 = CARTESIAN_POINT ( 'NONE',  ( -0.9973753280839886548, -0.6046776061558809534, -0.2411417322834644161 ) ) ;
#76495 = CARTESIAN_POINT ( 'NONE',  ( -1.371391076115484831, 0.2952755905511810774, -0.1292274648535930714 ) ) ;
#76496 = FACE_OUTER_BOUND ( 'NONE', #60873, .T. ) ;
#76497 = CARTESIAN_POINT ( 'NONE',  ( -1.699475065616797398, 0.2952755905511811885, 0.1292274648535926551 ) ) ;
#76498 = CARTESIAN_POINT ( 'NONE',  ( 0.4330708661417329575, 0.1771653543307087630, 0.000000000000000000 ) ) ;
#76499 = CARTESIAN_POINT ( 'NONE',  ( -1.646051170424378096, 0.000000000000000000, -0.3464511005275205946 ) ) ;
#76500 = CARTESIAN_POINT ( 'NONE',  ( 0.3917322834645669549, 0.1049643490035304660, 0.1056430446194224632 ) ) ;
#76501 = CARTESIAN_POINT ( 'NONE',  ( -0.2230971128608915943, -0.3690944881889765550, -0.3153832671262227771 ) ) ;
#76502 = CARTESIAN_POINT ( 'NONE',  ( -0.2296587926509179312, -0.05778040916215522460, 0.4822834645669289988 ) ) ;
#76503 = CARTESIAN_POINT ( 'NONE',  ( 1.272965879265092637, 0.05413385826771666132, 0.4176697321401328100 ) ) ;
#76504 = CARTESIAN_POINT ( 'NONE',  ( -0.4002624671916004129, -0.3162353388693405765, 0.4822834645669290543 ) ) ;
#76505 = EDGE_LOOP ( 'NONE', ( #55466, #30724, #76164, #15969 ) ) ;
#76506 = ORIENTED_EDGE ( 'NONE', *, *, #31518, .F. ) ;
#76507 = CARTESIAN_POINT ( 'NONE',  ( 0.3996062992125986035, -0.1070741851644052972, -1.448162729658792669 ) ) ;
#76508 = CARTESIAN_POINT ( 'NONE',  ( -0.4855643044619415427, 0.05413385826771626580, -0.4176697321401330321 ) ) ;
#76509 = CARTESIAN_POINT ( 'NONE',  ( 1.496062992125984703, -0.1870078740157480879, -0.4822834645669291653 ) ) ;
#76510 = CARTESIAN_POINT ( 'NONE',  ( -0.9973753280839886548, -0.5023911411419708095, -0.1820866141732282451 ) ) ;
#76511 = CARTESIAN_POINT ( 'NONE',  ( -1.509186351706035767, 0.05413385826771626580, -0.4176697321401330321 ) ) ;
#76512 = CARTESIAN_POINT ( 'NONE',  ( -1.157146581871515012E-16, 0.4724409448818898682, -0.9448818897637796255 ) ) ;
#76513 = CARTESIAN_POINT ( 'NONE',  ( -0.7330049731600565277, 2.188112158501061444, 0.5178675056770625229 ) ) ;
#76514 = CARTESIAN_POINT ( 'NONE',  ( -0.3917322834645671215, 0.1049643490035301469, -2.794619422572177658 ) ) ;
#76515 = CARTESIAN_POINT ( 'NONE',  ( 1.200787401574803681, 0.1660481256975885056, 0.3530559997133364547 ) ) ;
#76516 = CARTESIAN_POINT ( 'NONE',  ( -0.3392501089628019995, 0.1958661417322832277, -2.000656167979002920 ) ) ;
#76517 = CARTESIAN_POINT ( 'NONE',  ( 8.195543980992789655E-16, -0.1870078740157480879, -0.4822834645669291653 ) ) ;
#76518 = CARTESIAN_POINT ( 'NONE',  ( -1.200787401574802349, -0.4536011799217367080, 0.2665933059059888421 ) ) ;
#76519 = CARTESIAN_POINT ( 'NONE',  ( -0.2821522309711278487, 0.2952755905511811885, 0.1292274648535926551 ) ) ;
#76520 = CARTESIAN_POINT ( 'NONE',  ( 0.3458507752293908943, 0.3458507752293908943, -2.734251968503936148 ) ) ;
#76521 = CARTESIAN_POINT ( 'NONE',  ( -0.9120734908136475250, 0.2952755905511811885, 0.1292274648535926551 ) ) ;
#76522 = ADVANCED_FACE ( 'NONE', ( #5416 ), #44113, .F. ) ;
#76523 = CARTESIAN_POINT ( 'NONE',  ( -1.194225721784776262, 0.05413385826771626580, -0.4176697321401330321 ) ) ;
#76524 = CARTESIAN_POINT ( 'NONE',  ( 0.1974969037888704704, 0.3420746716998660508, -2.268372703412073754 ) ) ;
#76525 = CARTESIAN_POINT ( 'NONE',  ( 1.056430446194226436, -0.5511811023622048555, -0.09757992244046775898 ) ) ;
#76526 = CARTESIAN_POINT ( 'NONE',  ( -0.4199475065616791736, 0.1283753931104746893, -0.1820866141732285504 ) ) ;
#76527 = CARTESIAN_POINT ( 'NONE',  ( 0.6627296587926517768, -0.5511811023622048555, -0.09757992244046775898 ) ) ;
#76528 = CARTESIAN_POINT ( 'NONE',  ( -1.561679790026246017, 0.05413385826771666132, 0.4176697321401328100 ) ) ;
#76529 = CARTESIAN_POINT ( 'NONE',  ( 1.581364829396326277, -0.05778040916215522460, 0.4822834645669289988 ) ) ;
#76530 = CARTESIAN_POINT ( 'NONE',  ( 0.4330708661417329575, 0.1771653543307087630, 0.000000000000000000 ) ) ;
#76531 = CARTESIAN_POINT ( 'NONE',  ( -0.8595800524934373854, -0.05778040916215522460, 0.4822834645669289988 ) ) ;
#76532 = CARTESIAN_POINT ( 'NONE',  ( 1.200787401574803681, -0.5400638737290845981, -0.3530559997133363437 ) ) ;
#76533 = CARTESIAN_POINT ( 'NONE',  ( -0.4091458600556405756, 0.2362204724409446288, -0.1030183727034120617 ) ) ;
#76534 = CARTESIAN_POINT ( 'NONE',  ( -0.1181102362204717315, -0.5511811023622047445, 6.969142054262312111E-17 ) ) ;
#76535 = DIRECTION ( 'NONE',  ( 0.000000000000000000, 1.000000000000000000, 0.000000000000000000 ) ) ;
#76536 = CARTESIAN_POINT ( 'NONE',  ( 0.1443569553805781891, 0.05413385826771626580, -0.4176697321401330321 ) ) ;
#76537 = CYLINDRICAL_SURFACE ( 'NONE', #72084, 0.1771653543307088186 ) ;
#76538 = CARTESIAN_POINT ( 'NONE',  ( 1.450131233595801428, 0.1771653543307087630, 0.09757992244046791164 ) ) ;
#76539 = CARTESIAN_POINT ( 'NONE',  ( 0.01968503937007930540, 0.07958543189024085140, 0.2665933059059887866 ) ) ;
#76540 = CARTESIAN_POINT ( 'NONE',  ( -1.345144356955379816, -0.05778040916215560624, -0.4822834645669293319 ) ) ;
#76541 = CARTESIAN_POINT ( 'NONE',  ( -0.7020997375328074108, -0.08942795157527998196, 0.3641732283464567121 ) ) ;
#76542 = PLANE ( 'NONE',  #43461 ) ;
#76543 = CARTESIAN_POINT ( 'NONE',  ( -1.266404199475064773, -0.3162353388693405765, 0.4822834645669290543 ) ) ;
#76544 = CARTESIAN_POINT ( 'NONE',  ( -0.4002624671916004129, -0.3162353388693405765, 0.4822834645669290543 ) ) ;
#76545 = CARTESIAN_POINT ( 'NONE',  ( 0.3460692066303958092, 0.1998031496062993018, -0.5229658792650918597 ) ) ;
#76546 = CARTESIAN_POINT ( 'NONE',  ( 0.3392501089628018884, -0.1958661417322834220, -2.079396325459317740 ) ) ;
#76547 = CARTESIAN_POINT ( 'NONE',  ( 0.7480314960629927956, -0.5511811023622047445, 6.969142054262312111E-17 ) ) ;
#76548 = CARTESIAN_POINT ( 'NONE',  ( -0.2887139107611542133, -0.6046776061558809534, -0.2411417322834644161 ) ) ;
#76549 = CARTESIAN_POINT ( 'NONE',  ( -0.5839895013123351797, -0.6692913385826771977, 0.1292274648535927661 ) ) ;
#76550 = CARTESIAN_POINT ( 'NONE',  ( -0.7086614173228339419, -0.1870078740157479769, 0.3641732283464567677 ) ) ;
#76551 = CARTESIAN_POINT ( 'NONE',  ( -3.911874546793528307, 1.370070907001625482, 0.4441891910510556429 ) ) ;
#76552 = CARTESIAN_POINT ( 'NONE',  ( -0.01312335958005186876, 0.05413385826771626580, -0.4176697321401330321 ) ) ;
#76553 = CARTESIAN_POINT ( 'NONE',  ( -1.561679790026246017, -0.004921259842519576551, 0.3153832671262227771 ) ) ;
#76554 = CARTESIAN_POINT ( 'NONE',  ( 1.345144356955381593, -0.3162353388693409650, -0.4822834645669289433 ) ) ;
#76555 = DIRECTION ( 'NONE',  ( 0.000000000000000000, 0.000000000000000000, 1.000000000000000000 ) ) ;
#76556 = CARTESIAN_POINT ( 'NONE',  ( 0.1049643490035304799, -0.3917322834645670104, -2.286764722605985956 ) ) ;
#76557 = ORIENTED_EDGE ( 'NONE', *, *, #57094, .T. ) ;
#76558 = CARTESIAN_POINT ( 'NONE',  ( 0.000000000000000000, 0.7086614173228346081, 0.4527559055118110520 ) ) ;
#76559 = CARTESIAN_POINT ( 'NONE',  ( -1.266404199475064773, -0.3162353388693405765, 0.4822834645669290543 ) ) ;
#76560 = CARTESIAN_POINT ( 'NONE',  ( -0.9317585301837263412, 0.05413385826771666132, 0.4176697321401328100 ) ) ;
#76561 = CARTESIAN_POINT ( 'NONE',  ( 1.574803149606299746, -0.1870078740157479769, 0.4822834645669291653 ) ) ;
#76562 = CARTESIAN_POINT ( 'NONE',  ( 0.3392501089628018329, 0.1958661417322835607, -1.790682414698162805 ) ) ;
#76563 = CARTESIAN_POINT ( 'NONE',  ( -0.3149606299212459048, 2.559055118110236560, -3.937007874015763242 ) ) ;
#76564 = CARTESIAN_POINT ( 'NONE',  ( 1.023622047244095334, -0.1870078740157479769, 0.4822834645669291653 ) ) ;
#76565 = CARTESIAN_POINT ( 'NONE',  ( -0.01312335958005186876, 0.05413385826771626580, -0.4176697321401330321 ) ) ;
#76566 = DIRECTION ( 'NONE',  ( 1.000000000000000000, -0.000000000000000000, -0.000000000000000000 ) ) ;
#76567 = CARTESIAN_POINT ( 'NONE',  ( -0.7480314960629916854, 2.793565526369265584, 0.000000000000000000 ) ) ;
#76568 = CARTESIAN_POINT ( 'NONE',  ( 1.200787401574803681, -0.4536011799217368745, -0.2665933059059886201 ) ) ;
#76569 = CARTESIAN_POINT ( 'NONE',  ( 0.3996062992125986590, -0.1070741851644053111, -1.528871391076114916 ) ) ;
#76570 = ORIENTED_EDGE ( 'NONE', *, *, #66179, .T. ) ;
#76571 = CARTESIAN_POINT ( 'NONE',  ( 0.3917322834645670659, -0.1049643490035303273, 0.04919328264335768447 ) ) ;
#76572 = EDGE_LOOP ( 'NONE', ( #80018, #11458, #78896, #52430 ) ) ;
#76573 = CARTESIAN_POINT ( 'NONE',  ( 0.3740157480314966754, 0.1660481256975883668, -0.3530559997133364547 ) ) ;
#76574 = CARTESIAN_POINT ( 'NONE',  ( -0.6430446194225716283, -0.4281496062992124485, 0.4176697321401328655 ) ) ;
#76575 = CARTESIAN_POINT ( 'NONE',  ( -1.561679790026246017, -0.4281496062992127816, -0.4176697321401328100 ) ) ;
#76576 = CARTESIAN_POINT ( 'NONE',  ( 0.8530183727034128527, -0.4281496062992124485, 0.4176697321401328655 ) ) ;
#76577 = CARTESIAN_POINT ( 'NONE',  ( -1.561679790026246017, -0.3690944881889765550, -0.3153832671262227771 ) ) ;
#76578 = CARTESIAN_POINT ( 'NONE',  ( 1.377952755905512472, -0.6692913385826771977, 8.415575281601705876E-17 ) ) ;
#76579 = CARTESIAN_POINT ( 'NONE',  ( -0.07217847769028787330, -0.05778040916215522460, 0.4822834645669289988 ) ) ;
#76580 = CARTESIAN_POINT ( 'NONE',  ( -1.200787401574802349, -0.5400638737290844871, 0.3530559997133364547 ) ) ;
#76581 = CARTESIAN_POINT ( 'NONE',  ( 1.456692913385827515, 0.2952755905511811885, 0.000000000000000000 ) ) ;
#76582 = CARTESIAN_POINT ( 'NONE',  ( 1.646981627296588035, -0.3162353388693405765, 0.4822834645669290543 ) ) ;
#76583 = CARTESIAN_POINT ( 'NONE',  ( -0.1049643490035302024, -0.3917322834645671215, -0.06430446194225715451 ) ) ;
#76584 = CARTESIAN_POINT ( 'NONE',  ( 0.8989501312335964611, 0.1771653543307087630, 0.09757992244046791164 ) ) ;
#76585 = EDGE_LOOP ( 'NONE', ( #54653, #60447 ) ) ;
#76586 = CARTESIAN_POINT ( 'NONE',  ( -0.1974969037888703871, -0.3420746716998661063, -0.06561679790026252179 ) ) ;
#76587 = VERTEX_POINT ( 'NONE', #24760 ) ;
#76588 = CARTESIAN_POINT ( 'NONE',  ( 0.1837270341207354329, 0.1283753931104748280, 0.1820866141732283561 ) ) ;
#76589 = CARTESIAN_POINT ( 'NONE',  ( 2.784923006909812759, 1.160811571118577579, -0.2889173282905524442 ) ) ;
#76590 = CARTESIAN_POINT ( 'NONE',  ( 0.09186351706036799403, -0.4281496062992127816, -0.4176697321401328100 ) ) ;
#76591 = CARTESIAN_POINT ( 'NONE',  ( 0.3346456692913390985, 0.1660481256975885056, 0.3530559997133364547 ) ) ;
#76592 = CARTESIAN_POINT ( 'NONE',  ( -0.7020997375328076329, -0.3162353388693409650, -0.4822834645669289433 ) ) ;
#76593 = CARTESIAN_POINT ( 'NONE',  ( 0.1049643490035304799, -0.3917322834645670104, -1.814323777724096809 ) ) ;
#76594 = CARTESIAN_POINT ( 'NONE',  ( -1.076115485564303809, -0.6046776061558809534, -0.2411417322834644161 ) ) ;
#76595 = CARTESIAN_POINT ( 'NONE',  ( -0.1958661417322834220, -0.3392501089628018884, -2.669947506561679784 ) ) ;
#76596 = CARTESIAN_POINT ( 'NONE',  ( 1.161417322834646271, 0.07958543189024071263, -0.2665933059059888421 ) ) ;
#76597 = CARTESIAN_POINT ( 'NONE',  ( 0.7086614173228353852, -0.1870078740157479769, 0.4822834645669291653 ) ) ;
#76598 = CARTESIAN_POINT ( 'NONE',  ( 0.8398950131233602345, -0.6046776061558807314, 0.2411417322834647770 ) ) ;
#76599 = CARTESIAN_POINT ( 'NONE',  ( -0.2925321140481930704, -0.2925321140481933480, -1.003937007874015741 ) ) ;
#76600 = CARTESIAN_POINT ( 'NONE',  ( -1.338582677165353729, -0.1870078740157480879, -0.4822834645669291653 ) ) ;
#76601 = CARTESIAN_POINT ( 'NONE',  ( 0.3460692066303958092, 0.1998031496062993018, -0.5229658792650918597 ) ) ;
#76602 = CARTESIAN_POINT ( 'NONE',  ( 0.3460692066303959202, -0.1998031496062991630, -0.1817585301837270351 ) ) ;
#76603 = CARTESIAN_POINT ( 'NONE',  ( 0.06561679790026316017, 0.05413385826771626580, -0.4176697321401330321 ) ) ;
#76604 = CARTESIAN_POINT ( 'NONE',  ( 0.3996062992125986590, -0.1070741851644053111, -2.788713910761154047 ) ) ;
#76605 = EDGE_CURVE ( 'NONE', #15345, #45100, #82481, .T. ) ;
#76606 = CARTESIAN_POINT ( 'NONE',  ( 0.3392501089628018884, -0.1958661417322834220, -1.606955380577427928 ) ) ;
#76607 = CARTESIAN_POINT ( 'NONE',  ( 1.410761154855643795, -0.3162353388693405765, 0.4822834645669290543 ) ) ;
#76608 = CARTESIAN_POINT ( 'NONE',  ( 1.417322834645670104, -0.1870078740157480879, -0.4822834645669291653 ) ) ;
#76609 = CARTESIAN_POINT ( 'NONE',  ( 0.2559055118110243332, 0.07958543189024085140, 0.2665933059059887866 ) ) ;
#76610 = CARTESIAN_POINT ( 'NONE',  ( 1.056430446194226436, -0.6692913385826773087, -0.1292274648535924053 ) ) ;
#76611 = CARTESIAN_POINT ( 'NONE',  ( 0.4091458600556403535, 0.2362204724409449896, -1.310367454068241511 ) ) ;
#76612 = CARTESIAN_POINT ( 'NONE',  ( 0.2099737532808405305, -0.5023911411419708095, 0.1820866141732285504 ) ) ;
#76613 = CARTESIAN_POINT ( 'NONE',  ( 0.1902887139107617975, 0.2952755905511811885, 0.1292274648535926551 ) ) ;
#76614 = CARTESIAN_POINT ( 'NONE',  ( 0.2891555358219910499, 0.2891555358219910499, -1.001968503937007871 ) ) ;
#76615 = CARTESIAN_POINT ( 'NONE',  ( -1.312335958005248715, -0.6046776061558809534, -0.2411417322834644161 ) ) ;
#76616 = CARTESIAN_POINT ( 'NONE',  ( 0.9514435695538062676, -0.08942795157527998196, 0.3641732283464567121 ) ) ;
#76617 = CARTESIAN_POINT ( 'NONE',  ( 0.3412073490813655186, 0.1539470093639523085, 0.1968503937007873850 ) ) ;
#76618 = CARTESIAN_POINT ( 'NONE',  ( -0.1115485564304456306, 0.2952755905511810774, -0.1292274648535930714 ) ) ;
#76619 = CARTESIAN_POINT ( 'NONE',  ( -0.3280839895013117347, -0.004921259842519870586, -0.3153832671262229437 ) ) ;
#76620 = CARTESIAN_POINT ( 'NONE',  ( 0.4724409448818898682, 0.000000000000000000, -2.755905511811024056 ) ) ;
#76621 = CARTESIAN_POINT ( 'NONE',  ( -0.3674540682414692561, -0.6046776061558809534, -0.2411417322834644161 ) ) ;
#76622 = CARTESIAN_POINT ( 'NONE',  ( 0.1509186351706042484, -0.2845877964562159024, 0.3641732283464567677 ) ) ;
#76623 = CARTESIAN_POINT ( 'NONE',  ( -0.3996062992125985480, -7.340648628747423112E-17, -2.005905511811023612 ) ) ;
#76624 = CARTESIAN_POINT ( 'NONE',  ( -0.2230971128608915943, 0.05413385826771666132, 0.4176697321401328100 ) ) ;
#76625 = CARTESIAN_POINT ( 'NONE',  ( 1.003937007874016407, -0.4536011799217367080, 0.2665933059059888421 ) ) ;
#76626 = DIRECTION ( 'NONE',  ( 0.000000000000000000, 0.000000000000000000, 1.000000000000000000 ) ) ;
#76627 = CARTESIAN_POINT ( 'NONE',  ( -0.8136482939632537770, -0.5023911411419708095, 0.1820866141732285504 ) ) ;
#76628 = CARTESIAN_POINT ( 'NONE',  ( -0.5446194225721777693, -0.2845877964562161244, -0.3641732283464567121 ) ) ;
#76629 = CARTESIAN_POINT ( 'NONE',  ( -0.3083989501312330295, -0.3162353388693409650, -0.4822834645669289433 ) ) ;
#76630 = CARTESIAN_POINT ( 'NONE',  ( 0.02624671916010564918, 0.2306618581243848609, 0.2411417322834645549 ) ) ;
#76631 = CARTESIAN_POINT ( 'NONE',  ( 0.9448818897637802916, -0.1870078740157480601, -0.3641732283464567677 ) ) ;
#76632 = CARTESIAN_POINT ( 'NONE',  ( -1.559171609364246924, 0.4110443821404751730, 0.4177787735906735578 ) ) ;
#76633 = CARTESIAN_POINT ( 'NONE',  ( 1.423884514435696191, -0.08942795157527998196, 0.3641732283464567121 ) ) ;
#76634 = CARTESIAN_POINT ( 'NONE',  ( 0.8595800524934390507, -0.3162353388693405765, 0.4822834645669290543 ) ) ;
#76635 = CYLINDRICAL_SURFACE ( 'NONE', #70634, 0.09842519685039351207 ) ;
#76636 = CARTESIAN_POINT ( 'NONE',  ( -0.3215223097112853146, -0.3162353388693405765, 0.4822834645669290543 ) ) ;
#76637 = CARTESIAN_POINT ( 'NONE',  ( -0.2867679344610364334, -0.2867679344610367109, -1.088582677165354173 ) ) ;
#76638 = CARTESIAN_POINT ( 'NONE',  ( -1.528871391076114250, 0.2952755905511810774, -0.1292274648535930714 ) ) ;
#76639 = CARTESIAN_POINT ( 'NONE',  ( 1.089238845144357759, 0.05413385826771626580, -0.4176697321401330321 ) ) ;
#76640 = CARTESIAN_POINT ( 'NONE',  ( 0.4790026246719168435, -0.3162353388693409650, -0.4822834645669289433 ) ) ;
#76641 = CARTESIAN_POINT ( 'NONE',  ( -0.4109163706260607896, 1.299800539985194403, -3.915511880786665788 ) ) ;
#76642 = CARTESIAN_POINT ( 'NONE',  ( 0.2165354330708668673, -0.4536011799217367080, 0.2665933059059888421 ) ) ;
#76643 = CARTESIAN_POINT ( 'NONE',  ( 1.325459317585302665, -0.4281496062992124485, 0.4176697321401328655 ) ) ;
#76644 = CARTESIAN_POINT ( 'NONE',  ( -0.4658792650918627265, -0.08942795157527998196, 0.3641732283464567121 ) ) ;
#76645 = CARTESIAN_POINT ( 'NONE',  ( -0.5511811023622038563, -0.1870078740157479769, 0.4822834645669291653 ) ) ;
#76646 = CARTESIAN_POINT ( 'NONE',  ( 1.881758995267131418, 2.742776584231126247, 0.5314960629921260393 ) ) ;
#76647 = CARTESIAN_POINT ( 'NONE',  ( 0.07874015748031558404, -0.1870078740157480879, -0.4822834645669291653 ) ) ;
#76648 = CARTESIAN_POINT ( 'NONE',  ( -0.7349081364829387342, -0.6046776061558807314, 0.2411417322834647770 ) ) ;
#76649 = CARTESIAN_POINT ( 'NONE',  ( -0.8202099737532801971, -0.5511811023622046335, 0.09757992244046803654 ) ) ;
#76650 = CARTESIAN_POINT ( 'NONE',  ( 0.3674540682414705883, 0.2306618581243847221, -0.2411417322834647770 ) ) ;
#76651 = CARTESIAN_POINT ( 'NONE',  ( -1.463254593175852492, -0.6692913385826773087, -0.1292274648535924053 ) ) ;
#76652 = CARTESIAN_POINT ( 'NONE',  ( -0.2493438320209966919, -0.4281496062992124485, 0.4176697321401328655 ) ) ;
#76654 = CARTESIAN_POINT ( 'NONE',  ( 1.187664041994751285, -0.3162353388693409650, -0.4822834645669289433 ) ) ;
#76653 = DIRECTION ( 'NONE',  ( 0.000000000000000000, 0.000000000000000000, -1.000000000000000000 ) ) ;
#76655 = CARTESIAN_POINT ( 'NONE',  ( 1.167979002624672580, -0.4281496062992124485, 0.4176697321401328655 ) ) ;
#76656 = CARTESIAN_POINT ( 'NONE',  ( -0.3917322834645669549, -0.1049643490035306603, -2.085301837270341352 ) ) ;
#76657 = CARTESIAN_POINT ( 'NONE',  ( -1.581364829396324945, -0.05778040916215560624, -0.4822834645669293319 ) ) ;
#76658 = CARTESIAN_POINT ( 'NONE',  ( -0.7152230971128602510, -0.05778040916215560624, -0.4822834645669293319 ) ) ;
#76659 = CARTESIAN_POINT ( 'NONE',  ( 0.4724409448818896462, 0.1265901696524990294, -0.4396325459317584339 ) ) ;
#76660 = CARTESIAN_POINT ( 'NONE',  ( -0.3460692066303958092, -0.1998031496062994683, -0.05249343832020999384 ) ) ;
#76661 = ORIENTED_EDGE ( 'NONE', *, *, #50364, .F. ) ;
#76662 = CARTESIAN_POINT ( 'NONE',  ( -0.1181102362204717315, -0.5511811023622047445, 6.969142054262312111E-17 ) ) ;
#76663 = CARTESIAN_POINT ( 'NONE',  ( 0.1049643490035303689, 0.3917322834645670104, -1.560367454068241511 ) ) ;
#76664 = CARTESIAN_POINT ( 'NONE',  ( 0.7808398950131240079, -0.3162353388693405765, 0.4822834645669290543 ) ) ;
#76665 = CARTESIAN_POINT ( 'NONE',  ( -0.1265901696524993347, 0.4724409448818895907, -2.841207349081364963 ) ) ;
#76666 = LINE ( 'NONE', #77086, #38579 ) ;
#76667 = CARTESIAN_POINT ( 'NONE',  ( -0.3018372703412066094, -0.3690944881889765550, -0.3153832671262227771 ) ) ;
#76668 = LINE ( 'NONE', #51807, #79002 ) ;
#76669 = CARTESIAN_POINT ( 'NONE',  ( 1.154855643044620184, -0.6046776061558807314, 0.2411417322834647770 ) ) ;
#76670 = CARTESIAN_POINT ( 'NONE',  ( 0.8792650918635177559, -0.3690944881889765550, -0.3153832671262227771 ) ) ;
#76671 = CIRCLE ( 'NONE', #40397, 3.543307086614173151 ) ;
#76672 = CARTESIAN_POINT ( 'NONE',  ( -0.1968503937007867743, 0.2952755905511811885, 0.000000000000000000 ) ) ;
#76673 = CARTESIAN_POINT ( 'NONE',  ( -0.1958661417322836440, 0.3392501089628016664, -0.7230777970790532860 ) ) ;
#76674 = CARTESIAN_POINT ( 'NONE',  ( -0.2952755905511803003, -0.5400638737290845981, -0.3530559997133363437 ) ) ;
#76675 = CARTESIAN_POINT ( 'NONE',  ( -1.404199475065615932, -0.004921259842519576551, 0.3153832671262227771 ) ) ;
#76676 = CARTESIAN_POINT ( 'NONE',  ( -0.3018372703412066094, 0.05413385826771666132, 0.4176697321401328100 ) ) ;
#76677 = DIRECTION ( 'NONE',  ( 0.000000000000000000, 0.000000000000000000, -1.000000000000000000 ) ) ;
#76678 = CARTESIAN_POINT ( 'NONE',  ( 0.4581547953330915024, 1.765968763644078399, -0.5309055118110237448 ) ) ;
#76679 = ORIENTED_EDGE ( 'NONE', *, *, #57395, .F. ) ;
#76680 = CARTESIAN_POINT ( 'NONE',  ( -0.2867679344610367109, 0.2867679344610365444, -1.906187294784464026 ) ) ;
#76681 = CARTESIAN_POINT ( 'NONE',  ( 0.4461942257217856311, 0.2306618581243847221, -0.2411417322834647770 ) ) ;
#76682 = VERTEX_POINT ( 'NONE', #62668 ) ;
#76683 = CARTESIAN_POINT ( 'NONE',  ( -0.5643044619422565855, 0.05413385826771626580, -0.4176697321401330321 ) ) ;
#76684 = CARTESIAN_POINT ( 'NONE',  ( 1.502624671916010790, -0.3162353388693409650, -0.4822834645669289433 ) ) ;
#76685 = CARTESIAN_POINT ( 'NONE',  ( 0.7939632545931766261, -0.05778040916215522460, 0.4822834645669289988 ) ) ;
#76686 = CARTESIAN_POINT ( 'NONE',  ( -0.1312335958005241554, -0.6046776061558809534, -0.2411417322834644161 ) ) ;
#76687 = CARTESIAN_POINT ( 'NONE',  ( 0.3917322834645670104, 2.398668435337828261E-17, -1.305118110236220375 ) ) ;
#76688 = CARTESIAN_POINT ( 'NONE',  ( -0.8661417322834640276, -0.1870078740157480879, -0.4822834645669291653 ) ) ;
#76689 = CARTESIAN_POINT ( 'NONE',  ( -0.3215223097112853146, -0.05778040916215560624, -0.4822834645669293319 ) ) ;
#76690 = CARTESIAN_POINT ( 'NONE',  ( -1.069553805774277722, -0.6692913385826773087, -0.1292274648535924053 ) ) ;
#76691 = CARTESIAN_POINT ( 'NONE',  ( 0.03280839895013198948, -0.5511811023622048555, -0.09757992244046775898 ) ) ;
#76692 = CARTESIAN_POINT ( 'NONE',  ( -0.2952755905511810774, -3.179810529374183920E-17, 5.879133660591329580 ) ) ;
#76693 = CARTESIAN_POINT ( 'NONE',  ( -0.04593175853018302557, -0.6692913385826773087, -0.1292274648535924053 ) ) ;
#76694 = CARTESIAN_POINT ( 'NONE',  ( 0.4091458600556404646, -0.2362204724409448231, -0.9691601049868766582 ) ) ;
#76695 = CARTESIAN_POINT ( 'NONE',  ( 1.036745406824147508, -0.4281496062992127816, -0.4176697321401328100 ) ) ;
#76696 = CARTESIAN_POINT ( 'NONE',  ( 0.2867679344610365999, -0.2867679344610365444, -2.925196850393700920 ) ) ;
#76697 = ORIENTED_EDGE ( 'NONE', *, *, #68362, .F. ) ;
#76698 = EDGE_CURVE ( 'NONE', #21487, #36098, #82258, .T. ) ;
#76699 = ORIENTED_EDGE ( 'NONE', *, *, #21875, .T. ) ;
#76700 = CARTESIAN_POINT ( 'NONE',  ( 0.1968503937007881344, -0.6692913385826771977, 8.415575281601705876E-17 ) ) ;
#76701 = CARTESIAN_POINT ( 'NONE',  ( -0.4593175853018366950, -0.004921259842519576551, 0.3153832671262227771 ) ) ;
#76703 = CARTESIAN_POINT ( 'NONE',  ( -0.06840103802055999549, -4.511432564584533345E-15, 0.4281993546915565108 ) ) ;
#76702 = CARTESIAN_POINT ( 'NONE',  ( 1.404199475065617708, -0.004921259842519870586, -0.3153832671262229437 ) ) ;
#76704 = CARTESIAN_POINT ( 'NONE',  ( 0.3917322834645669549, 0.1049643490035304660, -1.311679790026246906 ) ) ;
#76705 = CARTESIAN_POINT ( 'NONE',  ( -0.3458507752293906723, -0.3458507752293910609, -0.2933070866141732069 ) ) ;
#76706 = CARTESIAN_POINT ( 'NONE',  ( 1.450131233595801428, -0.5511811023622048555, -0.09757992244046775898 ) ) ;
#76707 = CARTESIAN_POINT ( 'NONE',  ( -1.568241469816272105, -0.3162353388693409650, -0.4822834645669289433 ) ) ;
#76708 = CARTESIAN_POINT ( 'NONE',  ( -9.674558042662122972E-17, 0.3949938075777409963, 0.2381889763779528046 ) ) ;
#76709 = CARTESIAN_POINT ( 'NONE',  ( 0.5905511811023629321, -0.6692913385826771977, 8.415575281601705876E-17 ) ) ;
#76710 = CARTESIAN_POINT ( 'NONE',  ( -1.312335958005248715, 0.2306618581243848609, 0.2411417322834645549 ) ) ;
#76711 = CARTESIAN_POINT ( 'NONE',  ( -1.062992125984250968, 0.2952755905511811885, 0.000000000000000000 ) ) ;
#76712 = CARTESIAN_POINT ( 'NONE',  ( 0.2559055118110243332, -0.5400638737290845981, -0.3530559997133363437 ) ) ;
#76713 = CARTESIAN_POINT ( 'NONE',  ( -0.1058382717557503072, 0.3949938075777408852, -0.08333333333333334259 ) ) ;
#76714 = CARTESIAN_POINT ( 'NONE',  ( -1.482939632545930975, -0.004921259842519576551, 0.3153832671262227771 ) ) ;
#76715 = CARTESIAN_POINT ( 'NONE',  ( 0.8923884514435701520, -0.6046776061558809534, -0.2411417322834644161 ) ) ;
#76716 = CARTESIAN_POINT ( 'NONE',  ( 1.371391076115485941, 0.1771653543307087630, 0.09757992244046791164 ) ) ;
#76717 = CARTESIAN_POINT ( 'NONE',  ( -0.1958661417322834220, -0.3392501089628018884, -2.669947506561679784 ) ) ;
#76718 = CONTEXT_DEPENDENT_SHAPE_REPRESENTATION ( #34199, #47342 ) ;
#76719 = CARTESIAN_POINT ( 'NONE',  ( 0.6627296587926517768, -0.5511811023622048555, -0.09757992244046775898 ) ) ;
#76720 = CARTESIAN_POINT ( 'NONE',  ( -1.102362204724408601, -0.1870078740157480879, -0.4822834645669291653 ) ) ;
#76721 = CARTESIAN_POINT ( 'NONE',  ( 0.1070741851644054776, -0.3996062992125984925, -1.106955380577427706 ) ) ;
#76722 = CARTESIAN_POINT ( 'NONE',  ( 1.384514435695538559, 0.2952755905511810774, -0.1292274648535930714 ) ) ;
#76723 = CARTESIAN_POINT ( 'NONE',  ( 0.3917322834645670104, -0.1049643490035303411, -0.1036745406824146343 ) ) ;
#76725 = CARTESIAN_POINT ( 'NONE',  ( -0.2510736293007193032, 1.134572453438778883, 1.915946413328042386 ) ) ;
#76724 = CARTESIAN_POINT ( 'NONE',  ( 0.6167979002624679463, 0.05413385826771626580, -0.4176697321401330321 ) ) ;
#76726 = CARTESIAN_POINT ( 'NONE',  ( -1.660104986876639543, -0.08942795157528024563, -0.3641732283464568787 ) ) ;
#76727 = CARTESIAN_POINT ( 'NONE',  ( -0.1049868766404193215, -0.6046776061558807314, 0.2411417322834647770 ) ) ;
#76728 = CARTESIAN_POINT ( 'NONE',  ( 0.8661417322834652488, -0.1870078740157480601, -0.3641732283464567677 ) ) ;
#76729 = CARTESIAN_POINT ( 'NONE',  ( 0.9055118110236227702, 0.2952755905511811885, 0.000000000000000000 ) ) ;
#76730 = DIRECTION ( 'NONE',  ( 3.552713678800500929E-15, 0.000000000000000000, 1.000000000000000000 ) ) ;
#76731 = CARTESIAN_POINT ( 'NONE',  ( -0.7020997375328076329, -0.2845877964562161244, -0.3641732283464567121 ) ) ;
#76732 = CARTESIAN_POINT ( 'NONE',  ( -0.6561679790026240244, -0.6046776061558807314, 0.2411417322834647770 ) ) ;
#76733 = CARTESIAN_POINT ( 'NONE',  ( 1.587926509186352586, -0.4281496062992127816, -0.4176697321401328100 ) ) ;
#76734 = EDGE_CURVE ( 'NONE', #5577, #17151, #43693, .T. ) ;
#76735 = CARTESIAN_POINT ( 'NONE',  ( -1.082677165354329896, 0.1660481256975885056, 0.3530559997133364547 ) ) ;
#76736 = AXIS2_PLACEMENT_3D ( 'NONE', #68934, #69759, #75261 ) ;
#76737 = CARTESIAN_POINT ( 'NONE',  ( 1.003937007874016407, -0.5400638737290844871, 0.3530559997133364547 ) ) ;
#76738 = CARTESIAN_POINT ( 'NONE',  ( 0.3392501089628018329, 0.1958661417322835607, -0.7578933315298707063 ) ) ;
#76739 = CARTESIAN_POINT ( 'NONE',  ( -1.496062992125983815, -0.1870078740157479769, 0.3641732283464567677 ) ) ;
#76740 = DIRECTION ( 'NONE',  ( 0.000000000000000000, 0.000000000000000000, -1.000000000000000000 ) ) ;
#76741 = CARTESIAN_POINT ( 'NONE',  ( 1.017060367454068581, -0.05778040916215560624, -0.4822834645669293319 ) ) ;
#76742 = CARTESIAN_POINT ( 'NONE',  ( -0.2362204724409447953, -0.4091458600556404646, -2.504593175853018661 ) ) ;
#76743 = CARTESIAN_POINT ( 'NONE',  ( 0.9285414500055709786, 2.165354330708662012, 0.6299212598425202314 ) ) ;
#76744 = CARTESIAN_POINT ( 'NONE',  ( -1.338582677165353729, -0.1870078740157479769, 0.3641732283464567677 ) ) ;
#76745 = CARTESIAN_POINT ( 'NONE',  ( -1.213910761154854745, 0.1771653543307087075, -0.09757992244046823083 ) ) ;
#76746 = CARTESIAN_POINT ( 'NONE',  ( 1.568241469816273659, -0.08942795157528024563, -0.3641732283464568787 ) ) ;
#76747 = CARTESIAN_POINT ( 'NONE',  ( -0.1968503937007867743, 0.2952755905511811885, 0.000000000000000000 ) ) ;
#76748 = CARTESIAN_POINT ( 'NONE',  ( -0.3543307086614165824, 0.1771653543307087630, 0.000000000000000000 ) ) ;
#76749 = FACE_OUTER_BOUND ( 'NONE', #46971, .T. ) ;
#76750 = CARTESIAN_POINT ( 'NONE',  ( 1.082677165354331228, -0.4536011799217367080, 0.2665933059059888421 ) ) ;
#76751 = CARTESIAN_POINT ( 'NONE',  ( 0.9317585301837276734, 0.05413385826771626580, -0.4176697321401330321 ) ) ;
#76752 = CARTESIAN_POINT ( 'NONE',  ( 0.000000000000000000, 2.755905511811024056, 0.000000000000000000 ) ) ;
#76753 = CARTESIAN_POINT ( 'NONE',  ( -0.006561679790025524116, -0.08942795157528024563, -0.3641732283464568787 ) ) ;
#76754 = CARTESIAN_POINT ( 'NONE',  ( 0.4658792650918641698, -0.05778040916215560624, -0.4822834645669293319 ) ) ;
#76755 = CARTESIAN_POINT ( 'NONE',  ( 0.5314960629921264834, 0.07958543189024071263, -0.2665933059059888421 ) ) ;
#76756 = CARTESIAN_POINT ( 'NONE',  ( 1.450131233595801428, 0.2952755905511811885, 0.1292274648535926551 ) ) ;
#76757 = EDGE_CURVE ( 'NONE', #50071, #80735, #18060, .T. ) ;
#76758 = CARTESIAN_POINT ( 'NONE',  ( -1.463254593175852492, 0.2952755905511811885, 0.1292274648535926551 ) ) ;
#76759 = CARTESIAN_POINT ( 'NONE',  ( -0.4330708661417315697, 0.2952755905511811885, 0.000000000000000000 ) ) ;
#76760 = CARTESIAN_POINT ( 'NONE',  ( -0.3996062992125986590, 0.1070741851644051862, -0.5052493438320209140 ) ) ;
#76761 = CARTESIAN_POINT ( 'NONE',  ( -0.2925321140481932369, 0.2925321140481931259, -2.616141732283464805 ) ) ;
#76762 = CARTESIAN_POINT ( 'NONE',  ( 0.4790026246719167324, -0.05778040916215522460, 0.4822834645669289988 ) ) ;
#76763 = CARTESIAN_POINT ( 'NONE',  ( 1.253280839895013710, -0.2845877964562159024, 0.3641732283464567677 ) ) ;
#76764 = CARTESIAN_POINT ( 'NONE',  ( -0.5314960629921250401, 0.1660481256975885056, 0.3530559997133364547 ) ) ;
#76765 = CARTESIAN_POINT ( 'NONE',  ( 0.4265091863517067039, -0.6692913385826773087, -0.1292274648535924053 ) ) ;
#76766 = CARTESIAN_POINT ( 'NONE',  ( -9.787531504996567848E-17, 0.3996062992125986035, -2.204724409448818978 ) ) ;
#76767 = CARTESIAN_POINT ( 'NONE',  ( 0.1058382717557499880, 0.3949938075777411073, -1.410761154855643351 ) ) ;
#76768 = CARTESIAN_POINT ( 'NONE',  ( 0.2925321140481932369, 0.2925321140481932369, -2.814960629921259727 ) ) ;
#76769 = CARTESIAN_POINT ( 'NONE',  ( -0.1958661417322836718, 0.3392501089628017219, -1.107611548556430403 ) ) ;
#76770 = CARTESIAN_POINT ( 'NONE',  ( -1.135170603674539924, -0.5511811023622046335, 0.09757992244046803654 ) ) ;
#76771 = CARTESIAN_POINT ( 'NONE',  ( -1.056430446194224881, 0.2952755905511810774, -0.1292274648535930714 ) ) ;
#76772 = CARTESIAN_POINT ( 'NONE',  ( -0.2891555358219911054, 0.2891555358219909388, -2.616141732283464805 ) ) ;
#76773 = CARTESIAN_POINT ( 'NONE',  ( 1.043307086614173818, 0.1660481256975885056, 0.3530559997133364547 ) ) ;
#76774 = CARTESIAN_POINT ( 'NONE',  ( 1.443569553805774897, 0.2306618581243848609, 0.2411417322834645549 ) ) ;
#76775 = CARTESIAN_POINT ( 'NONE',  ( 0.6496062992125991586, 0.1660481256975885056, 0.3530559997133364547 ) ) ;
#76776 = CARTESIAN_POINT ( 'NONE',  ( 0.3458507752293908943, 0.3458507752293908943, -0.05708661417322836301 ) ) ;
#76777 = CARTESIAN_POINT ( 'NONE',  ( -0.3460692066303958092, -0.1998031496062994683, -2.099737532808398921 ) ) ;
#76778 = CARTESIAN_POINT ( 'NONE',  ( 1.528871391076116026, 0.2952755905511811885, 0.1292274648535926551 ) ) ;
#76779 = CARTESIAN_POINT ( 'NONE',  ( 0.4068241469816279987, -0.4281496062992127816, -0.4176697321401328100 ) ) ;
#76780 = CARTESIAN_POINT ( 'NONE',  ( 0.6233595800524939223, -0.3162353388693405765, 0.4822834645669290543 ) ) ;
#76781 = CARTESIAN_POINT ( 'NONE',  ( 1.023622047244095112, -0.1870078740157480601, -0.3641732283464567677 ) ) ;
#76782 = CARTESIAN_POINT ( 'NONE',  ( 1.299212598425197429, -0.6692913385826771977, 8.415575281601705876E-17 ) ) ;
#76783 = CARTESIAN_POINT ( 'NONE',  ( -0.3917322834645669549, -0.1049643490035306603, -0.1305774278215224293 ) ) ;
#76784 = CARTESIAN_POINT ( 'NONE',  ( 0.3083989501312343062, -0.3162353388693405765, 0.4822834645669290543 ) ) ;
#76785 = CARTESIAN_POINT ( 'NONE',  ( 1.213910761154856299, 0.2952755905511811885, 0.1292274648535926551 ) ) ;
#76786 = CARTESIAN_POINT ( 'NONE',  ( 0.3805774278215230400, -0.4281496062992124485, 0.4176697321401328655 ) ) ;
#76787 = CARTESIAN_POINT ( 'NONE',  ( 1.299212598425197429, -0.5511811023622047445, 6.969142054262312111E-17 ) ) ;
#76788 = CARTESIAN_POINT ( 'NONE',  ( -0.7874015748031489847, -0.1870078740157479769, 0.4822834645669291653 ) ) ;
#76789 = CARTESIAN_POINT ( 'NONE',  ( -1.076115485564303809, 0.2306618581243848609, 0.2411417322834645549 ) ) ;
#76790 = CIRCLE ( 'NONE', #48551, 2.204724409448819422 ) ;
#76791 = CARTESIAN_POINT ( 'NONE',  ( 1.345144356955381593, -0.3162353388693409650, -0.4822834645669289433 ) ) ;
#76792 = CARTESIAN_POINT ( 'NONE',  ( -0.1049643490035307020, 0.3917322834645669549, -0.5636482939632546652 ) ) ;
#76793 = CARTESIAN_POINT ( 'NONE',  ( -0.3392501089628019995, 0.1958661417322832277, -1.435695538057742970 ) ) ;
#76794 = CARTESIAN_POINT ( 'NONE',  ( -9.594673741351313045E-17, 0.3917322834645670104, -2.669291338582676865 ) ) ;
#76795 = EDGE_LOOP ( 'NONE', ( #11767, #39938, #29246, #37841 ) ) ;
#76796 = CARTESIAN_POINT ( 'NONE',  ( 0.3460692066303959202, 0.1998031496062993295, 0.02624671916010496570 ) ) ;
#76797 = VERTEX_POINT ( 'NONE', #42877 ) ;
#76798 = CARTESIAN_POINT ( 'NONE',  ( 1.686351706036745890, 0.2952755905511811885, 0.1292274648535926551 ) ) ;
#76799 = CARTESIAN_POINT ( 'NONE',  ( 1.266404199475066328, -0.08942795157527998196, 0.3641732283464567121 ) ) ;
#76800 = CARTESIAN_POINT ( 'NONE',  ( 0.1070741851644053527, 0.3996062992125986590, -1.410761154855643129 ) ) ;
#76801 = CARTESIAN_POINT ( 'NONE',  ( 1.332020997375329197, -0.2845877964562159024, 0.3641732283464567677 ) ) ;
#76802 = CARTESIAN_POINT ( 'NONE',  ( 0.6175017169405826456, 2.784432375088962958E-17, -0.3464511005275205946 ) ) ;
#76803 = CARTESIAN_POINT ( 'NONE',  ( -0.1181102362204717315, 0.2952755905511811885, 0.000000000000000000 ) ) ;
#76804 = CARTESIAN_POINT ( 'NONE',  ( 0.3893108287682404134, -0.05073257145186561845, -1.929133858267715773 ) ) ;
#76805 = CARTESIAN_POINT ( 'NONE',  ( -0.2867679344610364334, -0.2867679344610367109, -0.7736220472440945573 ) ) ;
#76806 = CARTESIAN_POINT ( 'NONE',  ( -0.7283464566929126471, -0.4536011799217367080, 0.2665933059059888421 ) ) ;
#76807 = FACE_OUTER_BOUND ( 'NONE', #32684, .T. ) ;
#76808 = CARTESIAN_POINT ( 'NONE',  ( -1.377952755905511140, -0.6692913385826771977, 8.415575281601705876E-17 ) ) ;
#76809 = CARTESIAN_POINT ( 'NONE',  ( 0.2559055118110243332, -0.5400638737290845981, -0.3530559997133363437 ) ) ;
#76810 = CARTESIAN_POINT ( 'NONE',  ( 1.397637795275591177, -0.5400638737290844871, 0.3530559997133364547 ) ) ;
#76811 = ORIENTED_EDGE ( 'NONE', *, *, #17436, .T. ) ;
#76812 = DIRECTION ( 'NONE',  ( -3.491481338843133355E-15, -0.000000000000000000, 1.000000000000000000 ) ) ;
#76813 = CARTESIAN_POINT ( 'NONE',  ( 0.3458507752293908943, -0.3458507752293908943, -2.145669291338581974 ) ) ;
#76814 = CARTESIAN_POINT ( 'NONE',  ( 0.2362204724409449064, 0.4091458600556404646, -2.664041994750656173 ) ) ;
#76815 = CARTESIAN_POINT ( 'NONE',  ( -0.4986876640419939388, 0.1283753931104746893, -0.1820866141732285504 ) ) ;
#76816 = CARTESIAN_POINT ( 'NONE',  ( -1.108923884514435132, -0.05778040916215560624, -0.4822834645669293319 ) ) ;
#76817 = CARTESIAN_POINT ( 'NONE',  ( 0.8792650918635177559, 0.05413385826771666132, 0.4176697321401328100 ) ) ;
#76818 = ORIENTED_EDGE ( 'NONE', *, *, #2159, .T. ) ;
#76820 = CARTESIAN_POINT ( 'NONE',  ( 0.6958886929845793379, 0.004960608223781096116, -0.3437734562760177970 ) ) ;
#76819 = CARTESIAN_POINT ( 'NONE',  ( 0.6299212598424790421, 2.165354330708661568, 3.886287458032468667 ) ) ;
#76821 = CARTESIAN_POINT ( 'NONE',  ( 1.043307086614173818, 0.1660481256975885056, 0.3530559997133364547 ) ) ;
#76822 = CARTESIAN_POINT ( 'NONE',  ( -1.174540682414697335, -0.3162353388693409650, -0.4822834645669289433 ) ) ;
#76823 = CARTESIAN_POINT ( 'NONE',  ( -0.3917322834645668994, -0.1049643490035306742, -0.9133665109898146950 ) ) ;
#76824 = CARTESIAN_POINT ( 'NONE',  ( -0.5577427821522301654, -0.08942795157528024563, -0.3641732283464568787 ) ) ;
#76825 = CARTESIAN_POINT ( 'NONE',  ( -0.3917322834645669549, -0.1049643490035306603, -0.7604986876640419391 ) ) ;
#76826 = CARTESIAN_POINT ( 'NONE',  ( -0.4593175853018364174, -0.3690944881889765550, -0.3153832671262227771 ) ) ;
#76827 = CARTESIAN_POINT ( 'NONE',  ( 0.2427821522309716595, -0.2845877964562161244, -0.3641732283464567121 ) ) ;
#76828 = EDGE_CURVE ( 'NONE', #77301, #48318, #55542, .T. ) ;
#76829 = CARTESIAN_POINT ( 'NONE',  ( -0.01312335958005186876, -0.4281496062992124485, 0.4176697321401328655 ) ) ;
#76830 = CARTESIAN_POINT ( 'NONE',  ( -1.135170603674539924, 0.1771653543307087075, -0.09757992244046823083 ) ) ;
#76831 = CARTESIAN_POINT ( 'NONE',  ( 0.1958661417322834775, 0.3392501089628018884, -2.656167979002624691 ) ) ;
#76832 = CARTESIAN_POINT ( 'NONE',  ( 1.115485564304462551, 0.05413385826771666132, 0.4176697321401328100 ) ) ;
#76833 = CARTESIAN_POINT ( 'NONE',  ( -1.246719160104985846, -0.4281496062992127816, -0.4176697321401328100 ) ) ;
#76834 = CARTESIAN_POINT ( 'NONE',  ( -0.3458507752293909498, 0.3458507752293907833, -1.198818897637795367 ) ) ;
#76835 = CARTESIAN_POINT ( 'NONE',  ( -0.2034120734908131112, -0.6692913385826773087, -0.1292274648535924053 ) ) ;
#76836 = CARTESIAN_POINT ( 'NONE',  ( -0.8333333333333323711, 0.2952755905511811885, 0.1292274648535926551 ) ) ;
#76837 = CARTESIAN_POINT ( 'NONE',  ( 0.6496062992125991586, -0.4536011799217368745, -0.2665933059059886201 ) ) ;
#76838 = CARTESIAN_POINT ( 'NONE',  ( -0.1443569553805768291, -0.004921259842519576551, 0.3153832671262227771 ) ) ;
#76839 = CARTESIAN_POINT ( 'NONE',  ( -0.6364829396325453192, -0.3162353388693405765, 0.4822834645669290543 ) ) ;
#76840 = CARTESIAN_POINT ( 'NONE',  ( -1.312335958005248715, 0.2306618581243848609, 0.2411417322834645549 ) ) ;
#76841 = DIRECTION ( 'NONE',  ( 1.000000000000000000, 0.000000000000000000, 0.000000000000000000 ) ) ;
#76842 = CARTESIAN_POINT ( 'NONE',  ( 1.266404199475066328, -0.2845877964562161244, -0.3641732283464567121 ) ) ;
#76843 = CARTESIAN_POINT ( 'NONE',  ( -0.06561679790026180015, 0.05413385826771666132, 0.4176697321401328100 ) ) ;
#76844 = CARTESIAN_POINT ( 'NONE',  ( -1.587926509186350810, -0.4281496062992124485, 0.4176697321401328655 ) ) ;
#76845 = ORIENTED_EDGE ( 'NONE', *, *, #63016, .T. ) ;
#76846 = CARTESIAN_POINT ( 'NONE',  ( -0.1998031496062991630, -0.3460692066303959202, -2.347112860892388575 ) ) ;
#76847 = ADVANCED_FACE ( 'NONE', ( #82443 ), #31390, .T. ) ;
#76848 = CARTESIAN_POINT ( 'NONE',  ( -0.8070866141732276899, 0.07958543189024071263, -0.2665933059059888421 ) ) ;
#76849 = CARTESIAN_POINT ( 'NONE',  ( 0.6496062992125991586, 0.1660481256975885056, 0.3530559997133364547 ) ) ;
#76850 = CARTESIAN_POINT ( 'NONE',  ( -0.9120734908136475250, 0.1771653543307087630, 0.09757992244046791164 ) ) ;
#76851 = CARTESIAN_POINT ( 'NONE',  ( -0.2925321140481932369, 0.2925321140481931259, -1.198818897637795367 ) ) ;
#76852 = CARTESIAN_POINT ( 'NONE',  ( -1.148293963254592542, -0.6692913385826773087, -0.1292274648535924053 ) ) ;
#76853 = CARTESIAN_POINT ( 'NONE',  ( 0.7742782152230979209, 0.05413385826771626580, -0.4176697321401330321 ) ) ;
#76854 = CARTESIAN_POINT ( 'NONE',  ( 0.6692913385826778638, -0.6692913385826771977, 8.415575281601705876E-17 ) ) ;
#76855 = EDGE_CURVE ( 'NONE', #36505, #62181, #63162, .T. ) ;
#76856 = CARTESIAN_POINT ( 'NONE',  ( 1.450131233595801428, 0.2952755905511811885, 0.1292274648535926551 ) ) ;
#76857 = CARTESIAN_POINT ( 'NONE',  ( -1.437007874015747477, -0.4536011799217367080, 0.2665933059059888421 ) ) ;
#76858 = CARTESIAN_POINT ( 'NONE',  ( -0.2925321140481932369, 0.2925321140481930704, -0.5688976377952755792 ) ) ;
#76859 = CARTESIAN_POINT ( 'NONE',  ( -0.3996062992125986035, -7.340648628747425578E-17, -0.9842519685039369248 ) ) ;
#76860 = CARTESIAN_POINT ( 'NONE',  ( 0.3949938075777409408, 0.1058382717557500574, -0.2821522309711286813 ) ) ;
#76861 = PRODUCT_RELATED_PRODUCT_CATEGORY ( 'part', '', ( #59425 ) ) ;
#76862 = CARTESIAN_POINT ( 'NONE',  ( 0.4732338166265936397, 1.502938029856536684, 2.557145251749653347 ) ) ;
#76863 = CARTESIAN_POINT ( 'NONE',  ( 1.108923884514436686, -0.2845877964562161244, -0.3641732283464567121 ) ) ;
#76864 = CARTESIAN_POINT ( 'NONE',  ( 0.5839895013123367340, -0.5511811023622048555, -0.09757992244046775898 ) ) ;
#76865 = CARTESIAN_POINT ( 'NONE',  ( 0.04593175853018440641, 0.2952755905511810774, -0.1292274648535930714 ) ) ;
#76866 = CARTESIAN_POINT ( 'NONE',  ( -0.4724409448818896462, -0.1265901696524993070, -2.327427821522309426 ) ) ;
#76867 = CARTESIAN_POINT ( 'NONE',  ( 0.1058382717557499880, 0.3949938075777409408, -1.172572178477690574 ) ) ;
#76868 = CARTESIAN_POINT ( 'NONE',  ( 0.2493438320209980519, -0.004921259842519576551, 0.3153832671262227771 ) ) ;
#76869 = CARTESIAN_POINT ( 'NONE',  ( -0.5511811023622038563, -0.1870078740157479769, 0.4822834645669291653 ) ) ;
#76870 = CARTESIAN_POINT ( 'NONE',  ( -1.384514435695537005, -0.6692913385826773087, -0.1292274648535924053 ) ) ;
#76871 = CARTESIAN_POINT ( 'NONE',  ( 0.7020997375328090762, -0.3162353388693405765, 0.4822834645669290543 ) ) ;
#76872 = CARTESIAN_POINT ( 'NONE',  ( -0.1265901696524993347, 0.4724409448818895907, -1.581364829396325389 ) ) ;
#76873 = B_SPLINE_CURVE_WITH_KNOTS ( 'NONE', 3,
 ( #70084, #63771, #12437, #5696 ),
 .UNSPECIFIED., .F., .F.,
 ( 4, 4 ),
 ( 3.210432057725814518E-07, 0.001287787053612007718 ),
 .UNSPECIFIED. ) ;
#76874 = DIRECTION ( 'NONE',  ( 0.000000000000000000, 0.000000000000000000, 1.000000000000000000 ) ) ;
#76875 = ADVANCED_FACE ( 'NONE', ( #23944 ), #8535, .F. ) ;
#76876 = ORIENTED_EDGE ( 'NONE', *, *, #14394, .T. ) ;
#76877 = VERTEX_POINT ( 'NONE', #12153 ) ;
#76878 = CARTESIAN_POINT ( 'NONE',  ( -1.200787401574802349, 0.1660481256975883668, -0.3530559997133364547 ) ) ;
#76879 = CARTESIAN_POINT ( 'NONE',  ( -0.7611548556430438595, -0.6046776061558809534, -0.2411417322834644161 ) ) ;
#76881 = CARTESIAN_POINT ( 'NONE',  ( -0.7808398950131222316, -0.3162353388693409650, -0.4822834645669289433 ) ) ;
#76880 = CARTESIAN_POINT ( 'NONE',  ( -0.6102362204724400829, -0.4536011799217368745, -0.2665933059059886201 ) ) ;
#76882 = CARTESIAN_POINT ( 'NONE',  ( 4.797336870675655290E-17, -0.3917322834645669549, -1.891056799703724645 ) ) ;
#76884 = EDGE_CURVE ( 'NONE', #4806, #39221, #48101, .T. ) ;
#76883 = CARTESIAN_POINT ( 'NONE',  ( 0.3460692066303959202, -0.1998031496062991630, -2.858923884514435798 ) ) ;
#76885 = CARTESIAN_POINT ( 'NONE',  ( 1.450131233595801428, -0.6692913385826773087, -0.1292274648535924053 ) ) ;
#76886 = CARTESIAN_POINT ( 'NONE',  ( -0.6430446194225716283, -0.4281496062992124485, 0.4176697321401328655 ) ) ;
#76887 = CARTESIAN_POINT ( 'NONE',  ( 0.3674540682414705883, 0.2306618581243847221, -0.2411417322834647770 ) ) ;
#76888 = CARTESIAN_POINT ( 'NONE',  ( -0.7217847769028863381, -0.4281496062992124485, 0.4176697321401328655 ) ) ;
#76889 = CARTESIAN_POINT ( 'NONE',  ( 0.2867679344610365999, 0.2867679344610365999, -1.389763779527558807 ) ) ;
#76890 = CARTESIAN_POINT ( 'NONE',  ( -0.9973753280839886548, 0.1283753931104748280, 0.1820866141732283561 ) ) ;
#76891 = ORIENTED_EDGE ( 'NONE', *, *, #80504, .F. ) ;
#76892 = CARTESIAN_POINT ( 'NONE',  ( -0.3949938075777409963, -7.255918531996591613E-17, -1.771653543307086576 ) ) ;
#76893 = ORIENTED_EDGE ( 'NONE', *, *, #19084, .T. ) ;
#76894 = PLANE ( 'NONE',  #5919 ) ;
#76895 = CARTESIAN_POINT ( 'NONE',  ( -1.056430446194224881, -0.6692913385826771977, 0.1292274648535927661 ) ) ;
#76896 = CARTESIAN_POINT ( 'NONE',  ( -0.8923884514435688198, -0.6046776061558807314, 0.2411417322834647770 ) ) ;
#76897 = CARTESIAN_POINT ( 'NONE',  ( 0.2925321140481932369, -0.2925321140481932369, -0.2559055118110235560 ) ) ;
#76898 = CARTESIAN_POINT ( 'NONE',  ( -1.227034120734907585, 0.2952755905511811885, 0.1292274648535926551 ) ) ;
#76899 = CARTESIAN_POINT ( 'NONE',  ( -1.154855643044618851, -0.6046776061558809534, -0.2411417322834644161 ) ) ;
#76900 = CARTESIAN_POINT ( 'NONE',  ( -1.633858267716534529, 0.1660481256975885056, 0.3530559997133364547 ) ) ;
#76901 = CARTESIAN_POINT ( 'NONE',  ( 0.5314960629920847390, 2.559055118110236560, 3.937007874015794773 ) ) ;
#76902 = CARTESIAN_POINT ( 'NONE',  ( 0.7086614173228353852, -0.1870078740157479769, 0.3641732283464567677 ) ) ;
#76903 = CARTESIAN_POINT ( 'NONE',  ( 1.141392835773559211, 0.4110443821404751730, 1.141392835773562764 ) ) ;
#76904 = CARTESIAN_POINT ( 'NONE',  ( 0.1958661417322836440, -0.3392501089628017219, -0.4914698162729659869 ) ) ;
#76905 = CARTESIAN_POINT ( 'NONE',  ( -0.2952755905511804668, 0.07958543189024085140, 0.2665933059059887866 ) ) ;
#76906 = CARTESIAN_POINT ( 'NONE',  ( -0.9711286089238838626, 0.2306618581243847221, -0.2411417322834647770 ) ) ;
#76907 = CARTESIAN_POINT ( 'NONE',  ( 1.423884514435696191, -0.05778040916215522460, 0.4822834645669289988 ) ) ;
#76908 = CARTESIAN_POINT ( 'NONE',  ( -0.3543307086614165824, 0.2952755905511811885, 0.000000000000000000 ) ) ;
#76909 = ORIENTED_EDGE ( 'NONE', *, *, #4894, .T. ) ;
#76910 = EDGE_LOOP ( 'NONE', ( #64349, #77267 ) ) ;
#76911 = CARTESIAN_POINT ( 'NONE',  ( -0.1070741851644051862, -0.3996062992125986590, -1.881233595800524849 ) ) ;
#76913 = AXIS2_PLACEMENT_3D ( 'NONE', #37108, #9793, #80925 ) ;
#76912 = CARTESIAN_POINT ( 'NONE',  ( -0.9973753280839886548, 0.2306618581243848609, 0.2411417322834645549 ) ) ;
#76914 = CARTESIAN_POINT ( 'NONE',  ( 1.476377952755906220, 0.1660481256975883668, -0.3530559997133364547 ) ) ;
#76915 = CARTESIAN_POINT ( 'NONE',  ( -1.325459317585300889, -0.3690944881889765550, -0.3153832671262227771 ) ) ;
#76916 = CARTESIAN_POINT ( 'NONE',  ( -1.246719160104986512, 0.05413385826771666132, 0.4176697321401328100 ) ) ;
#76917 = CARTESIAN_POINT ( 'NONE',  ( -0.2362204724409447953, -0.4091458600556404646, -1.010498687664042050 ) ) ;
#76918 = EDGE_CURVE ( 'NONE', #60631, #42276, #3178, .T. ) ;
#76919 = CARTESIAN_POINT ( 'NONE',  ( -0.7480314960629916854, 2.793565526369265584, 0.000000000000000000 ) ) ;
#76920 = CARTESIAN_POINT ( 'NONE',  ( 0.1958661417322834775, 0.3392501089628018884, 0.02099737532808403431 ) ) ;
#76921 = CARTESIAN_POINT ( 'NONE',  ( 0.1049643490035304799, -0.3917322834645669549, -2.059711286089238591 ) ) ;
#76922 = CARTESIAN_POINT ( 'NONE',  ( 0.06561679790026316017, -0.4281496062992124485, 0.4176697321401328655 ) ) ;
#76923 = CARTESIAN_POINT ( 'NONE',  ( -1.148293963254592542, 0.1771653543307087630, 0.09757992244046791164 ) ) ;
#76924 = CARTESIAN_POINT ( 'NONE',  ( -0.7020997375328076329, -0.3162353388693409650, -0.4822834645669289433 ) ) ;
#76925 = CARTESIAN_POINT ( 'NONE',  ( 0.4091458600556403535, 0.2362204724409449896, -2.570209973753280863 ) ) ;
#76926 = CARTESIAN_POINT ( 'NONE',  ( -1.220472440944881054, 0.2952755905511811885, 0.000000000000000000 ) ) ;
#76927 = CARTESIAN_POINT ( 'NONE',  ( -0.9776902887139098386, -0.6692913385826771977, 0.1292274648535927661 ) ) ;
#76928 = EDGE_CURVE ( 'NONE', #34363, #64782, #55097, .T. ) ;
#76929 = CARTESIAN_POINT ( 'NONE',  ( -0.1049868766404193215, 0.2306618581243847221, -0.2411417322834647770 ) ) ;
#76930 = CARTESIAN_POINT ( 'NONE',  ( 0.1058382717557500852, -0.3949938075777408852, -2.681758530183727451 ) ) ;
#76931 = CARTESIAN_POINT ( 'NONE',  ( 0.9776902887139113929, 0.1771653543307087630, 0.09757992244046791164 ) ) ;
#76932 = CARTESIAN_POINT ( 'NONE',  ( -0.5643044619422565855, -0.004921259842519870586, -0.3153832671262229437 ) ) ;
#76933 = CARTESIAN_POINT ( 'NONE',  ( 0.6102362204724416372, 0.07958543189024071263, -0.2665933059059888421 ) ) ;
#76934 = CARTESIAN_POINT ( 'NONE',  ( 1.345144356955381593, -0.2845877964562161244, -0.3641732283464567121 ) ) ;
#76935 = CARTESIAN_POINT ( 'NONE',  ( 1.259842519685040019, -0.1870078740157479769, 0.4822834645669291653 ) ) ;
#76936 = CARTESIAN_POINT ( 'NONE',  ( 0.5314960629921267055, -0.4536011799217367080, 0.2665933059059888421 ) ) ;
#76937 = CARTESIAN_POINT ( 'NONE',  ( 0.2867679344610365999, 0.2867679344610365999, -1.389763779527558807 ) ) ;
#76938 = CARTESIAN_POINT ( 'NONE',  ( -0.7611548556430438595, -0.6046776061558809534, -0.2411417322834644161 ) ) ;
#76939 = CARTESIAN_POINT ( 'NONE',  ( 1.043307086614173818, -0.5400638737290845981, -0.3530559997133363437 ) ) ;
#76940 =( BOUNDED_CURVE ( )  B_SPLINE_CURVE ( 1, ( #49893, #75999 ),
 .UNSPECIFIED., .F., .F. ) 
 B_SPLINE_CURVE_WITH_KNOTS ( ( 2, 2 ),
 ( 2.081668171172168513E-17, 0.001999999999999987899 ),
 .UNSPECIFIED. ) 
 CURVE ( )  GEOMETRIC_REPRESENTATION_ITEM ( )  RATIONAL_B_SPLINE_CURVE ( ( 0.9875488213027535656, 0.9875488213027535656 ) ) 
 REPRESENTATION_ITEM ( '' )  );
#76941 = EDGE_CURVE ( 'NONE', #58371, #13764, #78234, .T. ) ;
#76942 = CARTESIAN_POINT ( 'NONE',  ( 0.1265901696524989462, 0.4724409448818897572, -0.07020997375328083545 ) ) ;
#76943 = CARTESIAN_POINT ( 'NONE',  ( -0.6364829396325453192, -0.08942795157528024563, -0.3641732283464568787 ) ) ;
#76944 = CARTESIAN_POINT ( 'NONE',  ( 0.06873123812453012238, 8.471767977567108961E-16, -0.4445507791589058955 ) ) ;
#76945 = CARTESIAN_POINT ( 'NONE',  ( 0.1902887139107617975, -0.6692913385826773087, -0.1292274648535924053 ) ) ;
#76946 = CARTESIAN_POINT ( 'NONE',  ( -0.3503937007874015630, -0.3733313776025731778, -0.01968503937007957602 ) ) ;
#76947 = CARTESIAN_POINT ( 'NONE',  ( 0.9120734908136489683, -0.5511811023622046335, 0.09757992244046803654 ) ) ;
#76948 = CARTESIAN_POINT ( 'NONE',  ( 0.07217847769028949700, -0.08942795157528024563, -0.3641732283464568787 ) ) ;
#76949 = CARTESIAN_POINT ( 'NONE',  ( 0.04593175853018440641, -0.6692913385826771977, 0.1292274648535927661 ) ) ;
#76950 = CARTESIAN_POINT ( 'NONE',  ( -1.292650918635170010, -0.6692913385826771977, 0.1292274648535927661 ) ) ;
#76951 = CARTESIAN_POINT ( 'NONE',  ( -0.7480314960629914633, -0.5511811023622047445, 6.969142054262312111E-17 ) ) ;
#76952 = DIRECTION ( 'NONE',  ( 0.000000000000000000, 0.000000000000000000, -1.000000000000000000 ) ) ;
#76953 = CARTESIAN_POINT ( 'NONE',  ( -0.5774278215223089816, -0.6046776061558807314, 0.2411417322834647770 ) ) ;
#76954 = CARTESIAN_POINT ( 'NONE',  ( 0.3460692066303959202, -0.1998031496062991630, -0.9691601049868766582 ) ) ;
#76955 = CARTESIAN_POINT ( 'NONE',  ( 0.3917322834645670104, -0.1049643490035303411, -2.085958005249344271 ) ) ;
#76956 = CARTESIAN_POINT ( 'NONE',  ( 0.2821522309711292364, -0.5511811023622046335, 0.09757992244046803654 ) ) ;
#76957 = CARTESIAN_POINT ( 'NONE',  ( -0.5511811023622038563, -0.1870078740157479769, 0.4822834645669291653 ) ) ;
#76958 = CARTESIAN_POINT ( 'NONE',  ( -1.036745406824146176, -0.4281496062992124485, 0.4176697321401328655 ) ) ;
#76959 = CARTESIAN_POINT ( 'NONE',  ( -1.259842519685038686, -0.1870078740157480601, -0.3641732283464567677 ) ) ;
#76960 = CARTESIAN_POINT ( 'NONE',  ( -3.934081685436475517, 1.087899594981445617, -0.1524895619889924669 ) ) ;
#76961 = CARTESIAN_POINT ( 'NONE',  ( -0.5971128608923877978, -0.6692913385826773087, -0.1292274648535924053 ) ) ;
#76962 = CARTESIAN_POINT ( 'NONE',  ( -0.7480314960629914633, -0.5511811023622047445, 6.969142054262312111E-17 ) ) ;
#76963 = CARTESIAN_POINT ( 'NONE',  ( -1.384514435695537005, 0.1771653543307087630, 0.09757992244046791164 ) ) ;
#76964 = CARTESIAN_POINT ( 'NONE',  ( 1.141732283464567566, 0.2952755905511811885, 0.000000000000000000 ) ) ;
#76965 = CONICAL_SURFACE ( 'NONE', #62182, 65.61679790026244063, 1.030376826524312284 ) ;
#76966 = CARTESIAN_POINT ( 'NONE',  ( -0.1958661417322836995, 0.3392501089628017219, -1.899625614994437495 ) ) ;
#76967 = VERTEX_POINT ( 'NONE', #82852 ) ;
#76968 = CARTESIAN_POINT ( 'NONE',  ( -0.7480314960629922405, 1.900312960331933976, 0.000000000000000000 ) ) ;
#76969 = CARTESIAN_POINT ( 'NONE',  ( -1.541994750656167090, 0.2952755905511811885, 0.1292274648535926551 ) ) ;
#76970 = CARTESIAN_POINT ( 'NONE',  ( -1.082677165354329896, 0.1660481256975885056, 0.3530559997133364547 ) ) ;
#76971 = CARTESIAN_POINT ( 'NONE',  ( -1.469816272965878357, 0.2306618581243848609, 0.2411417322834645549 ) ) ;
#76972 = CARTESIAN_POINT ( 'NONE',  ( 4.797336870675656522E-17, -0.3917322834645670104, -2.053149606299212948 ) ) ;
#76973 = CARTESIAN_POINT ( 'NONE',  ( -0.3503937007874015630, -0.5120078740157480990, -0.4921259842519685179 ) ) ;
#76974 = CARTESIAN_POINT ( 'NONE',  ( 0.9711286089238851948, -0.6046776061558809534, -0.2411417322834644161 ) ) ;
#76975 = CARTESIAN_POINT ( 'NONE',  ( -0.05905511811023545637, 0.1660481256975885056, 0.3530559997133364547 ) ) ;
#76976 = LINE ( 'NONE', #38247, #38252 ) ;
#76977 = CARTESIAN_POINT ( 'NONE',  ( -0.9548908091195642545, -2.567464376874931580E-15, -0.4445507791589072832 ) ) ;
#76978 = CARTESIAN_POINT ( 'NONE',  ( 1.003937007874016185, 0.07958543189024071263, -0.2665933059059888421 ) ) ;
#76979 = EDGE_CURVE ( 'NONE', #34321, #65845, #42468, .T. ) ;
#76980 = CARTESIAN_POINT ( 'NONE',  ( -0.3996062992125986035, -7.340648628747425578E-17, -1.299212598425196985 ) ) ;
#76981 = ORIENTED_EDGE ( 'NONE', *, *, #75011, .F. ) ;
#76982 = CARTESIAN_POINT ( 'NONE',  ( 0.2867679344610366554, -0.2867679344610365999, 0.06231664222341019160 ) ) ;
#76983 = ORIENTED_EDGE ( 'NONE', *, *, #34274, .F. ) ;
#76984 = CARTESIAN_POINT ( 'NONE',  ( -0.04593175853018302557, -0.6692913385826773087, -0.1292274648535924053 ) ) ;
#76985 = CARTESIAN_POINT ( 'NONE',  ( -0.9383202099737524282, -0.05778040916215522460, 0.4822834645669289988 ) ) ;
#76986 = CARTESIAN_POINT ( 'NONE',  ( -1.463254593175852492, 0.2952755905511811885, 0.1292274648535926551 ) ) ;
#76987 = CARTESIAN_POINT ( 'NONE',  ( 0.8333333333333340365, -0.6692913385826771977, 0.1292274648535927661 ) ) ;
#76988 = CARTESIAN_POINT ( 'NONE',  ( -1.640419947506561060, -0.004921259842519576551, 0.3153832671262227771 ) ) ;
#76989 = CARTESIAN_POINT ( 'NONE',  ( 1.292650918635171564, 0.2952755905511811885, 0.1292274648535926551 ) ) ;
#76990 = CARTESIAN_POINT ( 'NONE',  ( -0.6430446194225712953, 0.05413385826771626580, -0.4176697321401330321 ) ) ;
#76991 = CARTESIAN_POINT ( 'NONE',  ( 0.4265091863517067039, -0.6692913385826773087, -0.1292274648535924053 ) ) ;
#76992 = CARTESIAN_POINT ( 'NONE',  ( 1.535433070866142335, -0.6692913385826771977, 8.415575281601705876E-17 ) ) ;
#76993 = CARTESIAN_POINT ( 'NONE',  ( 1.174540682414699111, -0.05778040916215560624, -0.4822834645669293319 ) ) ;
#76994 = CARTESIAN_POINT ( 'NONE',  ( 1.660104986876641320, -0.05778040916215522460, 0.4822834645669289988 ) ) ;
#76995 = CARTESIAN_POINT ( 'NONE',  ( -0.1902887139107604098, -0.6692913385826771977, 0.1292274648535927661 ) ) ;
#76996 = CARTESIAN_POINT ( 'NONE',  ( 0.3917322834645670104, 2.398668435337828261E-17, -0.2677165354330708347 ) ) ;
#76997 = CARTESIAN_POINT ( 'NONE',  ( 0.4527559055118117182, 0.07958543189024071263, -0.2665933059059888421 ) ) ;
#76998 = VERTEX_POINT ( 'NONE', #81214 ) ;
#76999 = CARTESIAN_POINT ( 'NONE',  ( 0.3949938075777411073, -0.1058382717557499464, -0.4265091863517062043 ) ) ;
#77000 = ORIENTED_EDGE ( 'NONE', *, *, #66685, .T. ) ;
#77001 = CARTESIAN_POINT ( 'NONE',  ( -0.4068241469816267775, -0.004921259842519870586, -0.3153832671262229437 ) ) ;
#77002 = DIRECTION ( 'NONE',  ( 0.000000000000000000, -1.000000000000000000, 0.000000000000000000 ) ) ;
#77003 = CARTESIAN_POINT ( 'NONE',  ( 0.1574803149606306130, -0.1870078740157479769, 0.4822834645669291653 ) ) ;
#77004 = CARTESIAN_POINT ( 'NONE',  ( 0.05905511811023681640, 0.1660481256975883668, -0.3530559997133364547 ) ) ;
#77005 = CARTESIAN_POINT ( 'NONE',  ( -0.7283464566929126471, 0.1660481256975883668, -0.3530559997133364547 ) ) ;
#77006 = CARTESIAN_POINT ( 'NONE',  ( -0.3917322834645670659, -7.196005306013484475E-17, -1.768392019193912423 ) ) ;
#77007 = CARTESIAN_POINT ( 'NONE',  ( -1.036745406824146176, -0.4281496062992124485, 0.4176697321401328655 ) ) ;
#77008 = CARTESIAN_POINT ( 'NONE',  ( -1.604771003085129655, 1.553800022087478805, -0.1466069496707747277 ) ) ;
#77009 = CARTESIAN_POINT ( 'NONE',  ( 1.089238845144357537, -0.3690944881889763329, 0.3153832671262228327 ) ) ;
#77010 = AXIS2_PLACEMENT_3D ( 'NONE', #13714, #34316, #47757 ) ;
#77011 = CARTESIAN_POINT ( 'NONE',  ( 0.5511811023622055217, -0.1870078740157479769, 0.4822834645669291653 ) ) ;
#77012 = CARTESIAN_POINT ( 'NONE',  ( 0.6824146981627303710, -0.6046776061558807314, 0.2411417322834647770 ) ) ;
#77013 = CARTESIAN_POINT ( 'NONE',  ( 0.2925321140481932369, -0.2925321140481932369, -1.358267716535433101 ) ) ;
#77014 = CARTESIAN_POINT ( 'NONE',  ( -1.476377952755905110, -0.5400638737290845981, -0.3530559997133363437 ) ) ;
#77015 = CARTESIAN_POINT ( 'NONE',  ( -0.3460692066303960313, 0.1998031496062989965, -0.7329396325459317518 ) ) ;
#77016 = CARTESIAN_POINT ( 'NONE',  ( 0.3996062992125986035, -0.1070741851644052972, -0.1883202099737532609 ) ) ;
#77017 = CARTESIAN_POINT ( 'NONE',  ( -0.1312335958005241554, 0.2306618581243848609, 0.2411417322834645549 ) ) ;
#77018 = CARTESIAN_POINT ( 'NONE',  ( -0.1070741851644051862, -0.3996062992125987146, -2.591863517060367439 ) ) ;
#77019 = CARTESIAN_POINT ( 'NONE',  ( -0.2867679344610365999, 0.2867679344610364889, -1.679133858267716661 ) ) ;
#77020 = CARTESIAN_POINT ( 'NONE',  ( -1.154855643044618851, 0.1283753931104748280, 0.1820866141732283561 ) ) ;
#77021 = CARTESIAN_POINT ( 'NONE',  ( 1.279527559055118724, 0.1660481256975885056, 0.3530559997133364547 ) ) ;
#77022 = CARTESIAN_POINT ( 'NONE',  ( 1.187664041994751285, -0.05778040916215522460, 0.4822834645669289988 ) ) ;
#77023 = CARTESIAN_POINT ( 'NONE',  ( 0.1574803149606306130, -0.1870078740157480601, -0.3641732283464567677 ) ) ;
#77024 = CARTESIAN_POINT ( 'NONE',  ( 0.5971128608923890191, -0.6692913385826771977, 0.1292274648535927661 ) ) ;
#77025 = CARTESIAN_POINT ( 'NONE',  ( -0.1265901696524993347, 0.4724409448818895907, -1.500656167979002031 ) ) ;
#77026 = CARTESIAN_POINT ( 'NONE',  ( 0.4461942257217856311, 0.1283753931104746893, -0.1820866141732285504 ) ) ;
#77027 = CARTESIAN_POINT ( 'NONE',  ( 0.2821522309711292364, -0.6692913385826771977, 0.1292274648535927661 ) ) ;
#77028 = AXIS2_PLACEMENT_3D ( 'NONE', #61854, #4195, #10527 ) ;
#77029 = CARTESIAN_POINT ( 'NONE',  ( 0.2891555358219910499, 0.2891555358219910499, -1.159448818897637956 ) ) ;
#77030 = CARTESIAN_POINT ( 'NONE',  ( -1.266404199475064773, -0.3162353388693405765, 0.4822834645669290543 ) ) ;
#77031 = CARTESIAN_POINT ( 'NONE',  ( 0.6364829396325465405, -0.08942795157527998196, 0.3641732283464567121 ) ) ;
#77032 = DIRECTION ( 'NONE',  ( -1.000000000000000000, -0.000000000000000000, -0.000000000000000000 ) ) ;
#77033 = CARTESIAN_POINT ( 'NONE',  ( -0.2034120734908131112, -0.6692913385826773087, -0.1292274648535924053 ) ) ;
#77034 = CARTESIAN_POINT ( 'NONE',  ( -0.2821522309711278487, -0.5511811023622048555, -0.09757992244046775898 ) ) ;
#77035 = CARTESIAN_POINT ( 'NONE',  ( 3.937007874015748143, 2.755905511811024056, -0.5314960629921260393 ) ) ;
#77036 = CARTESIAN_POINT ( 'NONE',  ( -0.1181102362204717315, 0.2952755905511811885, 0.000000000000000000 ) ) ;
#77037 = CARTESIAN_POINT ( 'NONE',  ( 0.3477690288713918276, 0.1771653543307087630, 0.09757992244046791164 ) ) ;
#77038 = CARTESIAN_POINT ( 'NONE',  ( 0.1070741851644054776, -0.3996062992125984925, -2.209317585301837639 ) ) ;
#77039 = CARTESIAN_POINT ( 'NONE',  ( 0.09842519685039434474, 0.1660481256975885056, 0.3530559997133364547 ) ) ;
#77040 = CARTESIAN_POINT ( 'NONE',  ( -0.2867679344610364334, -0.2867679344610368219, -1.713891445373016520 ) ) ;
#77041 = CARTESIAN_POINT ( 'NONE',  ( 1.154855643044620184, -0.5023911411419708095, 0.1820866141732285504 ) ) ;
#77042 = CARTESIAN_POINT ( 'NONE',  ( 0.1902887139107617975, 0.2952755905511811885, 0.1292274648535926551 ) ) ;
#77043 = CARTESIAN_POINT ( 'NONE',  ( -0.8595800524934373854, -0.2845877964562161244, -0.3641732283464567121 ) ) ;
#77044 = CARTESIAN_POINT ( 'NONE',  ( -0.5839895013123351797, 0.1771653543307087075, -0.09757992244046823083 ) ) ;
#77045 = CARTESIAN_POINT ( 'NONE',  ( -0.7545931758530176614, -0.6692913385826773087, -0.1292274648535924053 ) ) ;
#77046 = CARTESIAN_POINT ( 'NONE',  ( -0.07217847769028813698, -0.3162353388693409650, -0.4822834645669289433 ) ) ;
#77047 = CARTESIAN_POINT ( 'NONE',  ( 0.4199475065616805614, 0.1283753931104748280, 0.1820866141732283561 ) ) ;
#77048 = DIRECTION ( 'NONE',  ( 1.000000000000000000, 3.096699300667737464E-16, -1.692413147294446216E-16 ) ) ;
#77049 = CARTESIAN_POINT ( 'NONE',  ( 1.332020997375328974, -0.08942795157528024563, -0.3641732283464568787 ) ) ;
#77050 = CARTESIAN_POINT ( 'NONE',  ( 0.9251968503937015864, 0.1660481256975883668, -0.3530559997133364547 ) ) ;
#77051 = CARTESIAN_POINT ( 'NONE',  ( -0.2925321140481930149, -0.2925321140481933480, 0.1791338582677165503 ) ) ;
#77052 = CARTESIAN_POINT ( 'NONE',  ( -0.1312335958005241554, 0.2306618581243848609, 0.2411417322834645549 ) ) ;
#77053 = CARTESIAN_POINT ( 'NONE',  ( -0.3392501089628019995, 0.1958661417322832277, -1.055774278215223294 ) ) ;
#77054 = CARTESIAN_POINT ( 'NONE',  ( 1.463254593175853824, 0.1771653543307087075, -0.09757992244046823083 ) ) ;
#77055 = CARTESIAN_POINT ( 'NONE',  ( 0.7808398950131241190, -0.05778040916215560624, -0.4822834645669293319 ) ) ;
#77056 = CARTESIAN_POINT ( 'NONE',  ( 0.05249343832021075018, -0.6046776061558807314, 0.2411417322834647770 ) ) ;
#77057 = CARTESIAN_POINT ( 'NONE',  ( -0.3575644331232493700, 1.224046602586773336, -3.920799917772898713 ) ) ;
#77058 = CARTESIAN_POINT ( 'NONE',  ( 0.5511811023622055217, -0.1870078740157479769, 0.3641732283464567677 ) ) ;
#77059 = CARTESIAN_POINT ( 'NONE',  ( 0.7874015748031503170, -0.1870078740157480879, -0.4822834645669291653 ) ) ;
#77060 = CARTESIAN_POINT ( 'NONE',  ( -0.5118110236220466680, -0.5511811023622047445, 6.969142054262312111E-17 ) ) ;
#77061 = CARTESIAN_POINT ( 'NONE',  ( -0.5971128608923877978, -0.6692913385826773087, -0.1292274648535924053 ) ) ;
#77062 = CARTESIAN_POINT ( 'NONE',  ( 0.4724409448818915891, -0.1265901696524958653, -2.631233595800525293 ) ) ;
#77063 = CARTESIAN_POINT ( 'NONE',  ( 0.1640419947506569498, -0.05778040916215522460, 0.4822834645669289988 ) ) ;
#77064 = CARTESIAN_POINT ( 'NONE',  ( -1.371391076115484609, -0.6692913385826771977, 0.1292274648535927661 ) ) ;
#77065 = VECTOR ( 'NONE', #60909, 39.37007874015748143 ) ;
#77066 = CARTESIAN_POINT ( 'NONE',  ( -0.7611548556430438595, 0.1283753931104748280, 0.1820866141732283561 ) ) ;
#77067 = CARTESIAN_POINT ( 'NONE',  ( 0.1771653543307093182, 0.1660481256975885056, 0.3530559997133364547 ) ) ;
#77068 = CARTESIAN_POINT ( 'NONE',  ( -1.227034120734907585, 0.2952755905511811885, 0.1292274648535926551 ) ) ;
#77069 = CARTESIAN_POINT ( 'NONE',  ( -0.2034120734908128059, 0.2952755905511811885, 0.1292274648535926551 ) ) ;
#77071 = CARTESIAN_POINT ( 'NONE',  ( 1.272965879265092637, 0.05413385826771666132, 0.4176697321401328100 ) ) ;
#77070 = FACE_OUTER_BOUND ( 'NONE', #70057, .T. ) ;
#77072 = CARTESIAN_POINT ( 'NONE',  ( 1.456692913385827515, -0.6692913385826771977, 8.415575281601705876E-17 ) ) ;
#77073 = CARTESIAN_POINT ( 'NONE',  ( 0.1958661417322836440, -0.3392501089628017219, -2.603674540682414218 ) ) ;
#77074 = CARTESIAN_POINT ( 'NONE',  ( -1.528871391076114250, -0.6692913385826771977, 0.1292274648535927661 ) ) ;
#77075 = CARTESIAN_POINT ( 'NONE',  ( -0.9908136482939626788, -0.6692913385826773087, -0.1292274648535924053 ) ) ;
#77076 = CARTESIAN_POINT ( 'NONE',  ( 0.4724409448818896462, 0.1265901696524990294, -0.5971128608923884640 ) ) ;
#77077 = EDGE_CURVE ( 'NONE', #51714, #11621, #66326, .T. ) ;
#77078 = CARTESIAN_POINT ( 'NONE',  ( 0.1998031496062992740, 0.3460692066303959757, 0.01312335958005247417 ) ) ;
#77079 = ORIENTED_EDGE ( 'NONE', *, *, #24269, .F. ) ;
#77080 = CARTESIAN_POINT ( 'NONE',  ( -0.2099737532808391705, 0.1283753931104748280, 0.1820866141732283561 ) ) ;
#77082 = CARTESIAN_POINT ( 'NONE',  ( -0.3392501089628019995, 0.1958661417322832277, -1.593175853018372612 ) ) ;
#77081 = AXIS2_PLACEMENT_3D ( 'NONE', #30627, #36523, #41601 ) ;
#77083 = ORIENTED_EDGE ( 'NONE', *, *, #80583, .T. ) ;
#77084 = CARTESIAN_POINT ( 'NONE',  ( 0.1706036745406830368, 0.05413385826771666132, 0.4176697321401328100 ) ) ;
#77085 = CARTESIAN_POINT ( 'NONE',  ( 0.4724409448818897572, -0.1265901696524988906, -2.946194225721785465 ) ) ;
#77086 = CARTESIAN_POINT ( 'NONE',  ( 3.937007874015748143, 2.165354330708661568, -0.6299212598425196763 ) ) ;
#77087 = CARTESIAN_POINT ( 'NONE',  ( -0.3608923884514428360, 0.1771653543307087630, 0.09757992244046791164 ) ) ;
#77088 = CARTESIAN_POINT ( 'NONE',  ( 0.3674540682414705883, 0.2306618581243847221, -0.2411417322834647770 ) ) ;
#77089 = CARTESIAN_POINT ( 'NONE',  ( 0.7349081364829403995, 0.2306618581243848609, 0.2411417322834645549 ) ) ;
#77090 = CARTESIAN_POINT ( 'NONE',  ( 1.115485564304462551, -0.004921259842519576551, 0.3153832671262227771 ) ) ;
#77091 = CARTESIAN_POINT ( 'NONE',  ( 0.1181102362204730916, 0.2952755905511811885, 0.000000000000000000 ) ) ;
#77092 = CARTESIAN_POINT ( 'NONE',  ( -0.3917322834645669549, -7.196005306013483243E-17, -1.064285146160418360 ) ) ;
#77093 = CARTESIAN_POINT ( 'NONE',  ( -0.6955380577427815458, 0.05413385826771666132, 0.4176697321401328100 ) ) ;
#77094 = CARTESIAN_POINT ( 'NONE',  ( -1.476377952755905110, -0.4536011799217368745, -0.2665933059059886201 ) ) ;
#77095 = CARTESIAN_POINT ( 'NONE',  ( -0.6233595800524928121, -0.05778040916215522460, 0.4822834645669289988 ) ) ;
#77096 = DIRECTION ( 'NONE',  ( -0.000000000000000000, -1.000000000000000000, -0.000000000000000000 ) ) ;
#77097 = DIRECTION ( 'NONE',  ( 0.000000000000000000, -1.000000000000000000, 0.000000000000000000 ) ) ;
#77098 = VERTEX_POINT ( 'NONE', #75720 ) ;
#77099 = CARTESIAN_POINT ( 'NONE',  ( 0.3392501089628018884, -0.1958661417322833942, -2.463930076936694746 ) ) ;
#77100 = CARTESIAN_POINT ( 'NONE',  ( 0.1509186351706045259, -0.05778040916215560624, -0.4822834645669293319 ) ) ;
#77101 = ORIENTED_EDGE ( 'NONE', *, *, #30460, .F. ) ;
#77102 = CARTESIAN_POINT ( 'NONE',  ( -0.7020997375328076329, -0.3162353388693409650, -0.4822834645669289433 ) ) ;
#77103 = CARTESIAN_POINT ( 'NONE',  ( 1.312335958005249825, 0.2306618581243847221, -0.2411417322834647770 ) ) ;
#77104 = CARTESIAN_POINT ( 'NONE',  ( 1.377952755905512472, -0.6692913385826771977, 8.415575281601705876E-17 ) ) ;
#77105 = CARTESIAN_POINT ( 'NONE',  ( 0.7349081364829402885, -0.6046776061558809534, -0.2411417322834644161 ) ) ;
#77106 = CARTESIAN_POINT ( 'NONE',  ( 0.1312335958005257930, 0.2306618581243847221, -0.2411417322834647770 ) ) ;
#77107 = CARTESIAN_POINT ( 'NONE',  ( 0.1049643490035304938, -0.3917322834645669549, -1.429790026246719359 ) ) ;
#77108 = CARTESIAN_POINT ( 'NONE',  ( -1.017060367454067249, -0.3162353388693409650, -0.4822834645669289433 ) ) ;
#77109 = CARTESIAN_POINT ( 'NONE',  ( -0.3608923884514428360, 0.2952755905511811885, 0.1292274648535926551 ) ) ;
#77110 = CARTESIAN_POINT ( 'NONE',  ( -0.1706036745406816491, -0.004921259842519870586, -0.3153832671262229437 ) ) ;
#77111 = CARTESIAN_POINT ( 'NONE',  ( -0.2489800900487910418, -0.1588251575432186868, 5.781310865041811020 ) ) ;
#77112 = CARTESIAN_POINT ( 'NONE',  ( -0.1312335958005241554, 0.2306618581243848609, 0.2411417322834645549 ) ) ;
#77113 = DIRECTION ( 'NONE',  ( 0.000000000000000000, 1.000000000000000000, 1.408710688920637755E-15 ) ) ;
#77114 = CARTESIAN_POINT ( 'NONE',  ( 1.187664041994751285, -0.3162353388693409650, -0.4822834645669289433 ) ) ;
#77115 = DIRECTION ( 'NONE',  ( -0.000000000000000000, -1.000000000000000000, -0.000000000000000000 ) ) ;
#77116 = ORIENTED_EDGE ( 'NONE', *, *, #33182, .T. ) ;
#77117 = ORIENTED_EDGE ( 'NONE', *, *, #5158, .F. ) ;
#77118 = CARTESIAN_POINT ( 'NONE',  ( 0.1443569553805781891, 0.05413385826771626580, -0.4176697321401330321 ) ) ;
#77119 = CARTESIAN_POINT ( 'NONE',  ( -0.2230971128608915943, -0.3690944881889765550, -0.3153832671262227771 ) ) ;
#77121 = DIRECTION ( 'NONE',  ( 0.000000000000000000, -1.000000000000000000, -0.000000000000000000 ) ) ;
#77120 = CARTESIAN_POINT ( 'NONE',  ( 1.482939632545932307, -0.3690944881889763329, 0.3153832671262228327 ) ) ;
#77122 = CARTESIAN_POINT ( 'NONE',  ( -0.3917322834645671215, 0.1049643490035301469, -1.219816272965879023 ) ) ;
#77123 = CARTESIAN_POINT ( 'NONE',  ( -0.3458507752293909498, 0.3458507752293907833, -0.2539370078740156855 ) ) ;
#77124 = CARTESIAN_POINT ( 'NONE',  ( 1.404199475065617708, -0.004921259842519870586, -0.3153832671262229437 ) ) ;
#77125 = CARTESIAN_POINT ( 'NONE',  ( 1.515748031496063186, -0.5400638737290845981, -0.3530559997133363437 ) ) ;
#77126 = CARTESIAN_POINT ( 'NONE',  ( 0.3420746716998660508, 0.1974969037888705814, 0.1069553805774278443 ) ) ;
#77127 = CARTESIAN_POINT ( 'NONE',  ( -0.07217847769028813698, -0.3162353388693409650, -0.4822834645669289433 ) ) ;
#77128 = CARTESIAN_POINT ( 'NONE',  ( -1.135170603674539924, 0.2952755905511810774, -0.1292274648535930714 ) ) ;
#77129 = VECTOR ( 'NONE', #69709, 39.37007874015748854 ) ;
#77130 = CARTESIAN_POINT ( 'NONE',  ( -1.108923884514435132, -0.3162353388693405765, 0.4822834645669290543 ) ) ;
#77131 = CARTESIAN_POINT ( 'NONE',  ( 0.1181102362204730916, -0.6692913385826771977, 8.415575281601705876E-17 ) ) ;
#77132 = CARTESIAN_POINT ( 'NONE',  ( -0.3420746716998662729, 0.1974969037888702206, -0.2604986876640420501 ) ) ;
#77133 = CARTESIAN_POINT ( 'NONE',  ( -1.456692913385826182, 0.1771653543307087630, 0.000000000000000000 ) ) ;
#77134 = CARTESIAN_POINT ( 'NONE',  ( 0.8595800524934390507, -0.05778040916215560624, -0.4822834645669293319 ) ) ;
#77135 = CARTESIAN_POINT ( 'NONE',  ( 0.7480314960629927956, 0.1771653543307087630, 0.000000000000000000 ) ) ;
#77136 = CARTESIAN_POINT ( 'NONE',  ( 0.8267716535433077274, 0.2066929133858268208, 0.000000000000000000 ) ) ;
#77137 = CARTESIAN_POINT ( 'NONE',  ( 0.9973753280839902091, -0.5023911411419708095, 0.1820866141732285504 ) ) ;
#77138 = CARTESIAN_POINT ( 'NONE',  ( -1.220472440944881054, -0.6692913385826771977, 8.415575281601705876E-17 ) ) ;
#77139 = CARTESIAN_POINT ( 'NONE',  ( -0.1070741851644056997, 0.3996062992125984925, -0.8707349081364830212 ) ) ;
#77140 = CARTESIAN_POINT ( 'NONE',  ( 1.279527559055118724, -0.5400638737290845981, -0.3530559997133363437 ) ) ;
#77141 = CARTESIAN_POINT ( 'NONE',  ( 0.2867679344610365999, 0.2867679344610365999, -0.7598425196850391306 ) ) ;
#77143 = CARTESIAN_POINT ( 'NONE',  ( -3.900966923095589678, 2.755905511811024056, 0.5314960629921260393 ) ) ;
#77142 = CARTESIAN_POINT ( 'NONE',  ( 0.7742782152230979209, 0.05413385826771626580, -0.4176697321401330321 ) ) ;
#77144 = CARTESIAN_POINT ( 'NONE',  ( -1.603475055217291612, 1.054977578535736926, -0.04573490813648262154 ) ) ;
#77145 = CARTESIAN_POINT ( 'NONE',  ( -0.04593175853018302557, 0.2952755905511811885, 0.1292274648535926551 ) ) ;
#77146 = CARTESIAN_POINT ( 'NONE',  ( 0.5577427821522314977, -0.2845877964562161244, -0.3641732283464567121 ) ) ;
#77147 = AXIS2_PLACEMENT_3D ( 'NONE', #35466, #42184, #80518 ) ;
#77148 = CARTESIAN_POINT ( 'NONE',  ( 0.8530183727034128527, -0.4281496062992124485, 0.4176697321401328655 ) ) ;
#77149 = CARTESIAN_POINT ( 'NONE',  ( -1.614173228346456712, 0.9921945702958917535, -0.1372047244094478091 ) ) ;
#77150 = CARTESIAN_POINT ( 'NONE',  ( -0.9055118110236215490, 0.1771653543307087630, 0.000000000000000000 ) ) ;
#77151 = CARTESIAN_POINT ( 'NONE',  ( -0.5708661417322828946, 0.1660481256975883668, -0.3530559997133364547 ) ) ;
#77152 = CARTESIAN_POINT ( 'NONE',  ( 1.627296587926509996, -0.6046776061558807314, 0.2411417322834647770 ) ) ;
#77153 = CARTESIAN_POINT ( 'NONE',  ( -1.115485564304461219, -0.4281496062992124485, 0.4176697321401328655 ) ) ;
#77154 = CARTESIAN_POINT ( 'NONE',  ( 0.8792650918635177559, 0.05413385826771666132, 0.4176697321401328100 ) ) ;
#77155 = CARTESIAN_POINT ( 'NONE',  ( -1.325459317585300889, -0.004921259842519576551, 0.3153832671262227771 ) ) ;
#77156 = CARTESIAN_POINT ( 'NONE',  ( 0.9548908091195654757, -4.927456884911482678E-16, 0.4445507791589062840 ) ) ;
#77157 = CARTESIAN_POINT ( 'NONE',  ( 1.200787401574803681, -0.5400638737290845981, -0.3530559997133363437 ) ) ;
#77158 = CARTESIAN_POINT ( 'NONE',  ( 0.3458507752293908943, -0.3458507752293908943, -2.379921259842520342 ) ) ;
#77159 = CARTESIAN_POINT ( 'NONE',  ( -1.568241469816272105, -0.05778040916215522460, 0.4822834645669289988 ) ) ;
#77160 = CARTESIAN_POINT ( 'NONE',  ( -1.522309711286088607, -0.5023911411419708095, 0.1820866141732285504 ) ) ;
#77161 = CARTESIAN_POINT ( 'NONE',  ( -0.9383202099737524282, -0.08942795157527998196, 0.3641732283464567121 ) ) ;
#77162 = CARTESIAN_POINT ( 'NONE',  ( 1.686351706036745890, 0.1771653543307087630, 0.09757992244046791164 ) ) ;
#77163 = CARTESIAN_POINT ( 'NONE',  ( -0.3083989501312330295, -0.3162353388693409650, -0.4822834645669289433 ) ) ;
#77164 = CARTESIAN_POINT ( 'NONE',  ( -0.2427821522309703550, -0.2845877964562159024, 0.3641732283464567677 ) ) ;
#77165 = CARTESIAN_POINT ( 'NONE',  ( -1.463254593175852492, -0.5511811023622048555, -0.09757992244046775898 ) ) ;
#77166 = CARTESIAN_POINT ( 'NONE',  ( 1.095800524934383846, -0.2845877964562159024, 0.3641732283464567677 ) ) ;
#77167 = CARTESIAN_POINT ( 'NONE',  ( 0.5643044619422579178, 0.05413385826771666132, 0.4176697321401328100 ) ) ;
#77168 = PLANE ( 'NONE',  #19193 ) ;
#77169 = CARTESIAN_POINT ( 'NONE',  ( 0.4461942257217856311, 0.2306618581243847221, -0.2411417322834647770 ) ) ;
#77170 = CARTESIAN_POINT ( 'NONE',  ( 0.4724409448818904789, -0.1870078740157479769, 0.3641732283464567677 ) ) ;
#77171 = CARTESIAN_POINT ( 'NONE',  ( 1.561679790026247350, -0.4281496062992124485, 0.4176697321401328655 ) ) ;
#77172 = EDGE_CURVE ( 'NONE', #38994, #77522, #71726, .T. ) ;
#77173 = CARTESIAN_POINT ( 'NONE',  ( -1.437007874015747477, 0.1660481256975883668, -0.3530559997133364547 ) ) ;
#77174 = CARTESIAN_POINT ( 'NONE',  ( -0.4133858267716528645, 0.1660481256975883668, -0.3530559997133364547 ) ) ;
#77175 = CARTESIAN_POINT ( 'NONE',  ( 0.3996062992125985480, 0.1070741851644054637, -0.2821522309711286258 ) ) ;
#77176 = CARTESIAN_POINT ( 'NONE',  ( 0.3996062992125986035, -0.1070741851644052972, -2.865485564304462329 ) ) ;
#77177 = CARTESIAN_POINT ( 'NONE',  ( -0.03937007874015669567, -0.6692913385826771977, 8.415575281601705876E-17 ) ) ;
#77178 = CARTESIAN_POINT ( 'NONE',  ( 1.161417322834646271, 0.07958543189024071263, -0.2665933059059888421 ) ) ;
#77179 = CARTESIAN_POINT ( 'NONE',  ( -0.2624671916010490880, -0.6046776061558807314, 0.2411417322834647770 ) ) ;
#77180 = CARTESIAN_POINT ( 'NONE',  ( 0.3412073490813655186, 0.2306618581243848609, 0.2411417322834645549 ) ) ;
#77181 = CARTESIAN_POINT ( 'NONE',  ( -9.787531504996567848E-17, 0.3996062992125986035, -2.362204724409448620 ) ) ;
#77182 = CARTESIAN_POINT ( 'NONE',  ( -0.2891555358219911054, 0.2891555358219909388, -2.066929133858268042 ) ) ;
#77183 = CARTESIAN_POINT ( 'NONE',  ( 0.3392501089628018329, 0.1958661417322835607, -0.4383202099737532609 ) ) ;
#77184 = CARTESIAN_POINT ( 'NONE',  ( 0.2431769186048377551, -0.1675026378872651045, 5.643961825897843454 ) ) ;
#77185 = CARTESIAN_POINT ( 'NONE',  ( 0.2867679344610366554, -0.2867679344610365444, -1.035433070866141447 ) ) ;
#77186 = CARTESIAN_POINT ( 'NONE',  ( -0.8792650918635160906, -0.004921259842519870586, -0.3153832671262229437 ) ) ;
#77187 = CARTESIAN_POINT ( 'NONE',  ( -1.135170603674539924, -0.6692913385826771977, 0.1292274648535927661 ) ) ;
#77188 = CARTESIAN_POINT ( 'NONE',  ( 0.3949938075777409408, -0.1058382717557499186, -2.550524934383202158 ) ) ;
#77189 = CARTESIAN_POINT ( 'NONE',  ( 0.3083989501312343062, -0.05778040916215560624, -0.4822834645669293319 ) ) ;
#77190 = CARTESIAN_POINT ( 'NONE',  ( 1.377952755905512472, -0.6692913385826771977, 8.415575281601705876E-17 ) ) ;
#77191 = CARTESIAN_POINT ( 'NONE',  ( 0.6561679790026253567, 0.2306618581243848609, 0.2411417322834645549 ) ) ;
#77192 = CARTESIAN_POINT ( 'NONE',  ( -0.4724409448818895907, -0.1265901696524993070, -2.880577427821522374 ) ) ;
#77193 = CARTESIAN_POINT ( 'NONE',  ( -0.3996062992125986035, -0.1070741851644056997, -2.093175853018372834 ) ) ;
#77194 = CARTESIAN_POINT ( 'NONE',  ( 0.3392501089628018884, -0.1958661417322833942, -0.7316466123697656920 ) ) ;
#77195 = FACE_OUTER_BOUND ( 'NONE', #20591, .T. ) ;
#77196 = CARTESIAN_POINT ( 'NONE',  ( 0.3346456692913390985, 0.1660481256975885056, 0.3530559997133364547 ) ) ;
#77197 = CARTESIAN_POINT ( 'NONE',  ( 0.06561679790026316017, 0.05413385826771626580, -0.4176697321401330321 ) ) ;
#77198 = AXIS2_PLACEMENT_3D ( 'NONE', #51692, #18894, #19727 ) ;
#77199 = CARTESIAN_POINT ( 'NONE',  ( 0.8398950131233602345, 0.1283753931104746893, -0.1820866141732285504 ) ) ;
#77200 = CARTESIAN_POINT ( 'NONE',  ( 1.181102362204725198, -0.1870078740157479769, 0.4822834645669291653 ) ) ;
#77201 =( REPRESENTATION_RELATIONSHIP ('NONE','NONE', #79348, #82043 ) REPRESENTATION_RELATIONSHIP_WITH_TRANSFORMATION ( #43879 )SHAPE_REPRESENTATION_RELATIONSHIP( ) );
#77202 = CARTESIAN_POINT ( 'NONE',  ( -0.1049643490035302024, -0.3917322834645671215, -0.3143044619422573072 ) ) ;
#77203 = CARTESIAN_POINT ( 'NONE',  ( 0.5511811023622054106, -0.1870078740157480879, -0.4822834645669291653 ) ) ;
#77204 = CARTESIAN_POINT ( 'NONE',  ( 1.207349081364829990, 0.2306618581243848609, 0.2411417322834645549 ) ) ;
#77205 = CARTESIAN_POINT ( 'NONE',  ( 0.2165354330708668673, -0.5400638737290844871, 0.3530559997133364547 ) ) ;
#77206 = CARTESIAN_POINT ( 'NONE',  ( 1.227034120734908917, 0.1771653543307087075, -0.09757992244046823083 ) ) ;
#77207 = CARTESIAN_POINT ( 'NONE',  ( -1.076115485564303809, 0.2306618581243848609, 0.2411417322834645549 ) ) ;
#77208 = CARTESIAN_POINT ( 'NONE',  ( -0.9120734908136475250, 0.2952755905511811885, 0.1292274648535926551 ) ) ;
#77209 = CARTESIAN_POINT ( 'NONE',  ( 1.371391076115485719, -0.6692913385826773087, -0.1292274648535924053 ) ) ;
#77210 = CARTESIAN_POINT ( 'NONE',  ( -0.2867679344610364334, -0.2867679344610367109, -0.7736220472440945573 ) ) ;
#77211 = CARTESIAN_POINT ( 'NONE',  ( 0.1049643490035303689, 0.3917322834645670104, -2.032808398950130879 ) ) ;
#77212 = CARTESIAN_POINT ( 'NONE',  ( -0.2867679344610364334, -0.2867679344610367109, -2.885826771653543066 ) ) ;
#77213 = ORIENTED_EDGE ( 'NONE', *, *, #3251, .T. ) ;
#77214 = CARTESIAN_POINT ( 'NONE',  ( 0.1974969037888706369, -0.3420746716998659953, -2.926509186351706315 ) ) ;
#77215 = ORIENTED_EDGE ( 'NONE', *, *, #2734, .F. ) ;
#77216 = CARTESIAN_POINT ( 'NONE',  ( -0.3149606299212558969, 2.559055118110236560, -1.076935383196058638 ) ) ;
#77217 = CARTESIAN_POINT ( 'NONE',  ( 1.062992125984252745, -0.5511811023622047445, 6.969142054262312111E-17 ) ) ;
#77218 = CARTESIAN_POINT ( 'NONE',  ( -0.3460692066303958092, -0.1998031496062994683, -1.312335958005249381 ) ) ;
#77219 = CARTESIAN_POINT ( 'NONE',  ( 1.194225721784777594, -0.004921259842519576551, 0.3153832671262227771 ) ) ;
#77220 = CARTESIAN_POINT ( 'NONE',  ( 0.4724409448818898682, 2.892866454678787531E-17, -0.7480314960629921295 ) ) ;
#77221 = CARTESIAN_POINT ( 'NONE',  ( 6.267877385347666114E-17, 1.062992125984252745, 2.874015748031495843 ) ) ;
#77222 = CARTESIAN_POINT ( 'NONE',  ( -1.306827173596996738, 0.000000000000000000, -0.4445507791589060620 ) ) ;
#77223 = CARTESIAN_POINT ( 'NONE',  ( 4.797336870675656522E-17, -0.3917322834645670104, -0.9507874015748032370 ) ) ;
#77224 = CARTESIAN_POINT ( 'NONE',  ( -1.043307086614172041, -0.4536011799217367080, 0.2665933059059888421 ) ) ;
#77225 = CARTESIAN_POINT ( 'NONE',  ( -1.469816272965878357, -0.5023911411419708095, -0.1820866141732282451 ) ) ;
#77226 = CARTESIAN_POINT ( 'NONE',  ( -1.135170603674539924, 0.2952755905511810774, -0.1292274648535930714 ) ) ;
#77227 = CARTESIAN_POINT ( 'NONE',  ( 0.01968503937007930540, 0.1660481256975885056, 0.3530559997133364547 ) ) ;
#77228 = CARTESIAN_POINT ( 'NONE',  ( 1.601049868766404982, 0.2306618581243848609, 0.2411417322834645549 ) ) ;
#77229 = ORIENTED_EDGE ( 'NONE', *, *, #53988, .F. ) ;
#77230 = CARTESIAN_POINT ( 'NONE',  ( 0.5611900217179910388, 1.223219560026271499E-15, 0.4445507791589056734 ) ) ;
#77231 = DIRECTION ( 'NONE',  ( 1.000000000000000000, 0.000000000000000000, 0.000000000000000000 ) ) ;
#77232 = CARTESIAN_POINT ( 'NONE',  ( -0.1265901696524986964, -0.4724409448818899238, -2.119422572178477626 ) ) ;
#77233 = PLANE ( 'NONE',  #23718 ) ;
#77234 = CARTESIAN_POINT ( 'NONE',  ( 1.603475055217291612, 1.267857067133554061, 0.04573490813648273950 ) ) ;
#77235 = CARTESIAN_POINT ( 'NONE',  ( -1.089238845144356427, -0.3690944881889765550, -0.3153832671262227771 ) ) ;
#77236 = CARTESIAN_POINT ( 'NONE',  ( -0.9580052493438311334, 0.05413385826771626580, -0.4176697321401330321 ) ) ;
#77237 = CARTESIAN_POINT ( 'NONE',  ( 0.5708661417322842269, 0.1660481256975885056, 0.3530559997133364547 ) ) ;
#77238 = ORIENTED_EDGE ( 'NONE', *, *, #32695, .T. ) ;
#77240 = CARTESIAN_POINT ( 'NONE',  ( 0.1742125984251973736, -0.000000000000000000, -0.3937007874015748254 ) ) ;
#77239 = CARTESIAN_POINT ( 'NONE',  ( -2.362204724409448620, 0.03937007874015751446, 0.5118110236220224651 ) ) ;
#77241 = CARTESIAN_POINT ( 'NONE',  ( 1.332020997375329197, -0.3162353388693405765, 0.4822834645669290543 ) ) ;
#77242 = CARTESIAN_POINT ( 'NONE',  ( 1.568241469816273437, -0.2845877964562159024, 0.3641732283464567677 ) ) ;
#77243 = CARTESIAN_POINT ( 'NONE',  ( 4.797336870675655290E-17, -0.3917322834645669549, -0.7886945949793155997 ) ) ;
#77244 = CARTESIAN_POINT ( 'NONE',  ( -0.2165354330708654795, -0.4536011799217368745, -0.2665933059059886201 ) ) ;
#77245 = CARTESIAN_POINT ( 'NONE',  ( -1.266404199475064773, -0.08942795157528024563, -0.3641732283464568787 ) ) ;
#77246 = CARTESIAN_POINT ( 'NONE',  ( -0.1958661417322834220, -0.3392501089628018884, -0.9376640419947508409 ) ) ;
#77247 = PRODUCT_DEFINITION_FORMATION_WITH_SPECIFIED_SOURCE ( 'ANY', '', #46652, .NOT_KNOWN. ) ;
#77248 = CARTESIAN_POINT ( 'NONE',  ( -0.4199475065616791736, -0.5023911411419708095, 0.1820866141732285504 ) ) ;
#77249 = CARTESIAN_POINT ( 'NONE',  ( 0.3083989501312343062, -0.2845877964562159024, 0.3641732283464567677 ) ) ;
#77250 = CARTESIAN_POINT ( 'NONE',  ( 0.07217847769028949700, -0.05778040916215560624, -0.4822834645669293319 ) ) ;
#77251 = CARTESIAN_POINT ( 'NONE',  ( -1.030183727034119867, -0.2845877964562159024, 0.3641732283464567677 ) ) ;
#77252 = CARTESIAN_POINT ( 'NONE',  ( -0.3917322834645669549, -0.1049643490035306603, -2.557742782152230721 ) ) ;
#77253 = CARTESIAN_POINT ( 'NONE',  ( 1.259842519685040019, -0.1870078740157479769, 0.4822834645669291653 ) ) ;
#77254 = CARTESIAN_POINT ( 'NONE',  ( -1.555118110236219930, -0.5400638737290845981, -0.3530559997133363437 ) ) ;
#77255 = CARTESIAN_POINT ( 'NONE',  ( 0.4091458600556404646, -0.2362204724409448231, -1.126640419947506633 ) ) ;
#77256 = CARTESIAN_POINT ( 'NONE',  ( -0.2099737532808391705, -0.6046776061558809534, -0.2411417322834644161 ) ) ;
#77257 = CARTESIAN_POINT ( 'NONE',  ( -1.049868766404198794, -0.6046776061558807314, 0.2411417322834647770 ) ) ;
#77258 = CARTESIAN_POINT ( 'NONE',  ( 0.9514435695538062676, -0.2845877964562161244, -0.3641732283464567121 ) ) ;
#77259 = AXIS2_PLACEMENT_3D ( 'NONE', #5678, #11606, #25028 ) ;
#77260 = CARTESIAN_POINT ( 'NONE',  ( -0.1115485564304456306, 0.1771653543307087075, -0.09757992244046823083 ) ) ;
#77261 = CARTESIAN_POINT ( 'NONE',  ( -0.4855643044619415427, -0.4281496062992124485, 0.4176697321401328655 ) ) ;
#77262 = CARTESIAN_POINT ( 'NONE',  ( -1.509186351706035767, -0.4281496062992124485, 0.4176697321401328655 ) ) ;
#77263 = CARTESIAN_POINT ( 'NONE',  ( 0.4359958488159444423, 1.724409448818900570, 2.630268417803970138 ) ) ;
#77264 = CARTESIAN_POINT ( 'NONE',  ( 1.482939632545932307, -0.3690944881889763329, 0.3153832671262228327 ) ) ;
#77265 = CARTESIAN_POINT ( 'NONE',  ( -0.2493438320209966919, -0.4281496062992124485, 0.4176697321401328655 ) ) ;
#77266 = CARTESIAN_POINT ( 'NONE',  ( -1.627296587926508442, -0.6046776061558809534, -0.2411417322834644161 ) ) ;
#77267 = ORIENTED_EDGE ( 'NONE', *, *, #22774, .T. ) ;
#77268 = CARTESIAN_POINT ( 'NONE',  ( 0.3996062992125985480, 2.446882876249141654E-17, -2.557086614173228689 ) ) ;
#77269 = CARTESIAN_POINT ( 'NONE',  ( -0.8858267716535425107, -0.4536011799217367080, 0.2665933059059888421 ) ) ;
#77270 = CARTESIAN_POINT ( 'NONE',  ( 0.6955380577427828781, 0.05413385826771626580, -0.4176697321401330321 ) ) ;
#77271 = CARTESIAN_POINT ( 'NONE',  ( -1.023622047244094002, -0.1870078740157480601, -0.3641732283464567677 ) ) ;
#77272 = CARTESIAN_POINT ( 'NONE',  ( -0.1998031496062994405, 0.3460692066303957537, -1.192257217847769057 ) ) ;
#77273 = CARTESIAN_POINT ( 'NONE',  ( -0.7939632545931754048, -0.3162353388693405765, 0.4822834645669290543 ) ) ;
#77274 = CARTESIAN_POINT ( 'NONE',  ( 0.6824146981627303710, -0.6046776061558807314, 0.2411417322834647770 ) ) ;
#77275 = CARTESIAN_POINT ( 'NONE',  ( 0.5511811023622055217, -0.1870078740157479769, 0.4822834645669291653 ) ) ;
#77276 = CARTESIAN_POINT ( 'NONE',  ( 1.417322834645670104, -0.1870078740157479769, 0.4822834645669291653 ) ) ;
#77277 = CARTESIAN_POINT ( 'NONE',  ( -1.522309711286088607, 0.1283753931104746893, -0.1820866141732285504 ) ) ;
#77278 = CARTESIAN_POINT ( 'NONE',  ( -0.1998031496062991630, -0.3460692066303959202, -0.4573490813648293796 ) ) ;
#77279 = CARTESIAN_POINT ( 'NONE',  ( -9.787531504996567848E-17, 0.3996062992125986035, -0.7874015748031496509 ) ) ;
#77280 = CARTESIAN_POINT ( 'NONE',  ( 0.1058382717557500713, -0.3949938075777409408, -0.5577427821522310536 ) ) ;
#77281 = CARTESIAN_POINT ( 'NONE',  ( 0.2730112473383900507, 1.149291835544637319, -1.662080954481470529 ) ) ;
#77282 = CARTESIAN_POINT ( 'NONE',  ( 1.135170603674541256, -0.5511811023622048555, -0.09757992244046775898 ) ) ;
#77283 = CARTESIAN_POINT ( 'NONE',  ( 0.3543307086614179147, 0.1771653543307087630, 0.000000000000000000 ) ) ;
#77284 = CARTESIAN_POINT ( 'NONE',  ( 0.02624671916010564918, 0.2306618581243848609, 0.2411417322834645549 ) ) ;
#77285 = CARTESIAN_POINT ( 'NONE',  ( 1.443569553805774897, 0.2306618581243848609, 0.2411417322834645549 ) ) ;
#77286 = CARTESIAN_POINT ( 'NONE',  ( -0.1058382717557503072, 0.3949938075777408852, -1.185695538057742748 ) ) ;
#77287 = CARTESIAN_POINT ( 'NONE',  ( 0.3346456692913393205, -0.4536011799217368745, -0.2665933059059886201 ) ) ;
#77288 = CARTESIAN_POINT ( 'NONE',  ( -0.5249343832020990641, 0.2306618581243848609, 0.2411417322834645549 ) ) ;
#77289 = CARTESIAN_POINT ( 'NONE',  ( -1.082677165354329896, -0.5400638737290845981, -0.3530559997133363437 ) ) ;
#77290 = CARTESIAN_POINT ( 'NONE',  ( 0.6364829396325465405, -0.3162353388693409650, -0.4822834645669289433 ) ) ;
#77291 = CARTESIAN_POINT ( 'NONE',  ( 0.3458507752293908943, 0.3458507752293908943, -1.397637795275590067 ) ) ;
#77292 = CARTESIAN_POINT ( 'NONE',  ( -9.787531504996567848E-17, 0.3996062992125986035, -2.677165354330708347 ) ) ;
#77293 =( BOUNDED_CURVE ( )  B_SPLINE_CURVE ( 2, ( #67368, #10121, #76155, #56366, #49637, #62272, #37837, #18085, #75330, #11777, #12179, #24785, #61863 ),
 .UNSPECIFIED., .F., .F. ) 
 B_SPLINE_CURVE_WITH_KNOTS ( ( 3, 2, 2, 2, 2, 2, 3 ),
 ( 0.1875000000000000000, 0.1916666666666666796, 0.1958333333333333315, 0.2000000000000000111, 0.2041666666666666907, 0.2083333333333333703, 0.2125000000000000222 ),
 .UNSPECIFIED. ) 
 CURVE ( )  GEOMETRIC_REPRESENTATION_ITEM ( )  RATIONAL_B_SPLINE_CURVE ( ( 1.000000000000000000, 0.9659258262890683122, 1.000000000000000000, 0.9659258262890683122, 1.000000000000000000, 0.9659258262890683122, 1.000000000000000000, 0.9659258262890683122, 1.000000000000000000, 0.9659258262890683122, 1.000000000000000000, 0.9659258262890680902, 1.000000000000000222 ) ) 
 REPRESENTATION_ITEM ( '' )  );
#77294 = VERTEX_POINT ( 'NONE', #14245 ) ;
#77295 = VERTEX_POINT ( 'NONE', #7076 ) ;
#77296 = CARTESIAN_POINT ( 'NONE',  ( -1.076115485564303809, 0.2306618581243848609, 0.2411417322834645549 ) ) ;
#77297 = CARTESIAN_POINT ( 'NONE',  ( -0.7349081364829387342, -0.6046776061558807314, 0.2411417322834647770 ) ) ;
#77299 = CARTESIAN_POINT ( 'NONE',  ( -0.7874015748031489847, -0.1870078740157480879, -0.4822834645669291653 ) ) ;
#77298 = CARTESIAN_POINT ( 'NONE',  ( -0.6561679790026240244, 0.1283753931104746893, -0.1820866141732285504 ) ) ;
#77300 = CARTESIAN_POINT ( 'NONE',  ( -0.3392501089628018329, -0.1958661417322836440, -2.022290395504250160 ) ) ;
#77301 = VERTEX_POINT ( 'NONE', #33968 ) ;
#77302 = CARTESIAN_POINT ( 'NONE',  ( 0.4849061582275024929, 1.568468489416427580, -0.4921425059946356040 ) ) ;
#77303 = CARTESIAN_POINT ( 'NONE',  ( -1.614173228346455824, 0.1771653543307087630, 0.000000000000000000 ) ) ;
#77304 = CARTESIAN_POINT ( 'NONE',  ( -1.240157480314959759, 0.1660481256975885056, 0.3530559997133364547 ) ) ;
#77305 = CARTESIAN_POINT ( 'NONE',  ( 0.2230971128608929543, 0.05413385826771626580, -0.4176697321401330321 ) ) ;
#77306 = ADVANCED_FACE ( 'NONE', ( #26847 ), #76542, .T. ) ;
#77307 = CARTESIAN_POINT ( 'NONE',  ( -0.7283464566929126471, -0.5400638737290844871, 0.3530559997133364547 ) ) ;
#77308 = ADVANCED_FACE ( 'NONE', ( #77794 ), #17962, .T. ) ;
#77309 = CARTESIAN_POINT ( 'NONE',  ( -0.1049643490035302024, -0.3917322834645671215, -1.639107611548556109 ) ) ;
#77310 = CARTESIAN_POINT ( 'NONE',  ( -0.9711286089238838626, 0.1283753931104746893, -0.1820866141732285504 ) ) ;
#77311 = VERTEX_POINT ( 'NONE', #71894 ) ;
#77312 = CARTESIAN_POINT ( 'NONE',  ( 0.3949938075777409408, 0.1058382717557500574, -1.856955380577427928 ) ) ;
#77313 = ORIENTED_EDGE ( 'NONE', *, *, #30007, .T. ) ;
#77314 = CARTESIAN_POINT ( 'NONE',  ( 3.937007874015748143, 2.559055118110236560, 0.5314960629921260393 ) ) ;
#77315 = CARTESIAN_POINT ( 'NONE',  ( -1.272965879265091305, -0.4281496062992124485, 0.4176697321401328655 ) ) ;
#77316 = CARTESIAN_POINT ( 'NONE',  ( -0.6889763779527552368, 0.1660481256975885056, 0.3530559997133364547 ) ) ;
#77317 = CARTESIAN_POINT ( 'NONE',  ( -0.2925321140481930704, -0.2925321140481933480, -0.2165354330708661734 ) ) ;
#77318 = CARTESIAN_POINT ( 'NONE',  ( -1.010498687664041384, -0.4281496062992127816, -0.4176697321401328100 ) ) ;
#77319 = CARTESIAN_POINT ( 'NONE',  ( -1.437007874015747477, -0.5400638737290844871, 0.3530559997133364547 ) ) ;
#77320 = LINE ( 'NONE', #52457, #45834 ) ;
#77321 = DIRECTION ( 'NONE',  ( -0.000000000000000000, 0.000000000000000000, 1.000000000000000000 ) ) ;
#77322 = CARTESIAN_POINT ( 'NONE',  ( 0.6496062992125991586, -0.4536011799217368745, -0.2665933059059886201 ) ) ;
#77323 = CARTESIAN_POINT ( 'NONE',  ( 1.604771003085129433, 0.4934440724007135848, 0.1466069496707750885 ) ) ;
#77324 = CARTESIAN_POINT ( 'NONE',  ( 0.1049643490035304938, -0.3917322834645669549, -0.1699475065616798397 ) ) ;
#77325 = CARTESIAN_POINT ( 'NONE',  ( -0.4265091863517051496, 0.1771653543307087075, -0.09757992244046823083 ) ) ;
#77326 = CARTESIAN_POINT ( 'NONE',  ( -0.6889763779527552368, 0.1660481256975885056, 0.3530559997133364547 ) ) ;
#77327 = CARTESIAN_POINT ( 'NONE',  ( 1.430446194225722500, 0.05413385826771666132, 0.4176697321401328100 ) ) ;
#77328 = CARTESIAN_POINT ( 'NONE',  ( -0.4921259842519677963, 0.1660481256975883668, -0.3530559997133364547 ) ) ;
#77329 = ORIENTED_EDGE ( 'NONE', *, *, #6944, .F. ) ;
#77330 = EDGE_LOOP ( 'NONE', ( #48401, #14915, #59939, #62514, #70496, #79390 ) ) ;
#77331 = CARTESIAN_POINT ( 'NONE',  ( 4.893765752498283308E-17, -0.3996062992125985480, -2.045275590551181022 ) ) ;
#77332 = CARTESIAN_POINT ( 'NONE',  ( -1.135170603674539924, 0.2952755905511810774, -0.1292274648535930714 ) ) ;
#77333 = CARTESIAN_POINT ( 'NONE',  ( 1.489501312335958172, -0.05778040916215560624, -0.4822834645669293319 ) ) ;
#77334 = CARTESIAN_POINT ( 'NONE',  ( -1.286089238845143479, -0.5023911411419708095, 0.1820866141732285504 ) ) ;
#77335 = CARTESIAN_POINT ( 'NONE',  ( -1.489501312335957062, -0.3162353388693409650, -0.4822834645669289433 ) ) ;
#77336 = CARTESIAN_POINT ( 'NONE',  ( 0.3458507752293908943, 0.3458507752293908943, -0.9251968503937008093 ) ) ;
#77337 = CARTESIAN_POINT ( 'NONE',  ( 1.867405098639527417, 1.081388112195863949, 0.1351566381869950262 ) ) ;
#77338 = ADVANCED_FACE ( 'NONE', ( #25586 ), #20127, .F. ) ;
#77339 = CARTESIAN_POINT ( 'NONE',  ( -0.3392501089628019995, 0.1958661417322832277, -0.1758530183727033402 ) ) ;
#77340 = CARTESIAN_POINT ( 'NONE',  ( -0.4724409448818898682, -8.678599364036362592E-17, -0.7460629921259841479 ) ) ;
#77341 = CARTESIAN_POINT ( 'NONE',  ( -0.04593175853018302557, 0.2952755905511811885, 0.1292274648535926551 ) ) ;
#77342 = CARTESIAN_POINT ( 'NONE',  ( -1.207349081364828436, -0.5023911411419708095, 0.1820866141732285504 ) ) ;
#77343 = CARTESIAN_POINT ( 'NONE',  ( -0.8464566929133852113, -0.5400638737290845981, -0.3530559997133363437 ) ) ;
#77344 = CARTESIAN_POINT ( 'NONE',  ( -0.1265901696524986964, -0.4724409448818899238, -2.668635170603674833 ) ) ;
#77345 = CARTESIAN_POINT ( 'NONE',  ( -1.187664041994750175, -0.05778040916215560624, -0.4822834645669293319 ) ) ;
#77346 = CARTESIAN_POINT ( 'NONE',  ( -0.8923884514435688198, 0.2306618581243847221, -0.2411417322834647770 ) ) ;
#77347 = CARTESIAN_POINT ( 'NONE',  ( -0.1115485564304456306, 0.2952755905511810774, -0.1292274648535930714 ) ) ;
#77348 = CARTESIAN_POINT ( 'NONE',  ( 0.1058382717557499880, 0.3949938075777409408, -2.747375328083990098 ) ) ;
#77349 = CARTESIAN_POINT ( 'NONE',  ( 0.7086614173228352742, -0.1870078740157480601, -0.3641732283464567677 ) ) ;
#77350 = CARTESIAN_POINT ( 'NONE',  ( -0.8202099737532801971, -0.5511811023622046335, 0.09757992244046803654 ) ) ;
#77351 = CARTESIAN_POINT ( 'NONE',  ( -0.08351193659984793016, 1.070350416549052497, -1.608688096019881497 ) ) ;
#77352 = CARTESIAN_POINT ( 'NONE',  ( 0.5708661417322842269, 0.07958543189024085140, 0.2665933059059887866 ) ) ;
#77353 = CARTESIAN_POINT ( 'NONE',  ( 1.469816272965879911, 0.1283753931104746893, -0.1820866141732285504 ) ) ;
#77354 = CARTESIAN_POINT ( 'NONE',  ( 1.456692913385827515, 0.2952755905511811885, 0.000000000000000000 ) ) ;
#77355 = PRODUCT_DEFINITION_CONTEXT ( 'detailed design', #74523, 'design' ) ;
#77356 = CARTESIAN_POINT ( 'NONE',  ( -0.07874015748031421014, -0.1870078740157479769, 0.3641732283464567677 ) ) ;
#77357 = CARTESIAN_POINT ( 'NONE',  ( 0.3392501089628018329, 0.1958661417322835607, -1.383202099737532942 ) ) ;
#77358 = CARTESIAN_POINT ( 'NONE',  ( -0.7283464566929126471, -0.5400638737290844871, 0.3530559997133364547 ) ) ;
#77359 = CARTESIAN_POINT ( 'NONE',  ( 1.364829396325459854, -0.6046776061558809534, -0.2411417322834644161 ) ) ;
#77360 = CARTESIAN_POINT ( 'NONE',  ( -0.1265901696524993347, 0.4724409448818895907, -0.08333333333333335646 ) ) ;
#77361 = CARTESIAN_POINT ( 'NONE',  ( -0.4068241469816264999, -0.3690944881889763329, 0.3153832671262228327 ) ) ;
#77362 = CARTESIAN_POINT ( 'NONE',  ( 0.04593175853018440641, 0.2952755905511810219, -0.1292274648535930437 ) ) ;
#77363 = CARTESIAN_POINT ( 'NONE',  ( 0.4527559055118117182, 0.1660481256975883668, -0.3530559997133364547 ) ) ;
#77364 = DIRECTION ( 'NONE',  ( 0.000000000000000000, 0.000000000000000000, 1.000000000000000000 ) ) ;
#77365 = CARTESIAN_POINT ( 'NONE',  ( 0.8661417322834652488, -0.1870078740157480601, -0.3641732283464567677 ) ) ;
#77366 = CARTESIAN_POINT ( 'NONE',  ( 5.463695987328526437E-16, -0.1870078740157479769, 0.3641732283464567677 ) ) ;
#77367 = CARTESIAN_POINT ( 'NONE',  ( 0.1771653543307093182, -0.5400638737290845981, -0.3530559997133363437 ) ) ;
#77368 = CARTESIAN_POINT ( 'NONE',  ( -1.364829396325458521, 0.2306618581243847221, -0.2411417322834647770 ) ) ;
#77369 = CARTESIAN_POINT ( 'NONE',  ( -0.5183727034120726440, 0.1771653543307087630, 0.09757992244046791164 ) ) ;
#77370 = DIRECTION ( 'NONE',  ( 0.000000000000000000, 0.000000000000000000, -1.000000000000000000 ) ) ;
#77371 = CARTESIAN_POINT ( 'NONE',  ( -1.017060367454067249, -0.05778040916215522460, 0.4822834645669289988 ) ) ;
#77372 = CARTESIAN_POINT ( 'NONE',  ( 0.1998031496062994128, -0.3460692066303957537, -0.9560367454068241511 ) ) ;
#77373 = CARTESIAN_POINT ( 'NONE',  ( -0.2867679344610365999, 0.2867679344610364889, -2.466535433070865757 ) ) ;
#77374 = CARTESIAN_POINT ( 'NONE',  ( 0.09842519685039434474, -0.4536011799217368745, -0.2665933059059886201 ) ) ;
#77375 = CARTESIAN_POINT ( 'NONE',  ( -0.6889763779527552368, 0.1660481256975885056, 0.3530559997133364547 ) ) ;
#77376 = VECTOR ( 'NONE', #42739, 39.37007874015748143 ) ;
#77377 = CARTESIAN_POINT ( 'NONE',  ( -0.9580052493438311334, 0.05413385826771626580, -0.4176697321401330321 ) ) ;
#77378 = CARTESIAN_POINT ( 'NONE',  ( -1.404199475065615932, -0.3690944881889765550, -0.3153832671262227771 ) ) ;
#77379 = ADVANCED_FACE ( 'NONE', ( #31911 ), #38222, .F. ) ;
#77380 = CARTESIAN_POINT ( 'NONE',  ( -0.7414698162729651543, -0.5511811023622046335, 0.09757992244046803654 ) ) ;
#77381 = CARTESIAN_POINT ( 'NONE',  ( -1.581364829396324945, -0.2845877964562159024, 0.3641732283464567677 ) ) ;
#77382 = CARTESIAN_POINT ( 'NONE',  ( 1.410761154855643795, -0.3162353388693405765, 0.4822834645669290543 ) ) ;
#77383 = CARTESIAN_POINT ( 'NONE',  ( -0.4724409448818898682, 5.785732909357575061E-17, -2.755905511811024056 ) ) ;
#77384 = CARTESIAN_POINT ( 'NONE',  ( 0.1958661417322836718, -0.3392501089628017219, -2.135846087435382401 ) ) ;
#77385 = ORIENTED_EDGE ( 'NONE', *, *, #19613, .T. ) ;
#77386 = CARTESIAN_POINT ( 'NONE',  ( 0.000000000000000000, 1.929133858267716661, 2.362204724409448620 ) ) ;
#77387 = CARTESIAN_POINT ( 'NONE',  ( 1.614173228346457378, 0.1771653543307087630, 0.000000000000000000 ) ) ;
#77388 = CARTESIAN_POINT ( 'NONE',  ( -1.437007874015747477, -0.5400638737290844871, 0.3530559997133364547 ) ) ;
#77389 = EDGE_CURVE ( 'NONE', #21108, #42501, #13400, .T. ) ;
#77390 = CARTESIAN_POINT ( 'NONE',  ( 1.082677165354331228, -0.5400638737290844871, 0.3530559997133364547 ) ) ;
#77391 = CARTESIAN_POINT ( 'NONE',  ( 4.797336870675656522E-17, -0.3917322834645670104, -1.895669291338582640 ) ) ;
#77392 = CARTESIAN_POINT ( 'NONE',  ( 1.581364829396326277, -0.2845877964562161244, -0.3641732283464567121 ) ) ;
#77393 = CARTESIAN_POINT ( 'NONE',  ( 0.6889763779527566800, -0.5400638737290844871, 0.3530559997133364547 ) ) ;
#77394 = CARTESIAN_POINT ( 'NONE',  ( 0.09186351706036827158, 0.05413385826771666132, 0.4176697321401328100 ) ) ;
#77395 = FACE_OUTER_BOUND ( 'NONE', #51934, .T. ) ;
#77396 = CARTESIAN_POINT ( 'NONE',  ( 0.000000000000000000, 0.03937007874015751446, 2.362204724409448620 ) ) ;
#77397 = CARTESIAN_POINT ( 'NONE',  ( 0.7414698162729663755, -0.5511811023622048555, -0.09757992244046775898 ) ) ;
#77398 = CARTESIAN_POINT ( 'NONE',  ( 0.1998031496062994405, -0.3460692066303958092, -1.194225721784776928 ) ) ;
#77399 = ORIENTED_EDGE ( 'NONE', *, *, #45400, .F. ) ;
#77400 = CARTESIAN_POINT ( 'NONE',  ( 0.1958661417322836718, -0.3392501089628017219, -0.08860199294719349472 ) ) ;
#77401 = ORIENTED_EDGE ( 'NONE', *, *, #78409, .F. ) ;
#77402 = CARTESIAN_POINT ( 'NONE',  ( 0.1377952755905518800, -0.5400638737290844871, 0.3530559997133364547 ) ) ;
#77403 = CARTESIAN_POINT ( 'NONE',  ( -1.496062992125983815, -0.1870078740157479769, 0.4822834645669291653 ) ) ;
#77404 = CARTESIAN_POINT ( 'NONE',  ( 0.4593175853018380828, 0.05413385826771626580, -0.4176697321401330321 ) ) ;
#77405 = CARTESIAN_POINT ( 'NONE',  ( 1.187664041994751285, -0.05778040916215522460, 0.4822834645669289988 ) ) ;
#77406 = CARTESIAN_POINT ( 'NONE',  ( 1.286089238845145033, 0.2306618581243848609, 0.2411417322834645549 ) ) ;
#77407 = CARTESIAN_POINT ( 'NONE',  ( -0.6496062992125976043, 0.1660481256975883668, -0.3530559997133364547 ) ) ;
#77408 = CARTESIAN_POINT ( 'NONE',  ( 0.1771653543307093182, 0.1660481256975885056, 0.3530559997133364547 ) ) ;
#77409 = CARTESIAN_POINT ( 'NONE',  ( -1.476377952755905110, 0.1660481256975885056, 0.3530559997133364547 ) ) ;
#77410 = CARTESIAN_POINT ( 'NONE',  ( 1.325459317585302665, 0.05413385826771626580, -0.4176697321401330321 ) ) ;
#77411 = CARTESIAN_POINT ( 'NONE',  ( 1.089238845144357759, 0.05413385826771626580, -0.4176697321401330321 ) ) ;
#77412 = CARTESIAN_POINT ( 'NONE',  ( -0.2296587926509179312, -0.3162353388693409650, -0.4822834645669289433 ) ) ;
#77413 = CARTESIAN_POINT ( 'NONE',  ( 0.3392501089628018329, 0.1958661417322835607, -0.2808398950131232863 ) ) ;
#77414 = CARTESIAN_POINT ( 'NONE',  ( 0.6102362204724416372, 0.07958543189024071263, -0.2665933059059888421 ) ) ;
#77415 = ORIENTED_EDGE ( 'NONE', *, *, #77389, .T. ) ;
#77416 = CARTESIAN_POINT ( 'NONE',  ( -0.3949938075777411628, 0.1058382717557497937, -0.6627296587926508886 ) ) ;
#77417 = ORIENTED_EDGE ( 'NONE', *, *, #82130, .T. ) ;
#77418 = CARTESIAN_POINT ( 'NONE',  ( -0.3477690288713905509, -0.5511811023622046335, 0.09757992244046803654 ) ) ;
#77419 = AXIS2_PLACEMENT_3D ( 'NONE', #36848, #75580, #75167 ) ;
#77420 = VECTOR ( 'NONE', #4780, 39.37007874015748143 ) ;
#77421 = CARTESIAN_POINT ( 'NONE',  ( 2.619388402063373533, 1.366082762360723901, -0.4426340671871345500 ) ) ;
#77422 = CARTESIAN_POINT ( 'NONE',  ( 0.2230971128608929543, 0.05413385826771626580, -0.4176697321401330321 ) ) ;
#77423 = CARTESIAN_POINT ( 'NONE',  ( 0.2099737532808405305, 0.2306618581243847221, -0.2411417322834647770 ) ) ;
#77424 = CARTESIAN_POINT ( 'NONE',  ( -1.049868766404198794, 0.2306618581243847221, -0.2411417322834647770 ) ) ;
#77425 = CARTESIAN_POINT ( 'NONE',  ( -0.3917322834645670104, -0.1049643490035307020, -1.774953698983938954 ) ) ;
#77426 = CARTESIAN_POINT ( 'NONE',  ( -1.574803149606298192, -0.1870078740157480879, -0.4822834645669291653 ) ) ;
#77427 = CARTESIAN_POINT ( 'NONE',  ( 0.08317790770047603366, 1.066208230691911174, 0.2524721893675162532 ) ) ;
#77428 = CARTESIAN_POINT ( 'NONE',  ( 0.7545931758530188826, -0.5511811023622046335, 0.09757992244046803654 ) ) ;
#77429 = CARTESIAN_POINT ( 'NONE',  ( 0.6627296587926517768, -0.6692913385826773087, -0.1292274648535924053 ) ) ;
#77430 = CARTESIAN_POINT ( 'NONE',  ( 0.5643044619422579178, 0.05413385826771666132, 0.4176697321401328100 ) ) ;
#77431 = CARTESIAN_POINT ( 'NONE',  ( -9.787531504996567848E-17, 0.3996062992125986035, -1.259842519685039353 ) ) ;
#77432 = CARTESIAN_POINT ( 'NONE',  ( -2.586150256253501478, 1.653403552777528596, 0.4602852883866567768 ) ) ;
#77433 = CARTESIAN_POINT ( 'NONE',  ( 0.3460692066303958092, 0.1998031496062993018, -0.6804461942257218343 ) ) ;
#77434 = CARTESIAN_POINT ( 'NONE',  ( -0.3996062992125986590, 0.1070741851644051723, 0.04790026246719156916 ) ) ;
#77435 = CARTESIAN_POINT ( 'NONE',  ( -0.1049868766404193215, 0.2306618581243847221, -0.2411417322834647770 ) ) ;
#77436 = CARTESIAN_POINT ( 'NONE',  ( -0.1998031496062991907, -0.3460692066303959757, -2.742782152230971437 ) ) ;
#77437 =( BOUNDED_CURVE ( )  B_SPLINE_CURVE ( 1, ( #38214, #44923 ),
 .UNSPECIFIED., .F., .F. ) 
 B_SPLINE_CURVE_WITH_KNOTS ( ( 2, 2 ),
 ( 0.000000000000000000, 0.001999999999999998307 ),
 .UNSPECIFIED. ) 
 CURVE ( )  GEOMETRIC_REPRESENTATION_ITEM ( )  RATIONAL_B_SPLINE_CURVE ( ( 0.9875488213027527884, 0.9875488213027527884 ) ) 
 REPRESENTATION_ITEM ( '' )  );
#77438 = CARTESIAN_POINT ( 'NONE',  ( 0.1049643490035303689, 0.3917322834645670104, -2.125328083989501682 ) ) ;
#77439 = CARTESIAN_POINT ( 'NONE',  ( -0.9973753280839886548, 0.1283753931104748280, 0.1820866141732283561 ) ) ;
#77440 = CARTESIAN_POINT ( 'NONE',  ( 1.469816272965879911, 0.2306618581243847221, -0.2411417322834647770 ) ) ;
#77441 = AXIS2_PLACEMENT_3D ( 'NONE', #59515, #15335, #9426 ) ;
#77442 = CARTESIAN_POINT ( 'NONE',  ( 1.161417322834646493, -0.5400638737290844871, 0.3530559997133364547 ) ) ;
#77443 = CARTESIAN_POINT ( 'NONE',  ( 0.3215223097112867578, -0.2845877964562161244, -0.3641732283464567121 ) ) ;
#77444 = CARTESIAN_POINT ( 'NONE',  ( 0.6496062992125991586, 0.1660481256975885056, 0.3530559997133364547 ) ) ;
#77445 = CARTESIAN_POINT ( 'NONE',  ( 0.4724409448818896462, 0.1265901696524990294, -1.618766404199474929 ) ) ;
#77446 = CARTESIAN_POINT ( 'NONE',  ( 0.4724409448818904789, -0.1870078740157480601, -0.3641732283464567677 ) ) ;
#77447 = CARTESIAN_POINT ( 'NONE',  ( 0.1509186351706042484, -0.3162353388693405765, 0.4822834645669290543 ) ) ;
#77448 = CARTESIAN_POINT ( 'NONE',  ( -0.3420746716998660508, -0.1974969037888706924, -1.389107611548556553 ) ) ;
#77449 = CARTESIAN_POINT ( 'NONE',  ( -1.384514435695537005, 0.2952755905511811885, 0.1292274648535926551 ) ) ;
#77450 = CARTESIAN_POINT ( 'NONE',  ( 0.4461942257217855201, -0.5023911411419708095, 0.1820866141732285504 ) ) ;
#77451 = CARTESIAN_POINT ( 'NONE',  ( -2.554262525012342966, 1.537401574803149984, -0.4744094488188975722 ) ) ;
#77452 = CARTESIAN_POINT ( 'NONE',  ( -0.5839895013123351797, 0.2952755905511810774, -0.1292274648535930714 ) ) ;
#77453 = CARTESIAN_POINT ( 'NONE',  ( -0.2755905511811015396, -0.5511811023622047445, 6.969142054262312111E-17 ) ) ;
#77454 = DIRECTION ( 'NONE',  ( -1.000000000000000000, 1.445602896647338917E-16, -0.000000000000000000 ) ) ;
#77455 = CARTESIAN_POINT ( 'NONE',  ( -0.8727034120734901146, -0.05778040916215560624, -0.4822834645669293319 ) ) ;
#77456 = CARTESIAN_POINT ( 'NONE',  ( -0.03280839895013062252, 0.2952755905511810774, -0.1292274648535930714 ) ) ;
#77457 = CARTESIAN_POINT ( 'NONE',  ( 0.2296587926509192634, -0.08942795157528024563, -0.3641732283464568787 ) ) ;
#77458 = CARTESIAN_POINT ( 'NONE',  ( 0.3996062992125984925, 0.1070741851644054637, -2.091207349081364963 ) ) ;
#77459 = CARTESIAN_POINT ( 'NONE',  ( -0.1968503937007867743, 0.2952755905511811885, 0.000000000000000000 ) ) ;
#77460 = CARTESIAN_POINT ( 'NONE',  ( 0.1958661417322834497, 0.3392501089628018329, -1.956673597603987957 ) ) ;
#77461 = CARTESIAN_POINT ( 'NONE',  ( 0.6364829396325465405, -0.2845877964562161244, -0.3641732283464567121 ) ) ;
#77462 = CARTESIAN_POINT ( 'NONE',  ( 1.312335958005249825, 0.2306618581243847221, -0.2411417322834647770 ) ) ;
#77463 = CARTESIAN_POINT ( 'NONE',  ( -0.9776902887139098386, -0.5511811023622046335, 0.09757992244046803654 ) ) ;
#77464 = ADVANCED_FACE ( 'NONE', ( #20547 ), #19702, .F. ) ;
#77465 = CARTESIAN_POINT ( 'NONE',  ( -1.062992125984250968, 0.1771653543307087630, 0.000000000000000000 ) ) ;
#77466 = CARTESIAN_POINT ( 'NONE',  ( -0.5249343832020990641, 0.2306618581243848609, 0.2411417322834645549 ) ) ;
#77467 = CARTESIAN_POINT ( 'NONE',  ( -0.006561679790025524116, -0.3162353388693405765, 0.4822834645669290543 ) ) ;
#77468 = CARTESIAN_POINT ( 'NONE',  ( 0.7677165354330716118, 0.07958543189024071263, -0.2665933059059888421 ) ) ;
#77469 = CARTESIAN_POINT ( 'NONE',  ( -0.3458507752293909498, 0.3458507752293908388, -2.381889763779527769 ) ) ;
#77470 = CARTESIAN_POINT ( 'NONE',  ( 1.062992125984252745, -0.5511811023622047445, 6.969142054262312111E-17 ) ) ;
#77471 = ADVANCED_FACE ( 'NONE', ( #26009 ), #33585, .T. ) ;
#77472 = CARTESIAN_POINT ( 'NONE',  ( 0.6430446194225729606, -0.4281496062992127816, -0.4176697321401328100 ) ) ;
#77473 = CARTESIAN_POINT ( 'NONE',  ( -0.2925321140481932369, 0.2925321140481931259, 0.2185039370078740162 ) ) ;
#77474 = CARTESIAN_POINT ( 'NONE',  ( -0.1771653543307080136, -0.5400638737290844871, 0.3530559997133364547 ) ) ;
#77475 = AXIS2_PLACEMENT_3D ( 'NONE', #27967, #66702, #9035 ) ;
#77476 = CARTESIAN_POINT ( 'NONE',  ( -0.3392501089628017219, -0.1958661417322836718, -1.396981627296587813 ) ) ;
#77477 = CARTESIAN_POINT ( 'NONE',  ( 1.410761154855643795, -0.2845877964562159024, 0.3641732283464567677 ) ) ;
#77478 = CARTESIAN_POINT ( 'NONE',  ( 0.2821522309711292364, 0.2952755905511810774, -0.1292274648535930714 ) ) ;
#77479 = VECTOR ( 'NONE', #52428, 39.37007874015748143 ) ;
#77480 = CARTESIAN_POINT ( 'NONE',  ( -0.06561679790026180015, 0.05413385826771666132, 0.4176697321401328100 ) ) ;
#77481 = CARTESIAN_POINT ( 'NONE',  ( 0.5839895013123366230, 0.2066929133858267931, 0.1054918080437490802 ) ) ;
#77482 = CARTESIAN_POINT ( 'NONE',  ( -0.05905511811023545637, 0.07958543189024085140, 0.2665933059059887866 ) ) ;
#77483 = CARTESIAN_POINT ( 'NONE',  ( 0.6627296587926517768, -0.6692913385826773087, -0.1292274648535924053 ) ) ;
#77484 = CARTESIAN_POINT ( 'NONE',  ( -0.3937007874015740483, -0.1870078740157480601, -0.3641732283464567677 ) ) ;
#77485 = CARTESIAN_POINT ( 'NONE',  ( -0.5249343832020990641, 0.2306618581243848609, 0.2411417322834645549 ) ) ;
#77486 = CARTESIAN_POINT ( 'NONE',  ( 0.7989874411535518028, 0.02791078216816225699, 0.4328096321851905293 ) ) ;
#77487 = CARTESIAN_POINT ( 'NONE',  ( -0.1246719160104980823, 0.2952755905511811885, 0.1292274648535926551 ) ) ;
#77488 = CARTESIAN_POINT ( 'NONE',  ( -1.227034120734907141, -0.6692913385826773087, -0.1292274648535924053 ) ) ;
#77489 = CARTESIAN_POINT ( 'NONE',  ( -0.8858267716535425107, 0.07958543189024071263, -0.2665933059059888421 ) ) ;
#77490 = CARTESIAN_POINT ( 'NONE',  ( 0.4199475065616803948, -0.6046776061558809534, -0.2411417322834644161 ) ) ;
#77491 = CARTESIAN_POINT ( 'NONE',  ( -1.417322834645668772, -0.1870078740157479769, 0.4822834645669291653 ) ) ;
#77492 = CARTESIAN_POINT ( 'NONE',  ( -0.1509186351706028884, -0.3162353388693409650, -0.4822834645669289433 ) ) ;
#77493 = CARTESIAN_POINT ( 'NONE',  ( 0.4744094488189052328, 1.537401574803149984, -2.170146923806634653 ) ) ;
#77495 = CARTESIAN_POINT ( 'NONE',  ( 1.154855643044620184, 0.2306618581243847221, -0.2411417322834647770 ) ) ;
#77494 = CARTESIAN_POINT ( 'NONE',  ( -0.8792650918635160906, 0.05413385826771626580, -0.4176697321401330321 ) ) ;
#77496 = CARTESIAN_POINT ( 'NONE',  ( 1.443569553805774897, -0.6046776061558809534, -0.2411417322834644161 ) ) ;
#77497 = CARTESIAN_POINT ( 'NONE',  ( -0.3392501089628019995, 0.1958661417322832277, -2.538057742782152015 ) ) ;
#77499 = AXIS2_PLACEMENT_3D ( 'NONE', #35629, #54973, #61291 ) ;
#77498 = DIRECTION ( 'NONE',  ( 0.000000000000000000, -1.000000000000000000, 0.000000000000000000 ) ) ;
#77500 = CARTESIAN_POINT ( 'NONE',  ( -1.135170603674539924, -0.6692913385826771977, 0.1292274648535927661 ) ) ;
#77501 = CARTESIAN_POINT ( 'NONE',  ( 0.3458507752293908943, -0.3458507752293908943, -0.8858267716535430658 ) ) ;
#77502 = CARTESIAN_POINT ( 'NONE',  ( -0.3996062992125986035, -0.1070741851644056997, 0.1115485564304461580 ) ) ;
#77503 = ORIENTED_EDGE ( 'NONE', *, *, #27189, .F. ) ;
#77504 = CARTESIAN_POINT ( 'NONE',  ( -0.01968503937007793844, 0.07958543189024071263, -0.2665933059059888421 ) ) ;
#77505 = CARTESIAN_POINT ( 'NONE',  ( -0.1049643490035307020, 0.3917322834645669549, -1.888451443569553412 ) ) ;
#77506 = ORIENTED_EDGE ( 'NONE', *, *, #54690, .F. ) ;
#77507 = CARTESIAN_POINT ( 'NONE',  ( 0.1574803149606306130, -0.1870078740157479769, 0.4822834645669291653 ) ) ;
#77508 = CARTESIAN_POINT ( 'NONE',  ( 0.4330708661417329575, -0.6692913385826771977, 8.415575281601705876E-17 ) ) ;
#77509 = CARTESIAN_POINT ( 'NONE',  ( 5.785732909357575061E-17, -0.4724409448818898682, -2.755905511811023612 ) ) ;
#77510 = CARTESIAN_POINT ( 'NONE',  ( -0.5408419829024493364, -1.094630224652485432E-15, 0.4281993546915541238 ) ) ;
#77511 = CARTESIAN_POINT ( 'NONE',  ( -0.4790026246719152336, -0.08942795157528024563, -0.3641732283464568787 ) ) ;
#77512 = CARTESIAN_POINT ( 'NONE',  ( 6.372542394380578105E-15, 1.062992125984252523, -1.629220936382730134 ) ) ;
#77513 = CARTESIAN_POINT ( 'NONE',  ( 0.7480314960629927956, 0.2952755905511811885, 0.000000000000000000 ) ) ;
#77514 = CARTESIAN_POINT ( 'NONE',  ( 0.8923884514435701520, -0.5023911411419708095, -0.1820866141732282451 ) ) ;
#77515 = CARTESIAN_POINT ( 'NONE',  ( -0.2230971128608915943, 0.05413385826771666132, 0.4176697321401328100 ) ) ;
#77516 = CARTESIAN_POINT ( 'NONE',  ( -0.2867679344610366554, 0.2867679344610365444, -1.202080421750969741 ) ) ;
#77517 = CARTESIAN_POINT ( 'NONE',  ( -0.7020997375328074108, -0.05778040916215522460, 0.4822834645669289988 ) ) ;
#77518 = CARTESIAN_POINT ( 'NONE',  ( -1.227034120734907585, 0.1771653543307087630, 0.09757992244046791164 ) ) ;
#77519 = CARTESIAN_POINT ( 'NONE',  ( -1.043307086614172707, 0.1660481256975883668, -0.3530559997133364547 ) ) ;
#77520 = CARTESIAN_POINT ( 'NONE',  ( 1.318897637795276356, -0.5400638737290844871, 0.3530559997133364547 ) ) ;
#77521 = CARTESIAN_POINT ( 'NONE',  ( -0.4744094488188894121, 1.537401574803149984, -2.170146923806595574 ) ) ;
#77522 = VERTEX_POINT ( 'NONE', #52085 ) ;
#77523 = CARTESIAN_POINT ( 'NONE',  ( -0.1049643490035302301, -0.3917322834645671770, -2.273641363025933781 ) ) ;
#77524 = CARTESIAN_POINT ( 'NONE',  ( -0.07217847769028787330, -0.05778040916215522460, 0.4822834645669289988 ) ) ;
#77525 = ORIENTED_EDGE ( 'NONE', *, *, #81282, .T. ) ;
#77526 = CARTESIAN_POINT ( 'NONE',  ( -0.5971128608923877978, 0.2952755905511811885, 0.1292274648535926551 ) ) ;
#77527 = CARTESIAN_POINT ( 'NONE',  ( 1.489501312335958172, -0.05778040916215560624, -0.4822834645669293319 ) ) ;
#77528 = CARTESIAN_POINT ( 'NONE',  ( 1.062992125984252745, -0.6692913385826771977, 8.415575281601705876E-17 ) ) ;
#77529 = B_SPLINE_CURVE_WITH_KNOTS ( 'NONE', 3,
 ( #15775, #29620, #9857, #10278 ),
 .UNSPECIFIED., .F., .F.,
 ( 4, 4 ),
 ( 0.08422315286269969892, 0.08567085022608438016 ),
 .UNSPECIFIED. ) ;
#77530 = CARTESIAN_POINT ( 'NONE',  ( 0.2427821522309716595, -0.3162353388693409650, -0.4822834645669289433 ) ) ;
#77531 = CARTESIAN_POINT ( 'NONE',  ( 0.01312335958005323398, -0.4281496062992127816, -0.4176697321401328100 ) ) ;
#77532 = CARTESIAN_POINT ( 'NONE',  ( 4.797336870675656522E-17, -0.3917322834645670104, -1.738188976377952777 ) ) ;
#77533 = CARTESIAN_POINT ( 'NONE',  ( -1.213910761154854745, 0.2952755905511810774, -0.1292274648535930714 ) ) ;
#77534 = CARTESIAN_POINT ( 'NONE',  ( -0.3740157480314953431, 0.1660481256975885056, 0.3530559997133364547 ) ) ;
#77535 = CARTESIAN_POINT ( 'NONE',  ( -0.3018372703412066094, -0.3690944881889765550, -0.3153832671262227771 ) ) ;
#77536 = CARTESIAN_POINT ( 'NONE',  ( 2.570293882282742803, 2.742780008954323723, -0.5314960629921260393 ) ) ;
#77537 = CARTESIAN_POINT ( 'NONE',  ( 1.332020997375329197, -0.3162353388693405765, 0.4822834645669290543 ) ) ;
#77538 = CARTESIAN_POINT ( 'NONE',  ( -0.6955380577427815458, -0.4281496062992127816, -0.4176697321401328100 ) ) ;
#77539 = CARTESIAN_POINT ( 'NONE',  ( 0.2559055118110243887, 0.1012011053420777407, 0.2882089793578256898 ) ) ;
#77540 = CARTESIAN_POINT ( 'NONE',  ( 1.010498687664042716, 0.05413385826771626580, -0.4176697321401330321 ) ) ;
#77541 = DIRECTION ( 'NONE',  ( 0.000000000000000000, 0.000000000000000000, -1.000000000000000000 ) ) ;
#77542 = EDGE_LOOP ( 'NONE', ( #72854, #7188, #39845, #49953 ) ) ;
#77543 = ORIENTED_EDGE ( 'NONE', *, *, #7379, .F. ) ;
#77544 = CONICAL_SURFACE ( 'NONE', #3583, 0.1190944881889763746, 0.8726646259971648778 ) ;
#77545 = CARTESIAN_POINT ( 'NONE',  ( 0.3149606299212606708, -0.1870078740157480879, -0.4822834645669291653 ) ) ;
#77546 = CARTESIAN_POINT ( 'NONE',  ( -0.4986876640419942164, -0.5023911411419708095, 0.1820866141732285504 ) ) ;
#77547 = AXIS2_PLACEMENT_3D ( 'NONE', #7767, #40993, #20385 ) ;
#77548 = AXIS2_PLACEMENT_3D ( 'NONE', #60150, #66897, #29400 ) ;
#77550 = CARTESIAN_POINT ( 'NONE',  ( 0.1265901696524990572, -0.4724409448818897017, -0.4002624671916010235 ) ) ;
#77549 = CARTESIAN_POINT ( 'NONE',  ( 1.463254593175853824, -0.5511811023622046335, 0.09757992244046803654 ) ) ;
#77551 = CARTESIAN_POINT ( 'NONE',  ( 0.4724409448818898682, 2.892866454678787531E-17, -0.1948818897637795422 ) ) ;
#77552 = CARTESIAN_POINT ( 'NONE',  ( 0.4677827689124922084, 0.03937007874015747977, -2.154527559055118946 ) ) ;
#77553 = CARTESIAN_POINT ( 'NONE',  ( 1.410761154855643795, -0.3162353388693405765, 0.4822834645669290543 ) ) ;
#77554 = CARTESIAN_POINT ( 'NONE',  ( 0.3949938075777409408, -0.1058382717557499186, -0.1883202099737532886 ) ) ;
#77555 = CARTESIAN_POINT ( 'NONE',  ( 0.05249343832021075018, 0.2306618581243847221, -0.2411417322834647770 ) ) ;
#77556 = CARTESIAN_POINT ( 'NONE',  ( -1.568241469816272105, -0.3162353388693409650, -0.4822834645669289433 ) ) ;
#77557 = CARTESIAN_POINT ( 'NONE',  ( -1.587926509186350810, -0.4281496062992124485, 0.4176697321401328655 ) ) ;
#77558 = CARTESIAN_POINT ( 'NONE',  ( 0.3608923884514443348, 0.2952755905511810774, -0.1292274648535930714 ) ) ;
#77559 = CARTESIAN_POINT ( 'NONE',  ( -0.3949938075777408852, -0.1058382717557502933, 0.03477690288713909672 ) ) ;
#77560 = CARTESIAN_POINT ( 'NONE',  ( 1.528871391076116026, 0.2952755905511811885, 0.1292274648535926551 ) ) ;
#77561 = CARTESIAN_POINT ( 'NONE',  ( 0.6299212598425204535, -0.1870078740157479769, 0.4822834645669291653 ) ) ;
#77562 = CARTESIAN_POINT ( 'NONE',  ( 0.8464566929133866546, -0.4536011799217367080, 0.2665933059059888421 ) ) ;
#77563 = CARTESIAN_POINT ( 'NONE',  ( -0.01968503937007793844, 0.1660481256975883391, -0.3530559997133364547 ) ) ;
#77564 = CARTESIAN_POINT ( 'NONE',  ( 0.8267716535433078384, -0.5511811023622047445, 6.969142054262312111E-17 ) ) ;
#77565 = CARTESIAN_POINT ( 'NONE',  ( -1.246719160104985846, -0.4281496062992127816, -0.4176697321401328100 ) ) ;
#77566 = CARTESIAN_POINT ( 'NONE',  ( -0.1998031496062991630, -0.3460692066303959202, -0.7723097112860892732 ) ) ;
#77567 = CARTESIAN_POINT ( 'NONE',  ( 1.174540682414699111, -0.3162353388693405765, 0.4822834645669290543 ) ) ;
#77568 = CARTESIAN_POINT ( 'NONE',  ( -0.3917322834645671215, 0.1049643490035301469, -0.8123359580052491591 ) ) ;
#77570 = CARTESIAN_POINT ( 'NONE',  ( -0.1265901696524986964, -0.4724409448818899238, -0.4639107611548556331 ) ) ;
#77569 = CARTESIAN_POINT ( 'NONE',  ( 0.8136482939632553313, -0.6046776061558809534, -0.2411417322834644161 ) ) ;
#77571 = CARTESIAN_POINT ( 'NONE',  ( -0.3543307086614165824, 0.2066929133858268208, 0.000000000000000000 ) ) ;
#77572 = CARTESIAN_POINT ( 'NONE',  ( 0.2952755905511816326, -0.4536011799217367080, 0.2665933059059888421 ) ) ;
#77573 = ADVANCED_FACE ( 'NONE', ( #18870 ), #35444, .F. ) ;
#77574 = CARTESIAN_POINT ( 'NONE',  ( 0.4396325459317593221, 0.2952755905511810774, -0.1292274648535930714 ) ) ;
#77575 = FACE_OUTER_BOUND ( 'NONE', #69562, .T. ) ;
#77576 = CARTESIAN_POINT ( 'NONE',  ( -0.8333333333333323711, -0.5511811023622048555, -0.09757992244046775898 ) ) ;
#77577 = CARTESIAN_POINT ( 'NONE',  ( -1.089238845144356427, 0.05413385826771666132, 0.4176697321401328100 ) ) ;
#77578 = CARTESIAN_POINT ( 'NONE',  ( 0.9711286089238851948, -0.6046776061558809534, -0.2411417322834644161 ) ) ;
#77579 = CARTESIAN_POINT ( 'NONE',  ( -1.056430446194224881, 0.2952755905511810774, -0.1292274648535930714 ) ) ;
#77580 = CARTESIAN_POINT ( 'NONE',  ( 0.8202099737532814183, -0.6692913385826773087, -0.1292274648535924053 ) ) ;
#77581 = CARTESIAN_POINT ( 'NONE',  ( -1.233595800524933894, -0.5023911411419708095, -0.1820866141732282451 ) ) ;
#77582 = CARTESIAN_POINT ( 'NONE',  ( 1.044213977778944535, 1.299421820005424166, -0.4106937405380285400 ) ) ;
#77583 = CARTESIAN_POINT ( 'NONE',  ( 1.010498687664042716, 0.05413385826771626580, -0.4176697321401330321 ) ) ;
#77584 = CARTESIAN_POINT ( 'NONE',  ( -0.2362204724409447953, -0.4091458600556404646, -2.662073490813648746 ) ) ;
#77585 = FACE_OUTER_BOUND ( 'NONE', #8381, .T. ) ;
#77586 = CARTESIAN_POINT ( 'NONE',  ( 1.515748031496063408, 0.1660481256975885056, 0.3530559997133364547 ) ) ;
#77587 = CARTESIAN_POINT ( 'NONE',  ( -1.102362204724408601, -0.1870078740157479769, 0.3641732283464567677 ) ) ;
#77588 = CARTESIAN_POINT ( 'NONE',  ( 1.169606216052559544, -4.479759449472349425E-16, -0.3791483426435169335 ) ) ;
#77589 = CARTESIAN_POINT ( 'NONE',  ( -1.174540682414697335, -0.08942795157527998196, 0.3641732283464567121 ) ) ;
#77590 = CARTESIAN_POINT ( 'NONE',  ( -0.3740157480314953431, 0.07958543189024085140, 0.2665933059059887866 ) ) ;
#77591 = CARTESIAN_POINT ( 'NONE',  ( -1.732283464566928277, -0.1870078740157479769, 0.3641732283464567677 ) ) ;
#77592 = CARTESIAN_POINT ( 'NONE',  ( 1.017060367454068581, -0.08942795157528024563, -0.3641732283464568787 ) ) ;
#77593 = CARTESIAN_POINT ( 'NONE',  ( 0.6692913385826778638, -0.6692913385826771977, 8.415575281601705876E-17 ) ) ;
#77594 = CARTESIAN_POINT ( 'NONE',  ( 1.095800524934383846, -0.3162353388693405765, 0.4822834645669290543 ) ) ;
#77595 = CARTESIAN_POINT ( 'NONE',  ( -0.05249343832020911260, 0.2306618581243848609, 0.2411417322834645549 ) ) ;
#77596 = CARTESIAN_POINT ( 'NONE',  ( 0.6364829396325465405, -0.08942795157527998196, 0.3641732283464567121 ) ) ;
#77598 = CARTESIAN_POINT ( 'NONE',  ( 1.541994750656168645, -0.6692913385826771977, 0.1292274648535927661 ) ) ;
#77597 = AXIS2_PLACEMENT_3D ( 'NONE', #51381, #64034, #39618 ) ;
#77599 = DIRECTION ( 'NONE',  ( -0.000000000000000000, -1.000000000000000000, -0.000000000000000000 ) ) ;
#77600 = CARTESIAN_POINT ( 'NONE',  ( -0.6692913385826764205, -0.6692913385826771977, 8.415575281601705876E-17 ) ) ;
#77601 = CARTESIAN_POINT ( 'NONE',  ( -0.3996062992125986590, 0.1070741851644051862, -0.1902887139107611592 ) ) ;
#77602 = DIRECTION ( 'NONE',  ( -3.096699300667737957E-16, 1.000000000000000000, -0.000000000000000000 ) ) ;
#77603 = CARTESIAN_POINT ( 'NONE',  ( -0.1049868766404193215, 0.2306618581243847221, -0.2411417322834647770 ) ) ;
#77604 = AXIS2_PLACEMENT_3D ( 'NONE', #61494, #72887, #68241 ) ;
#77605 = CARTESIAN_POINT ( 'NONE',  ( -0.3740157480314953431, 0.1660481256975885056, 0.3530559997133364547 ) ) ;
#77606 = CARTESIAN_POINT ( 'NONE',  ( 0.4002624671916016896, -0.3162353388693409650, -0.4822834645669289433 ) ) ;
#77607 = CARTESIAN_POINT ( 'NONE',  ( -0.1998031496062991907, -0.3460692066303959757, -2.427821522309711266 ) ) ;
#77608 = CARTESIAN_POINT ( 'NONE',  ( 0.3420746716998659953, 0.1974969037888705536, -1.863517060367453793 ) ) ;
#77609 = CARTESIAN_POINT ( 'NONE',  ( -0.3392501089628019995, 0.1958661417322832277, -0.6482939632545930975 ) ) ;
#77610 = CARTESIAN_POINT ( 'NONE',  ( 0.2747679750349198979, -0.1085817515558208796, 5.561517368279697671 ) ) ;
#77611 = CARTESIAN_POINT ( 'NONE',  ( 0.3392501089628018884, -0.1958661417322834220, -0.8845144356955378928 ) ) ;
#77612 = CARTESIAN_POINT ( 'NONE',  ( -0.7480314960629914633, 0.1771653543307087630, 0.000000000000000000 ) ) ;
#77613 = CARTESIAN_POINT ( 'NONE',  ( 0.1958661417322836440, -0.3392501089628017219, -1.028871391076115360 ) ) ;
#77614 = CARTESIAN_POINT ( 'NONE',  ( -1.115485564304461219, -0.4281496062992124485, 0.4176697321401328655 ) ) ;
#77615 = CARTESIAN_POINT ( 'NONE',  ( 0.3917322834645669549, 2.398668435337827645E-17, 0.1168172160443062824 ) ) ;
#77616 = CARTESIAN_POINT ( 'NONE',  ( 0.5118110236220480003, -0.6692913385826771977, 8.415575281601705876E-17 ) ) ;
#77617 = CARTESIAN_POINT ( 'NONE',  ( -0.06561679790026180015, -0.3690944881889765550, -0.3153832671262227771 ) ) ;
#77618 = CARTESIAN_POINT ( 'NONE',  ( 1.351706036745407458, -0.4281496062992127816, -0.4176697321401328100 ) ) ;
#77619 = CARTESIAN_POINT ( 'NONE',  ( 0.3083989501312343062, -0.3162353388693405765, 0.4822834645669290543 ) ) ;
#77620 = CARTESIAN_POINT ( 'NONE',  ( -1.614173228346457378, 1.881821177735609085, 0.1372047244094476981 ) ) ;
#77621 = CARTESIAN_POINT ( 'NONE',  ( 0.1070741851644053527, 0.3996062992125986590, -2.670603674540682260 ) ) ;
#77622 = CARTESIAN_POINT ( 'NONE',  ( 4.797336870675656522E-17, -0.3917322834645670659, -1.177840838091550602 ) ) ;
#77623 = CARTESIAN_POINT ( 'NONE',  ( 1.135170603674541256, -0.6692913385826773087, -0.1292274648535924053 ) ) ;
#77624 = CARTESIAN_POINT ( 'NONE',  ( 0.4527559055118117182, -0.5400638737290844871, 0.3530559997133364547 ) ) ;
#77625 = CARTESIAN_POINT ( 'NONE',  ( 0.1771653543307093182, 0.1660481256975885056, 0.3530559997133364547 ) ) ;
#77626 = CARTESIAN_POINT ( 'NONE',  ( 0.9645669291338588858, 0.07958543189024085140, 0.2665933059059887866 ) ) ;
#77627 = CARTESIAN_POINT ( 'NONE',  ( 1.496062992125985147, -0.1870078740157479769, 0.4822834645669291653 ) ) ;
#77628 = CARTESIAN_POINT ( 'NONE',  ( -9.594673741351313045E-17, 0.3917322834645670104, -0.7145669291338584417 ) ) ;
#77629 = CARTESIAN_POINT ( 'NONE',  ( 0.1509186351706042484, -0.3162353388693405765, 0.4822834645669290543 ) ) ;
#77630 = CARTESIAN_POINT ( 'NONE',  ( 0.8661417322834653598, -0.1870078740157479769, 0.4822834645669291653 ) ) ;
#77631 = CARTESIAN_POINT ( 'NONE',  ( 0.2887139107611556010, 0.2306618581243847221, -0.2411417322834647770 ) ) ;
#77632 = CARTESIAN_POINT ( 'NONE',  ( 1.351706036745407680, -0.004921259842519576551, 0.3153832671262227771 ) ) ;
#77633 = CARTESIAN_POINT ( 'NONE',  ( -0.8136482939632537770, -0.6046776061558807314, 0.2411417322834647770 ) ) ;
#77634 = CARTESIAN_POINT ( 'NONE',  ( -1.272965879265091305, -0.4281496062992124485, 0.4176697321401328655 ) ) ;
#77635 = CARTESIAN_POINT ( 'NONE',  ( 1.141732283464567566, 0.2952755905511811885, 0.000000000000000000 ) ) ;
#77636 = CARTESIAN_POINT ( 'NONE',  ( -0.7137454485294950635, 2.362204724409448620, -0.4917280318828581298 ) ) ;
#77637 = CARTESIAN_POINT ( 'NONE',  ( -0.1958661417322836718, 0.3392501089628017219, -1.737532808398950079 ) ) ;
#77638 = CARTESIAN_POINT ( 'NONE',  ( 1.548556430446194954, 0.2306618581243847221, -0.2411417322834647770 ) ) ;
#77639 = ORIENTED_EDGE ( 'NONE', *, *, #28151, .F. ) ;
#77640 = CARTESIAN_POINT ( 'NONE',  ( -0.1070741851644056997, 0.3996062992125986035, 0.1509186351706036100 ) ) ;
#77641 = ORIENTED_EDGE ( 'NONE', *, *, #73388, .T. ) ;
#77642 = CARTESIAN_POINT ( 'NONE',  ( 1.535433070866142558, 0.2952755905511811885, 0.000000000000000000 ) ) ;
#77643 = CARTESIAN_POINT ( 'NONE',  ( 0.7545931758530188826, -0.5511811023622046335, 0.09757992244046803654 ) ) ;
#77644 = CARTESIAN_POINT ( 'NONE',  ( -0.4091458600556405756, 0.2362204724409446288, -2.465223097112860806 ) ) ;
#77645 = CARTESIAN_POINT ( 'NONE',  ( -0.03430998917087550032, 1.064156075168070537, 2.872937013333135337 ) ) ;
#77646 = CARTESIAN_POINT ( 'NONE',  ( 0.7749820319012125092, 2.784432375088962958E-17, -0.3464511005275205946 ) ) ;
#77647 = CARTESIAN_POINT ( 'NONE',  ( 0.1049643490035304938, -0.3917322834645669549, -0.7998687664041995715 ) ) ;
#77648 = CARTESIAN_POINT ( 'NONE',  ( -1.095800524934382292, -0.2845877964562161244, -0.3641732283464567121 ) ) ;
#77649 = CARTESIAN_POINT ( 'NONE',  ( -1.627296587926508442, -0.5023911411419708095, -0.1820866141732282451 ) ) ;
#77650 = CARTESIAN_POINT ( 'NONE',  ( -1.522309711286088607, -0.6046776061558807314, 0.2411417322834647770 ) ) ;
#77651 = CARTESIAN_POINT ( 'NONE',  ( -0.2427821522309703550, -0.05778040916215560624, -0.4822834645669293319 ) ) ;
#77652 = CARTESIAN_POINT ( 'NONE',  ( 1.541994750656168645, -0.6692913385826771977, 0.1292274648535927661 ) ) ;
#77653 = ORIENTED_EDGE ( 'NONE', *, *, #72813, .F. ) ;
#77654 = DIRECTION ( 'NONE',  ( 1.000000000000000000, -0.000000000000000000, -0.000000000000000000 ) ) ;
#77655 = DIRECTION ( 'NONE',  ( 6.982962677686266711E-15, 0.000000000000000000, -1.000000000000000000 ) ) ;
#77656 = CARTESIAN_POINT ( 'NONE',  ( -1.614173228346457378, 0.7794589730111965986, 0.1372047244094476981 ) ) ;
#77657 = DIRECTION ( 'NONE',  ( 0.000000000000000000, -1.000000000000000000, 0.000000000000000000 ) ) ;
#77658 = CARTESIAN_POINT ( 'NONE',  ( -1.115485564304461219, -0.004921259842519870586, -0.3153832671262229437 ) ) ;
#77659 = ADVANCED_FACE ( 'NONE', ( #12984 ), #38640, .F. ) ;
#77660 = CARTESIAN_POINT ( 'NONE',  ( -1.535433070866141225, -0.6692913385826771977, 8.415575281601705876E-17 ) ) ;
#77661 = CARTESIAN_POINT ( 'NONE',  ( 0.4658792650918641698, -0.05778040916215560624, -0.4822834645669293319 ) ) ;
#77662 = ORIENTED_EDGE ( 'NONE', *, *, #76404, .T. ) ;
#77664 = CYLINDRICAL_SURFACE ( 'NONE', #31738, 1.181102362204724310 ) ;
#77663 = LINE ( 'NONE', #51536, #58367 ) ;
#77665 = CARTESIAN_POINT ( 'NONE',  ( 1.292650918635171564, -0.6692913385826773087, -0.1292274648535924053 ) ) ;
#77666 = CARTESIAN_POINT ( 'NONE',  ( -1.673228346456691717, 0.1660481256975883668, -0.3530559997133364547 ) ) ;
#77667 = CARTESIAN_POINT ( 'NONE',  ( 0.2867679344610365999, 0.2867679344610365999, -0.8477497130895521593 ) ) ;
#77668 = ADVANCED_FACE ( 'NONE', ( #64738 ), #11232, .T. ) ;
#77669 = CARTESIAN_POINT ( 'NONE',  ( -0.2427821522309703550, -0.08942795157528024563, -0.3641732283464568787 ) ) ;
#77670 = CARTESIAN_POINT ( 'NONE',  ( -1.430446194225720724, -0.004921259842519870586, -0.3153832671262229437 ) ) ;
#77671 = CARTESIAN_POINT ( 'NONE',  ( -0.1265901696524993347, 0.4724409448818896462, -0.7939632545931758489 ) ) ;
#77672 = CARTESIAN_POINT ( 'NONE',  ( 0.3280839895013130669, 0.05413385826771666132, 0.4176697321401328100 ) ) ;
#77673 = CARTESIAN_POINT ( 'NONE',  ( -0.3740157480314953431, 0.07958543189024085140, 0.2665933059059887866 ) ) ;
#77674 = CARTESIAN_POINT ( 'NONE',  ( 0.07874015748031558404, -0.1870078740157480601, -0.3641732283464567677 ) ) ;
#77675 = CARTESIAN_POINT ( 'NONE',  ( -0.02624671916010428221, -0.6046776061558807314, 0.2411417322834647770 ) ) ;
#77676 = CARTESIAN_POINT ( 'NONE',  ( -1.017060367454067249, -0.08942795157527998196, 0.3641732283464567121 ) ) ;
#77677 = CARTESIAN_POINT ( 'NONE',  ( 0.3917322834645670104, 0.1049643490035304660, -0.1214103918973247487 ) ) ;
#77678 = CARTESIAN_POINT ( 'NONE',  ( 0.8923884514435701520, -0.6046776061558809534, -0.2411417322834644161 ) ) ;
#77679 = CARTESIAN_POINT ( 'NONE',  ( -1.561679790026246017, -0.4281496062992127816, -0.4176697321401328100 ) ) ;
#77680 = CARTESIAN_POINT ( 'NONE',  ( -0.4724409448818895907, -0.1265901696524993070, -1.225065616797899937 ) ) ;
#77681 = CARTESIAN_POINT ( 'NONE',  ( -0.4265091863517051496, 0.2952755905511810774, -0.1292274648535930714 ) ) ;
#77682 = CARTESIAN_POINT ( 'NONE',  ( 0.2690288713910767848, -0.5511811023622048555, -0.09757992244046775898 ) ) ;
#77683 = CARTESIAN_POINT ( 'NONE',  ( -0.7349081364829387342, -0.6046776061558807314, 0.2411417322834647770 ) ) ;
#77684 = CARTESIAN_POINT ( 'NONE',  ( 0.7808398950131241190, -0.08942795157528024563, -0.3641732283464568787 ) ) ;
#77685 = CARTESIAN_POINT ( 'NONE',  ( -0.1181102362204717315, 0.1771653543307087630, 0.000000000000000000 ) ) ;
#77686 = CARTESIAN_POINT ( 'NONE',  ( -0.7217847769028863381, 0.05413385826771626580, -0.4176697321401330321 ) ) ;
#77687 = CARTESIAN_POINT ( 'NONE',  ( -1.482939632545930975, 0.05413385826771666132, 0.4176697321401328100 ) ) ;
#77688 = LINE ( 'NONE', #56644, #36684 ) ;
#77689 = CARTESIAN_POINT ( 'NONE',  ( 1.286089238845145033, -0.5023911411419708095, -0.1820866141732282451 ) ) ;
#77690 = CARTESIAN_POINT ( 'NONE',  ( 0.5905511811023629321, 0.2952755905511811885, 0.000000000000000000 ) ) ;
#77691 = CARTESIAN_POINT ( 'NONE',  ( -1.423884514435694859, -0.05778040916215560624, -0.4822834645669293319 ) ) ;
#77692 = CARTESIAN_POINT ( 'NONE',  ( -1.463254593175852492, -0.6692913385826773087, -0.1292274648535924053 ) ) ;
#77693 = EDGE_LOOP ( 'NONE', ( #82868, #55773, #61769, #19207 ) ) ;
#77694 = CARTESIAN_POINT ( 'NONE',  ( 0.3460692066303958092, 0.1998031496062993018, -2.412729658792650778 ) ) ;
#77695 = CARTESIAN_POINT ( 'NONE',  ( -0.9711286089238838626, 0.1283753931104746893, -0.1820866141732285504 ) ) ;
#77696 = CARTESIAN_POINT ( 'NONE',  ( 0.5905511811023629321, -0.6692913385826771977, 8.415575281601705876E-17 ) ) ;
#77697 = CARTESIAN_POINT ( 'NONE',  ( -1.089238845144356427, -0.004921259842519576551, 0.3153832671262227771 ) ) ;
#77698 = CARTESIAN_POINT ( 'NONE',  ( 0.3996062992125985480, 2.446882876249141654E-17, -1.612204724409448842 ) ) ;
#77699 = CARTESIAN_POINT ( 'NONE',  ( -1.036745406824146176, 0.05413385826771626580, -0.4176697321401330321 ) ) ;
#77700 = CARTESIAN_POINT ( 'NONE',  ( 1.069553805774278832, 0.2952755905511810774, -0.1292274648535930714 ) ) ;
#77701 = CARTESIAN_POINT ( 'NONE',  ( 0.3608923884514443348, -0.6692913385826771977, 0.1292274648535927661 ) ) ;
#77702 = CARTESIAN_POINT ( 'NONE',  ( 1.496062992125984703, -0.1870078740157480879, -0.4822834645669291653 ) ) ;
#77703 = CARTESIAN_POINT ( 'NONE',  ( -1.673228346456691717, 0.07958543189024071263, -0.2665933059059888421 ) ) ;
#77704 = CARTESIAN_POINT ( 'NONE',  ( 0.3996062992125984925, 0.1070741851644054499, -0.9888451443569553634 ) ) ;
#77705 = CARTESIAN_POINT ( 'NONE',  ( 0.2925321140481932369, -0.2925321140481932369, -1.200787401574803015 ) ) ;
#77706 = CARTESIAN_POINT ( 'NONE',  ( 0.1974969037888706369, -0.3420746716998659953, -0.5643044619422573627 ) ) ;
#77707 = CARTESIAN_POINT ( 'NONE',  ( 0.4697171261335883474, 1.606100245667710702, 2.565525098582279728 ) ) ;
#77708 = CARTESIAN_POINT ( 'NONE',  ( 0.9120734908136490793, 0.1771653543307087075, -0.09757992244046823083 ) ) ;
#77709 = CARTESIAN_POINT ( 'NONE',  ( 0.4986876640419954376, 0.1283753931104748280, 0.1820866141732283561 ) ) ;
#77710 = CARTESIAN_POINT ( 'NONE',  ( -0.07217847769028813698, -0.3162353388693409650, -0.4822834645669289433 ) ) ;
#77711 = CARTESIAN_POINT ( 'NONE',  ( 1.154855643044620184, 0.2306618581243847221, -0.2411417322834647770 ) ) ;
#77712 = CARTESIAN_POINT ( 'NONE',  ( -0.1058382717557497660, -0.3949938075777411073, -1.881233595800524849 ) ) ;
#77713 = CARTESIAN_POINT ( 'NONE',  ( 0.5183727034120741983, -0.5511811023622046335, 0.09757992244046803654 ) ) ;
#77714 = CARTESIAN_POINT ( 'NONE',  ( -0.7020997375328074108, -0.05778040916215522460, 0.4822834645669289988 ) ) ;
#77715 = CARTESIAN_POINT ( 'NONE',  ( -1.345144356955379816, -0.3162353388693405765, 0.4822834645669290543 ) ) ;
#77716 = CARTESIAN_POINT ( 'NONE',  ( 0.8202099737532814183, -0.6692913385826773087, -0.1292274648535924053 ) ) ;
#77717 = CARTESIAN_POINT ( 'NONE',  ( -0.3458507752293909498, 0.3458507752293907833, -1.751968503937007648 ) ) ;
#77718 = AXIS2_PLACEMENT_3D ( 'NONE', #72951, #78865, #59897 ) ;
#77719 = CARTESIAN_POINT ( 'NONE',  ( 1.348312163386739426, 1.062992125984252079, 0.8371118098809627872 ) ) ;
#77720 = ORIENTED_EDGE ( 'NONE', *, *, #64730, .F. ) ;
#77721 = VERTEX_POINT ( 'NONE', #27263 ) ;
#77722 = CARTESIAN_POINT ( 'NONE',  ( -1.397637795275589623, 0.1660481256975885056, 0.3530559997133364547 ) ) ;
#77723 = CARTESIAN_POINT ( 'NONE',  ( -0.6824146981627288167, 0.2306618581243848609, 0.2411417322834645549 ) ) ;
#77725 = CARTESIAN_POINT ( 'NONE',  ( -0.7349081364829387342, -0.6046776061558807314, 0.2411417322834647770 ) ) ;
#77724 = CARTESIAN_POINT ( 'NONE',  ( -0.8202099737532799750, 0.1771653543307087075, -0.09757992244046823083 ) ) ;
#77726 = CARTESIAN_POINT ( 'NONE',  ( -9.594673741351310580E-17, 0.3917322834645669549, -2.127277272144670217 ) ) ;
#77727 = CARTESIAN_POINT ( 'NONE',  ( 0.1751536117528151582, -0.2379288306351265148, 0.1496817530000226215 ) ) ;
#77728 = CARTESIAN_POINT ( 'NONE',  ( 1.548556430446194954, 0.2306618581243847221, -0.2411417322834647770 ) ) ;
#77729 = CARTESIAN_POINT ( 'NONE',  ( -1.312335958005248715, -0.6046776061558809534, -0.2411417322834644161 ) ) ;
#77730 = CARTESIAN_POINT ( 'NONE',  ( 0.3215223097112867578, -0.05778040916215522460, 0.4822834645669289988 ) ) ;
#77731 = CARTESIAN_POINT ( 'NONE',  ( -0.8923884514435688198, -0.6046776061558807314, 0.2411417322834647770 ) ) ;
#77732 = CARTESIAN_POINT ( 'NONE',  ( 0.8005249343832027131, 0.05413385826771666132, 0.4176697321401328100 ) ) ;
#77733 = CARTESIAN_POINT ( 'NONE',  ( 0.2867679344610365999, -0.2867679344610365444, -1.507874015748031260 ) ) ;
#77734 = CARTESIAN_POINT ( 'NONE',  ( -0.7349081364829387342, -0.5023911411419708095, 0.1820866141732285504 ) ) ;
#77735 = ORIENTED_EDGE ( 'NONE', *, *, #63775, .T. ) ;
#77736 = CARTESIAN_POINT ( 'NONE',  ( -0.3420746716998659953, -0.1974969037888706647, -1.942257217847769279 ) ) ;
#77737 = ORIENTED_EDGE ( 'NONE', *, *, #49126, .T. ) ;
#77738 = CARTESIAN_POINT ( 'NONE',  ( -1.646981627296586703, -0.2845877964562161244, -0.3641732283464567121 ) ) ;
#77739 = CARTESIAN_POINT ( 'NONE',  ( -1.305774278215222184, -0.6692913385826773087, -0.1292274648535924053 ) ) ;
#77740 = CARTESIAN_POINT ( 'NONE',  ( -1.332020997375327642, -0.05778040916215522460, 0.4822834645669289988 ) ) ;
#77741 = CARTESIAN_POINT ( 'NONE',  ( 0.2925321140481932369, -0.2925321140481932369, -0.7283464566929134243 ) ) ;
#77742 = CARTESIAN_POINT ( 'NONE',  ( -1.043307086614172707, 0.1660481256975883668, -0.3530559997133364547 ) ) ;
#77743 = CARTESIAN_POINT ( 'NONE',  ( -1.404199475065615932, 0.05413385826771666132, 0.4176697321401328100 ) ) ;
#77744 = CARTESIAN_POINT ( 'NONE',  ( -1.377952755905511140, -0.6692913385826771977, 8.415575281601705876E-17 ) ) ;
#77745 = CARTESIAN_POINT ( 'NONE',  ( -0.3826031302655962807, -4.992347309556208597E-15, 0.3954985857520076920 ) ) ;
#77746 = CARTESIAN_POINT ( 'NONE',  ( -0.8561328129276786214, -2.191421614605370878E-15, 0.4445507791589071167 ) ) ;
#77747 = CARTESIAN_POINT ( 'NONE',  ( 0.2887139107611556010, 0.1283753931104746893, -0.1820866141732285504 ) ) ;
#77748 = CARTESIAN_POINT ( 'NONE',  ( 5.333846858410640380E-15, 1.062992125984252079, -1.444810848096780953 ) ) ;
#77749 = CARTESIAN_POINT ( 'NONE',  ( 0.3392501089628018884, -0.1958661417322834220, -0.1896325459317586282 ) ) ;
#77750 = CARTESIAN_POINT ( 'NONE',  ( -0.2821522309711278487, 0.1771653543307087630, 0.09757992244046791164 ) ) ;
#77751 = CARTESIAN_POINT ( 'NONE',  ( -0.7611548556430438595, -0.6046776061558809534, -0.2411417322834644161 ) ) ;
#77752 = CARTESIAN_POINT ( 'NONE',  ( 1.187664041994751285, -0.3162353388693409650, -0.4822834645669289433 ) ) ;
#77753 = CARTESIAN_POINT ( 'NONE',  ( -0.3937007874015740483, -0.1870078740157479769, 0.4822834645669291653 ) ) ;
#77754 = ORIENTED_EDGE ( 'NONE', *, *, #68913, .T. ) ;
#77755 = VERTEX_POINT ( 'NONE', #64318 ) ;
#77756 = CARTESIAN_POINT ( 'NONE',  ( -0.2925321140481932369, 0.2925321140481931259, -1.986220472440944906 ) ) ;
#77757 = CARTESIAN_POINT ( 'NONE',  ( -1.017060367454067249, -0.05778040916215522460, 0.4822834645669289988 ) ) ;
#77758 = CARTESIAN_POINT ( 'NONE',  ( 1.272965879265092637, 0.05413385826771666132, 0.4176697321401328100 ) ) ;
#77759 = PLANE ( 'NONE',  #37961 ) ;
#77760 = LENGTH_MEASURE_WITH_UNIT ( LENGTH_MEASURE( 0.02539999999999999897 ), #58806 );
#77761 = CARTESIAN_POINT ( 'NONE',  ( 0.4724409448818896462, 0.1265901696524990294, -0.7545931758530182165 ) ) ;
#77762 = CARTESIAN_POINT ( 'NONE',  ( -2.167714792466712392, 1.572145545125847921, 0.4734416007054412789 ) ) ;
#77763 = CARTESIAN_POINT ( 'NONE',  ( 0.3917322834645670104, -0.1049643490035303411, -0.4186351706036745557 ) ) ;
#77764 = FACE_OUTER_BOUND ( 'NONE', #79425, .T. ) ;
#77765 = CARTESIAN_POINT ( 'NONE',  ( -0.3280839895013117347, 0.05413385826771626580, -0.4176697321401330321 ) ) ;
#77766 = CARTESIAN_POINT ( 'NONE',  ( -1.594488188976377119, 0.07958543189024071263, -0.2665933059059888421 ) ) ;
#77767 = CARTESIAN_POINT ( 'NONE',  ( -0.6364829396325453192, -0.3162353388693405765, 0.4822834645669290543 ) ) ;
#77768 = CARTESIAN_POINT ( 'NONE',  ( -0.3460692066303960313, 0.1998031496062989965, 0.2119422572178477349 ) ) ;
#77770 = CARTESIAN_POINT ( 'NONE',  ( -0.3503937007874015630, 0.3044824468161027586, -0.01968503937007903132 ) ) ;
#77769 = CARTESIAN_POINT ( 'NONE',  ( -1.430446194225721390, -0.4281496062992124485, 0.4176697321401328655 ) ) ;
#77771 = CARTESIAN_POINT ( 'NONE',  ( -0.8727034120734901146, -0.05778040916215560624, -0.4822834645669293319 ) ) ;
#77772 = CARTESIAN_POINT ( 'NONE',  ( -0.4002624671916004129, -0.05778040916215560624, -0.4822834645669293319 ) ) ;
#77773 = CARTESIAN_POINT ( 'NONE',  ( -0.3949938075777411073, 0.1058382717557497660, -2.786745406824147064 ) ) ;
#77774 = CARTESIAN_POINT ( 'NONE',  ( 0.9383202099737536495, -0.2845877964562159024, 0.3641732283464567677 ) ) ;
#77775 = DIRECTION ( 'NONE',  ( 0.000000000000000000, 1.000000000000000000, 0.000000000000000000 ) ) ;
#77776 = CARTESIAN_POINT ( 'NONE',  ( 0.7152230971128616943, -0.08942795157527998196, 0.3641732283464567121 ) ) ;
#77777 = CARTESIAN_POINT ( 'NONE',  ( 1.246719160104987623, -0.3690944881889763329, 0.3153832671262228327 ) ) ;
#77778 = CARTESIAN_POINT ( 'NONE',  ( 1.318897637795276356, 0.1660481256975883668, -0.3530559997133364547 ) ) ;
#77779 = CARTESIAN_POINT ( 'NONE',  ( 0.09842519685039434474, 0.07958543189024085140, 0.2665933059059887866 ) ) ;
#77780 = CARTESIAN_POINT ( 'NONE',  ( -0.3917322834645670104, -7.196005306013484475E-17, -1.606299212598425452 ) ) ;
#77781 = CARTESIAN_POINT ( 'NONE',  ( -1.010498687664041384, 0.05413385826771666132, 0.4176697321401328100 ) ) ;
#77782 = CARTESIAN_POINT ( 'NONE',  ( 1.089238845144357537, -0.4281496062992124485, 0.4176697321401328655 ) ) ;
#77783 = B_SPLINE_CURVE_WITH_KNOTS ( 'NONE', 3,
 ( #33017, #59519, #46882, #53611, #8604, #58687, #46051, #21227, #34275, #21639, #26284, #59936, #51945, #52362, #39328, #27118, #33446, #1462 ),
 .UNSPECIFIED., .F., .F.,
 ( 4, 2, 2, 2, 2, 2, 2, 2, 4 ),
 ( 5.794108576630504547E-15, 2.503579458505735792E-05, 5.007158916432061067E-05, 0.0001001431783228451036, 0.0002002863566398940896, 0.0004005727132739911127, 0.0008011454265421859722, 0.001602290853078575149, 0.003204581706151352419 ),
 .UNSPECIFIED. ) ;
#77784 = CARTESIAN_POINT ( 'NONE',  ( 0.1265901696524989462, 0.4724409448818897572, 0.08727034120734905587 ) ) ;
#77785 = CARTESIAN_POINT ( 'NONE',  ( -0.6627296587926501115, 0.1771653543307087075, -0.09757992244046823083 ) ) ;
#77786 = CARTESIAN_POINT ( 'NONE',  ( 0.01968503937007930540, 0.1660481256975885056, 0.3530559997133364547 ) ) ;
#77787 = CARTESIAN_POINT ( 'NONE',  ( 0.2034120734908144990, -0.6692913385826771977, 0.1292274648535927661 ) ) ;
#77788 = CARTESIAN_POINT ( 'NONE',  ( -0.1265901696524993347, 0.4724409448818896462, -0.7132545931758530466 ) ) ;
#77789 = CARTESIAN_POINT ( 'NONE',  ( 0.9711286089238851948, 0.1283753931104748280, 0.1820866141732283561 ) ) ;
#77790 = CARTESIAN_POINT ( 'NONE',  ( -0.006561679790025524116, -0.2845877964562159024, 0.3641732283464567677 ) ) ;
#77791 = CARTESIAN_POINT ( 'NONE',  ( -0.4265091863517051496, -0.6692913385826771977, 0.1292274648535927661 ) ) ;
#77792 = CARTESIAN_POINT ( 'NONE',  ( -1.548556430446193399, 0.2306618581243848609, 0.2411417322834645549 ) ) ;
#77793 = CARTESIAN_POINT ( 'NONE',  ( -0.7283464566929126471, -0.4536011799217367080, 0.2665933059059888421 ) ) ;
#77794 = FACE_OUTER_BOUND ( 'NONE', #12507, .T. ) ;
#77795 = EDGE_CURVE ( 'NONE', #40450, #20906, #30019, .T. ) ;
#77796 = CARTESIAN_POINT ( 'NONE',  ( 0.4921259842519691285, -0.5400638737290845981, -0.3530559997133363437 ) ) ;
#77797 = CARTESIAN_POINT ( 'NONE',  ( -1.043307086614172041, -0.5400638737290844871, 0.3530559997133364547 ) ) ;
#77798 = CARTESIAN_POINT ( 'NONE',  ( -0.3996062992125984925, -0.1070741851644056858, -1.067585301837270517 ) ) ;
#77799 = CARTESIAN_POINT ( 'NONE',  ( 0.2867679344610365999, 0.2867679344610365999, -2.742125984251967630 ) ) ;
#77800 = CARTESIAN_POINT ( 'NONE',  ( 0.1443569553805781891, -0.3690944881889763329, 0.3153832671262228327 ) ) ;
#77801 = CARTESIAN_POINT ( 'NONE',  ( -0.6364829396325453192, -0.05778040916215560624, -0.4822834645669293319 ) ) ;
#77802 = CARTESIAN_POINT ( 'NONE',  ( -0.9317585301837263412, -0.4281496062992127816, -0.4176697321401328100 ) ) ;
#77803 = CARTESIAN_POINT ( 'NONE',  ( -1.200787401574802349, -0.4536011799217367080, 0.2665933059059888421 ) ) ;
#77804 = CARTESIAN_POINT ( 'NONE',  ( -3.911208592539883622, 1.384429027863568473, -0.4501334968650620993 ) ) ;
#77805 =( BOUNDED_CURVE ( )  B_SPLINE_CURVE ( 2, ( #19696, #46612, #1192, #13815, #58834, #8329, #27677, #77788, #20121, #79051, #46192, #71888, #27257 ),
 .UNSPECIFIED., .F., .F. ) 
 B_SPLINE_CURVE_WITH_KNOTS ( ( 3, 2, 2, 2, 2, 2, 3 ),
 ( 0.2875000000000000333, 0.2916666666666667407, 0.2958333333333333925, 0.3000000000000000444, 0.3041666666666666408, 0.3083333333333333481, 0.3125000000000000000 ),
 .UNSPECIFIED. ) 
 CURVE ( )  GEOMETRIC_REPRESENTATION_ITEM ( )  RATIONAL_B_SPLINE_CURVE ( ( 0.9999999999999995559, 0.9659258262890687563, 1.000000000000000000, 0.9659258262890683122, 1.000000000000000000, 0.9659258262890683122, 1.000000000000000000, 0.9659258262890683122, 1.000000000000000000, 0.9659258262890683122, 1.000000000000000000, 0.9659258262890683122, 1.000000000000000000 ) ) 
 REPRESENTATION_ITEM ( '' )  );
#77806 = CARTESIAN_POINT ( 'NONE',  ( -1.010498687664041384, -0.004921259842519576551, 0.3153832671262227771 ) ) ;
#77807 = CARTESIAN_POINT ( 'NONE',  ( -0.7746288504648931594, 0.004960608223778823628, 0.3437734562760190182 ) ) ;
#77808 = CARTESIAN_POINT ( 'NONE',  ( 1.371391076115485719, -0.6692913385826773087, -0.1292274648535924053 ) ) ;
#77809 = LINE ( 'NONE', #77383, #17924 ) ;
#77810 = CARTESIAN_POINT ( 'NONE',  ( -0.1049643490035302301, -0.3917322834645671770, -2.431121677986564311 ) ) ;
#77811 = ORIENTED_EDGE ( 'NONE', *, *, #22324, .T. ) ;
#77812 = CARTESIAN_POINT ( 'NONE',  ( 0.006307039255732630779, -0.3948371832379766189, -2.032323646524576638E-15 ) ) ;
#77813 = CARTESIAN_POINT ( 'NONE',  ( 1.568241469816273437, -0.2845877964562159024, 0.3641732283464567677 ) ) ;
#77814 = CARTESIAN_POINT ( 'NONE',  ( -1.364829396325458521, 0.2306618581243847221, -0.2411417322834647770 ) ) ;
#77815 = CARTESIAN_POINT ( 'NONE',  ( 1.213910761154856299, -0.6692913385826773087, -0.1292274648535924053 ) ) ;
#77816 = CARTESIAN_POINT ( 'NONE',  ( 0.2867679344610365999, 0.2867679344610365999, -1.954724409448818978 ) ) ;
#77817 = CARTESIAN_POINT ( 'NONE',  ( 1.627296587926509996, -0.5023911411419708095, 0.1820866141732285504 ) ) ;
#77818 = EDGE_CURVE ( 'NONE', #24318, #29055, #59135, .T. ) ;
#77819 = CARTESIAN_POINT ( 'NONE',  ( 0.3805774278215230400, -0.4281496062992124485, 0.4176697321401328655 ) ) ;
#77820 = CARTESIAN_POINT ( 'NONE',  ( -0.1771653543307080136, 0.1660481256975883668, -0.3530559997133364547 ) ) ;
#77821 = CARTESIAN_POINT ( 'NONE',  ( 0.2507089876491974678, 1.134347693112636835, -3.929038657107195576 ) ) ;
#77822 = DIRECTION ( 'NONE',  ( 0.000000000000000000, -1.000000000000000000, 0.000000000000000000 ) ) ;
#77823 = CARTESIAN_POINT ( 'NONE',  ( 0.6889763779527563470, 0.07958543189024071263, -0.2665933059059888421 ) ) ;
#77824 = CARTESIAN_POINT ( 'NONE',  ( -0.3996062992125987146, 0.1070741851644051862, -1.292650918635170454 ) ) ;
#77825 = EDGE_LOOP ( 'NONE', ( #20890, #65554, #58974, #31775 ) ) ;
#77826 = CARTESIAN_POINT ( 'NONE',  ( -0.1958661417322833942, -0.3392501089628018884, -0.06235527378708850127 ) ) ;
#77827 = ORIENTED_EDGE ( 'NONE', *, *, #33231, .T. ) ;
#77828 = CARTESIAN_POINT ( 'NONE',  ( 0.1115485564304467270, -0.6692913385826773087, -0.1292274648535924053 ) ) ;
#77829 = CARTESIAN_POINT ( 'NONE',  ( 1.135170603674541256, 0.2952755905511811885, 0.1292274648535926551 ) ) ;
#77830 = CARTESIAN_POINT ( 'NONE',  ( 0.7283464566929143125, 0.1660481256975885056, 0.3530559997133364547 ) ) ;
#77831 = CARTESIAN_POINT ( 'NONE',  ( 1.312335958005250269, -0.6046776061558807314, 0.2411417322834647770 ) ) ;
#77832 = CARTESIAN_POINT ( 'NONE',  ( -0.3346456692913377662, 0.1660481256975883668, -0.3530559997133364547 ) ) ;
#77833 = CARTESIAN_POINT ( 'NONE',  ( 0.09842519685039434474, -0.5400638737290845981, -0.3530559997133363437 ) ) ;
#77834 = CARTESIAN_POINT ( 'NONE',  ( -1.502624671916009680, -0.3162353388693405765, 0.4822834645669290543 ) ) ;
#77836 = EDGE_CURVE ( 'NONE', #36023, #17178, #16650, .T. ) ;
#77835 = CARTESIAN_POINT ( 'NONE',  ( 1.246719160104987623, -0.4281496062992124485, 0.4176697321401328655 ) ) ;
#77837 = CARTESIAN_POINT ( 'NONE',  ( 1.299212598425197429, -0.6692913385826771977, 8.415575281601705876E-17 ) ) ;
#77838 = CARTESIAN_POINT ( 'NONE',  ( 0.3917322834645670104, 2.398668435337828261E-17, -0.1102362204724409017 ) ) ;
#77839 = CARTESIAN_POINT ( 'NONE',  ( 0.2690288713910767848, 0.1771653543307087630, 0.09757992244046791164 ) ) ;
#77840 = ORIENTED_EDGE ( 'NONE', *, *, #44940, .F. ) ;
#77841 = CARTESIAN_POINT ( 'NONE',  ( -0.1974969037888703871, -0.3420746716998661063, -0.6955380577427822120 ) ) ;
#77842 = ORIENTED_EDGE ( 'NONE', *, *, #80522, .F. ) ;
#77843 = CARTESIAN_POINT ( 'NONE',  ( -0.2559055118110230564, 0.07958543189024071263, -0.2665933059059888421 ) ) ;
#77844 = CARTESIAN_POINT ( 'NONE',  ( -0.01312335958005186876, 0.05413385826771626580, -0.4176697321401330321 ) ) ;
#77845 = PLANE ( 'NONE',  #54249 ) ;
#77846 = CARTESIAN_POINT ( 'NONE',  ( -0.02624671916010428221, -0.6046776061558807314, 0.2411417322834647770 ) ) ;
#77847 = CARTESIAN_POINT ( 'NONE',  ( 0.05249343832021075018, 0.2306618581243847221, -0.2411417322834647770 ) ) ;
#77848 = CARTESIAN_POINT ( 'NONE',  ( -1.062992125984250968, 0.2952755905511811885, 0.000000000000000000 ) ) ;
#77849 = CARTESIAN_POINT ( 'NONE',  ( 1.207349081364829990, 0.1283753931104748280, 0.1820866141732283561 ) ) ;
#77850 = DIRECTION ( 'NONE',  ( -0.000000000000000000, -1.000000000000000000, -0.000000000000000000 ) ) ;
#77851 = LINE ( 'NONE', #51306, #8834 ) ;
#77852 = CARTESIAN_POINT ( 'NONE',  ( 1.049868766404200127, -0.5023911411419708095, -0.1820866141732282451 ) ) ;
#77853 = CARTESIAN_POINT ( 'NONE',  ( 0.2690288713910767848, 0.2952755905511811885, 0.1292274648535926551 ) ) ;
#77854 = CARTESIAN_POINT ( 'NONE',  ( 0.7152230971128616943, -0.05778040916215522460, 0.4822834645669289988 ) ) ;
#77855 = CARTESIAN_POINT ( 'NONE',  ( 0.2925321140481932369, -0.2925321140481932369, -1.200787401574803015 ) ) ;
#77856 = CARTESIAN_POINT ( 'NONE',  ( -1.686351706036744558, 0.2952755905511810774, -0.1292274648535930714 ) ) ;
#77857 = CARTESIAN_POINT ( 'NONE',  ( 0.1070741851644053388, 0.3996062992125986035, -0.8576115485564304031 ) ) ;
#77858 = CARTESIAN_POINT ( 'NONE',  ( 0.3996062992125985480, 2.446882876249141654E-17, -0.03740157480314963701 ) ) ;
#77859 = CARTESIAN_POINT ( 'NONE',  ( -0.03280839895013062252, -0.6692913385826771977, 0.1292274648535927661 ) ) ;
#77860 = CARTESIAN_POINT ( 'NONE',  ( 0.2925321140481932369, 0.2925321140481932369, -2.500000000000000444 ) ) ;
#77861 = CARTESIAN_POINT ( 'NONE',  ( -9.594673741351313045E-17, 0.3917322834645670104, -1.974409448818897683 ) ) ;
#77862 = CARTESIAN_POINT ( 'NONE',  ( -1.056430446194224881, -0.5511811023622046335, 0.09757992244046803654 ) ) ;
#77863 = CARTESIAN_POINT ( 'NONE',  ( 1.122047244094488860, 0.1660481256975885056, 0.3530559997133364547 ) ) ;
#77864 = CARTESIAN_POINT ( 'NONE',  ( 1.404199475065617708, 0.05413385826771626580, -0.4176697321401330321 ) ) ;
#77865 = CARTESIAN_POINT ( 'NONE',  ( -0.09186351706036663400, -0.3690944881889763329, 0.3153832671262228327 ) ) ;
#77866 = CARTESIAN_POINT ( 'NONE',  ( 0.6102362204724416372, -0.5400638737290844871, 0.3530559997133364547 ) ) ;
#77867 = CARTESIAN_POINT ( 'NONE',  ( -0.1265901696524993347, 0.4724409448818895907, -1.658136482939632117 ) ) ;
#77868 = CARTESIAN_POINT ( 'NONE',  ( 0.2427821522309719648, -0.08942795157527998196, 0.3641732283464567121 ) ) ;
#77869 = CARTESIAN_POINT ( 'NONE',  ( -0.1771653543307080136, -0.5400638737290844871, 0.3530559997133364547 ) ) ;
#77870 = CARTESIAN_POINT ( 'NONE',  ( 0.3949938075777409963, 2.418639510665530743E-17, -1.297244094488188892 ) ) ;
#77871 = CARTESIAN_POINT ( 'NONE',  ( -1.069553805774277722, 0.2952755905511811885, 0.1292274648535926551 ) ) ;
#77872 = CARTESIAN_POINT ( 'NONE',  ( 0.6102362204724416372, -0.4536011799217367080, 0.2665933059059888421 ) ) ;
#77873 = CARTESIAN_POINT ( 'NONE',  ( -0.4724409448818898682, -8.678599364036362592E-17, -0.8267716535433070613 ) ) ;
#77874 = CARTESIAN_POINT ( 'NONE',  ( -0.8530183727034112984, -0.4281496062992127816, -0.4176697321401328100 ) ) ;
#77875 = CARTESIAN_POINT ( 'NONE',  ( -0.4790026246719152336, -0.08942795157528024563, -0.3641732283464568787 ) ) ;
#77876 = CARTESIAN_POINT ( 'NONE',  ( -1.586052503253849055, 0.4724409448818907564, -0.1653254495020551051 ) ) ;
#77877 = CARTESIAN_POINT ( 'NONE',  ( -0.6036745406824141069, 0.2306618581243848609, 0.2411417322834645549 ) ) ;
#77878 = CARTESIAN_POINT ( 'NONE',  ( -0.3674540682414689785, 0.2306618581243848609, 0.2411417322834645549 ) ) ;
#77879 = CARTESIAN_POINT ( 'NONE',  ( 0.4527559055118117182, -0.4536011799217367080, 0.2665933059059888421 ) ) ;
#77880 = CARTESIAN_POINT ( 'NONE',  ( 0.3996062992125986035, -0.1070741851644052972, -2.235564304461942431 ) ) ;
#77881 = CARTESIAN_POINT ( 'NONE',  ( -0.1049868766404193215, -0.6046776061558807314, 0.2411417322834647770 ) ) ;
#77882 = CARTESIAN_POINT ( 'NONE',  ( 0.1958661417322834497, 0.3392501089628018329, -2.114153912564617599 ) ) ;
#77883 = CARTESIAN_POINT ( 'NONE',  ( -1.515748031496062076, 0.07958543189024071263, -0.2665933059059888421 ) ) ;
#77884 = CARTESIAN_POINT ( 'NONE',  ( 0.5971128608923891301, 0.1771653543307087075, -0.09757992244046823083 ) ) ;
#77885 = CARTESIAN_POINT ( 'NONE',  ( 1.469816272965879911, 0.2306618581243847221, -0.2411417322834647770 ) ) ;
#77886 = VECTOR ( 'NONE', #21128, 39.37007874015748143 ) ;
#77887 = CARTESIAN_POINT ( 'NONE',  ( -0.8464566929133852113, -0.4536011799217368745, -0.2665933059059886201 ) ) ;
#77888 = CARTESIAN_POINT ( 'NONE',  ( -1.049868766404198794, 0.1283753931104746893, -0.1820866141732285504 ) ) ;
#77889 = CARTESIAN_POINT ( 'NONE',  ( -0.7349081364829387342, -0.6046776061558807314, 0.2411417322834647770 ) ) ;
#77890 = CARTESIAN_POINT ( 'NONE',  ( -0.2099737532808391705, -0.6046776061558809534, -0.2411417322834644161 ) ) ;
#77891 = CARTESIAN_POINT ( 'NONE',  ( 0.7020997375328090762, -0.2845877964562159024, 0.3641732283464567677 ) ) ;
#77892 = CARTESIAN_POINT ( 'NONE',  ( -0.2431027332089026605, 0.1676825148875300264, 5.760293869191740690 ) ) ;
#77893 = CARTESIAN_POINT ( 'NONE',  ( 1.167979002624672580, -0.004921259842519870586, -0.3153832671262229437 ) ) ;
#77894 = EDGE_CURVE ( 'NONE', #16662, #12926, #28512, .T. ) ;
#77895 = CARTESIAN_POINT ( 'NONE',  ( 0.3740157480314966754, -0.5400638737290844871, 0.3530559997133364547 ) ) ;
#77896 = CARTESIAN_POINT ( 'NONE',  ( 0.1998031496062992463, 0.3460692066303959202, 0.09383202099737532331 ) ) ;
#77897 = CARTESIAN_POINT ( 'NONE',  ( -0.8858267716535425107, 0.1660481256975883668, -0.3530559997133364547 ) ) ;
#77898 = CARTESIAN_POINT ( 'NONE',  ( 0.3917322834645669549, 0.1049643490035304660, -1.469160104986876769 ) ) ;
#77899 = CARTESIAN_POINT ( 'NONE',  ( 1.299212598425197429, 0.1771653543307087630, 0.000000000000000000 ) ) ;
#77900 = CARTESIAN_POINT ( 'NONE',  ( 0.4396325459317593221, 0.2952755905511810774, -0.1292274648535930714 ) ) ;
#77901 = CARTESIAN_POINT ( 'NONE',  ( 0.04593175853018440641, -0.6692913385826771977, 0.1292274648535927661 ) ) ;
#77902 = CARTESIAN_POINT ( 'NONE',  ( 1.595398199321655275, 1.013096522517430209, 0.1559797534342494407 ) ) ;
#77903 = CARTESIAN_POINT ( 'NONE',  ( -0.07874015748031421014, -0.1870078740157479769, 0.3641732283464567677 ) ) ;
#77904 = CARTESIAN_POINT ( 'NONE',  ( 0.9842519685039378130, -0.6692913385826771977, 8.415575281601705876E-17 ) ) ;
#77905 = CARTESIAN_POINT ( 'NONE',  ( -0.2362204724409442680, -0.1870078740157480601, -0.3641732283464567677 ) ) ;
#77906 = CARTESIAN_POINT ( 'NONE',  ( -0.8333333333333323711, 0.2952755905511811885, 0.1292274648535926551 ) ) ;
#77907 = CARTESIAN_POINT ( 'NONE',  ( 0.7974104941589355011, -4.927456884911482678E-16, 0.4445507791589062840 ) ) ;
#77908 = CARTESIAN_POINT ( 'NONE',  ( -0.05905511811023545637, -0.5400638737290845981, -0.3530559997133363437 ) ) ;
#77909 = ORIENTED_EDGE ( 'NONE', *, *, #41314, .F. ) ;
#77910 = CARTESIAN_POINT ( 'NONE',  ( -1.154855643044618851, 0.2306618581243848609, 0.2411417322834645549 ) ) ;
#77911 = CARTESIAN_POINT ( 'NONE',  ( -0.5314960629921254842, -0.4536011799217368745, -0.2665933059059886201 ) ) ;
#77912 = CARTESIAN_POINT ( 'NONE',  ( 0.1246719160104994284, -0.6692913385826771977, 0.1292274648535927661 ) ) ;
#77913 = CARTESIAN_POINT ( 'NONE',  ( -1.141732283464566011, -0.6692913385826771977, 8.415575281601705876E-17 ) ) ;
#77914 = CARTESIAN_POINT ( 'NONE',  ( -0.5774278215223089816, -0.6046776061558807314, 0.2411417322834647770 ) ) ;
#77915 = CARTESIAN_POINT ( 'NONE',  ( -0.7426113562971994320, 2.199547029021313715, 0.5309055118110236338 ) ) ;
#77917 = CARTESIAN_POINT ( 'NONE',  ( 0.7742782152230978099, -0.4281496062992124485, 0.4176697321401328655 ) ) ;
#77916 = DIRECTION ( 'NONE',  ( -3.491481338843132961E-15, -0.000000000000000000, 1.000000000000000000 ) ) ;
#77918 = CARTESIAN_POINT ( 'NONE',  ( 1.358267716535433323, 0.1660481256975885056, 0.3530559997133364547 ) ) ;
#77919 = CARTESIAN_POINT ( 'NONE',  ( -0.1958661417322834220, -0.3392501089628018884, -2.262467191601049699 ) ) ;
#77920 = CARTESIAN_POINT ( 'NONE',  ( -1.574803149606298192, -0.1870078740157480879, -0.4822834645669291653 ) ) ;
#77921 = CARTESIAN_POINT ( 'NONE',  ( -1.437007874015747477, -0.5400638737290844871, 0.3530559997133364547 ) ) ;
#77922 = CARTESIAN_POINT ( 'NONE',  ( 0.2362204724409451007, -0.4091458600556402980, -0.5643044619422572516 ) ) ;
#77923 = CARTESIAN_POINT ( 'NONE',  ( 0.1998031496062994405, -0.3460692066303958092, 0.06561679790026245240 ) ) ;
#77924 = ORIENTED_EDGE ( 'NONE', *, *, #51138, .F. ) ;
#77925 = CARTESIAN_POINT ( 'NONE',  ( 0.05249343832021075018, -0.5023911411419708095, 0.1820866141732285504 ) ) ;
#77926 = CARTESIAN_POINT ( 'NONE',  ( -0.3917322834645671215, 0.1049643490035301469, -1.599737532808399143 ) ) ;
#77927 = ORIENTED_EDGE ( 'NONE', *, *, #44328, .T. ) ;
#77928 = CARTESIAN_POINT ( 'NONE',  ( 0.2099737532808405305, 0.2306618581243847221, -0.2411417322834647770 ) ) ;
#77929 = CARTESIAN_POINT ( 'NONE',  ( -0.05249343832020938322, -0.6046776061558809534, -0.2411417322834644161 ) ) ;
#77930 = CARTESIAN_POINT ( 'NONE',  ( -1.157146581871515012E-16, 0.4724409448818898682, -2.677165354330708347 ) ) ;
#77931 = DIRECTION ( 'NONE',  ( -0.000000000000000000, -1.000000000000000000, -0.000000000000000000 ) ) ;
#77932 = CARTESIAN_POINT ( 'NONE',  ( -0.8202099737532799750, 0.1771653543307087075, -0.09757992244046823083 ) ) ;
#77933 = DIRECTION ( 'NONE',  ( 0.000000000000000000, 0.4999999999999998335, 0.8660254037844385966 ) ) ;
#77934 = CARTESIAN_POINT ( 'NONE',  ( 0.9317585301837276734, 0.05413385826771626580, -0.4176697321401330321 ) ) ;
#77935 = CARTESIAN_POINT ( 'NONE',  ( 1.102362204724410155, -0.1870078740157479769, 0.3641732283464567677 ) ) ;
#77936 = CARTESIAN_POINT ( 'NONE',  ( -0.4199475065616791736, -0.6046776061558807314, 0.2411417322834647770 ) ) ;
#77937 = CARTESIAN_POINT ( 'NONE',  ( 0.3917322834645668994, 0.1049643490035304522, -0.9921066684701294047 ) ) ;
#77938 = CARTESIAN_POINT ( 'NONE',  ( -0.6627296587926501115, 0.2952755905511810774, -0.1292274648535930714 ) ) ;
#77939 = CARTESIAN_POINT ( 'NONE',  ( -1.601049868766403650, -0.5023911411419708095, 0.1820866141732285504 ) ) ;
#77940 =( BOUNDED_CURVE ( )  B_SPLINE_CURVE ( 2, ( #49689, #18136, #17326, #82115, #18545, #24835, #58388, #11408, #11827, #10987, #13375, #39028, #64712 ),
 .UNSPECIFIED., .F., .F. ) 
 B_SPLINE_CURVE_WITH_KNOTS ( ( 3, 2, 2, 2, 2, 2, 3 ),
 ( 0.5369674582711644328, 0.5378787878787878451, 0.5416666666666666297, 0.5454545454545454142, 0.5492424242424241987, 0.5530303030303029832, 0.5539416326379265065 ),
 .UNSPECIFIED. ) 
 CURVE ( )  GEOMETRIC_REPRESENTATION_ITEM ( )  RATIONAL_B_SPLINE_CURVE ( ( 0.9875488213027523443, 0.9918020599134680371, 1.000000000000000000, 0.9659258262890683122, 1.000000000000000000, 0.9659258262890683122, 1.000000000000000000, 0.9659258262890683122, 1.000000000000000000, 0.9659258262890683122, 1.000000000000000000, 0.9918020599134671489, 0.9875488213027514561 ) ) 
 REPRESENTATION_ITEM ( '' )  );
#77941 = CARTESIAN_POINT ( 'NONE',  ( 1.161417322834646493, -0.5400638737290844871, 0.3530559997133364547 ) ) ;
#77942 = CARTESIAN_POINT ( 'NONE',  ( 1.574803149606299746, -0.1870078740157480601, -0.3641732283464567677 ) ) ;
#77943 = ORIENTED_EDGE ( 'NONE', *, *, #9565, .F. ) ;
#77944 = CARTESIAN_POINT ( 'NONE',  ( -0.3392501089628019995, 0.1958661417322831999, -2.385189919456379926 ) ) ;
#77945 = CARTESIAN_POINT ( 'NONE',  ( 0.07217847769028949700, -0.3162353388693405765, 0.4822834645669290543 ) ) ;
#77946 = ORIENTED_EDGE ( 'NONE', *, *, #79009, .F. ) ;
#77947 = CARTESIAN_POINT ( 'NONE',  ( -0.7874015748031489847, -0.1870078740157479769, 0.4822834645669291653 ) ) ;
#77948 = CARTESIAN_POINT ( 'NONE',  ( 1.207349081364829990, -0.6046776061558809534, -0.2411417322834644161 ) ) ;
#77949 = CARTESIAN_POINT ( 'NONE',  ( 1.161417322834646271, 0.1660481256975883668, -0.3530559997133364547 ) ) ;
#77950 = ADVANCED_FACE ( 'NONE', ( #2848 ), #8335, .F. ) ;
#77951 = CARTESIAN_POINT ( 'NONE',  ( 0.2493438320209980519, -0.4281496062992127816, -0.4176697321401328100 ) ) ;
#77952 = CARTESIAN_POINT ( 'NONE',  ( -0.3018372703412066094, -0.4281496062992127816, -0.4176697321401328100 ) ) ;
#77953 = CARTESIAN_POINT ( 'NONE',  ( -0.3917322834645671215, 0.1049643490035301469, -1.692257217847769057 ) ) ;
#77954 = CARTESIAN_POINT ( 'NONE',  ( -1.266404199475064773, -0.3162353388693405765, 0.4822834645669290543 ) ) ;
#77955 = CARTESIAN_POINT ( 'NONE',  ( -0.1049868766404193215, -0.6046776061558807314, 0.2411417322834647770 ) ) ;
#77956 = ADVANCED_FACE ( 'NONE', ( #8748 ), #61321, .F. ) ;
#77957 = CARTESIAN_POINT ( 'NONE',  ( -0.2887139107611542133, -0.5023911411419708095, -0.1820866141732282451 ) ) ;
#77958 = DIRECTION ( 'NONE',  ( -0.000000000000000000, -1.000000000000000000, -0.000000000000000000 ) ) ;
#77959 = CARTESIAN_POINT ( 'NONE',  ( 1.417322834645670104, -0.1870078740157480879, -0.4822834645669291653 ) ) ;
#77960 = CARTESIAN_POINT ( 'NONE',  ( -0.4461942257217840213, 0.2306618581243848609, 0.2411417322834645549 ) ) ;
#77961 = CARTESIAN_POINT ( 'NONE',  ( 0.3021879055830045124, 0.004960608223779807216, -0.3437734562760184631 ) ) ;
#77962 = CARTESIAN_POINT ( 'NONE',  ( 1.181102362204724976, -0.1870078740157480879, -0.4822834645669291653 ) ) ;
#77963 = DIRECTION ( 'NONE',  ( 1.000000000000000000, 1.734723475976808080E-16, 3.491481338843132961E-15 ) ) ;
#77964 = ORIENTED_EDGE ( 'NONE', *, *, #6890, .T. ) ;
#77965 = CARTESIAN_POINT ( 'NONE',  ( 0.2821522309711292364, 0.2952755905511810774, -0.1292274648535930714 ) ) ;
#77966 = CARTESIAN_POINT ( 'NONE',  ( -0.1771653543307080136, -0.4536011799217367080, 0.2665933059059888421 ) ) ;
#77968 = CARTESIAN_POINT ( 'NONE',  ( -3.821484228344193657, 2.755905511811024056, 0.5314960629921260393 ) ) ;
#77967 = CARTESIAN_POINT ( 'NONE',  ( 1.286089238845145033, -0.5023911411419708095, -0.1820866141732282451 ) ) ;
#77969 = CARTESIAN_POINT ( 'NONE',  ( 0.4091458600556404646, -0.2362204724409448231, -0.3392388451443569819 ) ) ;
#77970 = CARTESIAN_POINT ( 'NONE',  ( 1.515748031496063408, 0.07958543189024085140, 0.2665933059059887866 ) ) ;
#77971 = CARTESIAN_POINT ( 'NONE',  ( 1.056430446194226436, -0.6692913385826773087, -0.1292274648535924053 ) ) ;
#77972 = CARTESIAN_POINT ( 'NONE',  ( 0.3420746716998660508, -0.1974969037888704149, -0.02427821522309712640 ) ) ;
#77973 = CARTESIAN_POINT ( 'NONE',  ( 0.2165354330708668673, 0.1660481256975883668, -0.3530559997133364547 ) ) ;
#77974 = CARTESIAN_POINT ( 'NONE',  ( -0.3249695492770445782, -2.567464376874931580E-15, -0.4445507791589072832 ) ) ;
#77975 = CARTESIAN_POINT ( 'NONE',  ( 1.587926509186352142, -0.004921259842519576551, 0.3153832671262227771 ) ) ;
#77976 = CARTESIAN_POINT ( 'NONE',  ( -0.2034120734908131112, -0.6692913385826773087, -0.1292274648535924053 ) ) ;
#77977 = CARTESIAN_POINT ( 'NONE',  ( -9.674558042662122972E-17, 0.3949938075777409963, 0.08070866141732281618 ) ) ;
#77978 = CARTESIAN_POINT ( 'NONE',  ( 1.496062992125985147, -0.1870078740157479769, 0.4822834645669291653 ) ) ;
#77979 = CARTESIAN_POINT ( 'NONE',  ( 0.6627296587926515548, 0.2952755905511811885, 0.1292274648535926551 ) ) ;
#77980 = CARTESIAN_POINT ( 'NONE',  ( 0.9973753280839902091, -0.5023911411419708095, 0.1820866141732285504 ) ) ;
#77981 = CARTESIAN_POINT ( 'NONE',  ( -2.787279214012418738, 0.000000000000000000, 0.000000000000000000 ) ) ;
#77982 = CARTESIAN_POINT ( 'NONE',  ( 0.8202099737532814183, -0.5511811023622048555, -0.09757992244046775898 ) ) ;
#77983 = CARTESIAN_POINT ( 'NONE',  ( -1.325459317585300889, 0.05413385826771666132, 0.4176697321401328100 ) ) ;
#77984 = EDGE_CURVE ( 'NONE', #52887, #75845, #41145, .T. ) ;
#77985 = CARTESIAN_POINT ( 'NONE',  ( 0.3996062992125986035, -0.1070741851644052972, -0.8182414698162727706 ) ) ;
#77986 = CARTESIAN_POINT ( 'NONE',  ( 1.227034120734908917, 0.2952755905511810774, -0.1292274648535930714 ) ) ;
#77987 = CARTESIAN_POINT ( 'NONE',  ( -0.3917322834645670104, -7.196005306013484475E-17, -0.8188976377952754682 ) ) ;
#77989 = FACE_OUTER_BOUND ( 'NONE', #20473, .T. ) ;
#77988 = CARTESIAN_POINT ( 'NONE',  ( 0.7480314960629927956, 0.2952755905511811885, 0.000000000000000000 ) ) ;
#77990 = CARTESIAN_POINT ( 'NONE',  ( -0.7137454485294948414, 2.793565526369265584, -0.4917280318828580743 ) ) ;
#77991 = CARTESIAN_POINT ( 'NONE',  ( 0.4855643044619428750, -0.004921259842519576551, 0.3153832671262227771 ) ) ;
#77992 = EDGE_CURVE ( 'NONE', #33187, #12202, #63662, .T. ) ;
#77993 = CARTESIAN_POINT ( 'NONE',  ( 0.7152230971128616943, -0.05778040916215522460, 0.4822834645669289988 ) ) ;
#77994 = CARTESIAN_POINT ( 'NONE',  ( 0.7677165354330716118, 0.1012011053420775880, -0.2882089793578256898 ) ) ;
#77995 = CARTESIAN_POINT ( 'NONE',  ( -0.8530183727034112984, -0.3690944881889765550, -0.3153832671262227771 ) ) ;
#77996 = CARTESIAN_POINT ( 'NONE',  ( -1.135170603674539924, -0.6692913385826771977, 0.1292274648535927661 ) ) ;
#77997 = CARTESIAN_POINT ( 'NONE',  ( -1.535433070866141225, 0.2952755905511811885, 0.000000000000000000 ) ) ;
#77998 = CARTESIAN_POINT ( 'NONE',  ( 0.8267716535433078384, -0.6692913385826771977, 8.415575281601705876E-17 ) ) ;
#77999 = CARTESIAN_POINT ( 'NONE',  ( 1.679790026246720025, 0.2306618581243848609, 0.2411417322834645549 ) ) ;
#78000 = EDGE_CURVE ( 'NONE', #69342, #26718, #35245, .T. ) ;
#78001 = CARTESIAN_POINT ( 'NONE',  ( -0.3970677821444029698, -0.02963302784745281207, -1.220472440944882386 ) ) ;
#78002 = CARTESIAN_POINT ( 'NONE',  ( 0.8530183727034126306, 0.05413385826771626580, -0.4176697321401330321 ) ) ;
#78003 = CARTESIAN_POINT ( 'NONE',  ( 0.1998031496062994128, -0.3460692066303957537, 0.1463254593175852825 ) ) ;
#78004 = CARTESIAN_POINT ( 'NONE',  ( 0.3134538944422693985, 1.179955895207738914, 3.924571280271134111 ) ) ;
#78005 = CARTESIAN_POINT ( 'NONE',  ( 1.463254593175853824, -0.6692913385826771977, 0.1292274648535927661 ) ) ;
#78006 = CARTESIAN_POINT ( 'NONE',  ( -1.338582677165353729, -0.1870078740157480601, -0.3641732283464567677 ) ) ;
#78007 = CARTESIAN_POINT ( 'NONE',  ( 1.036745406824147731, -0.004921259842519576551, 0.3153832671262227771 ) ) ;
#78008 = CARTESIAN_POINT ( 'NONE',  ( -1.122047244094487306, 0.07958543189024071263, -0.2665933059059888421 ) ) ;
#78009 = CARTESIAN_POINT ( 'NONE',  ( -0.6167979002624665030, -0.3690944881889765550, -0.3153832671262227771 ) ) ;
#78010 = CARTESIAN_POINT ( 'NONE',  ( -1.391076115485563758, 0.1283753931104748280, 0.1820866141732283561 ) ) ;
#78011 = CARTESIAN_POINT ( 'NONE',  ( 1.049868766404200127, -0.5023911411419708095, -0.1820866141732282451 ) ) ;
#78012 = CARTESIAN_POINT ( 'NONE',  ( 0.4855643044619430415, -0.4281496062992127816, -0.4176697321401328100 ) ) ;
#78013 = CARTESIAN_POINT ( 'NONE',  ( 1.161417322834646271, 0.1660481256975883668, -0.3530559997133364547 ) ) ;
#78014 = AXIS2_PLACEMENT_3D ( 'NONE', #43559, #18332, #42741 ) ;
#78015 = CARTESIAN_POINT ( 'NONE',  ( 0.1181102362204730916, 0.2952755905511811885, 0.000000000000000000 ) ) ;
#78016 = CARTESIAN_POINT ( 'NONE',  ( 0.6167979002624678353, -0.3690944881889763329, 0.3153832671262228327 ) ) ;
#78017 = CARTESIAN_POINT ( 'NONE',  ( 1.345144356955381593, -0.3162353388693409650, -0.4822834645669289433 ) ) ;
#78018 = FACE_OUTER_BOUND ( 'NONE', #60527, .T. ) ;
#78019 = CARTESIAN_POINT ( 'NONE',  ( -0.4986876640419942164, -0.6046776061558807314, 0.2411417322834647770 ) ) ;
#78020 = CARTESIAN_POINT ( 'NONE',  ( 4.893765752498283924E-17, -0.3996062992125986035, -0.3937007874015748254 ) ) ;
#78021 = CARTESIAN_POINT ( 'NONE',  ( 0.4091458600556403535, 0.2362204724409449896, -1.152887139107611425 ) ) ;
#78022 = CARTESIAN_POINT ( 'NONE',  ( 0.03280839895013198948, 0.2952755905511811885, 0.1292274648535926551 ) ) ;
#78023 = CARTESIAN_POINT ( 'NONE',  ( -0.2034120734908128059, 0.2952755905511811885, 0.1292274648535926551 ) ) ;
#78024 = CARTESIAN_POINT ( 'NONE',  ( -0.2165354330708654795, -0.5400638737290845981, -0.3530559997133363437 ) ) ;
#78025 = CARTESIAN_POINT ( 'NONE',  ( 0.2925321140481932369, -0.2925321140481932369, -2.618110236220472675 ) ) ;
#78026 = CARTESIAN_POINT ( 'NONE',  ( -0.1974969037888703871, -0.3420746716998661063, -2.112860892388451539 ) ) ;
#78027 = CARTESIAN_POINT ( 'NONE',  ( -0.1049643490035307020, 0.3917322834645669549, -0.4711286089238844177 ) ) ;
#78028 = DIRECTION ( 'NONE',  ( 0.000000000000000000, 0.000000000000000000, -1.000000000000000000 ) ) ;
#78029 = CARTESIAN_POINT ( 'NONE',  ( -9.594673741351313045E-17, 0.3917322834645670104, -1.094488188976378007 ) ) ;
#78030 = CARTESIAN_POINT ( 'NONE',  ( -0.9776902887139098386, -0.5511811023622046335, 0.09757992244046803654 ) ) ;
#78031 = CARTESIAN_POINT ( 'NONE',  ( -0.3392501089628019995, 0.1958661417322832277, -1.120734908136482799 ) ) ;
#78032 = CARTESIAN_POINT ( 'NONE',  ( -1.017060367454067249, -0.3162353388693409650, -0.4822834645669289433 ) ) ;
#78033 = CARTESIAN_POINT ( 'NONE',  ( 0.1049643490035304522, -0.3917322834645668994, -0.007854699966192403571 ) ) ;
#78034 = CARTESIAN_POINT ( 'NONE',  ( 0.5971128608923891301, 0.2952755905511810774, -0.1292274648535930714 ) ) ;
#78035 = CARTESIAN_POINT ( 'NONE',  ( -0.5839895013123351797, 0.1771653543307087075, -0.09757992244046823083 ) ) ;
#78036 = CARTESIAN_POINT ( 'NONE',  ( 1.128608923884514947, 0.2306618581243848609, 0.2411417322834645549 ) ) ;
#78037 = CARTESIAN_POINT ( 'NONE',  ( 0.5380577427821529035, 0.05413385826771626580, -0.4176697321401330321 ) ) ;
#78038 = CARTESIAN_POINT ( 'NONE',  ( -0.4602855208775665785, 1.653389129435536509, -2.138261236553457678 ) ) ;
#78039 = CARTESIAN_POINT ( 'NONE',  ( -0.1070741851644056997, 0.3996062992125986035, -2.526246719160104792 ) ) ;
#78040 = CARTESIAN_POINT ( 'NONE',  ( -0.3392501089628017219, -0.1958661417322836995, -1.309074433892075451 ) ) ;
#78041 = CARTESIAN_POINT ( 'NONE',  ( 1.443569553805774897, -0.6046776061558809534, -0.2411417322834644161 ) ) ;
#78042 = CARTESIAN_POINT ( 'NONE',  ( 0.3674540682414705883, 0.2306618581243847221, -0.2411417322834647770 ) ) ;
#78043 = EDGE_CURVE ( 'NONE', #58583, #15221, #56214, .T. ) ;
#78044 = CARTESIAN_POINT ( 'NONE',  ( 0.09842519685039434474, -0.5400638737290845981, -0.3530559997133363437 ) ) ;
#78045 = CARTESIAN_POINT ( 'NONE',  ( 1.371391076115485719, -0.6692913385826773087, -0.1292274648535924053 ) ) ;
#78046 = CARTESIAN_POINT ( 'NONE',  ( 0.8989501312335964611, 0.2952755905511811885, 0.1292274648535926551 ) ) ;
#78047 = CARTESIAN_POINT ( 'NONE',  ( -0.3917322834645670104, -7.196005306013484475E-17, -0.5964566929133858775 ) ) ;
#78048 = CARTESIAN_POINT ( 'NONE',  ( -0.1115485564304456306, 0.2952755905511810774, -0.1292274648535930714 ) ) ;
#78049 = CARTESIAN_POINT ( 'NONE',  ( 1.227034120734908917, 0.2952755905511810774, -0.1292274648535930714 ) ) ;
#78050 = CARTESIAN_POINT ( 'NONE',  ( 0.3083989501312343062, -0.05778040916215560624, -0.4822834645669293319 ) ) ;
#78051 = CARTESIAN_POINT ( 'NONE',  ( 1.082677165354331228, 0.07958543189024071263, -0.2665933059059888421 ) ) ;
#78052 = CARTESIAN_POINT ( 'NONE',  ( -0.8989501312335946848, 0.2952755905511810774, -0.1292274648535930714 ) ) ;
#78053 = CARTESIAN_POINT ( 'NONE',  ( -1.384514435695537005, 0.2952755905511811885, 0.1292274648535926551 ) ) ;
#78054 = CARTESIAN_POINT ( 'NONE',  ( 0.8858267716535438430, -0.5400638737290845981, -0.3530559997133363437 ) ) ;
#78055 = CARTESIAN_POINT ( 'NONE',  ( 0.2798680777852625701, -0.2749078412849261244, -1.929133858267715773 ) ) ;
#78056 = CARTESIAN_POINT ( 'NONE',  ( -0.2867679344610364334, -0.2867679344610367109, -2.098425196850393526 ) ) ;
#78057 = ORIENTED_EDGE ( 'NONE', *, *, #73157, .T. ) ;
#78058 = CARTESIAN_POINT ( 'NONE',  ( -0.3996062992125987146, 0.1070741851644051862, -0.1902887139107611592 ) ) ;
#78059 = ORIENTED_EDGE ( 'NONE', *, *, #35860, .T. ) ;
#78060 = CARTESIAN_POINT ( 'NONE',  ( 1.345144356955381593, -0.05778040916215522460, 0.4822834645669289988 ) ) ;
#78061 = CARTESIAN_POINT ( 'NONE',  ( 0.9383202099737536495, -0.2845877964562159024, 0.3641732283464567677 ) ) ;
#78062 = CARTESIAN_POINT ( 'NONE',  ( -0.3458507752293909498, 0.3458507752293908388, -2.458661417322834719 ) ) ;
#78063 = CARTESIAN_POINT ( 'NONE',  ( -0.2100141437675596967, 1.111707297776193926, 2.829210744671456723 ) ) ;
#78064 = CARTESIAN_POINT ( 'NONE',  ( 3.937007874015748143, 2.165354330708662012, 0.6299212598425202314 ) ) ;
#78065 = CARTESIAN_POINT ( 'NONE',  ( 4.797336870675656522E-17, -0.3917322834645670104, -0.7933070866141732624 ) ) ;
#78066 = CARTESIAN_POINT ( 'NONE',  ( -1.122047244094487306, 0.07958543189024071263, -0.2665933059059888421 ) ) ;
#78067 = CARTESIAN_POINT ( 'NONE',  ( -1.712598425196849572, 0.07958543189024085140, 0.2665933059059887866 ) ) ;
#78068 = DIRECTION ( 'NONE',  ( 0.000000000000000000, 0.000000000000000000, 1.000000000000000000 ) ) ;
#78069 = CARTESIAN_POINT ( 'NONE',  ( -0.2755905511811018171, 0.2952755905511811885, 0.000000000000000000 ) ) ;
#78070 = CARTESIAN_POINT ( 'NONE',  ( 1.194225721784777594, -0.4281496062992127816, -0.4176697321401328100 ) ) ;
#78071 = ORIENTED_EDGE ( 'NONE', *, *, #6986, .T. ) ;
#78072 = VECTOR ( 'NONE', #16165, 39.37007874015748143 ) ;
#78073 = CARTESIAN_POINT ( 'NONE',  ( -1.627296587926508442, -0.6046776061558809534, -0.2411417322834644161 ) ) ;
#78074 = CARTESIAN_POINT ( 'NONE',  ( 0.000000000000000000, 2.165354330708661568, 0.000000000000000000 ) ) ;
#78075 = CARTESIAN_POINT ( 'NONE',  ( 0.4724409448818880919, 0.1265901696525020825, -2.644356955380577467 ) ) ;
#78076 = CARTESIAN_POINT ( 'NONE',  ( 3.900966923095589678, 2.677165354330708791, -0.5314960629921260393 ) ) ;
#78077 = CARTESIAN_POINT ( 'NONE',  ( -0.7808398950131222316, -0.2845877964562161244, -0.3641732283464567121 ) ) ;
#78078 = CARTESIAN_POINT ( 'NONE',  ( -1.528871391076114250, -0.6692913385826771977, 0.1292274648535927661 ) ) ;
#78079 = CARTESIAN_POINT ( 'NONE',  ( 0.7414698162729663755, 0.2952755905511811885, 0.1292274648535926551 ) ) ;
#78080 = ORIENTED_EDGE ( 'NONE', *, *, #75407, .T. ) ;
#78082 = CARTESIAN_POINT ( 'NONE',  ( 0.000000000000000000, 0.7086614173228346081, 0.000000000000000000 ) ) ;
#78081 = CARTESIAN_POINT ( 'NONE',  ( -0.7443564586554828333, 2.208176010637902031, 0.5309055118110236338 ) ) ;
#78083 = CARTESIAN_POINT ( 'NONE',  ( 1.181102362204725198, -0.1870078740157479769, 0.4822834645669291653 ) ) ;
#78084 = CARTESIAN_POINT ( 'NONE',  ( 1.555118110236221041, -0.4536011799217367080, 0.2665933059059888421 ) ) ;
#78086 = B_SPLINE_CURVE_WITH_KNOTS ( 'NONE', 3,
 ( #7026, #7451, #23391, #22980, #3218, #79840, #54543 ),
 .UNSPECIFIED., .F., .F.,
 ( 4, 3, 4 ),
 ( 1.734723475976807094E-18, 0.001246230184515576727, 0.002492489877932654602 ),
 .UNSPECIFIED. ) ;
#78085 = CARTESIAN_POINT ( 'NONE',  ( 0.3392501089628018329, 0.1958661417322835052, -0.8411880332995258502 ) ) ;
#78087 = CARTESIAN_POINT ( 'NONE',  ( -0.9776902887139098386, -0.5511811023622046335, 0.09757992244046803654 ) ) ;
#78088 = CARTESIAN_POINT ( 'NONE',  ( -1.541994750656167090, -0.5511811023622048555, -0.09757992244046775898 ) ) ;
#78089 = CARTESIAN_POINT ( 'NONE',  ( -9.594673741351313045E-17, 0.3917322834645670104, -1.187007874015748143 ) ) ;
#78090 = CARTESIAN_POINT ( 'NONE',  ( 0.5971128608923890191, -0.6692913385826771977, 0.1292274648535927661 ) ) ;
#78091 = CARTESIAN_POINT ( 'NONE',  ( -0.7414698162729651543, -0.5511811023622046335, 0.09757992244046803654 ) ) ;
#78092 = CARTESIAN_POINT ( 'NONE',  ( -0.09842519685039295696, 0.07958543189024071263, -0.2665933059059888421 ) ) ;
#78093 = CARTESIAN_POINT ( 'NONE',  ( -0.2099737532808391705, -0.6046776061558809534, -0.2411417322834644161 ) ) ;
#78094 = CARTESIAN_POINT ( 'NONE',  ( -1.095800524934382292, -0.2845877964562161244, -0.3641732283464567121 ) ) ;
#78095 = CARTESIAN_POINT ( 'NONE',  ( -0.1049643490035302301, -0.3917322834645671770, 0.08856336138351518505 ) ) ;
#78096 = CARTESIAN_POINT ( 'NONE',  ( 0.6692913385826777528, 0.2952755905511811885, 0.000000000000000000 ) ) ;
#78097 = CARTESIAN_POINT ( 'NONE',  ( -1.318897637795274802, 0.1660481256975885056, 0.3530559997133364547 ) ) ;
#78098 = CARTESIAN_POINT ( 'NONE',  ( -0.2362204724409451284, 0.4091458600556402425, -1.349737532808398921 ) ) ;
#78099 = CARTESIAN_POINT ( 'NONE',  ( -0.6233595800524928121, -0.05778040916215522460, 0.4822834645669289988 ) ) ;
#78100 = CARTESIAN_POINT ( 'NONE',  ( -0.1706036745406816491, -0.3690944881889763329, 0.3153832671262228327 ) ) ;
#78101 = CARTESIAN_POINT ( 'NONE',  ( -1.463254593175852492, 0.2952755905511811885, 0.1292274648535926551 ) ) ;
#78102 = CARTESIAN_POINT ( 'NONE',  ( 0.6824146981627303710, -0.5023911411419708095, 0.1820866141732285504 ) ) ;
#78103 = CARTESIAN_POINT ( 'NONE',  ( -0.3280839895013117347, -0.3690944881889763329, 0.3153832671262228327 ) ) ;
#78104 = CARTESIAN_POINT ( 'NONE',  ( -0.7349081364829390672, 0.2306618581243847221, -0.2411417322834647770 ) ) ;
#78105 = CARTESIAN_POINT ( 'NONE',  ( -1.161417322834644716, -0.5400638737290845981, -0.3530559997133363437 ) ) ;
#78106 = CARTESIAN_POINT ( 'NONE',  ( -1.404199475065615932, -0.4281496062992127816, -0.4176697321401328100 ) ) ;
#78107 = CYLINDRICAL_SURFACE ( 'NONE', #77010, 0.4724409448818898682 ) ;
#78108 = CARTESIAN_POINT ( 'NONE',  ( 1.240157480314961314, 0.07958543189024071263, -0.2665933059059888421 ) ) ;
#78109 = CARTESIAN_POINT ( 'NONE',  ( 0.2296587926509192634, -0.3162353388693405765, 0.4822834645669290543 ) ) ;
#78110 = CARTESIAN_POINT ( 'NONE',  ( -1.469816272965878357, 0.2306618581243848609, 0.2411417322834645549 ) ) ;
#78111 = CARTESIAN_POINT ( 'NONE',  ( -1.692913385826770645, 0.2952755905511811885, 0.000000000000000000 ) ) ;
#78112 = EDGE_LOOP ( 'NONE', ( #22058, #51838, #38541, #65640 ) ) ;
#78113 = CARTESIAN_POINT ( 'NONE',  ( 0.1998031496062994128, -0.3460692066303957537, -2.373359580052493367 ) ) ;
#78114 = CARTESIAN_POINT ( 'NONE',  ( -1.082677165354329896, -0.4536011799217368745, -0.2665933059059886201 ) ) ;
#78115 = CARTESIAN_POINT ( 'NONE',  ( 0.6627296587926515548, 0.2952755905511811885, 0.1292274648535926551 ) ) ;
#78116 = CARTESIAN_POINT ( 'NONE',  ( -1.095800524934382292, -0.08942795157527998196, 0.3641732283464567121 ) ) ;
#78117 = CARTESIAN_POINT ( 'NONE',  ( 0.1070741851644054776, -0.3996062992125984925, -1.894356955380577023 ) ) ;
#78118 = CARTESIAN_POINT ( 'NONE',  ( -1.305774278215222184, -0.6692913385826773087, -0.1292274648535924053 ) ) ;
#78119 = CARTESIAN_POINT ( 'NONE',  ( 1.056430446194226658, 0.2952755905511811885, 0.1292274648535926551 ) ) ;
#78120 = CARTESIAN_POINT ( 'NONE',  ( 0.3871391076115493490, -0.3162353388693405765, 0.4822834645669290543 ) ) ;
#78121 = CARTESIAN_POINT ( 'NONE',  ( 1.397637795275591177, -0.5400638737290844871, 0.3530559997133364547 ) ) ;
#78122 = CARTESIAN_POINT ( 'NONE',  ( -1.430446194225721390, -0.3690944881889763329, 0.3153832671262228327 ) ) ;
#78123 = CARTESIAN_POINT ( 'NONE',  ( 0.1070741851644053527, 0.3996062992125985480, -1.172572178477690352 ) ) ;
#78124 = CARTESIAN_POINT ( 'NONE',  ( -0.2925321140481932924, 0.2925321140481931814, -1.279527559055118058 ) ) ;
#78125 = CARTESIAN_POINT ( 'NONE',  ( -9.674558042662121740E-17, 0.3949938075777409963, -0.7874015748031496509 ) ) ;
#78126 = CARTESIAN_POINT ( 'NONE',  ( 0.3443296571407519213, 1.210789077865271013, -1.720740846584503103 ) ) ;
#78127 = CARTESIAN_POINT ( 'NONE',  ( 0.9383202099737538715, -0.08942795157528024563, -0.3641732283464568787 ) ) ;
#78128 = CARTESIAN_POINT ( 'NONE',  ( 0.1312335958005255154, -0.5023911411419708095, 0.1820866141732285504 ) ) ;
#78129 = COLOUR_RGB ( '', 0.31764706, 0.68627451, 0.89019608) ;
#78130 = CARTESIAN_POINT ( 'NONE',  ( 0.2099737532808405305, 0.2306618581243847221, -0.2411417322834647770 ) ) ;
#78131 = CARTESIAN_POINT ( 'NONE',  ( 1.233595800524935227, -0.6046776061558807314, 0.2411417322834647770 ) ) ;
#78132 = CARTESIAN_POINT ( 'NONE',  ( 0.2891555358219910499, 0.2891555358219910499, -1.946850393700787496 ) ) ;
#78133 = CARTESIAN_POINT ( 'NONE',  ( 0.2034120734908144990, -0.5511811023622046335, 0.09757992244046803654 ) ) ;
#78134 = CARTESIAN_POINT ( 'NONE',  ( -0.7545931758530176614, -0.6692913385826773087, -0.1292274648535924053 ) ) ;
#78135 = CARTESIAN_POINT ( 'NONE',  ( -1.489501312335957062, -0.05778040916215522460, 0.4822834645669289988 ) ) ;
#78136 = CARTESIAN_POINT ( 'NONE',  ( 0.7086614173228353852, -0.1870078740157479769, 0.4822834645669291653 ) ) ;
#78137 = CARTESIAN_POINT ( 'NONE',  ( 0.4724409448818898682, 2.892866454678787531E-17, -2.165354330708661568 ) ) ;
#78138 = CARTESIAN_POINT ( 'NONE',  ( 1.603475055217291612, 1.330568129716842130, 0.04573490813648269093 ) ) ;
#78139 = VERTEX_POINT ( 'NONE', #79465 ) ;
#78140 = EDGE_CURVE ( 'NONE', #80835, #48838, #39460, .T. ) ;
#78141 = ORIENTED_EDGE ( 'NONE', *, *, #50179, .F. ) ;
#78142 = CARTESIAN_POINT ( 'NONE',  ( -1.312335958005248715, -0.6046776061558809534, -0.2411417322834644161 ) ) ;
#78144 = CARTESIAN_POINT ( 'NONE',  ( -1.253280839895012377, -0.3162353388693409650, -0.4822834645669289433 ) ) ;
#78143 = CARTESIAN_POINT ( 'NONE',  ( -0.6036745406824141069, -0.5023911411419708095, -0.1820866141732282451 ) ) ;
#78145 = CARTESIAN_POINT ( 'NONE',  ( 0.3392501089628018329, 0.1958661417322835052, -2.258510867945195066 ) ) ;
#78146 = CARTESIAN_POINT ( 'NONE',  ( 0.1998031496062994128, -0.3460692066303957537, -2.845800524934383624 ) ) ;
#78147 = CARTESIAN_POINT ( 'NONE',  ( 1.502624671916010790, -0.05778040916215522460, 0.4822834645669289988 ) ) ;
#78148 = VECTOR ( 'NONE', #61508, 39.37007874015748143 ) ;
#78149 = CARTESIAN_POINT ( 'NONE',  ( -1.062992125984250968, 0.2952755905511811885, 0.000000000000000000 ) ) ;
#78150 = CARTESIAN_POINT ( 'NONE',  ( 0.2821522309711292364, -0.6692913385826771977, 0.1292274648535927661 ) ) ;
#78151 = CARTESIAN_POINT ( 'NONE',  ( -1.456692913385826182, 0.2952755905511811885, 0.000000000000000000 ) ) ;
#78152 = CARTESIAN_POINT ( 'NONE',  ( -0.3392501089628018329, -0.1958661417322836440, -2.652211655346770502 ) ) ;
#78153 = CARTESIAN_POINT ( 'NONE',  ( 0.4461942257217855201, -0.6046776061558807314, 0.2411417322834647770 ) ) ;
#78154 = CARTESIAN_POINT ( 'NONE',  ( -0.2867679344610364334, -0.2867679344610367109, -1.783464566929133577 ) ) ;
#78155 = CARTESIAN_POINT ( 'NONE',  ( -0.6692913385826764205, 0.1771653543307087630, 0.000000000000000000 ) ) ;
#78156 = VERTEX_POINT ( 'NONE', #21375 ) ;
#78157 = CARTESIAN_POINT ( 'NONE',  ( 0.3420746716998660508, -0.1974969037888703871, -1.994750656167979086 ) ) ;
#78158 = ORIENTED_EDGE ( 'NONE', *, *, #13121, .F. ) ;
#78159 = LINE ( 'NONE', #46144, #20726 ) ;
#78160 = CARTESIAN_POINT ( 'NONE',  ( -1.318897637795274802, -0.5400638737290845981, -0.3530559997133363437 ) ) ;
#78161 = CARTESIAN_POINT ( 'NONE',  ( -1.351706036745406347, -0.4281496062992124485, 0.4176697321401328655 ) ) ;
#78162 = CARTESIAN_POINT ( 'NONE',  ( 0.3460692066303959757, -0.1998031496062991907, -0.7349081364829396223 ) ) ;
#78163 = CARTESIAN_POINT ( 'NONE',  ( -1.627296587926508442, -0.6046776061558809534, -0.2411417322834644161 ) ) ;
#78164 = CARTESIAN_POINT ( 'NONE',  ( -1.181102362204723644, -0.1870078740157480879, -0.4822834645669291653 ) ) ;
#78165 = CARTESIAN_POINT ( 'NONE',  ( -1.502624671916009680, -0.3162353388693405765, 0.4822834645669290543 ) ) ;
#78166 = CARTESIAN_POINT ( 'NONE',  ( -0.03443470937339728616, 0.2929341459200028863, -1.537015892239756099 ) ) ;
#78167 = CARTESIAN_POINT ( 'NONE',  ( 1.614173228346457378, 1.267785121476991073, -0.1372047244094476148 ) ) ;
#78168 = CARTESIAN_POINT ( 'NONE',  ( 0.3083989501312343062, -0.08942795157528024563, -0.3641732283464568787 ) ) ;
#78169 = CARTESIAN_POINT ( 'NONE',  ( 0.4469779880791947546, 1.697109554835854572, 2.112686649479581735 ) ) ;
#78170 = CARTESIAN_POINT ( 'NONE',  ( -0.3392501089628017219, -0.1958661417322836718, -0.2946194225721785465 ) ) ;
#78171 = CARTESIAN_POINT ( 'NONE',  ( -0.4330708661417315697, 0.1771653543307087630, 0.000000000000000000 ) ) ;
#78172 = CARTESIAN_POINT ( 'NONE',  ( -0.6299212598425188991, -0.1870078740157480879, -0.4822834645669291653 ) ) ;
#78173 = CARTESIAN_POINT ( 'NONE',  ( 0.7480314960629927956, -0.6692913385826771977, 8.415575281601705876E-17 ) ) ;
#78174 = CARTESIAN_POINT ( 'NONE',  ( -0.8727034120734901146, -0.3162353388693405765, 0.4822834645669290543 ) ) ;
#78175 = ORIENTED_EDGE ( 'NONE', *, *, #55030, .T. ) ;
#78176 = VERTEX_POINT ( 'NONE', #40318 ) ;
#78177 = CARTESIAN_POINT ( 'NONE',  ( 0.1998031496062992463, 0.3460692066303959202, -1.953412073490813805 ) ) ;
#78178 = CARTESIAN_POINT ( 'NONE',  ( -1.062992125984250968, -0.6692913385826771977, 8.415575281601705876E-17 ) ) ;
#78179 = CARTESIAN_POINT ( 'NONE',  ( 0.7480314960629927956, -0.6692913385826771977, 8.415575281601705876E-17 ) ) ;
#78180 = DIRECTION ( 'NONE',  ( 0.000000000000000000, 0.000000000000000000, 1.000000000000000000 ) ) ;
#78181 = CARTESIAN_POINT ( 'NONE',  ( -2.199130528046420221E-22, 1.075705580628688596, 0.2362204724409449064 ) ) ;
#78182 = CARTESIAN_POINT ( 'NONE',  ( 0.2362204724409449064, 0.4091458600556404646, -1.089238845144356871 ) ) ;
#78183 = CARTESIAN_POINT ( 'NONE',  ( 2.170146923806595129, 1.537401574803149984, 0.4744094488188975722 ) ) ;
#78184 = CARTESIAN_POINT ( 'NONE',  ( -0.3917322834645670104, -7.196005306013484475E-17, -0.1889763779527558474 ) ) ;
#78185 = CARTESIAN_POINT ( 'NONE',  ( 0.3917322834645670104, -0.1049643490035303273, -2.558398950131233196 ) ) ;
#78186 = CARTESIAN_POINT ( 'NONE',  ( -0.4199475065616791736, -0.6046776061558807314, 0.2411417322834647770 ) ) ;
#78187 = CARTESIAN_POINT ( 'NONE',  ( -1.614173228346455824, 0.1771653543307087630, 0.000000000000000000 ) ) ;
#78188 = CARTESIAN_POINT ( 'NONE',  ( -0.8858267716535425107, 0.1660481256975883668, -0.3530559997133364547 ) ) ;
#78189 = CARTESIAN_POINT ( 'NONE',  ( -0.2925321140481932369, 0.2925321140481931259, 0.06102362204724406242 ) ) ;
#78191 = DIRECTION ( 'NONE',  ( 0.000000000000000000, 0.000000000000000000, 1.000000000000000000 ) ) ;
#78190 = CARTESIAN_POINT ( 'NONE',  ( -1.286089238845143479, -0.6046776061558807314, 0.2411417322834647770 ) ) ;
#78192 = CARTESIAN_POINT ( 'NONE',  ( -0.8267716535433065062, -0.6692913385826771977, 8.415575281601705876E-17 ) ) ;
#78193 = CARTESIAN_POINT ( 'NONE',  ( -0.3871391076115479057, -0.3162353388693409650, -0.4822834645669289433 ) ) ;
#78194 = CARTESIAN_POINT ( 'NONE',  ( 0.3949938075777409408, -0.1058382717557499186, -2.550524934383202158 ) ) ;
#78195 = CARTESIAN_POINT ( 'NONE',  ( 0.7611548556430451917, -0.5023911411419708095, 0.1820866141732285504 ) ) ;
#78196 = LINE ( 'NONE', #46179, #33074 ) ;
#78197 = CARTESIAN_POINT ( 'NONE',  ( 0.3346456692913393205, -0.4536011799217368745, -0.2665933059059886201 ) ) ;
#78198 = CARTESIAN_POINT ( 'NONE',  ( 1.489501312335958172, -0.08942795157528024563, -0.3641732283464568787 ) ) ;
#78199 = VECTOR ( 'NONE', #70910, 39.37007874015748143 ) ;
#78200 = CARTESIAN_POINT ( 'NONE',  ( 1.496062992125984703, -0.1870078740157480879, -0.4822834645669291653 ) ) ;
#78201 = CARTESIAN_POINT ( 'NONE',  ( 0.1509186351706045259, -0.08942795157528024563, -0.3641732283464568787 ) ) ;
#78202 = CARTESIAN_POINT ( 'NONE',  ( -0.3392501089628017219, -0.1958661417322836718, -1.934383202099737575 ) ) ;
#78203 = CARTESIAN_POINT ( 'NONE',  ( -1.423884514435694859, -0.05778040916215560624, -0.4822834645669293319 ) ) ;
#78204 = CARTESIAN_POINT ( 'NONE',  ( 1.358267716535433323, -0.5400638737290845981, -0.3530559997133363437 ) ) ;
#78205 = CARTESIAN_POINT ( 'NONE',  ( 0.3458507752293908943, -0.3458507752293908943, -0.01771653543307087630 ) ) ;
#78206 = CARTESIAN_POINT ( 'NONE',  ( -0.4855643044619415427, -0.004921259842519870586, -0.3153832671262229437 ) ) ;
#78207 = CARTESIAN_POINT ( 'NONE',  ( -0.4461942257217840213, 0.2306618581243848609, 0.2411417322834645549 ) ) ;
#78208 = CARTESIAN_POINT ( 'NONE',  ( 0.2296587926509192634, -0.3162353388693405765, 0.4822834645669290543 ) ) ;
#78209 = CARTESIAN_POINT ( 'NONE',  ( -1.016821367227983997, 1.553445615596289908, -0.4744094488188977388 ) ) ;
#78210 = CARTESIAN_POINT ( 'NONE',  ( 0.8858267716535438430, -0.4536011799217368745, -0.2665933059059886201 ) ) ;
#78211 = CARTESIAN_POINT ( 'NONE',  ( 0.3083989501312343062, -0.2845877964562159024, 0.3641732283464567677 ) ) ;
#78212 = CARTESIAN_POINT ( 'NONE',  ( -0.1246719160104980823, -0.6692913385826773087, -0.1292274648535924053 ) ) ;
#78213 = CARTESIAN_POINT ( 'NONE',  ( -1.660104986876639543, -0.05778040916215560624, -0.4822834645669293319 ) ) ;
#78214 = CARTESIAN_POINT ( 'NONE',  ( -0.6233595800524928121, -0.2845877964562161244, -0.3641732283464567121 ) ) ;
#78215 = DIRECTION ( 'NONE',  ( 0.000000000000000000, 0.000000000000000000, -1.000000000000000000 ) ) ;
#78216 = CARTESIAN_POINT ( 'NONE',  ( 0.4133858267716541968, 0.1660481256975885056, 0.3530559997133364547 ) ) ;
#78217 = CARTESIAN_POINT ( 'NONE',  ( -0.7611548556430438595, -0.6046776061558809534, -0.2411417322834644161 ) ) ;
#78218 = CARTESIAN_POINT ( 'NONE',  ( 0.1998031496062994128, -0.3460692066303957537, -1.270997375328083878 ) ) ;
#78219 = CARTESIAN_POINT ( 'NONE',  ( 0.3392501089628018329, 0.1958661417322835607, -2.578083989501311901 ) ) ;
#78220 = CARTESIAN_POINT ( 'NONE',  ( 0.1049868766404206816, -0.5023911411419708095, -0.1820866141732282451 ) ) ;
#78221 = CARTESIAN_POINT ( 'NONE',  ( -0.5971128608923877978, -0.6692913385826773087, -0.1292274648535924053 ) ) ;
#78222 = CARTESIAN_POINT ( 'NONE',  ( -0.9645669291338575535, 0.1660481256975883668, -0.3530559997133364547 ) ) ;
#78223 = CARTESIAN_POINT ( 'NONE',  ( -1.351706036745406347, -0.3690944881889763329, 0.3153832671262228327 ) ) ;
#78224 = CARTESIAN_POINT ( 'NONE',  ( 1.673228346456693494, 0.1660481256975885056, 0.3530559997133364547 ) ) ;
#78225 = CARTESIAN_POINT ( 'NONE',  ( -0.7349081364829387342, -0.5023911411419708095, 0.1820866141732285504 ) ) ;
#78226 = LINE ( 'NONE', #20559, #26453 ) ;
#78227 = CARTESIAN_POINT ( 'NONE',  ( 1.456692913385827515, 0.2952755905511811885, 0.000000000000000000 ) ) ;
#78228 = CARTESIAN_POINT ( 'NONE',  ( 4.893765752498283924E-17, -0.3996062992125986035, -0.07874015748031498729 ) ) ;
#78229 = CARTESIAN_POINT ( 'NONE',  ( 0.2867679344610366554, 0.2867679344610366554, -2.339258160926195984 ) ) ;
#78230 = ORIENTED_EDGE ( 'NONE', *, *, #20875, .T. ) ;
#78231 = CARTESIAN_POINT ( 'NONE',  ( 0.4562720003150377845, 1.668198494846154567, -2.594288149172116142 ) ) ;
#78232 = CARTESIAN_POINT ( 'NONE',  ( 1.463254593175853824, 0.1771653543307087075, -0.09757992244046823083 ) ) ;
#78233 = CARTESIAN_POINT ( 'NONE',  ( -1.312335958005248715, -0.6046776061558809534, -0.2411417322834644161 ) ) ;
#78234 = B_SPLINE_CURVE_WITH_KNOTS ( 'NONE', 3,
 ( #50021, #55920, #4179, #31492, #49611, #57153, #17650 ),
 .UNSPECIFIED., .F., .F.,
 ( 4, 3, 4 ),
 ( 0.000000000000000000, 0.001246232571205256601, 0.002492492258783257208 ),
 .UNSPECIFIED. ) ;
#78235 = CARTESIAN_POINT ( 'NONE',  ( 1.062992125984252745, -0.6692913385826771977, 8.415575281601705876E-17 ) ) ;
#78236 = CARTESIAN_POINT ( 'NONE',  ( 0.3917322834645670104, 2.398668435337828261E-17, -2.407480314960630086 ) ) ;
#78237 = CARTESIAN_POINT ( 'NONE',  ( 1.601049868766404982, -0.5023911411419708095, -0.1820866141732282451 ) ) ;
#78238 = EDGE_CURVE ( 'NONE', #69738, #11377, #13939, .T. ) ;
#78239 = CARTESIAN_POINT ( 'NONE',  ( 0.3412073490813655186, -0.6046776061558809534, -0.2411417322834644161 ) ) ;
#78240 = CARTESIAN_POINT ( 'NONE',  ( -0.5052493438320203589, 0.2952755905511810774, -0.1292274648535930714 ) ) ;
#78241 = CARTESIAN_POINT ( 'NONE',  ( 0.1527255018715594492, 1.087979116479378616, -3.934072586421137441 ) ) ;
#78242 = CARTESIAN_POINT ( 'NONE',  ( 0.3460692066303959757, -0.1998031496062991907, -1.994750656167979086 ) ) ;
#78243 = CARTESIAN_POINT ( 'NONE',  ( 0.9251968503937015864, -0.4536011799217367080, 0.2665933059059888421 ) ) ;
#78244 = CARTESIAN_POINT ( 'NONE',  ( 0.3996062992125986035, 2.446882876249141962E-17, -1.220472440944881942 ) ) ;
#78245 = ORIENTED_EDGE ( 'NONE', *, *, #15589, .F. ) ;
#78246 = CARTESIAN_POINT ( 'NONE',  ( 0.2867679344610366554, 0.2867679344610366554, -0.1345337514773772281 ) ) ;
#78247 = ORIENTED_EDGE ( 'NONE', *, *, #11555, .T. ) ;
#78248 = CARTESIAN_POINT ( 'NONE',  ( -0.1181102362204717315, 0.2952755905511811885, 0.000000000000000000 ) ) ;
#78249 = PRODUCT_DEFINITION_SHAPE ( 'NONE', 'NONE',  #83313 ) ;
#78250 = CARTESIAN_POINT ( 'NONE',  ( 1.423884514435696191, -0.05778040916215522460, 0.4822834645669289988 ) ) ;
#78251 = CARTESIAN_POINT ( 'NONE',  ( 0.3805774278215230400, -0.4281496062992124485, 0.4176697321401328655 ) ) ;
#78252 = CARTESIAN_POINT ( 'NONE',  ( 1.345144356955381593, -0.05778040916215522460, 0.4822834645669289988 ) ) ;
#78253 = CARTESIAN_POINT ( 'NONE',  ( -0.5511811023622038563, -0.1870078740157479769, 0.4822834645669291653 ) ) ;
#78254 = CARTESIAN_POINT ( 'NONE',  ( -0.08530183727034056085, -0.05778040916215560624, -0.4822834645669293319 ) ) ;
#78255 = CARTESIAN_POINT ( 'NONE',  ( -1.528871391076114250, -0.6692913385826771977, 0.1292274648535927661 ) ) ;
#78256 = CARTESIAN_POINT ( 'NONE',  ( 1.417322834645670104, -0.1870078740157479769, 0.4822834645669291653 ) ) ;
#78257 = CARTESIAN_POINT ( 'NONE',  ( 1.200787401574803681, 0.1660481256975885056, 0.3530559997133364547 ) ) ;
#78258 = CARTESIAN_POINT ( 'NONE',  ( -0.1049643490035302024, -0.3917322834645671215, -0.6942257217847765949 ) ) ;
#78259 = CARTESIAN_POINT ( 'NONE',  ( 0.5839895013123367340, 0.1771653543307087630, 0.09757992244046791164 ) ) ;
#78260 = ORIENTED_EDGE ( 'NONE', *, *, #31580, .T. ) ;
#78261 = CARTESIAN_POINT ( 'NONE',  ( -9.674558042662121740E-17, 0.3949938075777409963, -0.4724409448818898127 ) ) ;
#78262 = VERTEX_POINT ( 'NONE', #27683 ) ;
#78263 = CARTESIAN_POINT ( 'NONE',  ( -0.2952755905511804668, 0.07958543189024085140, 0.2665933059059887866 ) ) ;
#78264 = CARTESIAN_POINT ( 'NONE',  ( -0.1902887139107604098, 0.2952755905511810774, -0.1292274648535930714 ) ) ;
#78265 = CARTESIAN_POINT ( 'NONE',  ( 2.610466197084835294, 1.379671404989097239, 0.4476723508032718346 ) ) ;
#78266 = CARTESIAN_POINT ( 'NONE',  ( 0.02624671916010564918, 0.2306618581243848609, 0.2411417322834645549 ) ) ;
#78267 = CARTESIAN_POINT ( 'NONE',  ( 0.1115485564304467270, -0.6692913385826773087, -0.1292274648535924053 ) ) ;
#78268 = CARTESIAN_POINT ( 'NONE',  ( -0.9776902887139098386, 0.2952755905511810774, -0.1292274648535930714 ) ) ;
#78269 = CARTESIAN_POINT ( 'NONE',  ( -1.010498687664041384, -0.4281496062992127816, -0.4176697321401328100 ) ) ;
#78270 = CARTESIAN_POINT ( 'NONE',  ( 1.253280839895013710, -0.08942795157528024563, -0.3641732283464568787 ) ) ;
#78271 = CARTESIAN_POINT ( 'NONE',  ( -1.568241469816272105, -0.3162353388693409650, -0.4822834645669289433 ) ) ;
#78272 = DIRECTION ( 'NONE',  ( 0.000000000000000000, -1.000000000000000000, 0.000000000000000000 ) ) ;
#78273 = CARTESIAN_POINT ( 'NONE',  ( 0.9055118110236227702, -0.5511811023622047445, 6.969142054262312111E-17 ) ) ;
#78274 = CARTESIAN_POINT ( 'NONE',  ( 0.5577427821522316087, -0.05778040916215522460, 0.4822834645669289988 ) ) ;
#78275 = CARTESIAN_POINT ( 'NONE',  ( 0.7349081364829403995, 0.2306618581243848609, 0.2411417322834645549 ) ) ;
#78276 = CARTESIAN_POINT ( 'NONE',  ( -0.1070741851644051862, -0.3996062992125987146, -1.332020997375328086 ) ) ;
#78277 = CARTESIAN_POINT ( 'NONE',  ( -1.679790026246718693, 0.2306618581243847221, -0.2411417322834647770 ) ) ;
#78278 = CARTESIAN_POINT ( 'NONE',  ( -0.1998031496062991630, -0.3460692066303959202, -0.9297900262467192478 ) ) ;
#78279 = CARTESIAN_POINT ( 'NONE',  ( 0.3996062992125985480, 2.446882876249141654E-17, -0.3523622047244094335 ) ) ;
#78280 = CARTESIAN_POINT ( 'NONE',  ( -0.6496062992125976043, -0.5400638737290844871, 0.3530559997133364547 ) ) ;
#78281 = B_SPLINE_CURVE_WITH_KNOTS ( 'NONE', 3,
 ( #43456, #30014, #43047, #42644, #55677, #81386, #12323 ),
 .UNSPECIFIED., .F., .F.,
 ( 4, 3, 4 ),
 ( 5.551115123125782702E-17, 0.001246230184515611855, 0.002492489877932689731 ),
 .UNSPECIFIED. ) ;
#78282 = CARTESIAN_POINT ( 'NONE',  ( -0.4724409448818898682, -8.678599364036362592E-17, -0.1968503937007874127 ) ) ;
#78283 = CARTESIAN_POINT ( 'NONE',  ( 0.3392501089628018884, -0.1958661417322834220, -2.236876640419947826 ) ) ;
#78284 = CARTESIAN_POINT ( 'NONE',  ( -1.292650918635170010, 0.1771653543307087075, -0.09757992244046823083 ) ) ;
#78285 = CARTESIAN_POINT ( 'NONE',  ( 1.417322834645670104, -0.1870078740157479769, 0.4822834645669291653 ) ) ;
#78286 = CARTESIAN_POINT ( 'NONE',  ( 1.062992125984252745, 0.2952755905511811885, 0.000000000000000000 ) ) ;
#78287 = CARTESIAN_POINT ( 'NONE',  ( -0.1837270341207340729, 0.1283753931104746893, -0.1820866141732285504 ) ) ;
#78288 = CARTESIAN_POINT ( 'NONE',  ( 0.6167979002624678353, -0.4281496062992124485, 0.4176697321401328655 ) ) ;
#78289 = CARTESIAN_POINT ( 'NONE',  ( 0.4724409448818898682, 2.892866454678787531E-17, -2.084645669291338432 ) ) ;
#78290 = CARTESIAN_POINT ( 'NONE',  ( -0.2296587926509179312, -0.08942795157527998196, 0.3641732283464567121 ) ) ;
#78291 = CARTESIAN_POINT ( 'NONE',  ( -0.2362204724409442680, -0.1870078740157480879, -0.4822834645669291653 ) ) ;
#78292 = CARTESIAN_POINT ( 'NONE',  ( 0.1974969037888706092, -0.3420746716998660508, -1.428477690288714186 ) ) ;
#78293 = CARTESIAN_POINT ( 'NONE',  ( -1.095800524934382292, -0.05778040916215522460, 0.4822834645669289988 ) ) ;
#78294 = CARTESIAN_POINT ( 'NONE',  ( 0.6233595800524939223, -0.2845877964562159024, 0.3641732283464567677 ) ) ;
#78295 = CARTESIAN_POINT ( 'NONE',  ( -2.565964038698705707, 1.605872332714550099, -0.4695140184743391010 ) ) ;
#78296 = CARTESIAN_POINT ( 'NONE',  ( -0.7874015748031489847, -0.1870078740157479769, 0.4822834645669291653 ) ) ;
#78297 = CARTESIAN_POINT ( 'NONE',  ( -0.2624671916010490880, -0.5023911411419708095, 0.1820866141732285504 ) ) ;
#78298 = CARTESIAN_POINT ( 'NONE',  ( 1.614173228346456712, 2.401574803149606474, 0.5309055118110233007 ) ) ;
#78299 = CARTESIAN_POINT ( 'NONE',  ( -0.8333333333333323711, -0.6692913385826773087, -0.1292274648535924053 ) ) ;
#78300 = CARTESIAN_POINT ( 'NONE',  ( -0.6036745406824141069, -0.6046776061558809534, -0.2411417322834644161 ) ) ;
#78301 = CARTESIAN_POINT ( 'NONE',  ( 0.01968503937007957949, -0.5400638737290845981, -0.3530559997133363437 ) ) ;
#78302 = CARTESIAN_POINT ( 'NONE',  ( 0.1998031496062994128, -0.3460692066303957537, -2.058398950131233640 ) ) ;
#78303 = CARTESIAN_POINT ( 'NONE',  ( 0.1958661417322834497, 0.3392501089628018329, -2.271634227525247685 ) ) ;
#78304 = CARTESIAN_POINT ( 'NONE',  ( -1.653543307086613234, -0.1870078740157480601, -0.3641732283464567677 ) ) ;
#78305 = CARTESIAN_POINT ( 'NONE',  ( 0.9383202099737538715, -0.08942795157528024563, -0.3641732283464568787 ) ) ;
#78306 = CARTESIAN_POINT ( 'NONE',  ( 1.240157480314961314, -0.5400638737290844871, 0.3530559997133364547 ) ) ;
#78307 = CARTESIAN_POINT ( 'NONE',  ( -0.9514435695538050464, -0.2845877964562159024, 0.3641732283464567677 ) ) ;
#78308 = CARTESIAN_POINT ( 'NONE',  ( -1.082677165354329896, 0.07958543189024085140, 0.2665933059059887866 ) ) ;
#78309 = VECTOR ( 'NONE', #38019, 39.37007874015748143 ) ;
#78310 = CARTESIAN_POINT ( 'NONE',  ( -0.5905511811023613777, -0.6692913385826771977, 8.415575281601705876E-17 ) ) ;
#78311 = CARTESIAN_POINT ( 'NONE',  ( 0.09186351706036799403, -0.4281496062992127816, -0.4176697321401328100 ) ) ;
#78312 = CARTESIAN_POINT ( 'NONE',  ( 0.6430446194225729606, -0.3690944881889765550, -0.3153832671262227771 ) ) ;
#78313 = CARTESIAN_POINT ( 'NONE',  ( -0.2952755905511810774, 1.832348042626885162E-19, 5.524802951929911998 ) ) ;
#78314 = CARTESIAN_POINT ( 'NONE',  ( 0.9186351706036751663, -0.5023911411419708095, 0.1820866141732285504 ) ) ;
#78315 = AXIS2_PLACEMENT_3D ( 'NONE', #22830, #74190, #16536 ) ;
#78316 = CARTESIAN_POINT ( 'NONE',  ( 0.5249343832021005074, -0.6046776061558807314, 0.2411417322834647770 ) ) ;
#78317 = CARTESIAN_POINT ( 'NONE',  ( -0.3460692066303957537, -0.1998031496062994405, 0.1856955380577427484 ) ) ;
#78318 = CARTESIAN_POINT ( 'NONE',  ( -0.8923884514435688198, 0.2306618581243847221, -0.2411417322834647770 ) ) ;
#78319 = CARTESIAN_POINT ( 'NONE',  ( -0.2867679344610365999, 0.2867679344610364889, -1.206692913385826627 ) ) ;
#78320 = CARTESIAN_POINT ( 'NONE',  ( 1.351706036745407458, -0.3690944881889765550, -0.3153832671262227771 ) ) ;
#78321 = CARTESIAN_POINT ( 'NONE',  ( 0.3674540682414705883, -0.6046776061558807314, 0.2411417322834647770 ) ) ;
#78322 = CARTESIAN_POINT ( 'NONE',  ( 0.1574803149606306130, -0.1870078740157480879, -0.4822834645669291653 ) ) ;
#78323 = CARTESIAN_POINT ( 'NONE',  ( 0.006561679790026889343, -0.2845877964562161244, -0.3641732283464567121 ) ) ;
#78324 = CARTESIAN_POINT ( 'NONE',  ( 0.6171485355042644061, 0.004960608223779807216, -0.3437734562760184631 ) ) ;
#78325 = CARTESIAN_POINT ( 'NONE',  ( -0.1443569553805765515, -0.3690944881889765550, -0.3153832671262227771 ) ) ;
#78326 = CARTESIAN_POINT ( 'NONE',  ( 0.6955380577427828781, -0.4281496062992124485, 0.4176697321401328655 ) ) ;
#78327 = CARTESIAN_POINT ( 'NONE',  ( -0.9448818897637790704, -0.1870078740157479769, 0.3641732283464567677 ) ) ;
#78328 = CARTESIAN_POINT ( 'NONE',  ( -0.7808398950131222316, -0.3162353388693409650, -0.4822834645669289433 ) ) ;
#78329 = CARTESIAN_POINT ( 'NONE',  ( 0.8537221893815273299, 2.409604939980833412E-17, -0.3464511005275205946 ) ) ;
#78330 = ORIENTED_EDGE ( 'NONE', *, *, #57885, .F. ) ;
#78331 =( REPRESENTATION_RELATIONSHIP ('NONE','NONE', #79348, #33107 ) REPRESENTATION_RELATIONSHIP_WITH_TRANSFORMATION ( #55276 )SHAPE_REPRESENTATION_RELATIONSHIP( ) );
#78332 = CARTESIAN_POINT ( 'NONE',  ( -1.148293963254592542, 0.2952755905511811885, 0.1292274648535926551 ) ) ;
#78333 = CARTESIAN_POINT ( 'NONE',  ( -1.312335958005248715, -0.5023911411419708095, -0.1820866141732282451 ) ) ;
#78334 = CARTESIAN_POINT ( 'NONE',  ( -0.1443569553805768291, 0.05413385826771666132, 0.4176697321401328100 ) ) ;
#78335 = CARTESIAN_POINT ( 'NONE',  ( -1.679790026246718693, 0.2306618581243847221, -0.2411417322834647770 ) ) ;
#78336 = CARTESIAN_POINT ( 'NONE',  ( -0.5708661417322825615, -0.5400638737290844871, 0.3530559997133364547 ) ) ;
#78337 = DIRECTION ( 'NONE',  ( 0.000000000000000000, 1.000000000000000000, 0.000000000000000000 ) ) ;
#78339 = CARTESIAN_POINT ( 'NONE',  ( 1.036745406824147508, -0.4281496062992127816, -0.4176697321401328100 ) ) ;
#78338 = CARTESIAN_POINT ( 'NONE',  ( 1.640419947506562393, -0.4281496062992124485, 0.4176697321401328655 ) ) ;
#78340 = CARTESIAN_POINT ( 'NONE',  ( 1.194225721784777594, 0.05413385826771666132, 0.4176697321401328100 ) ) ;
#78341 = CARTESIAN_POINT ( 'NONE',  ( -0.2867679344610366554, 0.2867679344610365444, -2.374015748031496287 ) ) ;
#78342 = LINE ( 'NONE', #8869, #55605 ) ;
#78343 = CARTESIAN_POINT ( 'NONE',  ( -1.476377952755905110, -0.5400638737290845981, -0.3530559997133363437 ) ) ;
#78344 = CARTESIAN_POINT ( 'NONE',  ( 0.3996062992125986035, 0.1070741851644054776, 0.03280839895013121232 ) ) ;
#78345 = ORIENTED_EDGE ( 'NONE', *, *, #57908, .T. ) ;
#78346 = CARTESIAN_POINT ( 'NONE',  ( 0.05905511811023709395, -0.4536011799217367080, 0.2665933059059888421 ) ) ;
#78347 = CARTESIAN_POINT ( 'NONE',  ( -0.1958661417322836718, 0.3392501089628017219, -1.895013123359580165 ) ) ;
#78348 = ORIENTED_EDGE ( 'NONE', *, *, #11980, .F. ) ;
#78349 = CARTESIAN_POINT ( 'NONE',  ( 0.2230971128608929543, 0.05413385826771626580, -0.4176697321401330321 ) ) ;
#78350 = CARTESIAN_POINT ( 'NONE',  ( 0.09186351706036799403, -0.4281496062992127816, -0.4176697321401328100 ) ) ;
#78351 = CARTESIAN_POINT ( 'NONE',  ( -0.5380577427821514602, 0.05413385826771666132, 0.4176697321401328100 ) ) ;
#78352 = CARTESIAN_POINT ( 'NONE',  ( -1.559171609364246924, 0.4110443821404751730, 0.4177787735906735578 ) ) ;
#78353 = CARTESIAN_POINT ( 'NONE',  ( -0.7152230971128602510, -0.2845877964562159024, 0.3641732283464567677 ) ) ;
#78354 = CARTESIAN_POINT ( 'NONE',  ( -0.2647380121165202049, -0.1323808228461570424, 0.1574803149606299746 ) ) ;
#78355 = CARTESIAN_POINT ( 'NONE',  ( 0.5774278215223104249, 0.2306618581243848609, 0.2411417322834645549 ) ) ;
#78356 = CARTESIAN_POINT ( 'NONE',  ( 0.4002624671916016896, -0.2845877964562161244, -0.3641732283464567121 ) ) ;
#78357 = CARTESIAN_POINT ( 'NONE',  ( -0.5052493438320203589, 0.2952755905511810774, -0.1292274648535930714 ) ) ;
#78358 = B_SPLINE_CURVE_WITH_KNOTS ( 'NONE', 3,
 ( #31034, #19233, #36946, #37363 ),
 .UNSPECIFIED., .F., .F.,
 ( 4, 4 ),
 ( 3.593986969197074047E-07, 0.001287825409103299885 ),
 .UNSPECIFIED. ) ;
#78359 = CARTESIAN_POINT ( 'NONE',  ( -0.1049643490035306742, 0.3917322834645668994, -1.188957062170916679 ) ) ;
#78360 = CARTESIAN_POINT ( 'NONE',  ( -0.7086614173228339419, -0.1870078740157479769, 0.4822834645669291653 ) ) ;
#78361 = CARTESIAN_POINT ( 'NONE',  ( 0.000000000000000000, 2.755905511811024056, 0.000000000000000000 ) ) ;
#78362 = CARTESIAN_POINT ( 'NONE',  ( 1.443569553805774897, -0.6046776061558809534, -0.2411417322834644161 ) ) ;
#78363 = CARTESIAN_POINT ( 'NONE',  ( 1.555118110236221041, 0.07958543189024071263, -0.2665933059059888421 ) ) ;
#78364 = ORIENTED_EDGE ( 'NONE', *, *, #82011, .F. ) ;
#78365 = CARTESIAN_POINT ( 'NONE',  ( 0.2867679344610366554, -0.2867679344610365999, -2.299888082186038574 ) ) ;
#78366 = CARTESIAN_POINT ( 'NONE',  ( -0.1968503937007867743, 0.2952755905511811885, 0.000000000000000000 ) ) ;
#78367 = VERTEX_POINT ( 'NONE', #41962 ) ;
#78368 = CARTESIAN_POINT ( 'NONE',  ( -0.9908136482939626788, -0.6692913385826773087, -0.1292274648535924053 ) ) ;
#78369 = CARTESIAN_POINT ( 'NONE',  ( 1.594488188976378673, 0.1660481256975885056, 0.3530559997133364547 ) ) ;
#78370 = CARTESIAN_POINT ( 'NONE',  ( 1.181102362204724976, -0.1870078740157480879, -0.4822834645669291653 ) ) ;
#78371 = CARTESIAN_POINT ( 'NONE',  ( 0.07874015748031558404, -0.1870078740157480879, -0.4822834645669291653 ) ) ;
#78372 = AXIS2_PLACEMENT_3D ( 'NONE', #74696, #16206, #23741 ) ;
#78373 = CARTESIAN_POINT ( 'NONE',  ( -0.3674540682414689785, 0.2306618581243848609, 0.2411417322834645549 ) ) ;
#78374 = CARTESIAN_POINT ( 'NONE',  ( -0.3917322834645670104, -7.196005306013484475E-17, -1.698818897637795367 ) ) ;
#78375 = CARTESIAN_POINT ( 'NONE',  ( -1.305774278215222184, -0.6692913385826773087, -0.1292274648535924053 ) ) ;
#78376 = CARTESIAN_POINT ( 'NONE',  ( -0.7480314960629914633, -0.6692913385826771977, 8.415575281601705876E-17 ) ) ;
#78377 = CARTESIAN_POINT ( 'NONE',  ( 0.03937007874015833325, -0.5511811023622047445, 6.969142054262312111E-17 ) ) ;
#78378 = CARTESIAN_POINT ( 'NONE',  ( 1.653543307086614789, -0.1870078740157479769, 0.4822834645669291653 ) ) ;
#78379 = EDGE_CURVE ( 'NONE', #29384, #49469, #467, .T. ) ;
#78380 = CARTESIAN_POINT ( 'NONE',  ( -0.4921259842519677963, -0.5400638737290844871, 0.3530559997133364547 ) ) ;
#78381 = CARTESIAN_POINT ( 'NONE',  ( -0.2486400153428821869, 2.660739321503277841E-15, -0.3464511005275191513 ) ) ;
#78382 = CARTESIAN_POINT ( 'NONE',  ( 0.6692913385826777528, 0.2952755905511811885, 0.000000000000000000 ) ) ;
#78383 = CARTESIAN_POINT ( 'NONE',  ( 3.920801026570782888, 1.224049986093448616, -0.3575349072971868991 ) ) ;
#78384 = EDGE_CURVE ( 'NONE', #80970, #54650, #51501, .T. ) ;
#78385 = CARTESIAN_POINT ( 'NONE',  ( -0.1509186351706028884, -0.3162353388693409650, -0.4822834645669289433 ) ) ;
#78386 = CARTESIAN_POINT ( 'NONE',  ( -0.3280839895013117347, -0.3690944881889763329, 0.3153832671262228327 ) ) ;
#78388 = CARTESIAN_POINT ( 'NONE',  ( 0.6979622409133220406, -4.135162568743707313E-16, -0.4118484887281965157 ) ) ;
#78387 = CARTESIAN_POINT ( 'NONE',  ( 1.076115485564305141, 0.1283753931104746893, -0.1820866141732285504 ) ) ;
#78389 = CARTESIAN_POINT ( 'NONE',  ( 5.785732909357575061E-17, -0.4724409448818898682, -0.1555118110236220763 ) ) ;
#78390 = CARTESIAN_POINT ( 'NONE',  ( 2.118110236220474007, 0.000000000000000000, -0.4498537592782824723 ) ) ;
#78391 = CARTESIAN_POINT ( 'NONE',  ( 1.030183727034121421, -0.3162353388693409650, -0.4822834645669289433 ) ) ;
#78392 = CARTESIAN_POINT ( 'NONE',  ( 0.3949938075777408852, 0.1058382717557500435, -0.2014435695538058235 ) ) ;
#78393 = CARTESIAN_POINT ( 'NONE',  ( 0.09186351706036799403, -0.4281496062992127816, -0.4176697321401328100 ) ) ;
#78394 = CARTESIAN_POINT ( 'NONE',  ( -1.456692913385826182, 0.2952755905511811885, 0.000000000000000000 ) ) ;
#78395 = CARTESIAN_POINT ( 'NONE',  ( -1.469816272965878357, -0.6046776061558809534, -0.2411417322834644161 ) ) ;
#78396 = CARTESIAN_POINT ( 'NONE',  ( 0.04593175853018440641, 0.2952755905511810774, -0.1292274648535930714 ) ) ;
#78397 = CARTESIAN_POINT ( 'NONE',  ( -0.1058382717557503072, 0.3949938075777408852, 0.07414698162729657649 ) ) ;
#78398 = CARTESIAN_POINT ( 'NONE',  ( -1.548556430446193399, -0.5023911411419708095, -0.1820866141732282451 ) ) ;
#78399 = CARTESIAN_POINT ( 'NONE',  ( 0.4593175853018379162, -0.4281496062992124485, 0.4176697321401328655 ) ) ;
#78400 = CARTESIAN_POINT ( 'NONE',  ( 1.082677165354331228, 0.07958543189024071263, -0.2665933059059888421 ) ) ;
#78401 = CARTESIAN_POINT ( 'NONE',  ( -0.01000891935578489267, 8.471767977567108961E-16, -0.4445507791589058955 ) ) ;
#78402 = CARTESIAN_POINT ( 'NONE',  ( 0.4724409448818904789, -0.1870078740157480601, -0.3641732283464567677 ) ) ;
#78403 = CARTESIAN_POINT ( 'NONE',  ( -1.338582677165353729, -0.1870078740157479769, 0.4822834645669291653 ) ) ;
#78404 = B_SPLINE_CURVE_WITH_KNOTS ( 'NONE', 3,
 ( #22613, #36069, #4078, #4490 ),
 .UNSPECIFIED., .F., .F.,
 ( 4, 4 ),
 ( 0.09865403381126922056, 0.1000779257405588624 ),
 .UNSPECIFIED. ) ;
#78405 = CARTESIAN_POINT ( 'NONE',  ( 0.3996062992125985480, 2.446882876249141654E-17, -0.8248031496062991907 ) ) ;
#78406 = CARTESIAN_POINT ( 'NONE',  ( 1.272965879265092637, -0.4281496062992127816, -0.4176697321401328100 ) ) ;
#78407 = EDGE_CURVE ( 'NONE', #52641, #25114, #35658, .T. ) ;
#78408 = CARTESIAN_POINT ( 'NONE',  ( -0.1049643490035307020, 0.3917322834645669549, -0.4711286089238844177 ) ) ;
#78409 = EDGE_CURVE ( 'NONE', #63931, #25317, #69017, .T. ) ;
#78411 = DIRECTION ( 'NONE',  ( -0.8479387356305989609, -2.625811289636361676E-16, -0.5300942374872427143 ) ) ;
#78410 = CARTESIAN_POINT ( 'NONE',  ( 0.4921259842519691285, -0.5400638737290845981, -0.3530559997133363437 ) ) ;
#78412 = DIRECTION ( 'NONE',  ( -0.4999999999999902855, 0.7071067811865615615, 0.4999999999999899525 ) ) ;
#78413 = CARTESIAN_POINT ( 'NONE',  ( 0.3740157480314966754, 0.07958543189024071263, -0.2665933059059888421 ) ) ;
#78414 = B_SPLINE_CURVE_WITH_KNOTS ( 'NONE', 3,
 ( #24599, #32157, #38468, #5249 ),
 .UNSPECIFIED., .F., .F.,
 ( 4, 4 ),
 ( 0.07436403195037287472, 0.07455104739251855461 ),
 .UNSPECIFIED. ) ;
#78415 = CARTESIAN_POINT ( 'NONE',  ( 0.5314960629921267055, -0.5400638737290844871, 0.3530559997133364547 ) ) ;
#78416 = CARTESIAN_POINT ( 'NONE',  ( 0.7217847769028878924, 0.009842519685039467087, 0.3409548833797002021 ) ) ;
#78417 = CARTESIAN_POINT ( 'NONE',  ( -0.7677165354330699465, 0.07958543189024085140, 0.2665933059059887866 ) ) ;
#78418 = CARTESIAN_POINT ( 'NONE',  ( -1.220472440944881054, 0.2952755905511811885, 0.000000000000000000 ) ) ;
#78419 = VECTOR ( 'NONE', #76347, 39.37007874015748143 ) ;
#78420 = CARTESIAN_POINT ( 'NONE',  ( -1.430446194225721390, -0.4281496062992124485, 0.4176697321401328655 ) ) ;
#78421 = CARTESIAN_POINT ( 'NONE',  ( 1.154855643044620184, -0.6046776061558807314, 0.2411417322834647770 ) ) ;
#78422 = CARTESIAN_POINT ( 'NONE',  ( 1.522309711286089939, 0.2306618581243848609, 0.2411417322834645549 ) ) ;
#78423 = CARTESIAN_POINT ( 'NONE',  ( 1.017181940522988270, 1.506165534434959152, -0.4736389124302199383 ) ) ;
#78424 = CARTESIAN_POINT ( 'NONE',  ( 0.5577427821522314977, -0.3162353388693409650, -0.4822834645669289433 ) ) ;
#78425 = CARTESIAN_POINT ( 'NONE',  ( -0.4724409448818899238, 0.1265901696524986686, -2.786745406824146620 ) ) ;
#78426 = CARTESIAN_POINT ( 'NONE',  ( 0.000000000000000000, 0.000000000000000000, 0.000000000000000000 ) ) ;
#78427 = CARTESIAN_POINT ( 'NONE',  ( 1.345144356955381593, -0.05778040916215522460, 0.4822834645669289988 ) ) ;
#78428 = CARTESIAN_POINT ( 'NONE',  ( -1.286089238845143479, -0.5023911411419708095, 0.1820866141732285504 ) ) ;
#78429 = CARTESIAN_POINT ( 'NONE',  ( 1.135170603674541256, -0.5511811023622048555, -0.09757992244046775898 ) ) ;
#78430 = CARTESIAN_POINT ( 'NONE',  ( -1.292650918635170010, 0.1771653543307087075, -0.09757992244046823083 ) ) ;
#78431 = CARTESIAN_POINT ( 'NONE',  ( -0.3346456692913377662, 0.07958543189024071263, -0.2665933059059888421 ) ) ;
#78432 = CARTESIAN_POINT ( 'NONE',  ( -0.1265901696524993347, 0.4724409448818896462, -2.053805774278214979 ) ) ;
#78433 = CARTESIAN_POINT ( 'NONE',  ( 0.3412073490813655186, 0.1283753931104748280, 0.1820866141732283561 ) ) ;
#78434 = VECTOR ( 'NONE', #34117, 39.37007874015748143 ) ;
#78435 = CARTESIAN_POINT ( 'NONE',  ( 0.7020997375328090762, -0.3162353388693405765, 0.4822834645669290543 ) ) ;
#78436 = CARTESIAN_POINT ( 'NONE',  ( 0.9251968503937015864, -0.5400638737290844871, 0.3530559997133364547 ) ) ;
#78437 = CARTESIAN_POINT ( 'NONE',  ( 0.07874015748031558404, -0.1870078740157479769, 0.4822834645669291653 ) ) ;
#78438 = CARTESIAN_POINT ( 'NONE',  ( 0.09842519685039434474, -0.4536011799217368745, -0.2665933059059886201 ) ) ;
#78439 = CARTESIAN_POINT ( 'NONE',  ( 1.397637795275591177, -0.5400638737290844871, 0.3530559997133364547 ) ) ;
#78440 = CARTESIAN_POINT ( 'NONE',  ( -0.1902887139107604098, 0.2066929133858267098, -0.1054918080437494132 ) ) ;
#78441 = CARTESIAN_POINT ( 'NONE',  ( -0.6233595800524928121, -0.05778040916215522460, 0.4822834645669289988 ) ) ;
#78442 = CARTESIAN_POINT ( 'NONE',  ( -0.3460692066303958092, -0.1998031496062994683, -0.6824146981627295938 ) ) ;
#78443 = CARTESIAN_POINT ( 'NONE',  ( -0.3114559808008819930, 1.319608357126878184, 0.03199222220977063907 ) ) ;
#78444 = CARTESIAN_POINT ( 'NONE',  ( 0.1902887139107617975, 0.2952755905511811885, 0.1292274648535926551 ) ) ;
#78445 = CARTESIAN_POINT ( 'NONE',  ( -0.7545931758530176614, -0.6692913385826773087, -0.1292274648535924053 ) ) ;
#78446 = CARTESIAN_POINT ( 'NONE',  ( -0.2493438320209966919, 0.05413385826771626580, -0.4176697321401330321 ) ) ;
#78447 = CARTESIAN_POINT ( 'NONE',  ( -9.787531504996567848E-17, 0.3996062992125986035, -2.677165354330708347 ) ) ;
#78448 = CARTESIAN_POINT ( 'NONE',  ( -9.674558042662121740E-17, 0.3949938075777409963, -1.732283464566929165 ) ) ;
#78449 = CARTESIAN_POINT ( 'NONE',  ( 0.1958661417322836440, -0.3392501089628017219, -0.7139107611548556331 ) ) ;
#78450 = CARTESIAN_POINT ( 'NONE',  ( -0.3392501089628019995, 0.1958661417322832277, -0.9632545931758529356 ) ) ;
#78451 = CARTESIAN_POINT ( 'NONE',  ( -0.9842519685039365918, -0.5511811023622047445, 6.969142054262312111E-17 ) ) ;
#78452 = CARTESIAN_POINT ( 'NONE',  ( -0.3917322834645670104, -7.196005306013484475E-17, -1.291338582677165503 ) ) ;
#78453 = CARTESIAN_POINT ( 'NONE',  ( -1.673228346456691717, 0.1660481256975883668, -0.3530559997133364547 ) ) ;
#78454 = CARTESIAN_POINT ( 'NONE',  ( 0.3917322834645669549, 2.398668435337827645E-17, -0.04066309891632365059 ) ) ;
#78455 = EDGE_CURVE ( 'NONE', #66675, #43601, #66411, .T. ) ;
#78456 = CARTESIAN_POINT ( 'NONE',  ( 0.6167979002624679463, 0.05413385826771626580, -0.4176697321401330321 ) ) ;
#78457 = CARTESIAN_POINT ( 'NONE',  ( -0.4002624671916004129, -0.08942795157528024563, -0.3641732283464568787 ) ) ;
#78458 = CARTESIAN_POINT ( 'NONE',  ( 1.358267716535433323, -0.5400638737290845981, -0.3530559997133363437 ) ) ;
#78459 = CARTESIAN_POINT ( 'NONE',  ( 0.2296587926509192634, -0.05778040916215560624, -0.4822834645669293319 ) ) ;
#78460 = CARTESIAN_POINT ( 'NONE',  ( 0.2774227409090211371, 1.152252460295412062, 1.087290629417145382 ) ) ;
#78461 = CARTESIAN_POINT ( 'NONE',  ( -0.1998031496062991907, -0.3460692066303959757, -2.585301837270341352 ) ) ;
#78462 = CARTESIAN_POINT ( 'NONE',  ( -0.3917322834645670104, -0.1049643490035307020, -1.302512754102049142 ) ) ;
#78463 = CARTESIAN_POINT ( 'NONE',  ( 1.397637795275591177, 0.1660481256975883668, -0.3530559997133364547 ) ) ;
#78464 = CARTESIAN_POINT ( 'NONE',  ( 0.5314960629921264834, 0.1660481256975883668, -0.3530559997133364547 ) ) ;
#78465 = CARTESIAN_POINT ( 'NONE',  ( 0.2165354330708668673, 0.1660481256975883668, -0.3530559997133364547 ) ) ;
#78466 = CARTESIAN_POINT ( 'NONE',  ( 1.397637795275591177, -0.5400638737290844871, 0.3530559997133364547 ) ) ;
#78467 = CARTESIAN_POINT ( 'NONE',  ( 0.7414698162729663755, 0.2952755905511811885, 0.1292274648535926551 ) ) ;
#78468 = CARTESIAN_POINT ( 'NONE',  ( 0.1049643490035303689, 0.3917322834645670104, -0.3930446194225722945 ) ) ;
#78469 = CARTESIAN_POINT ( 'NONE',  ( 0.2493438320209980519, -0.4281496062992127816, -0.4176697321401328100 ) ) ;
#78470 = CARTESIAN_POINT ( 'NONE',  ( 1.200787401574803681, 0.1660481256975885056, 0.3530559997133364547 ) ) ;
#78471 = CARTESIAN_POINT ( 'NONE',  ( 0.2755905511811031494, 0.2952755905511811885, 0.000000000000000000 ) ) ;
#78472 = AXIS2_PLACEMENT_3D ( 'NONE', #76128, #56339, #25173 ) ;
#78473 = CARTESIAN_POINT ( 'NONE',  ( 1.338582677165355062, -0.1870078740157479769, 0.3641732283464567677 ) ) ;
#78474 = CARTESIAN_POINT ( 'NONE',  ( -1.417322834645668772, -0.1870078740157479769, 0.4822834645669291653 ) ) ;
#78475 = CARTESIAN_POINT ( 'NONE',  ( -1.259842519685038686, -0.1870078740157479769, 0.4822834645669291653 ) ) ;
#78476 = CARTESIAN_POINT ( 'NONE',  ( 0.7939632545931766261, -0.05778040916215522460, 0.4822834645669289988 ) ) ;
#78477 = CARTESIAN_POINT ( 'NONE',  ( -0.08989863708912321227, -0.3814249188617225839, -1.929133858267717105 ) ) ;
#78478 = CARTESIAN_POINT ( 'NONE',  ( 0.3917322834645670104, -0.1049643490035303411, -1.835958005249343827 ) ) ;
#78479 = ORIENTED_EDGE ( 'NONE', *, *, #38792, .T. ) ;
#78480 = CARTESIAN_POINT ( 'NONE',  ( -0.1998031496062991907, -0.3460692066303959757, -0.5380577427821522374 ) ) ;
#78481 = ORIENTED_EDGE ( 'NONE', *, *, #3931, .T. ) ;
#78482 = CARTESIAN_POINT ( 'NONE',  ( 1.174540682414699111, -0.3162353388693405765, 0.4822834645669290543 ) ) ;
#78483 = CARTESIAN_POINT ( 'NONE',  ( 0.8005249343832027131, -0.004921259842519576551, 0.3153832671262227771 ) ) ;
#78484 = CARTESIAN_POINT ( 'NONE',  ( -0.5314960629921122726, 2.755905511811024056, -3.937007874015763687 ) ) ;
#78485 = B_SPLINE_CURVE_WITH_KNOTS ( 'NONE', 3,
 ( #63606, #62791, #11450, #56864 ),
 .UNSPECIFIED., .F., .F.,
 ( 4, 4 ),
 ( 2.687447247556935660E-15, 0.002136818956430557546 ),
 .UNSPECIFIED. ) ;
#78486 = CARTESIAN_POINT ( 'NONE',  ( 0.000000000000000000, 0.000000000000000000, -0.3129921259842520787 ) ) ;
#78487 = CARTESIAN_POINT ( 'NONE',  ( -0.2362204724409447953, -0.4091458600556404646, -1.167979002624671914 ) ) ;
#78488 = CARTESIAN_POINT ( 'NONE',  ( -0.3917322834645670104, -7.196005306013484475E-17, -0.7539370078740157410 ) ) ;
#78489 = AXIS2_PLACEMENT_3D ( 'NONE', #8384, #66046, #41196 ) ;
#78490 = CARTESIAN_POINT ( 'NONE',  ( 1.410761154855643795, -0.3162353388693405765, 0.4822834645669290543 ) ) ;
#78491 = PLANE ( 'NONE',  #26461 ) ;
#78492 = CARTESIAN_POINT ( 'NONE',  ( -0.3346456692913377662, -0.5400638737290844871, 0.3530559997133364547 ) ) ;
#78493 = CARTESIAN_POINT ( 'NONE',  ( 0.9514435695538062676, -0.05778040916215522460, 0.4822834645669289988 ) ) ;
#78494 = VERTEX_POINT ( 'NONE', #2441 ) ;
#78495 = CARTESIAN_POINT ( 'NONE',  ( -1.568241469816272105, -0.05778040916215522460, 0.4822834645669289988 ) ) ;
#78496 = CARTESIAN_POINT ( 'NONE',  ( 1.348312163386739426, 0.2929341459200028863, 0.8371118098809627872 ) ) ;
#78497 = DIRECTION ( 'NONE',  ( 1.047444401652940007E-14, -6.123233995736767268E-17, -1.000000000000000000 ) ) ;
#78498 = CARTESIAN_POINT ( 'NONE',  ( -1.614173228346457378, 0.7794589730111968207, -0.1372047244094477536 ) ) ;
#78499 = CARTESIAN_POINT ( 'NONE',  ( -0.3038629456265427575, -2.551093532135090261E-15, 0.3954974714151479609 ) ) ;
#78500 = CARTESIAN_POINT ( 'NONE',  ( -1.017060367454067249, -0.08942795157527998196, 0.3641732283464567121 ) ) ;
#78501 = EDGE_CURVE ( 'NONE', #56774, #10845, #81609, .T. ) ;
#78502 = CARTESIAN_POINT ( 'NONE',  ( 0.8785612751854029456, 3.421639014772782816E-16, 0.3464511005275203726 ) ) ;
#78503 = CARTESIAN_POINT ( 'NONE',  ( 0.7480314960629927956, 0.2952755905511811885, 0.000000000000000000 ) ) ;
#78504 = EDGE_LOOP ( 'NONE', ( #57030, #78481, #62211, #50166, #28324 ) ) ;
#78506 = CARTESIAN_POINT ( 'NONE',  ( -0.4064735117398301512, 0.004960608223778500969, -0.3437734562760191848 ) ) ;
#78505 = LINE ( 'NONE', #13687, #1976 ) ;
#78507 = CARTESIAN_POINT ( 'NONE',  ( 0.7349081364829403995, 0.2306618581243848609, 0.2411417322834645549 ) ) ;
#78508 = CARTESIAN_POINT ( 'NONE',  ( 1.496062992125984703, -0.1870078740157480601, -0.3641732283464567677 ) ) ;
#78509 = CARTESIAN_POINT ( 'NONE',  ( 0.3917322834645669549, 2.398668435337827645E-17, -0.9855449886801030956 ) ) ;
#78510 = CARTESIAN_POINT ( 'NONE',  ( -0.7545931758530177724, 0.1771653543307087630, 0.09757992244046791164 ) ) ;
#78511 = CARTESIAN_POINT ( 'NONE',  ( -1.522309711286088607, -0.5023911411419708095, 0.1820866141732285504 ) ) ;
#78512 = CARTESIAN_POINT ( 'NONE',  ( -0.2362204724409451284, 0.4091458600556402425, -0.8005249343832020470 ) ) ;
#78513 = CARTESIAN_POINT ( 'NONE',  ( 0.4986876640419954376, 0.2306618581243848609, 0.2411417322834645549 ) ) ;
#78514 = CARTESIAN_POINT ( 'NONE',  ( -1.122047244094487306, 0.07958543189024071263, -0.2665933059059888421 ) ) ;
#78515 = CARTESIAN_POINT ( 'NONE',  ( -0.03280839895013062252, -0.5511811023622046335, 0.09757992244046803654 ) ) ;
#78516 = CARTESIAN_POINT ( 'NONE',  ( -0.3149606299212590610, -0.1870078740157479769, 0.4822834645669291653 ) ) ;
#78517 = CARTESIAN_POINT ( 'NONE',  ( -1.062992125984250968, -0.5511811023622047445, 6.969142054262312111E-17 ) ) ;
#78518 = CARTESIAN_POINT ( 'NONE',  ( 0.2867679344610366554, -0.2867679344610365999, -0.2526439876978496257 ) ) ;
#78519 = CARTESIAN_POINT ( 'NONE',  ( 0.5839895013123367340, -0.6692913385826773087, -0.1292274648535924053 ) ) ;
#78520 = DIRECTION ( 'NONE',  ( 0.000000000000000000, -1.000000000000000000, 0.000000000000000000 ) ) ;
#78521 = CARTESIAN_POINT ( 'NONE',  ( -0.1265901696524986964, -0.4724409448818899238, -1.566272965879265344 ) ) ;
#78522 = CARTESIAN_POINT ( 'NONE',  ( -0.9317585301837263412, 0.05413385826771666132, 0.4176697321401328100 ) ) ;
#78523 = CARTESIAN_POINT ( 'NONE',  ( -0.3018372703412066094, -0.004921259842519576551, 0.3153832671262227771 ) ) ;
#78524 = EDGE_CURVE ( 'NONE', #32475, #33739, #17149, .T. ) ;
#78525 = CARTESIAN_POINT ( 'NONE',  ( -1.437007874015747477, 0.1660481256975883668, -0.3530559997133364547 ) ) ;
#78526 = CARTESIAN_POINT ( 'NONE',  ( 0.8070866141732289112, -0.4536011799217368745, -0.2665933059059886201 ) ) ;
#78527 = CARTESIAN_POINT ( 'NONE',  ( -0.8727034120734901146, -0.08942795157528024563, -0.3641732283464568787 ) ) ;
#78528 = CARTESIAN_POINT ( 'NONE',  ( -1.227034120734907585, 0.2952755905511811885, 0.1292274648535926551 ) ) ;
#78529 = CARTESIAN_POINT ( 'NONE',  ( -1.062992125984250968, 0.2952755905511811885, 0.000000000000000000 ) ) ;
#78530 = CARTESIAN_POINT ( 'NONE',  ( 1.640419947506562393, -0.4281496062992124485, 0.4176697321401328655 ) ) ;
#78531 = CARTESIAN_POINT ( 'NONE',  ( 0.7874015748031503170, -0.1870078740157480601, -0.3641732283464567677 ) ) ;
#78532 = CIRCLE ( 'NONE', #42217, 0.009842519685039378616 ) ;
#78533 = CARTESIAN_POINT ( 'NONE',  ( 0.1968503937007881344, -0.6692913385826771977, 8.415575281601705876E-17 ) ) ;
#78534 = EDGE_CURVE ( 'NONE', #75751, #8617, #81529, .T. ) ;
#78535 = CARTESIAN_POINT ( 'NONE',  ( -1.574803149606298192, -0.1870078740157480879, -0.4822834645669291653 ) ) ;
#78536 = CARTESIAN_POINT ( 'NONE',  ( -1.574803149606298636, -0.1870078740157479769, 0.4822834645669291653 ) ) ;
#78537 = VERTEX_POINT ( 'NONE', #49516 ) ;
#78538 = CARTESIAN_POINT ( 'NONE',  ( 0.3460692066303959202, -0.1998031496062991630, -2.858923884514435798 ) ) ;
#78539 = CARTESIAN_POINT ( 'NONE',  ( -1.443569553805773564, 0.1283753931104746893, -0.1820866141732285504 ) ) ;
#78540 = CARTESIAN_POINT ( 'NONE',  ( -0.6233595800524928121, -0.3162353388693409650, -0.4822834645669289433 ) ) ;
#78541 = CARTESIAN_POINT ( 'NONE',  ( 0.8464566929133865436, 0.1660481256975883668, -0.3530559997133364547 ) ) ;
#78542 = CARTESIAN_POINT ( 'NONE',  ( -1.456692913385826182, -0.5511811023622047445, 6.969142054262312111E-17 ) ) ;
#78543 = CARTESIAN_POINT ( 'NONE',  ( 0.1998031496062992463, 0.3460692066303959202, -1.795931758530183719 ) ) ;
#78544 = CARTESIAN_POINT ( 'NONE',  ( -1.594488188976377563, -0.5400638737290844871, 0.3530559997133364547 ) ) ;
#78545 = CARTESIAN_POINT ( 'NONE',  ( 1.030183727034121421, -0.05778040916215522460, 0.4822834645669289988 ) ) ;
#78546 = CARTESIAN_POINT ( 'NONE',  ( 0.3543307086614181922, -0.6692913385826771977, 8.415575281601705876E-17 ) ) ;
#78547 = CARTESIAN_POINT ( 'NONE',  ( 1.364829396325459854, -0.6046776061558809534, -0.2411417322834644161 ) ) ;
#78548 = PLANE ( 'NONE',  #73530 ) ;
#78549 = CARTESIAN_POINT ( 'NONE',  ( -0.1070741851644051862, -0.3996062992125987146, -1.489501312335957950 ) ) ;
#78550 = VECTOR ( 'NONE', #7165, 39.37007874015748143 ) ;
#78551 = CARTESIAN_POINT ( 'NONE',  ( -0.3949938075777411628, 0.1058382717557497937, -0.8202099737532810853 ) ) ;
#78552 = DIRECTION ( 'NONE',  ( -0.000000000000000000, -1.000000000000000000, -0.000000000000000000 ) ) ;
#78553 = CARTESIAN_POINT ( 'NONE',  ( 0.3674540682414705883, 0.1283753931104746893, -0.1820866141732285504 ) ) ;
#78554 = CARTESIAN_POINT ( 'NONE',  ( 0.2165354330708668673, 0.1660481256975883668, -0.3530559997133364547 ) ) ;
#78555 = CARTESIAN_POINT ( 'NONE',  ( 1.358267716535433323, -0.5400638737290845981, -0.3530559997133363437 ) ) ;
#78556 = CARTESIAN_POINT ( 'NONE',  ( -0.3949938075777408852, -0.1058382717557502933, -1.540026246719160108 ) ) ;
#78557 = CARTESIAN_POINT ( 'NONE',  ( 0.3937007874015754361, -0.1870078740157479769, 0.3641732283464567677 ) ) ;
#78558 = CARTESIAN_POINT ( 'NONE',  ( -0.5446194225721777693, -0.05778040916215522460, 0.4822834645669289988 ) ) ;
#78559 = CARTESIAN_POINT ( 'NONE',  ( 1.496062992125984703, -0.1870078740157480879, -0.4822834645669291653 ) ) ;
#78560 = CARTESIAN_POINT ( 'NONE',  ( 0.4527559055118117182, 0.1660481256975883668, -0.3530559997133364547 ) ) ;
#78561 = CARTESIAN_POINT ( 'NONE',  ( -0.1265901696524993347, 0.4724409448818895907, -1.896325459317584894 ) ) ;
#78562 = CARTESIAN_POINT ( 'NONE',  ( 0.3089825338612027239, -0.2417350488526308905, -2.755905511811024944 ) ) ;
#78563 = ORIENTED_EDGE ( 'NONE', *, *, #18464, .T. ) ;
#78564 = VERTEX_POINT ( 'NONE', #55000 ) ;
#78565 = CARTESIAN_POINT ( 'NONE',  ( 1.535433070866142335, -0.5511811023622047445, 6.969142054262312111E-17 ) ) ;
#78567 = CARTESIAN_POINT ( 'NONE',  ( -1.174540682414697335, -0.05778040916215522460, 0.4822834645669289988 ) ) ;
#78566 = CARTESIAN_POINT ( 'NONE',  ( -1.010498687664041384, -0.004921259842519576551, 0.3153832671262227771 ) ) ;
#78568 = CARTESIAN_POINT ( 'NONE',  ( 0.1958661417322834497, 0.3392501089628018329, -2.429114542485877770 ) ) ;
#78569 = CARTESIAN_POINT ( 'NONE',  ( -0.3460692066303957537, -0.1998031496062994405, -2.806430446194225770 ) ) ;
#78570 = CARTESIAN_POINT ( 'NONE',  ( 1.482939632545932307, -0.4281496062992124485, 0.4176697321401328655 ) ) ;
#78571 = CARTESIAN_POINT ( 'NONE',  ( -1.272965879265091305, -0.4281496062992124485, 0.4176697321401328655 ) ) ;
#78572 = CARTESIAN_POINT ( 'NONE',  ( 0.5118110236220478892, 0.2952755905511811885, 0.000000000000000000 ) ) ;
#78573 = CARTESIAN_POINT ( 'NONE',  ( -1.167979002624671470, 0.05413385826771666132, 0.4176697321401328100 ) ) ;
#78574 = CARTESIAN_POINT ( 'NONE',  ( 0.3392501089628018329, -0.1958661417322834497, -2.862185408627609728 ) ) ;
#78575 = CARTESIAN_POINT ( 'NONE',  ( 0.6758530183727039509, 0.2952755905511810774, -0.1292274648535930714 ) ) ;
#78576 = CARTESIAN_POINT ( 'NONE',  ( -0.2867679344610365999, 0.2867679344610364889, -1.901574803149606252 ) ) ;
#78577 = CARTESIAN_POINT ( 'NONE',  ( -1.082677165354329896, -0.4536011799217368745, -0.2665933059059886201 ) ) ;
#78578 = EDGE_LOOP ( 'NONE', ( #69545, #68223, #37436, #67191 ) ) ;
#78579 = CARTESIAN_POINT ( 'NONE',  ( -0.3949938075777409963, -7.255918531996591613E-17, -2.086614173228346303 ) ) ;
#78580 = EDGE_LOOP ( 'NONE', ( #32075, #5686, #2467, #16021 ) ) ;
#78581 = CARTESIAN_POINT ( 'NONE',  ( -1.679790026246718693, 0.1283753931104746893, -0.1820866141732285504 ) ) ;
#78582 = CARTESIAN_POINT ( 'NONE',  ( -0.9645669291338575535, -0.5400638737290844871, 0.3530559997133364547 ) ) ;
#78583 = CARTESIAN_POINT ( 'NONE',  ( -1.312335958005248715, 0.2306618581243848609, 0.2411417322834645549 ) ) ;
#78584 = CARTESIAN_POINT ( 'NONE',  ( -0.3996062992125986035, -0.1070741851644056997, -0.5183727034120735322 ) ) ;
#78585 = CARTESIAN_POINT ( 'NONE',  ( -1.712598425196849572, 0.1660481256975885056, 0.3530559997133364547 ) ) ;
#78586 = CARTESIAN_POINT ( 'NONE',  ( -1.561679790026246017, 0.05413385826771666132, 0.4176697321401328100 ) ) ;
#78587 = CARTESIAN_POINT ( 'NONE',  ( -1.653543307086613234, -0.1870078740157479769, 0.4822834645669291653 ) ) ;
#78588 = DIRECTION ( 'NONE',  ( -1.000000000000000000, 0.000000000000000000, 0.000000000000000000 ) ) ;
#78589 = CYLINDRICAL_SURFACE ( 'NONE', #46916, 0.4744094488188972947 ) ;
#78590 = CARTESIAN_POINT ( 'NONE',  ( 0.09186351706036827158, -0.004921259842519576551, 0.3153832671262227771 ) ) ;
#78591 = CARTESIAN_POINT ( 'NONE',  ( 0.5314960629921396951, 2.755905511811024056, -3.937007874015760578 ) ) ;
#78592 = CARTESIAN_POINT ( 'NONE',  ( 0.3392501089628018329, 0.1958661417322835607, -0.2158792650918636147 ) ) ;
#78593 = CARTESIAN_POINT ( 'NONE',  ( -0.9776902887139098386, -0.5511811023622046335, 0.09757992244046803654 ) ) ;
#78594 = VECTOR ( 'NONE', #73819, 39.37007874015748143 ) ;
#78595 = CARTESIAN_POINT ( 'NONE',  ( -0.5905511811023613777, -0.6692913385826771977, 8.415575281601705876E-17 ) ) ;
#78596 = CARTESIAN_POINT ( 'NONE',  ( 0.9711286089238851948, 0.2306618581243848609, 0.2411417322834645549 ) ) ;
#78597 = CARTESIAN_POINT ( 'NONE',  ( -0.8202099737532799750, 0.2952755905511810774, -0.1292274648535930714 ) ) ;
#78598 = EDGE_LOOP ( 'NONE', ( #49215, #49233, #41279, #9723 ) ) ;
#78599 = VERTEX_POINT ( 'NONE', #18375 ) ;
#78600 = CARTESIAN_POINT ( 'NONE',  ( -1.010498687664041384, 0.05413385826771666132, 0.4176697321401328100 ) ) ;
#78601 = CARTESIAN_POINT ( 'NONE',  ( 0.7086614173228352742, -0.1870078740157480879, -0.4822834645669291653 ) ) ;
#78602 = CARTESIAN_POINT ( 'NONE',  ( -1.456692913385826182, -0.5511811023622047445, 6.969142054262312111E-17 ) ) ;
#78603 = CARTESIAN_POINT ( 'NONE',  ( -1.673228346456691717, 0.1660481256975883668, -0.3530559997133364547 ) ) ;
#78604 = CARTESIAN_POINT ( 'NONE',  ( -0.1265901696524993347, 0.4724409448818895907, -1.266404199475065440 ) ) ;
#78605 = CARTESIAN_POINT ( 'NONE',  ( -2.170146923806675510, 1.537401574803149984, 0.4744094488188970171 ) ) ;
#78606 = CARTESIAN_POINT ( 'NONE',  ( -0.3392501089628017219, -0.1958661417322836718, -0.3595800524934382736 ) ) ;
#78607 = CARTESIAN_POINT ( 'NONE',  ( 0.3392501089628018884, -0.1958661417322834220, -2.236876640419947826 ) ) ;
#78608 = CARTESIAN_POINT ( 'NONE',  ( -0.4527559055118102749, -0.5400638737290845981, -0.3530559997133363437 ) ) ;
#78609 = CARTESIAN_POINT ( 'NONE',  ( -1.541994750656167090, -0.5511811023622048555, -0.09757992244046775898 ) ) ;
#78610 = CARTESIAN_POINT ( 'NONE',  ( 0.3996062992125985480, 2.446882876249141654E-17, -0.1948818897637795700 ) ) ;
#78612 = CYLINDRICAL_SURFACE ( 'NONE', #59988, 1.122047244094488194 ) ;
#78611 = CARTESIAN_POINT ( 'NONE',  ( -1.266404199475064773, -0.3162353388693405765, 0.4822834645669290543 ) ) ;
#78613 = CARTESIAN_POINT ( 'NONE',  ( -1.489501312335957062, -0.3162353388693409650, -0.4822834645669289433 ) ) ;
#78614 = CARTESIAN_POINT ( 'NONE',  ( -0.3215223097112853146, -0.3162353388693405765, 0.4822834645669290543 ) ) ;
#78615 = CIRCLE ( 'NONE', #61105, 2.401574803149606474 ) ;
#78616 = CARTESIAN_POINT ( 'NONE',  ( 0.3420746716998660508, -0.1974969037888704149, -2.858923884514436242 ) ) ;
#78617 = CARTESIAN_POINT ( 'NONE',  ( 0.4265091863517067039, -0.5511811023622048555, -0.09757992244046775898 ) ) ;
#78618 = FACE_OUTER_BOUND ( 'NONE', #79019, .T. ) ;
#78619 = CARTESIAN_POINT ( 'NONE',  ( 0.3608923884514443348, -0.5511811023622046335, 0.09757992244046803654 ) ) ;
#78620 = CARTESIAN_POINT ( 'NONE',  ( 1.456692913385827515, 0.1771653543307087630, 0.000000000000000000 ) ) ;
#78621 = CARTESIAN_POINT ( 'NONE',  ( 0.8595800524934390507, -0.05778040916215560624, -0.4822834645669293319 ) ) ;
#78622 = CARTESIAN_POINT ( 'NONE',  ( 0.01968503937007957949, -0.4536011799217368745, -0.2665933059059886201 ) ) ;
#78623 = CARTESIAN_POINT ( 'NONE',  ( 0.3392501089628018329, 0.1958661417322835607, -2.013123359580052618 ) ) ;
#78624 = CARTESIAN_POINT ( 'NONE',  ( -1.286089238845143479, 0.2306618581243847221, -0.2411417322834647770 ) ) ;
#78625 = CARTESIAN_POINT ( 'NONE',  ( 0.05249343832021075018, 0.1283753931104746893, -0.1820866141732285504 ) ) ;
#78626 = CARTESIAN_POINT ( 'NONE',  ( -0.4091458600556402980, -0.2362204724409451284, -0.2867454068241469534 ) ) ;
#78627 = CARTESIAN_POINT ( 'NONE',  ( -0.4593175853018364174, -0.3690944881889765550, -0.3153832671262227771 ) ) ;
#78628 = FACE_OUTER_BOUND ( 'NONE', #28226, .T. ) ;
#78629 = EDGE_CURVE ( 'NONE', #51714, #11621, #82346, .T. ) ;
#78630 = CARTESIAN_POINT ( 'NONE',  ( -0.03937007874015669567, 0.2952755905511811885, 0.000000000000000000 ) ) ;
#78631 = DIRECTION ( 'NONE',  ( 0.000000000000000000, 0.000000000000000000, -1.000000000000000000 ) ) ;
#78632 = CARTESIAN_POINT ( 'NONE',  ( 0.6364829396325465405, -0.08942795157527998196, 0.3641732283464567121 ) ) ;
#78633 = CARTESIAN_POINT ( 'NONE',  ( -0.1640419947506555343, -0.2845877964562159024, 0.3641732283464567677 ) ) ;
#78634 = CARTESIAN_POINT ( 'NONE',  ( -0.3083989501312330295, -0.3162353388693409650, -0.4822834645669289433 ) ) ;
#78635 = DIRECTION ( 'NONE',  ( 0.000000000000000000, 0.000000000000000000, 1.000000000000000000 ) ) ;
#78636 = CARTESIAN_POINT ( 'NONE',  ( -1.318897637795274802, 0.07958543189024085140, 0.2665933059059887866 ) ) ;
#78637 = CARTESIAN_POINT ( 'NONE',  ( 0.4709442531824356015, 0.03757601356358733491, -1.929133858267717549 ) ) ;
#78638 = CARTESIAN_POINT ( 'NONE',  ( 0.5314960629921267055, -0.5400638737290844871, 0.3530559997133364547 ) ) ;
#78639 = CARTESIAN_POINT ( 'NONE',  ( -0.9973753280839886548, 0.2306618581243848609, 0.2411417322834645549 ) ) ;
#78640 = CARTESIAN_POINT ( 'NONE',  ( 0.1998031496062994128, -0.3460692066303957537, -1.585958005249344049 ) ) ;
#78641 = CARTESIAN_POINT ( 'NONE',  ( -0.3392501089628017219, -0.1958661417322836718, -2.499343832020997080 ) ) ;
#78642 = CARTESIAN_POINT ( 'NONE',  ( 0.3805774278215230400, -0.004921259842519870586, -0.3153832671262229437 ) ) ;
#78643 = CARTESIAN_POINT ( 'NONE',  ( -1.312335958005248715, 0.2306618581243848609, 0.2411417322834645549 ) ) ;
#78644 = CARTESIAN_POINT ( 'NONE',  ( -1.115485564304461219, -0.004921259842519870586, -0.3153832671262229437 ) ) ;
#78645 = CARTESIAN_POINT ( 'NONE',  ( 1.692913385826772421, 0.2952755905511811885, 0.000000000000000000 ) ) ;
#78646 = B_SPLINE_CURVE_WITH_KNOTS ( 'NONE', 3,
 ( #17606, #4964, #23485, #30631, #56296, #81993, #24307, #49977 ),
 .UNSPECIFIED., .F., .F.,
 ( 4, 2, 2, 4 ),
 ( 0.01399351151594419376, 0.01520974288759853639, 0.01642597425925287902, 0.01885843700256156080 ),
 .UNSPECIFIED. ) ;
#78647 = CARTESIAN_POINT ( 'NONE',  ( -0.9251968503937002541, -0.4536011799217368745, -0.2665933059059886201 ) ) ;
#78648 = CARTESIAN_POINT ( 'NONE',  ( 0.000000000000000000, 0.000000000000000000, -2.755905511811024056 ) ) ;
#78649 = CARTESIAN_POINT ( 'NONE',  ( 0.9448818897637802916, -0.1870078740157479769, 0.4822834645669291653 ) ) ;
#78650 = CARTESIAN_POINT ( 'NONE',  ( -0.3460692066303958092, -0.1998031496062994683, -0.05249343832020997996 ) ) ;
#78651 = CARTESIAN_POINT ( 'NONE',  ( 0.1958661417322834775, 0.3392501089628018884, -2.345819840716222515 ) ) ;
#78652 = CARTESIAN_POINT ( 'NONE',  ( -0.3949938075777409408, -0.1058382717557502933, -0.6758530183727035068 ) ) ;
#78653 = DIRECTION ( 'NONE',  ( -0.000000000000000000, -1.000000000000000000, -0.000000000000000000 ) ) ;
#78654 = CARTESIAN_POINT ( 'NONE',  ( -1.712598425196849572, 0.1660481256975885056, 0.3530559997133364547 ) ) ;
#78655 = CARTESIAN_POINT ( 'NONE',  ( -1.108923884514435132, -0.3162353388693405765, 0.4822834645669290543 ) ) ;
#78656 = CARTESIAN_POINT ( 'NONE',  ( 1.207349081364829990, -0.6046776061558809534, -0.2411417322834644161 ) ) ;
#78657 = CARTESIAN_POINT ( 'NONE',  ( -0.1049643490035302024, -0.3917322834645671215, -2.204068241469816503 ) ) ;
#78658 = CARTESIAN_POINT ( 'NONE',  ( 1.561679790026247350, -0.004921259842519870586, -0.3153832671262229437 ) ) ;
#78659 = CARTESIAN_POINT ( 'NONE',  ( 0.3608923884514443348, -0.6692913385826771977, 0.1292274648535927661 ) ) ;
#78660 = CARTESIAN_POINT ( 'NONE',  ( -0.2624671916010490880, -0.6046776061558807314, 0.2411417322834647770 ) ) ;
#78661 = CARTESIAN_POINT ( 'NONE',  ( 1.555118110236221041, 0.1660481256975883668, -0.3530559997133364547 ) ) ;
#78662 = CARTESIAN_POINT ( 'NONE',  ( -0.3460692066303958092, -0.1998031496062994683, -2.099737532808398921 ) ) ;
#78663 = CARTESIAN_POINT ( 'NONE',  ( 0.5839895013123367340, -0.5511811023622048555, -0.09757992244046775898 ) ) ;
#78664 = CARTESIAN_POINT ( 'NONE',  ( -0.1998031496062991907, -0.3460692066303959757, -1.797900262467191590 ) ) ;
#78665 = EDGE_LOOP ( 'NONE', ( #62800, #5463, #75475, #20050 ) ) ;
#78667 = CARTESIAN_POINT ( 'NONE',  ( -0.1958661417322836995, 0.3392501089628017219, -0.3248224653881383595 ) ) ;
#78666 = VECTOR ( 'NONE', #52021, 39.37007874015748143 ) ;
#78668 = ORIENTED_EDGE ( 'NONE', *, *, #33231, .F. ) ;
#78669 = CARTESIAN_POINT ( 'NONE',  ( 0.1246719160104994284, -0.6692913385826771977, 0.1292274648535927661 ) ) ;
#78670 = CARTESIAN_POINT ( 'NONE',  ( 1.220472440944882386, -0.6692913385826771977, 8.415575281601705876E-17 ) ) ;
#78671 = CARTESIAN_POINT ( 'NONE',  ( 0.2624671916010504757, 0.2306618581243848609, 0.2411417322834645549 ) ) ;
#78672 = CARTESIAN_POINT ( 'NONE',  ( -0.5708661417322825615, -0.4536011799217367080, 0.2665933059059888421 ) ) ;
#78673 = CARTESIAN_POINT ( 'NONE',  ( 1.200787401574803681, 0.1660481256975885056, 0.3530559997133364547 ) ) ;
#78674 = CARTESIAN_POINT ( 'NONE',  ( -0.3018372703412066094, -0.4281496062992127816, -0.4176697321401328100 ) ) ;
#78675 = CARTESIAN_POINT ( 'NONE',  ( 0.1049868766404206816, -0.6046776061558809534, -0.2411417322834644161 ) ) ;
#78676 = CARTESIAN_POINT ( 'NONE',  ( -1.640419947506561060, 0.05413385826771666132, 0.4176697321401328100 ) ) ;
#78677 = CARTESIAN_POINT ( 'NONE',  ( 1.030183727034121421, -0.3162353388693409650, -0.4822834645669289433 ) ) ;
#78678 = CARTESIAN_POINT ( 'NONE',  ( 1.135170603674541256, -0.6692913385826773087, -0.1292274648535924053 ) ) ;
#78679 = CARTESIAN_POINT ( 'NONE',  ( 0.1049643490035303689, 0.3917322834645670104, -0.7729658792650916377 ) ) ;
#78680 = CARTESIAN_POINT ( 'NONE',  ( 0.5905511811023629321, 0.1771653543307087630, 0.000000000000000000 ) ) ;
#78681 = ORIENTED_EDGE ( 'NONE', *, *, #1687, .T. ) ;
#78682 = CARTESIAN_POINT ( 'NONE',  ( -0.3420746716998659953, -0.1974969037888706647, -0.6824146981627297048 ) ) ;
#78683 = ORIENTED_EDGE ( 'NONE', *, *, #41951, .F. ) ;
#78684 = CARTESIAN_POINT ( 'NONE',  ( -0.2821522309711278487, 0.1771653543307087630, 0.09757992244046791164 ) ) ;
#78685 = CARTESIAN_POINT ( 'NONE',  ( 0.1181102362204730916, 0.2952755905511811885, 0.000000000000000000 ) ) ;
#78686 = CARTESIAN_POINT ( 'NONE',  ( -1.456124044357799185, 1.149361882009420466, 0.2731108461632001383 ) ) ;
#78687 = CARTESIAN_POINT ( 'NONE',  ( -0.2427821522309703550, -0.05778040916215560624, -0.4822834645669293319 ) ) ;
#78688 = CARTESIAN_POINT ( 'NONE',  ( -0.2887139107611542133, 0.2306618581243848609, 0.2411417322834645549 ) ) ;
#78689 = CARTESIAN_POINT ( 'NONE',  ( -0.8070866141732276899, 0.1660481256975883668, -0.3530559997133364547 ) ) ;
#78690 = CARTESIAN_POINT ( 'NONE',  ( -1.167979002624671470, -0.4281496062992127816, -0.4176697321401328100 ) ) ;
#78691 = CARTESIAN_POINT ( 'NONE',  ( 1.154855643044620184, -0.5023911411419708095, 0.1820866141732285504 ) ) ;
#78692 = LINE ( 'NONE', #21015, #907 ) ;
#78693 = CARTESIAN_POINT ( 'NONE',  ( 0.1148797229700118799, 1.057468328962668069, 0.2688218391471720037 ) ) ;
#78694 = CARTESIAN_POINT ( 'NONE',  ( 0.7808398950131240079, -0.2845877964562159024, 0.3641732283464567677 ) ) ;
#78695 = CARTESIAN_POINT ( 'NONE',  ( 0.4855643044619430415, -0.4281496062992127816, -0.4176697321401328100 ) ) ;
#78696 = CARTESIAN_POINT ( 'NONE',  ( 0.3871391076115493490, -0.3162353388693405765, 0.4822834645669290543 ) ) ;
#78697 = CARTESIAN_POINT ( 'NONE',  ( 0.3996062992125986035, 2.446882876249141962E-17, -1.220472440944881942 ) ) ;
#78698 = CARTESIAN_POINT ( 'NONE',  ( -1.607611548556429737, -0.6692913385826771977, 0.1292274648535927661 ) ) ;
#78699 = CARTESIAN_POINT ( 'NONE',  ( -0.3996062992125984925, -0.1070741851644056858, -0.7526246719160103460 ) ) ;
#78700 = CARTESIAN_POINT ( 'NONE',  ( -0.1070741851644056997, 0.3996062992125984925, -0.7132545931758530466 ) ) ;
#78701 = CARTESIAN_POINT ( 'NONE',  ( -0.3740157480314953431, -0.5400638737290845981, -0.3530559997133363437 ) ) ;
#78702 = CARTESIAN_POINT ( 'NONE',  ( -0.3458507752293906723, -0.3458507752293910609, -0.05905511811023620578 ) ) ;
#78703 = CARTESIAN_POINT ( 'NONE',  ( -0.1958661417322834220, -0.3392501089628018884, -2.040026246719160330 ) ) ;
#78704 = CARTESIAN_POINT ( 'NONE',  ( -1.345144356955379816, -0.2845877964562159024, 0.3641732283464567677 ) ) ;
#78705 = CARTESIAN_POINT ( 'NONE',  ( 0.9776902887139113929, 0.2952755905511811885, 0.1292274648535926551 ) ) ;
#78706 = CARTESIAN_POINT ( 'NONE',  ( 0.9842519685039378130, -0.6692913385826771977, 8.415575281601705876E-17 ) ) ;
#78707 = CARTESIAN_POINT ( 'NONE',  ( -0.1574803149606292529, -0.1870078740157480601, -0.3641732283464567677 ) ) ;
#78708 = CARTESIAN_POINT ( 'NONE',  ( 0.4330708661417329575, -0.6692913385826771977, 8.415575281601705876E-17 ) ) ;
#78709 = CARTESIAN_POINT ( 'NONE',  ( 0.3458507752293908943, 0.3458507752293908943, -1.946850393700787274 ) ) ;
#78710 = CARTESIAN_POINT ( 'NONE',  ( -0.2755905511811015396, -0.5511811023622047445, 6.969142054262312111E-17 ) ) ;
#78711 = CARTESIAN_POINT ( 'NONE',  ( -0.1968503937007867743, -0.6692913385826771977, 8.415575281601705876E-17 ) ) ;
#78712 = CARTESIAN_POINT ( 'NONE',  ( 0.3420746716998660508, -0.1974969037888704149, -1.441601049868766804 ) ) ;
#78713 = CARTESIAN_POINT ( 'NONE',  ( -1.653543307086613234, -0.1870078740157480879, -0.4822834645669291653 ) ) ;
#78714 = CARTESIAN_POINT ( 'NONE',  ( 0.6692913385826777528, 0.1771653543307087630, 0.000000000000000000 ) ) ;
#78715 = CARTESIAN_POINT ( 'NONE',  ( 1.601049868766404982, -0.5023911411419708095, -0.1820866141732282451 ) ) ;
#78716 = CARTESIAN_POINT ( 'NONE',  ( -0.6692913385826764205, -0.6692913385826771977, 8.415575281601705876E-17 ) ) ;
#78717 = CARTESIAN_POINT ( 'NONE',  ( -0.7677165354330699465, -0.4536011799217368745, -0.2665933059059886201 ) ) ;
#78718 = CARTESIAN_POINT ( 'NONE',  ( -0.5314960629921350321, 2.755905511811024056, 2.583694225513478937 ) ) ;
#78719 = CARTESIAN_POINT ( 'NONE',  ( -0.6824146981627291497, -0.6046776061558809534, -0.2411417322834644161 ) ) ;
#78720 = CARTESIAN_POINT ( 'NONE',  ( -0.5839895013123351797, -0.6692913385826771977, 0.1292274648535927661 ) ) ;
#78721 = CARTESIAN_POINT ( 'NONE',  ( -0.1443569553805765515, -0.4281496062992127816, -0.4176697321401328100 ) ) ;
#78722 = CARTESIAN_POINT ( 'NONE',  ( 0.3460692066303958092, 0.1998031496062993018, -2.727690288713910949 ) ) ;
#78723 = EDGE_CURVE ( 'NONE', #21899, #40183, #24977, .T. ) ;
#78724 = CARTESIAN_POINT ( 'NONE',  ( -0.3392501089628018329, -0.1958661417322836440, -1.864810080543620074 ) ) ;
#78725 = VECTOR ( 'NONE', #64374, 39.37007874015748143 ) ;
#78726 = CARTESIAN_POINT ( 'NONE',  ( -0.5314960629921123836, 2.697625129285034173, -3.898413161119333115 ) ) ;
#78727 = CARTESIAN_POINT ( 'NONE',  ( 0.8202099737532814183, -0.5511811023622048555, -0.09757992244046775898 ) ) ;
#78728 = CARTESIAN_POINT ( 'NONE',  ( 1.227034120734908917, -0.6692913385826771977, 0.1292274648535927661 ) ) ;
#78729 = CARTESIAN_POINT ( 'NONE',  ( -1.358267716535432434, 0.07958543189024071263, -0.2665933059059888421 ) ) ;
#78730 = CARTESIAN_POINT ( 'NONE',  ( -1.023622047244094002, -0.1870078740157480601, -0.3641732283464567677 ) ) ;
#78731 = ADVANCED_FACE ( 'NONE', ( #56244 ), #62608, .F. ) ;
#78732 = CARTESIAN_POINT ( 'NONE',  ( -0.5511811023622041894, -0.1870078740157480879, -0.4822834645669291653 ) ) ;
#78733 = CARTESIAN_POINT ( 'NONE',  ( 0.6889763779527566800, -0.4536011799217367080, 0.2665933059059888421 ) ) ;
#78734 = CARTESIAN_POINT ( 'NONE',  ( 0.4724409448818880919, 0.1265901696525020825, -2.329396325459317740 ) ) ;
#78735 = CARTESIAN_POINT ( 'NONE',  ( 1.141732283464567566, 0.1771653543307087630, 0.000000000000000000 ) ) ;
#78736 = CARTESIAN_POINT ( 'NONE',  ( 0.3871391076115493490, -0.3162353388693405765, 0.4822834645669290543 ) ) ;
#78737 = DIRECTION ( 'NONE',  ( 0.000000000000000000, 0.000000000000000000, -1.000000000000000000 ) ) ;
#78738 = CARTESIAN_POINT ( 'NONE',  ( -0.6824146981627291497, -0.6046776061558809534, -0.2411417322834644161 ) ) ;
#78739 = CARTESIAN_POINT ( 'NONE',  ( -0.3917322834645671215, 0.1049643490035301469, -1.534776902887139194 ) ) ;
#78740 = CARTESIAN_POINT ( 'NONE',  ( -1.725721784776902190, -0.05778040916215522460, 0.4822834645669289988 ) ) ;
#78741 = CARTESIAN_POINT ( 'NONE',  ( 0.3608923884514443348, -0.6692913385826771977, 0.1292274648535927661 ) ) ;
#78742 = CARTESIAN_POINT ( 'NONE',  ( 0.1443569553805781891, 0.05413385826771626580, -0.4176697321401330321 ) ) ;
#78743 = CARTESIAN_POINT ( 'NONE',  ( -0.07874015748031421014, -0.1870078740157479769, 0.3641732283464567677 ) ) ;
#78744 = CARTESIAN_POINT ( 'NONE',  ( 0.000000000000000000, 0.000000000000000000, 0.000000000000000000 ) ) ;
#78745 = CARTESIAN_POINT ( 'NONE',  ( 0.05249343832021075018, -0.5023911411419708095, 0.1820866141732285504 ) ) ;
#78746 = CARTESIAN_POINT ( 'NONE',  ( 0.6824146981627303710, -0.6046776061558807314, 0.2411417322834647770 ) ) ;
#78747 = CARTESIAN_POINT ( 'NONE',  ( -0.8136482939632537770, -0.5023911411419708095, 0.1820866141732285504 ) ) ;
#78748 = CARTESIAN_POINT ( 'NONE',  ( -9.787531504996566615E-17, 0.3996062992125985480, -0.8641732283464567121 ) ) ;
#78749 = CARTESIAN_POINT ( 'NONE',  ( -1.089238845144356427, -0.4281496062992127816, -0.4176697321401328100 ) ) ;
#78750 = CARTESIAN_POINT ( 'NONE',  ( 0.1837270341207354329, 0.1539470093639523085, 0.1968503937007873850 ) ) ;
#78751 = EDGE_LOOP ( 'NONE', ( #81573, #12694, #48952, #35926 ) ) ;
#78752 = CARTESIAN_POINT ( 'NONE',  ( -1.187664041994749731, -0.3162353388693405765, 0.4822834645669290543 ) ) ;
#78753 = CARTESIAN_POINT ( 'NONE',  ( -1.154855643044618851, -0.5023911411419708095, -0.1820866141732282451 ) ) ;
#78754 = CARTESIAN_POINT ( 'NONE',  ( -0.1640419947506555343, -0.3162353388693405765, 0.4822834645669290543 ) ) ;
#78755 = CARTESIAN_POINT ( 'NONE',  ( -1.515748031496062076, 0.1660481256975883668, -0.3530559997133364547 ) ) ;
#78756 = CARTESIAN_POINT ( 'NONE',  ( -0.8923884514435688198, -0.6046776061558807314, 0.2411417322834647770 ) ) ;
#78757 = CARTESIAN_POINT ( 'NONE',  ( -0.1674892343164145203, -2.567464376874931580E-15, -0.4445507791589072832 ) ) ;
#78758 = CARTESIAN_POINT ( 'NONE',  ( 0.7611548556430451917, -0.6046776061558807314, 0.2411417322834647770 ) ) ;
#78759 = CARTESIAN_POINT ( 'NONE',  ( 0.8070866141732289112, -0.5400638737290845981, -0.3530559997133363437 ) ) ;
#78760 = CARTESIAN_POINT ( 'NONE',  ( -0.1958661417322836718, 0.3392501089628017219, -2.367454068241469756 ) ) ;
#78761 = CARTESIAN_POINT ( 'NONE',  ( 1.502624671916010790, -0.3162353388693409650, -0.4822834645669289433 ) ) ;
#78762 = AXIS2_PLACEMENT_3D ( 'NONE', #15362, #54888, #73434 ) ;
#78763 = CARTESIAN_POINT ( 'NONE',  ( -1.410761154855642463, -0.05778040916215522460, 0.4822834645669289988 ) ) ;
#78764 = CARTESIAN_POINT ( 'NONE',  ( -0.1998031496062994683, 0.3460692066303958092, -0.6430446194225721834 ) ) ;
#78765 = ORIENTED_EDGE ( 'NONE', *, *, #9399, .F. ) ;
#78766 = CARTESIAN_POINT ( 'NONE',  ( -0.4068241469816264999, -0.3690944881889763329, 0.3153832671262228327 ) ) ;
#78767 = CARTESIAN_POINT ( 'NONE',  ( -0.3917322834645670104, -7.196005306013484475E-17, -1.606299212598425452 ) ) ;
#78768 = ORIENTED_EDGE ( 'NONE', *, *, #48666, .T. ) ;
#78769 = CARTESIAN_POINT ( 'NONE',  ( 0.4527559055118117182, -0.5400638737290844871, 0.3530559997133364547 ) ) ;
#78770 = CARTESIAN_POINT ( 'NONE',  ( 0.03280839895013198948, 0.2952755905511811885, 0.1292274648535926551 ) ) ;
#78771 = CARTESIAN_POINT ( 'NONE',  ( -0.7086614173228339419, -0.1870078740157479769, 0.4822834645669291653 ) ) ;
#78772 = CARTESIAN_POINT ( 'NONE',  ( 1.384514435695538559, 0.2952755905511810774, -0.1292274648535930714 ) ) ;
#78773 = CARTESIAN_POINT ( 'NONE',  ( -0.8333333333333323711, 0.1771653543307087630, 0.09757992244046791164 ) ) ;
#78774 = CARTESIAN_POINT ( 'NONE',  ( 0.05172391896678928819, 1.065813321887014276, -1.498852247951555583 ) ) ;
#78775 = CARTESIAN_POINT ( 'NONE',  ( 0.6299212598425204535, -0.1870078740157480879, -0.4822834645669291653 ) ) ;
#78776 = CARTESIAN_POINT ( 'NONE',  ( 0.4724409448818904789, -0.1870078740157479769, 0.3641732283464567677 ) ) ;
#78777 = CARTESIAN_POINT ( 'NONE',  ( -0.4330708661417315697, -0.6692913385826771977, 8.415575281601705876E-17 ) ) ;
#78778 = CARTESIAN_POINT ( 'NONE',  ( 0.3917322834645669549, 2.398668435337827645E-17, -0.9855449886801030956 ) ) ;
#78779 = CARTESIAN_POINT ( 'NONE',  ( -0.9776902887139098386, 0.2952755905511810774, -0.1292274648535930714 ) ) ;
#78780 = CARTESIAN_POINT ( 'NONE',  ( 1.220472440944881942, 2.401574803149606474, -0.5309055118110238558 ) ) ;
#78781 = CARTESIAN_POINT ( 'NONE',  ( 1.404199475065617708, 0.05413385826771626580, -0.4176697321401330321 ) ) ;
#78782 = CARTESIAN_POINT ( 'NONE',  ( 1.620734908136483465, -0.5511811023622046335, 0.09757992244046803654 ) ) ;
#78783 = ORIENTED_EDGE ( 'NONE', *, *, #3893, .F. ) ;
#78784 = CARTESIAN_POINT ( 'NONE',  ( 0.3392501089628018884, -0.1958661417322833942, -2.306449761976065105 ) ) ;
#78785 = CARTESIAN_POINT ( 'NONE',  ( -0.03280839895013062252, 0.2952755905511810774, -0.1292274648535930714 ) ) ;
#78786 = ORIENTED_EDGE ( 'NONE', *, *, #79432, .F. ) ;
#78787 = AXIS2_PLACEMENT_3D ( 'NONE', #55675, #43045, #42228 ) ;
#78788 = CARTESIAN_POINT ( 'NONE',  ( -1.062992125984250968, 0.2952755905511811885, 0.000000000000000000 ) ) ;
#78789 = CARTESIAN_POINT ( 'NONE',  ( 1.135170603674541256, 0.2952755905511811885, 0.1292274648535926551 ) ) ;
#78790 = CARTESIAN_POINT ( 'NONE',  ( 1.246719160104987623, -0.4281496062992124485, 0.4176697321401328655 ) ) ;
#78791 = CARTESIAN_POINT ( 'NONE',  ( 0.2887139107611556010, -0.6046776061558807314, 0.2411417322834647770 ) ) ;
#78792 = ADVANCED_FACE ( 'NONE', ( #56868 ), #5537, .F. ) ;
#78793 = CARTESIAN_POINT ( 'NONE',  ( -0.3215223097112853146, -0.05778040916215560624, -0.4822834645669293319 ) ) ;
#78794 = CARTESIAN_POINT ( 'NONE',  ( -0.3392501089628019995, 0.1958661417322832277, -1.843175853018372834 ) ) ;
#78795 = CARTESIAN_POINT ( 'NONE',  ( -1.161417322834644716, -0.5400638737290845981, -0.3530559997133363437 ) ) ;
#78796 = CARTESIAN_POINT ( 'NONE',  ( -0.7086614173228339419, -0.1870078740157479769, 0.4822834645669291653 ) ) ;
#78797 = CARTESIAN_POINT ( 'NONE',  ( -0.6430446194225712953, -0.004921259842519870586, -0.3153832671262229437 ) ) ;
#78798 = CARTESIAN_POINT ( 'NONE',  ( -0.03178304480585582292, 0.3983403474834776858, -2.755905511811024500 ) ) ;
#78799 = CARTESIAN_POINT ( 'NONE',  ( -0.6824146981627291497, -0.6046776061558809534, -0.2411417322834644161 ) ) ;
#78800 = LINE ( 'NONE', #13989, #6327 ) ;
#78801 = CARTESIAN_POINT ( 'NONE',  ( 0.5708661417322841158, -0.5400638737290845981, -0.3530559997133363437 ) ) ;
#78802 = CARTESIAN_POINT ( 'NONE',  ( 0.3460692066303959202, 0.1998031496062993295, -2.020997375328084100 ) ) ;
#78803 = CARTESIAN_POINT ( 'NONE',  ( 3.933461957825151067, 1.093339152432855510, -0.1676739346958345533 ) ) ;
#78804 = CARTESIAN_POINT ( 'NONE',  ( -0.2952755905511803003, -0.5400638737290845981, -0.3530559997133363437 ) ) ;
#78806 = CARTESIAN_POINT ( 'NONE',  ( -0.8789144566217194088, 0.004960608223777852183, -0.3437734562760195733 ) ) ;
#78805 = CARTESIAN_POINT ( 'NONE',  ( 1.049868766404200349, 0.1283753931104748280, 0.1820866141732283561 ) ) ;
#78807 = CARTESIAN_POINT ( 'NONE',  ( -0.2362204724409447953, -0.4091458600556404646, -0.7723097112860892732 ) ) ;
#78808 = CARTESIAN_POINT ( 'NONE',  ( 1.161417322834646493, -0.4536011799217367080, 0.2665933059059888421 ) ) ;
#78809 = CARTESIAN_POINT ( 'NONE',  ( 1.095800524934383846, -0.3162353388693405765, 0.4822834645669290543 ) ) ;
#78810 = CARTESIAN_POINT ( 'NONE',  ( -0.1058382717557497660, -0.3949938075777411073, -0.1489501312335957950 ) ) ;
#78811 = CARTESIAN_POINT ( 'NONE',  ( 0.09842519685039434474, -0.5400638737290845981, -0.3530559997133363437 ) ) ;
#78812 = CARTESIAN_POINT ( 'NONE',  ( -1.574803149606298192, -0.1870078740157480879, -0.4822834645669291653 ) ) ;
#78813 = CARTESIAN_POINT ( 'NONE',  ( -1.515748031496062076, 0.1660481256975883668, -0.3530559997133364547 ) ) ;
#78814 = CARTESIAN_POINT ( 'NONE',  ( -0.2887139107611542133, 0.2306618581243848609, 0.2411417322834645549 ) ) ;
#78815 = CARTESIAN_POINT ( 'NONE',  ( 0.3949938075777409408, -0.1058382717557499186, -0.6607611548556431291 ) ) ;
#78816 = CARTESIAN_POINT ( 'NONE',  ( 1.266404199475066328, -0.3162353388693409650, -0.4822834645669289433 ) ) ;
#78817 = CARTESIAN_POINT ( 'NONE',  ( 0.5052493438320215802, 0.2952755905511811885, 0.1292274648535926551 ) ) ;
#78818 = CARTESIAN_POINT ( 'NONE',  ( 0.8070866141732289112, -0.4536011799217368745, -0.2665933059059886201 ) ) ;
#78819 = CARTESIAN_POINT ( 'NONE',  ( 0.2878949040089971434, 1.168214014193575956, 0.1242954387040235420 ) ) ;
#78820 = CARTESIAN_POINT ( 'NONE',  ( 0.3740157480314966754, -0.4536011799217367080, 0.2665933059059888421 ) ) ;
#78821 = DIRECTION ( 'NONE',  ( -0.000000000000000000, -1.000000000000000000, -0.000000000000000000 ) ) ;
#78822 = CARTESIAN_POINT ( 'NONE',  ( -0.1070741851644051862, -0.3996062992125986590, -1.251312335958005395 ) ) ;
#78823 = CARTESIAN_POINT ( 'NONE',  ( 0.8923884514435703741, 0.2306618581243848609, 0.2411417322834645549 ) ) ;
#78824 = AXIS2_PLACEMENT_3D ( 'NONE', #71448, #65973, #46174 ) ;
#78825 = CARTESIAN_POINT ( 'NONE',  ( -0.1958661417322836718, 0.3392501089628017219, -0.4776902887139107268 ) ) ;
#78826 = CIRCLE ( 'NONE', #42497, 1.122047244094488194 ) ;
#78828 = LINE ( 'NONE', #14443, #15733 ) ;
#78827 = CARTESIAN_POINT ( 'NONE',  ( 0.2230971128608932319, -0.4281496062992124485, 0.4176697321401328655 ) ) ;
#78829 = CARTESIAN_POINT ( 'NONE',  ( -0.1742125984251974291, -0.1742125984251974014, -0.3937007874015748254 ) ) ;
#78830 = CARTESIAN_POINT ( 'NONE',  ( 0.4527559055118117182, -0.4536011799217367080, 0.2665933059059888421 ) ) ;
#78831 = CARTESIAN_POINT ( 'NONE',  ( 0.3674540682414705883, -0.6046776061558807314, 0.2411417322834647770 ) ) ;
#78832 = CYLINDRICAL_SURFACE ( 'NONE', #82827, 0.2165354330708660624 ) ;
#78833 = CARTESIAN_POINT ( 'NONE',  ( -1.108923884514435132, -0.2845877964562159024, 0.3641732283464567677 ) ) ;
#78834 = CARTESIAN_POINT ( 'NONE',  ( -0.9973753280839886548, -0.6046776061558809534, -0.2411417322834644161 ) ) ;
#78835 = CARTESIAN_POINT ( 'NONE',  ( -1.377952755905511140, 0.2952755905511811885, 0.000000000000000000 ) ) ;
#78836 = CARTESIAN_POINT ( 'NONE',  ( 0.3477690288713918276, -0.6692913385826773087, -0.1292274648535924053 ) ) ;
#78837 = CARTESIAN_POINT ( 'NONE',  ( -1.581364829396324945, -0.08942795157528024563, -0.3641732283464568787 ) ) ;
#78838 = CARTESIAN_POINT ( 'NONE',  ( 1.047355619713164820, 1.286041797112411400, -0.4026416502575907441 ) ) ;
#78839 = CARTESIAN_POINT ( 'NONE',  ( 0.7217847769028878924, -0.4281496062992127816, -0.4176697321401328100 ) ) ;
#78840 = CARTESIAN_POINT ( 'NONE',  ( -0.4091458600556405756, 0.2362204724409446288, -2.780183727034120977 ) ) ;
#78841 = CARTESIAN_POINT ( 'NONE',  ( 0.4494576562008150700, 1.384774454230845109, 3.911270836792677841 ) ) ;
#78842 = CARTESIAN_POINT ( 'NONE',  ( 1.437007874015748810, -0.5400638737290845981, -0.3530559997133363437 ) ) ;
#78843 = CARTESIAN_POINT ( 'NONE',  ( -1.246719160104986512, -0.004921259842519576551, 0.3153832671262227771 ) ) ;
#78844 = CARTESIAN_POINT ( 'NONE',  ( 1.187664041994751285, -0.08942795157527998196, 0.3641732283464567121 ) ) ;
#78845 = CARTESIAN_POINT ( 'NONE',  ( -1.135170603674539924, 0.1771653543307087075, -0.09757992244046823083 ) ) ;
#78846 = CARTESIAN_POINT ( 'NONE',  ( -0.7677165354330699465, -0.4536011799217368745, -0.2665933059059886201 ) ) ;
#78847 = CARTESIAN_POINT ( 'NONE',  ( 1.555118110236221041, -0.5400638737290844871, 0.3530559997133364547 ) ) ;
#78848 = CARTESIAN_POINT ( 'NONE',  ( 0.6430446194225728496, -0.004921259842519576551, 0.3153832671262227771 ) ) ;
#78849 = CARTESIAN_POINT ( 'NONE',  ( 0.4790026246719168435, -0.3162353388693409650, -0.4822834645669289433 ) ) ;
#78850 = CARTESIAN_POINT ( 'NONE',  ( 1.141732283464567566, 0.2952755905511811885, 0.000000000000000000 ) ) ;
#78851 = CARTESIAN_POINT ( 'NONE',  ( -0.1377952755905504645, -0.5400638737290845981, -0.3530559997133363437 ) ) ;
#78852 = EDGE_CURVE ( 'NONE', #48126, #72870, #50256, .T. ) ;
#78853 = CARTESIAN_POINT ( 'NONE',  ( 0.1312335958005255154, -0.5023911411419708095, 0.1820866141732285504 ) ) ;
#78854 = CARTESIAN_POINT ( 'NONE',  ( 1.259842519685040019, -0.1870078740157479769, 0.4822834645669291653 ) ) ;
#78855 =( BOUNDED_CURVE ( )  B_SPLINE_CURVE ( 1, ( #41533, #23409 ),
 .UNSPECIFIED., .F., .F. ) 
 B_SPLINE_CURVE_WITH_KNOTS ( ( 2, 2 ),
 ( 0.000000000000000000, 0.002000000000000005246 ),
 .UNSPECIFIED. ) 
 CURVE ( )  GEOMETRIC_REPRESENTATION_ITEM ( )  RATIONAL_B_SPLINE_CURVE ( ( 0.9875488213027523443, 0.9875488213027523443 ) ) 
 REPRESENTATION_ITEM ( '' )  );
#78856 = CARTESIAN_POINT ( 'NONE',  ( -0.2034120734908128059, 0.2066929133858267931, 0.1054918080437490802 ) ) ;
#78857 = CARTESIAN_POINT ( 'NONE',  ( -0.7349081364829390672, 0.2306618581243847221, -0.2411417322834647770 ) ) ;
#78858 = CARTESIAN_POINT ( 'NONE',  ( -0.3996062992125985480, -0.1070741851644057135, -0.9908136482939633449 ) ) ;
#78859 = FACE_OUTER_BOUND ( 'NONE', #70785, .T. ) ;
#78860 = CARTESIAN_POINT ( 'NONE',  ( -1.003937007874014853, 0.1660481256975885056, 0.3530559997133364547 ) ) ;
#78861 = CARTESIAN_POINT ( 'NONE',  ( -0.05249343832020938322, -0.6046776061558809534, -0.2411417322834644161 ) ) ;
#78862 = CARTESIAN_POINT ( 'NONE',  ( 0.1070741851644053527, 0.3996062992125986590, -2.513123359580052174 ) ) ;
#78863 = CARTESIAN_POINT ( 'NONE',  ( 4.837279021331060870E-17, -0.3949938075777409963, -1.968503937007873850 ) ) ;
#78864 = CARTESIAN_POINT ( 'NONE',  ( -0.1049643490035302024, -0.3917322834645671215, -0.5367454068241469534 ) ) ;
#78865 = DIRECTION ( 'NONE',  ( -0.000000000000000000, -0.000000000000000000, 1.000000000000000000 ) ) ;
#78866 = CARTESIAN_POINT ( 'NONE',  ( -1.325459317585300889, -0.3690944881889765550, -0.3153832671262227771 ) ) ;
#78867 = CARTESIAN_POINT ( 'NONE',  ( -9.594673741351313045E-17, 0.3917322834645670104, -0.9370078740157480324 ) ) ;
#78868 = CARTESIAN_POINT ( 'NONE',  ( -1.601049868766403650, -0.6046776061558807314, 0.2411417322834647770 ) ) ;
#78869 = EDGE_CURVE ( 'NONE', #66965, #46125, #82539, .T. ) ;
#78870 = CARTESIAN_POINT ( 'NONE',  ( -9.594673741351310580E-17, 0.3917322834645669549, -0.08003317765648111648 ) ) ;
#78871 = CARTESIAN_POINT ( 'NONE',  ( 0.4199475065616805614, 0.2306618581243848609, 0.2411417322834645549 ) ) ;
#78872 = CARTESIAN_POINT ( 'NONE',  ( -0.4855643044619415427, -0.3690944881889763329, 0.3153832671262228327 ) ) ;
#78873 = ADVANCED_FACE ( 'NONE', ( #24882 ), #44231, .F. ) ;
#78874 = CARTESIAN_POINT ( 'NONE',  ( 0.6824146981627303710, 0.2306618581243847221, -0.2411417322834647770 ) ) ;
#78875 = CARTESIAN_POINT ( 'NONE',  ( 0.1771653543307093182, 0.1660481256975885056, 0.3530559997133364547 ) ) ;
#78876 = CARTESIAN_POINT ( 'NONE',  ( -0.2362204724409451284, 0.4091458600556402425, -0.08989501312335958227 ) ) ;
#78877 = VECTOR ( 'NONE', #12757, 39.37007874015748143 ) ;
#78878 = CARTESIAN_POINT ( 'NONE',  ( 0.3460692066303959202, 0.1998031496062993295, -2.493438320209973469 ) ) ;
#78879 = CARTESIAN_POINT ( 'NONE',  ( -0.1958661417322836995, 0.3392501089628017219, -1.112224040191287955 ) ) ;
#78880 = CARTESIAN_POINT ( 'NONE',  ( 1.082677165354331228, 0.1660481256975883668, -0.3530559997133364547 ) ) ;
#78881 = AXIS2_PLACEMENT_3D ( 'NONE', #78361, #20692, #73707 ) ;
#78882 = CONICAL_SURFACE ( 'NONE', #42566, 0.1978346456692914035, 0.8726646259971685415 ) ;
#78883 = CARTESIAN_POINT ( 'NONE',  ( 0.2362204724409456558, -0.1870078740157480879, -0.4822834645669291653 ) ) ;
#78884 = CARTESIAN_POINT ( 'NONE',  ( 1.535433070866142335, -0.6692913385826771977, 8.415575281601705876E-17 ) ) ;
#78885 = CARTESIAN_POINT ( 'NONE',  ( 1.095800524934383846, -0.05778040916215560624, -0.4822834645669293319 ) ) ;
#78886 = CARTESIAN_POINT ( 'NONE',  ( 4.797336870675656522E-17, -0.3917322834645670104, -0.4783464566929135353 ) ) ;
#78887 = CARTESIAN_POINT ( 'NONE',  ( 0.1115485564304467270, -0.6692913385826773087, -0.1292274648535924053 ) ) ;
#78888 = CARTESIAN_POINT ( 'NONE',  ( 0.8267716535433078384, -0.6692913385826771977, 8.415575281601705876E-17 ) ) ;
#78889 = CARTESIAN_POINT ( 'NONE',  ( 0.02624671916010564918, -0.6046776061558809534, -0.2411417322834644161 ) ) ;
#78890 = CARTESIAN_POINT ( 'NONE',  ( 0.5708661417322842269, 0.07958543189024085140, 0.2665933059059887866 ) ) ;
#78891 = CARTESIAN_POINT ( 'NONE',  ( -1.351706036745406347, 0.05413385826771626580, -0.4176697321401330321 ) ) ;
#78892 = CARTESIAN_POINT ( 'NONE',  ( -1.574803149606298636, -0.1870078740157479769, 0.4822834645669291653 ) ) ;
#78893 = CARTESIAN_POINT ( 'NONE',  ( 0.8267716535433077274, 0.2952755905511811885, 0.000000000000000000 ) ) ;
#78894 = CARTESIAN_POINT ( 'NONE',  ( -0.4091458600556405756, 0.2362204724409446288, -0.5754593175853018883 ) ) ;
#78895 = CARTESIAN_POINT ( 'NONE',  ( -9.594673741351313045E-17, 0.3917322834645670104, -1.881889763779527769 ) ) ;
#78896 = ORIENTED_EDGE ( 'NONE', *, *, #32173, .F. ) ;
#78897 = CARTESIAN_POINT ( 'NONE',  ( -0.1998031496062994683, 0.3460692066303958092, -0.3280839895013123453 ) ) ;
#78898 = ORIENTED_EDGE ( 'NONE', *, *, #50835, .T. ) ;
#78899 = CARTESIAN_POINT ( 'NONE',  ( 1.194225721784777594, 0.05413385826771666132, 0.4176697321401328100 ) ) ;
#78900 = CARTESIAN_POINT ( 'NONE',  ( 1.095800524934383846, -0.2845877964562159024, 0.3641732283464567677 ) ) ;
#78901 = FACE_OUTER_BOUND ( 'NONE', #68925, .T. ) ;
#78902 = DIRECTION ( 'NONE',  ( 0.000000000000000000, -1.000000000000000000, -0.000000000000000000 ) ) ;
#78903 = LINE ( 'NONE', #72573, #32440 ) ;
#78904 = CARTESIAN_POINT ( 'NONE',  ( 0.3917322834645670104, 2.398668435337828261E-17, -1.147637795275590733 ) ) ;
#78905 = CARTESIAN_POINT ( 'NONE',  ( 1.437007874015748810, 0.1660481256975885056, 0.3530559997133364547 ) ) ;
#78906 = CARTESIAN_POINT ( 'NONE',  ( -1.555118110236219930, -0.5400638737290845981, -0.3530559997133363437 ) ) ;
#78907 = CARTESIAN_POINT ( 'NONE',  ( -0.3740157480314953431, -0.5400638737290845981, -0.3530559997133363437 ) ) ;
#78908 = CARTESIAN_POINT ( 'NONE',  ( 0.9448818897637802916, -0.1870078740157479769, 0.4822834645669291653 ) ) ;
#78909 = VERTEX_POINT ( 'NONE', #70334 ) ;
#78910 = CARTESIAN_POINT ( 'NONE',  ( -1.633858267716534529, -0.5400638737290845981, -0.3530559997133363437 ) ) ;
#78911 = CARTESIAN_POINT ( 'NONE',  ( -1.087387972035418926, 1.151979311713951182, -0.2770360422623977525 ) ) ;
#78912 = CARTESIAN_POINT ( 'NONE',  ( 1.346647322158897486, 4.103338224919997224, 5.973313079581513918 ) ) ;
#78913 = CARTESIAN_POINT ( 'NONE',  ( 1.660104986876641320, -0.08942795157527998196, 0.3641732283464567121 ) ) ;
#78914 = DIRECTION ( 'NONE',  ( 1.000000000000000000, 0.000000000000000000, 0.000000000000000000 ) ) ;
#78915 = CARTESIAN_POINT ( 'NONE',  ( -0.8923884514435688198, -0.5023911411419708095, 0.1820866141732285504 ) ) ;
#78916 = CARTESIAN_POINT ( 'NONE',  ( -1.391076115485563314, -0.6046776061558809534, -0.2411417322834644161 ) ) ;
#78917 = CARTESIAN_POINT ( 'NONE',  ( 0.8070866141732289112, -0.5400638737290845981, -0.3530559997133363437 ) ) ;
#78918 = ORIENTED_EDGE ( 'NONE', *, *, #75903, .F. ) ;
#78920 = CARTESIAN_POINT ( 'NONE',  ( 0.5314960629920851831, 2.677165354330708791, 3.900966923095595451 ) ) ;
#78919 = CARTESIAN_POINT ( 'NONE',  ( 1.450131233595801428, -0.6692913385826773087, -0.1292274648535924053 ) ) ;
#78921 = CARTESIAN_POINT ( 'NONE',  ( -0.7217847769028863381, -0.004921259842519870586, -0.3153832671262229437 ) ) ;
#78922 = CARTESIAN_POINT ( 'NONE',  ( 0.7545931758530189937, 0.2952755905511810774, -0.1292274648535930714 ) ) ;
#78923 = CARTESIAN_POINT ( 'NONE',  ( -1.607611548556429737, -0.6692913385826771977, 0.1292274648535927661 ) ) ;
#78924 = CARTESIAN_POINT ( 'NONE',  ( -0.1049643490035306742, 0.3917322834645668994, -1.031476747210287037 ) ) ;
#78925 = CARTESIAN_POINT ( 'NONE',  ( -0.8595800524934373854, -0.2845877964562161244, -0.3641732283464567121 ) ) ;
#78926 = CARTESIAN_POINT ( 'NONE',  ( -1.646981627296586703, -0.08942795157527998196, 0.3641732283464567121 ) ) ;
#78927 = DIRECTION ( 'NONE',  ( -1.000000000000000000, -3.096699300667737464E-16, 1.692413147294446216E-16 ) ) ;
#78928 = CARTESIAN_POINT ( 'NONE',  ( 0.6167979002624678353, -0.4281496062992124485, 0.4176697321401328655 ) ) ;
#78929 = CARTESIAN_POINT ( 'NONE',  ( -0.8267716535433065062, 0.1771653543307087630, 0.000000000000000000 ) ) ;
#78930 = CARTESIAN_POINT ( 'NONE',  ( -0.3937007874015740483, -0.1870078740157480601, -0.3641732283464567677 ) ) ;
#78931 = CARTESIAN_POINT ( 'NONE',  ( -0.2690288713910754526, 0.2952755905511810774, -0.1292274648535930714 ) ) ;
#78932 = CARTESIAN_POINT ( 'NONE',  ( 1.627296587926509996, -0.6046776061558807314, 0.2411417322834647770 ) ) ;
#78933 = CARTESIAN_POINT ( 'NONE',  ( -0.3917322834645670104, -0.1049643490035307020, -0.04267023441700976139 ) ) ;
#78934 = CARTESIAN_POINT ( 'NONE',  ( 0.7086614173228352742, -0.1870078740157480879, -0.4822834645669291653 ) ) ;
#78935 = VECTOR ( 'NONE', #12073, 39.37007874015748143 ) ;
#78936 = EDGE_CURVE ( 'NONE', #79833, #66112, #74595, .T. ) ;
#78937 =( BOUNDED_CURVE ( )  B_SPLINE_CURVE ( 2, ( #59786, #6773, #902, #65291, #33301, #1319, #58536, #26559, #53468, #21493, #26968, #13518, #72843 ),
 .UNSPECIFIED., .F., .F. ) 
 B_SPLINE_CURVE_WITH_KNOTS ( ( 3, 2, 2, 2, 2, 2, 3 ),
 ( 0.1733310946348008696, 0.1742424242424242542, 0.1780303030303030387, 0.1818181818181818232, 0.1856060606060606077, 0.1893939393939393923, 0.1903052690015628601 ),
 .UNSPECIFIED. ) 
 CURVE ( )  GEOMETRIC_REPRESENTATION_ITEM ( )  RATIONAL_B_SPLINE_CURVE ( ( 0.9875488213027527884, 0.9918020599134683701, 1.000000000000000000, 0.9659258262890683122, 1.000000000000000000, 0.9659258262890683122, 1.000000000000000000, 0.9659258262890683122, 1.000000000000000000, 0.9659258262890683122, 1.000000000000000000, 0.9918020599134675930, 0.9875488213027519002 ) ) 
 REPRESENTATION_ITEM ( '' )  );
#78938 = VECTOR ( 'NONE', #27062, 39.37007874015748143 ) ;
#78939 = CARTESIAN_POINT ( 'NONE',  ( 1.080276388343102000E-18, 0.09842519685039372024, -8.537024980200822558E-18 ) ) ;
#78940 = CIRCLE ( 'NONE', #42621, 0.5120078740157480990 ) ;
#78941 = CARTESIAN_POINT ( 'NONE',  ( -0.2362204724409451284, 0.4091458600556402425, -1.664698162729658426 ) ) ;
#78942 = AXIS2_PLACEMENT_3D ( 'NONE', #37482, #81299, #61919 ) ;
#78943 = CARTESIAN_POINT ( 'NONE',  ( -0.9776902887139098386, -0.6692913385826771977, 0.1292274648535927661 ) ) ;
#78944 = CARTESIAN_POINT ( 'NONE',  ( -0.2362204724409442680, -0.1870078740157480601, -0.3641732283464567677 ) ) ;
#78945 = CARTESIAN_POINT ( 'NONE',  ( -1.430446194225720724, 0.05413385826771626580, -0.4176697321401330321 ) ) ;
#78946 = CARTESIAN_POINT ( 'NONE',  ( 0.2952755905511819101, 0.07958543189024071263, -0.2665933059059888421 ) ) ;
#78947 = CARTESIAN_POINT ( 'NONE',  ( -0.7677165354330699465, 0.07958543189024085140, 0.2665933059059887866 ) ) ;
#78948 = CARTESIAN_POINT ( 'NONE',  ( -1.167979002624671470, -0.4281496062992127816, -0.4176697321401328100 ) ) ;
#78949 = CARTESIAN_POINT ( 'NONE',  ( -1.587926509186350810, -0.4281496062992124485, 0.4176697321401328655 ) ) ;
#78950 = CARTESIAN_POINT ( 'NONE',  ( -1.443569553805773564, 0.2306618581243847221, -0.2411417322834647770 ) ) ;
#78951 = CARTESIAN_POINT ( 'NONE',  ( 1.056430446194226436, 0.2066929133858267931, 0.1054918080437490802 ) ) ;
#78952 = CARTESIAN_POINT ( 'NONE',  ( 0.7480314960629927956, 0.1771653543307087630, 0.000000000000000000 ) ) ;
#78953 = CARTESIAN_POINT ( 'NONE',  ( 0.3018372703412079971, 0.05413385826771626580, -0.4176697321401330321 ) ) ;
#78954 = CARTESIAN_POINT ( 'NONE',  ( -1.430446194225720724, 0.05413385826771626580, -0.4176697321401330321 ) ) ;
#78955 = CARTESIAN_POINT ( 'NONE',  ( 1.227034120734908917, -0.5511811023622046335, 0.09757992244046803654 ) ) ;
#78956 = ORIENTED_EDGE ( 'NONE', *, *, #72867, .F. ) ;
#78957 = CARTESIAN_POINT ( 'NONE',  ( 0.2925321140481932369, -0.2925321140481931814, -2.694881889763780070 ) ) ;
#78958 = CARTESIAN_POINT ( 'NONE',  ( -1.115485564304461219, -0.004921259842519870586, -0.3153832671262229437 ) ) ;
#78959 = CARTESIAN_POINT ( 'NONE',  ( -0.2821522309711278487, -0.6692913385826773087, -0.1292274648535924053 ) ) ;
#78960 = CARTESIAN_POINT ( 'NONE',  ( 0.1968503937007881344, 0.2952755905511811885, 0.000000000000000000 ) ) ;
#78961 = CARTESIAN_POINT ( 'NONE',  ( -1.509186351706035767, -0.004921259842519870586, -0.3153832671262229437 ) ) ;
#78962 = CARTESIAN_POINT ( 'NONE',  ( -0.1998031496062994405, 0.3460692066303957537, -1.979658792650918597 ) ) ;
#78963 = CARTESIAN_POINT ( 'NONE',  ( -1.207349081364828880, 0.2306618581243847221, -0.2411417322834647770 ) ) ;
#78964 = CARTESIAN_POINT ( 'NONE',  ( 0.3543307086614181922, -0.6692913385826771977, 8.415575281601705876E-17 ) ) ;
#78965 = CARTESIAN_POINT ( 'NONE',  ( 0.1640419947506569498, -0.3162353388693409650, -0.4822834645669289433 ) ) ;
#78966 = CARTESIAN_POINT ( 'NONE',  ( 1.220472440944882386, -0.6692913385826771977, 8.415575281601705876E-17 ) ) ;
#78967 = CARTESIAN_POINT ( 'NONE',  ( -0.2925321140481930149, -0.2925321140481933480, -1.080708661417322691 ) ) ;
#78968 = CARTESIAN_POINT ( 'NONE',  ( 0.2925321140481932369, 0.2925321140481932369, -1.555118110236220597 ) ) ;
#78969 = CARTESIAN_POINT ( 'NONE',  ( 0.1058382717557500713, -0.3949938075777409408, -0.8727034120734908917 ) ) ;
#78970 = CARTESIAN_POINT ( 'NONE',  ( 0.3917322834645670104, -0.1049643490035303273, -0.2611548556430445256 ) ) ;
#78971 = CARTESIAN_POINT ( 'NONE',  ( 0.3412073490813655186, 0.1283753931104748280, 0.1820866141732283561 ) ) ;
#78972 = CARTESIAN_POINT ( 'NONE',  ( -0.3346456692913377662, -0.5400638737290844871, 0.3530559997133364547 ) ) ;
#78973 = CARTESIAN_POINT ( 'NONE',  ( 1.194225721784777594, -0.4281496062992127816, -0.4176697321401328100 ) ) ;
#78974 = CARTESIAN_POINT ( 'NONE',  ( 0.2891555358219910499, -0.2891555358219909944, -1.750000000000000000 ) ) ;
#78975 = CARTESIAN_POINT ( 'NONE',  ( -0.2034120734908128059, 0.1771653543307087630, 0.09757992244046791164 ) ) ;
#78976 = CARTESIAN_POINT ( 'NONE',  ( -1.167979002624671470, 0.05413385826771666132, 0.4176697321401328100 ) ) ;
#78977 = CARTESIAN_POINT ( 'NONE',  ( -1.581364829396324945, -0.05778040916215560624, -0.4822834645669293319 ) ) ;
#78978 = CARTESIAN_POINT ( 'NONE',  ( -0.2362204724409451284, 0.4091458600556402425, -1.902887139107611647 ) ) ;
#78979 = CARTESIAN_POINT ( 'NONE',  ( 0.3796925558546759838, 0.09865214182459616787, -2.755905511811022279 ) ) ;
#78980 = VERTEX_POINT ( 'NONE', #58111 ) ;
#78981 = ORIENTED_EDGE ( 'NONE', *, *, #15919, .F. ) ;
#78982 = CARTESIAN_POINT ( 'NONE',  ( 1.430446194225722500, 0.05413385826771666132, 0.4176697321401328100 ) ) ;
#78983 = CARTESIAN_POINT ( 'NONE',  ( 1.607611548556431069, 0.1771653543307087630, 0.09757992244046791164 ) ) ;
#78984 = EDGE_CURVE ( 'NONE', #49485, #43641, #32872, .T. ) ;
#78986 = CARTESIAN_POINT ( 'NONE',  ( -1.345144356955379816, -0.3162353388693405765, 0.4822834645669290543 ) ) ;
#78985 = CARTESIAN_POINT ( 'NONE',  ( -1.318897637795274802, 0.07958543189024085140, 0.2665933059059887866 ) ) ;
#78987 = CARTESIAN_POINT ( 'NONE',  ( -0.2867679344610366554, 0.2867679344610365444, -2.304442626475378564 ) ) ;
#78988 = DIRECTION ( 'NONE',  ( -1.000000000000000000, -8.673617379884021667E-16, 0.000000000000000000 ) ) ;
#78989 = CARTESIAN_POINT ( 'NONE',  ( 1.246719160104987623, 0.05413385826771626580, -0.4176697321401330321 ) ) ;
#78990 = CARTESIAN_POINT ( 'NONE',  ( -1.141732283464566011, -0.6692913385826771977, 8.415575281601705876E-17 ) ) ;
#78991 = CARTESIAN_POINT ( 'NONE',  ( 0.08530183727034192087, -0.3162353388693409650, -0.4822834645669289433 ) ) ;
#78992 = CARTESIAN_POINT ( 'NONE',  ( -0.2165354330708654795, -0.5400638737290845981, -0.3530559997133363437 ) ) ;
#78993 = CARTESIAN_POINT ( 'NONE',  ( -1.299212598425196097, 0.2952755905511811885, 0.000000000000000000 ) ) ;
#78994 = CARTESIAN_POINT ( 'NONE',  ( 0.1958661417322834775, 0.3392501089628018884, 0.08595800524934374409 ) ) ;
#78995 = CARTESIAN_POINT ( 'NONE',  ( 0.5839895013123367340, -0.6692913385826773087, -0.1292274648535924053 ) ) ;
#78996 = CARTESIAN_POINT ( 'NONE',  ( 0.3392501089628018884, -0.1958661417322834220, -1.671916010498687655 ) ) ;
#78997 = CARTESIAN_POINT ( 'NONE',  ( -1.266404199475064773, -0.08942795157528024563, -0.3641732283464568787 ) ) ;
#78998 = VERTEX_POINT ( 'NONE', #19834 ) ;
#78999 = CARTESIAN_POINT ( 'NONE',  ( 0.1974969037888704704, 0.3420746716998660508, -2.349081364829396446 ) ) ;
#79000 = ORIENTED_EDGE ( 'NONE', *, *, #54265, .T. ) ;
#79001 = CARTESIAN_POINT ( 'NONE',  ( -1.551230140488696119, 1.386514373439803327, 0.4497748127911043725 ) ) ;
#79002 = VECTOR ( 'NONE', #13535, 39.37007874015748143 ) ;
#79003 = CARTESIAN_POINT ( 'NONE',  ( -0.9711286089238838626, -0.6046776061558807314, 0.2411417322834647770 ) ) ;
#79004 = CARTESIAN_POINT ( 'NONE',  ( -1.430446194225720724, 0.05413385826771626580, -0.4176697321401330321 ) ) ;
#79005 = CARTESIAN_POINT ( 'NONE',  ( -0.3460692066303958092, -0.1998031496062994683, -0.5249343832020997302 ) ) ;
#79006 = CARTESIAN_POINT ( 'NONE',  ( -1.548556430446193399, 0.2306618581243848609, 0.2411417322834645549 ) ) ;
#79007 = CARTESIAN_POINT ( 'NONE',  ( -1.614173228346456268, -0.6692913385826771977, 8.415575281601705876E-17 ) ) ;
#79008 = CARTESIAN_POINT ( 'NONE',  ( -1.345144356955379816, -0.3162353388693405765, 0.4822834645669290543 ) ) ;
#79009 = EDGE_CURVE ( 'NONE', #70661, #32372, #12662, .T. ) ;
#79010 = CARTESIAN_POINT ( 'NONE',  ( 4.797336870675656522E-17, -0.3917322834645670104, 0.1515748031496061965 ) ) ;
#79011 = CARTESIAN_POINT ( 'NONE',  ( 0.1377952755905518800, 0.07958543189024071263, -0.2665933059059888421 ) ) ;
#79012 = CARTESIAN_POINT ( 'NONE',  ( -0.3917322834645670104, -7.196005306013484475E-17, -0.7539370078740157410 ) ) ;
#79013 = CARTESIAN_POINT ( 'NONE',  ( -0.9448818897637790704, -0.1870078740157479769, 0.3641732283464567677 ) ) ;
#79014 = CARTESIAN_POINT ( 'NONE',  ( -1.128608923884513837, 0.2306618581243847221, -0.2411417322834647770 ) ) ;
#79015 = EDGE_CURVE ( 'NONE', #41807, #21784, #8586, .T. ) ;
#79016 = CARTESIAN_POINT ( 'NONE',  ( 0.8464566929133865436, 0.1660481256975883668, -0.3530559997133364547 ) ) ;
#79017 = CARTESIAN_POINT ( 'NONE',  ( -0.9908136482939626788, 0.2952755905511811885, 0.1292274648535926551 ) ) ;
#79018 = CARTESIAN_POINT ( 'NONE',  ( -0.1958661417322836718, 0.3392501089628017219, 0.1522309711286089495 ) ) ;
#79019 = EDGE_LOOP ( 'NONE', ( #57182, #55146, #57717, #64885, #78057 ) ) ;
#79020 = CARTESIAN_POINT ( 'NONE',  ( -1.515748031496062076, -0.5400638737290844871, 0.3530559997133364547 ) ) ;
#79021 = CARTESIAN_POINT ( 'NONE',  ( 1.056430446194226436, -0.6692913385826773087, -0.1292274648535924053 ) ) ;
#79022 = CARTESIAN_POINT ( 'NONE',  ( -1.541994750656167090, 0.1771653543307087630, 0.09757992244046791164 ) ) ;
#79023 =( CONVERSION_BASED_UNIT ( 'INCH', #15454 ) LENGTH_UNIT ( ) NAMED_UNIT ( #5085 ) );
#79024 = CARTESIAN_POINT ( 'NONE',  ( -0.4724409448818899238, 0.1265901696524986686, -1.292650918635170454 ) ) ;
#79025 = LINE ( 'NONE', #80271, #14318 ) ;
#79026 = CARTESIAN_POINT ( 'NONE',  ( -0.1958661417322834220, -0.3392501089628018884, -0.3727034120734908362 ) ) ;
#79027 = CARTESIAN_POINT ( 'NONE',  ( -0.1958661417322836718, 0.3392501089628017219, -2.302493438320210029 ) ) ;
#79028 = CARTESIAN_POINT ( 'NONE',  ( -0.1574803149606292529, -0.1870078740157480879, -0.4822834645669291653 ) ) ;
#79029 = CARTESIAN_POINT ( 'NONE',  ( -1.351706036745406347, -0.3690944881889763329, 0.3153832671262228327 ) ) ;
#79030 = CARTESIAN_POINT ( 'NONE',  ( 0.3996062992125986035, -0.1070741851644052972, 0.1266404199475064940 ) ) ;
#79032 = FACE_OUTER_BOUND ( 'NONE', #37954, .T. ) ;
#79031 = CARTESIAN_POINT ( 'NONE',  ( -1.673228346456691717, 0.1660481256975883668, -0.3530559997133364547 ) ) ;
#79033 = CARTESIAN_POINT ( 'NONE',  ( -1.292650918635170010, -0.6692913385826771977, 0.1292274648535927661 ) ) ;
#79034 = CARTESIAN_POINT ( 'NONE',  ( -0.3608923884514428360, -0.6692913385826773087, -0.1292274648535924053 ) ) ;
#79035 = CARTESIAN_POINT ( 'NONE',  ( -9.594673741351310580E-17, 0.3917322834645669549, 0.07744713730414881647 ) ) ;
#79036 = CARTESIAN_POINT ( 'NONE',  ( 0.6102362204724416372, -0.4536011799217367080, 0.2665933059059888421 ) ) ;
#79037 = CARTESIAN_POINT ( 'NONE',  ( -0.3392501089628017219, -0.1958661417322836718, -0.1371391076115486551 ) ) ;
#79038 = CARTESIAN_POINT ( 'NONE',  ( 0.1443569553805781891, -0.004921259842519870586, -0.3153832671262229437 ) ) ;
#79039 = CARTESIAN_POINT ( 'NONE',  ( 0.9973753280839902091, 0.1283753931104746893, -0.1820866141732285504 ) ) ;
#79040 = CARTESIAN_POINT ( 'NONE',  ( 1.056430446194226436, -0.6692913385826773087, -0.1292274648535924053 ) ) ;
#79041 = CARTESIAN_POINT ( 'NONE',  ( 0.1968503937007881344, -0.5511811023622047445, 6.969142054262312111E-17 ) ) ;
#79042 = CARTESIAN_POINT ( 'NONE',  ( -0.3917322834645671215, 0.1049643490035301469, -1.914698162729658648 ) ) ;
#79043 = CARTESIAN_POINT ( 'NONE',  ( -1.069553805774277722, -0.6692913385826773087, -0.1292274648535924053 ) ) ;
#79044 = CARTESIAN_POINT ( 'NONE',  ( -0.2821522309711278487, 0.1771653543307087630, 0.09757992244046791164 ) ) ;
#79045 = EDGE_CURVE ( 'NONE', #60812, #55552, #78342, .T. ) ;
#79046 = CARTESIAN_POINT ( 'NONE',  ( -1.246719160104985846, -0.3690944881889765550, -0.3153832671262227771 ) ) ;
#79047 = CARTESIAN_POINT ( 'NONE',  ( -0.4724409448818899238, 0.1265901696524986686, -0.4245406824146981672 ) ) ;
#79048 = CARTESIAN_POINT ( 'NONE',  ( -0.9711286089238838626, 0.1283753931104746893, -0.1820866141732285504 ) ) ;
#79049 = CARTESIAN_POINT ( 'NONE',  ( 1.614173228346456712, 2.401574803149606474, -0.5309055118110239668 ) ) ;
#79050 = CARTESIAN_POINT ( 'NONE',  ( -0.05905511811023545637, 0.1660481256975885056, 0.3530559997133364547 ) ) ;
#79051 = CARTESIAN_POINT ( 'NONE',  ( -0.3458507752293909498, 0.3458507752293908388, -0.7263779527559055538 ) ) ;
#79052 = ADVANCED_FACE ( 'NONE', ( #21086 ), #19317, .F. ) ;
#79053 = CARTESIAN_POINT ( 'NONE',  ( 0.5577427821522314977, -0.2845877964562161244, -0.3641732283464567121 ) ) ;
#79054 = CARTESIAN_POINT ( 'NONE',  ( -0.3215223097112853146, -0.2845877964562159024, 0.3641732283464567677 ) ) ;
#79055 = CARTESIAN_POINT ( 'NONE',  ( -0.4330708661417315697, -0.6692913385826771977, 8.415575281601705876E-17 ) ) ;
#79056 = CARTESIAN_POINT ( 'NONE',  ( -1.607611548556429737, -0.6692913385826771977, 0.1292274648535927661 ) ) ;
#79057 = CARTESIAN_POINT ( 'NONE',  ( -1.102362204724408601, -0.1870078740157480601, -0.3641732283464567677 ) ) ;
#79058 = CARTESIAN_POINT ( 'NONE',  ( -0.3307086614173228023, -0.3733313776025732333, 0.000000000000000000 ) ) ;
#79059 = CARTESIAN_POINT ( 'NONE',  ( 0.4461942257217856311, 0.2306618581243847221, -0.2411417322834647770 ) ) ;
#79060 = CARTESIAN_POINT ( 'NONE',  ( 0.3460692066303959202, -0.1998031496062991630, -1.441601049868766582 ) ) ;
#79061 = ADVANCED_FACE ( 'NONE', ( #79182 ), #31449, .F. ) ;
#79062 = CARTESIAN_POINT ( 'NONE',  ( 1.555118110236221041, -0.5400638737290844871, 0.3530559997133364547 ) ) ;
#79063 = CARTESIAN_POINT ( 'NONE',  ( -0.09186351706036689768, -0.004921259842519870586, -0.3153832671262229437 ) ) ;
#79064 = AXIS2_PLACEMENT_3D ( 'NONE', #11762, #57163, #18070 ) ;
#79065 = CARTESIAN_POINT ( 'NONE',  ( -1.450131233595799651, 0.2952755905511810774, -0.1292274648535930714 ) ) ;
#79066 = CARTESIAN_POINT ( 'NONE',  ( 1.581364829396326277, -0.3162353388693409650, -0.4822834645669289433 ) ) ;
#79067 = CARTESIAN_POINT ( 'NONE',  ( 2.630268417803937719, 1.724409448818898127, 0.4359958488159723644 ) ) ;
#79068 = CARTESIAN_POINT ( 'NONE',  ( -0.6496062992125976043, -0.4536011799217367080, 0.2665933059059888421 ) ) ;
#79069 = CARTESIAN_POINT ( 'NONE',  ( -0.7677165354330700575, 0.1012011053420777407, 0.2882089793578257453 ) ) ;
#79070 = CARTESIAN_POINT ( 'NONE',  ( 0.8267716535433077274, 0.2952755905511811885, 0.000000000000000000 ) ) ;
#79071 = CARTESIAN_POINT ( 'NONE',  ( -0.3996062992125986035, -0.1070741851644056997, -0.04593175853018373334 ) ) ;
#79072 = CARTESIAN_POINT ( 'NONE',  ( 0.2867679344610366554, 0.2867679344610366554, -2.654218790847456155 ) ) ;
#79073 = CARTESIAN_POINT ( 'NONE',  ( -3.831845081856512181, 2.755400581649067426, -0.5314960629921259283 ) ) ;
#79074 = CARTESIAN_POINT ( 'NONE',  ( -1.673228346456691717, 0.1660481256975883668, -0.3530559997133364547 ) ) ;
#79075 = CARTESIAN_POINT ( 'NONE',  ( -1.128608923884513837, -0.6046776061558807314, 0.2411417322834647770 ) ) ;
#79076 = CARTESIAN_POINT ( 'NONE',  ( 1.430446194225722500, 0.05413385826771666132, 0.4176697321401328100 ) ) ;
#79077 = CARTESIAN_POINT ( 'NONE',  ( -0.2867679344610364334, -0.2867679344610367109, -2.348425196850393970 ) ) ;
#79078 = CARTESIAN_POINT ( 'NONE',  ( 1.174540682414699111, -0.2845877964562159024, 0.3641732283464567677 ) ) ;
#79079 = CARTESIAN_POINT ( 'NONE',  ( 0.3149606299212606708, -0.1870078740157480879, -0.4822834645669291653 ) ) ;
#79080 = CARTESIAN_POINT ( 'NONE',  ( -0.3346456692913377662, 0.1660481256975883668, -0.3530559997133364547 ) ) ;
#79081 = CARTESIAN_POINT ( 'NONE',  ( 1.686351706036745890, 0.2952755905511811885, 0.1292274648535926551 ) ) ;
#79082 = FACE_OUTER_BOUND ( 'NONE', #4954, .T. ) ;
#79083 = CARTESIAN_POINT ( 'NONE',  ( 0.9120734908136489683, -0.5511811023622046335, 0.09757992244046803654 ) ) ;
#79084 = VERTEX_POINT ( 'NONE', #40032 ) ;
#79085 = CARTESIAN_POINT ( 'NONE',  ( -0.2867679344610365444, -0.2867679344610367664, -0.3707542239183220789 ) ) ;
#79086 = ORIENTED_EDGE ( 'NONE', *, *, #40252, .T. ) ;
#79087 = CARTESIAN_POINT ( 'NONE',  ( -0.3477690288713905509, -0.6692913385826771977, 0.1292274648535927661 ) ) ;
#79088 = CARTESIAN_POINT ( 'NONE',  ( 1.266404199475066328, -0.05778040916215522460, 0.4822834645669289988 ) ) ;
#79089 = CARTESIAN_POINT ( 'NONE',  ( 0.3412073490813655186, -0.6046776061558809534, -0.2411417322834644161 ) ) ;
#79090 = CARTESIAN_POINT ( 'NONE',  ( -0.1902887139107604098, 0.1771653543307087075, -0.09757992244046823083 ) ) ;
#79091 = CARTESIAN_POINT ( 'NONE',  ( 1.167979002624672580, -0.4281496062992124485, 0.4176697321401328655 ) ) ;
#79092 = CARTESIAN_POINT ( 'NONE',  ( -0.9448818897637790704, -0.1870078740157480879, -0.4822834645669291653 ) ) ;
#79093 = CARTESIAN_POINT ( 'NONE',  ( 0.1640419947506569498, -0.05778040916215522460, 0.4822834645669289988 ) ) ;
#79094 = CARTESIAN_POINT ( 'NONE',  ( -0.8202099737532801971, -0.6692913385826771977, 0.1292274648535927661 ) ) ;
#79095 = CARTESIAN_POINT ( 'NONE',  ( 1.266404199475066328, -0.05778040916215522460, 0.4822834645669289988 ) ) ;
#79096 = CARTESIAN_POINT ( 'NONE',  ( 0.8530183727034126306, 0.05413385826771626580, -0.4176697321401330321 ) ) ;
#79097 = CARTESIAN_POINT ( 'NONE',  ( 1.312335958005250269, -0.6046776061558807314, 0.2411417322834647770 ) ) ;
#79098 = CARTESIAN_POINT ( 'NONE',  ( 4.797336870675656522E-17, -0.3917322834645670104, -0.5433070866141732624 ) ) ;
#79099 = CARTESIAN_POINT ( 'NONE',  ( -0.08530183727034056085, -0.2845877964562159024, 0.3641732283464567677 ) ) ;
#79100 = EDGE_LOOP ( 'NONE', ( #46228, #33330, #64581, #19735 ) ) ;
#79101 = CARTESIAN_POINT ( 'NONE',  ( 0.2891555358219910499, -0.2891555358219909944, -1.043307086614173373 ) ) ;
#79102 = ORIENTED_EDGE ( 'NONE', *, *, #9376, .T. ) ;
#79103 = CARTESIAN_POINT ( 'NONE',  ( -0.7086614173228339419, -0.1870078740157480601, -0.3641732283464567677 ) ) ;
#79104 = CARTESIAN_POINT ( 'NONE',  ( -0.1246719160104980823, -0.6692913385826773087, -0.1292274648535924053 ) ) ;
#79105 = CARTESIAN_POINT ( 'NONE',  ( 2.856580783922613609, 1.081851677178490068, 0.1334749385307572034 ) ) ;
#79106 = CARTESIAN_POINT ( 'NONE',  ( -0.1902887139107604098, -0.6692913385826771977, 0.1292274648535927661 ) ) ;
#79107 = CARTESIAN_POINT ( 'NONE',  ( -0.2493438320209966919, 0.05413385826771626580, -0.4176697321401330321 ) ) ;
#79108 = CARTESIAN_POINT ( 'NONE',  ( -0.7217847769028863381, -0.4281496062992124485, 0.4176697321401328655 ) ) ;
#79109 = ADVANCED_FACE ( 'NONE', ( #1733 ), #53880, .F. ) ;
#79110 = CARTESIAN_POINT ( 'NONE',  ( -1.555118110236219930, 0.1660481256975885056, 0.3530559997133364547 ) ) ;
#79111 = CARTESIAN_POINT ( 'NONE',  ( 1.377952755905512472, 0.1771653543307087630, 0.000000000000000000 ) ) ;
#79112 = CARTESIAN_POINT ( 'NONE',  ( -1.541994750656167090, -0.6692913385826773087, -0.1292274648535924053 ) ) ;
#79113 = CARTESIAN_POINT ( 'NONE',  ( 0.2945512653497797673, 0.02373080790438491378, 5.526002588227517442 ) ) ;
#79114 = CARTESIAN_POINT ( 'NONE',  ( 0.6561679790026253567, 0.1283753931104748280, 0.1820866141732283561 ) ) ;
#79115 = CARTESIAN_POINT ( 'NONE',  ( 0.01312335958005323398, -0.4281496062992127816, -0.4176697321401328100 ) ) ;
#79116 = CARTESIAN_POINT ( 'NONE',  ( 0.1968503937007881344, -0.6692913385826771977, 8.415575281601705876E-17 ) ) ;
#79117 = ORIENTED_EDGE ( 'NONE', *, *, #6402, .F. ) ;
#79118 = CARTESIAN_POINT ( 'NONE',  ( 0.3996062992125986590, -0.1070741851644053111, -1.686351706036745446 ) ) ;
#79119 = CARTESIAN_POINT ( 'NONE',  ( -1.614173228346456268, -0.6692913385826771977, 8.415575281601705876E-17 ) ) ;
#79120 = CARTESIAN_POINT ( 'NONE',  ( -9.787531504996566615E-17, 0.3996062992125985480, -1.021653543307086576 ) ) ;
#79121 = CARTESIAN_POINT ( 'NONE',  ( -0.3460692066303960313, 0.1998031496062989965, -0.4179790026246719137 ) ) ;
#79122 = CARTESIAN_POINT ( 'NONE',  ( -0.6955380577427815458, -0.4281496062992127816, -0.4176697321401328100 ) ) ;
#79123 = CARTESIAN_POINT ( 'NONE',  ( 0.2362204724409451007, -0.4091458600556402980, -0.09186351706036745279 ) ) ;
#79124 = CARTESIAN_POINT ( 'NONE',  ( 0.1958661417322834775, 0.3392501089628018884, -2.276246719160105236 ) ) ;
#79125 = CARTESIAN_POINT ( 'NONE',  ( -1.587926509186350810, -0.004921259842519870586, -0.3153832671262229437 ) ) ;
#79126 = CARTESIAN_POINT ( 'NONE',  ( 0.7217847769028878924, -0.4281496062992127816, -0.4176697321401328100 ) ) ;
#79127 = CARTESIAN_POINT ( 'NONE',  ( 0.8398950131233602345, -0.6046776061558807314, 0.2411417322834647770 ) ) ;
#79128 = CARTESIAN_POINT ( 'NONE',  ( -0.3543307086614165824, 0.1771653543307087630, 0.000000000000000000 ) ) ;
#79129 = CARTESIAN_POINT ( 'NONE',  ( -0.02624671916010428221, -0.6046776061558807314, 0.2411417322834647770 ) ) ;
#79130 = CARTESIAN_POINT ( 'NONE',  ( -1.157146581871515012E-16, 0.4724409448818898682, -1.966535433070865979 ) ) ;
#79131 = CARTESIAN_POINT ( 'NONE',  ( 0.01968503937007957949, -0.4536011799217368745, -0.2665933059059886201 ) ) ;
#79132 = CARTESIAN_POINT ( 'NONE',  ( 0.08530183727034192087, -0.3162353388693409650, -0.4822834645669289433 ) ) ;
#79133 = CARTESIAN_POINT ( 'NONE',  ( 0.2891555358219910499, 0.2891555358219910499, -1.316929133858267598 ) ) ;
#79134 = CARTESIAN_POINT ( 'NONE',  ( 1.587926509186352142, -0.004921259842519576551, 0.3153832671262227771 ) ) ;
#79135 = CARTESIAN_POINT ( 'NONE',  ( 0.2821522309711292364, -0.5511811023622046335, 0.09757992244046803654 ) ) ;
#79136 = CARTESIAN_POINT ( 'NONE',  ( 1.686351706036745890, 0.1771653543307087630, 0.09757992244046791164 ) ) ;
#79137 = CARTESIAN_POINT ( 'NONE',  ( -0.9317585301837263412, 0.05413385826771666132, 0.4176697321401328100 ) ) ;
#79138 = CARTESIAN_POINT ( 'NONE',  ( -0.8005249343832011588, -0.004921259842519870586, -0.3153832671262229437 ) ) ;
#79139 = LINE ( 'NONE', #72395, #35907 ) ;
#79140 = CARTESIAN_POINT ( 'NONE',  ( -0.9120734908136475250, 0.2952755905511811885, 0.1292274648535926551 ) ) ;
#79141 = CARTESIAN_POINT ( 'NONE',  ( -0.4921259842519677963, 0.1660481256975883668, -0.3530559997133364547 ) ) ;
#79142 = CARTESIAN_POINT ( 'NONE',  ( -0.06561679790026180015, 0.05413385826771666132, 0.4176697321401328100 ) ) ;
#79143 = CARTESIAN_POINT ( 'NONE',  ( -0.2925321140481930149, -0.2925321140481933480, -2.655511811023622215 ) ) ;
#79144 = CARTESIAN_POINT ( 'NONE',  ( 0.2867679344610365999, -0.2867679344610365999, -2.068222154034434546 ) ) ;
#79145 = CARTESIAN_POINT ( 'NONE',  ( -1.852066570651491384, 1.064797240280318080, 0.04222672046130301199 ) ) ;
#79146 = CARTESIAN_POINT ( 'NONE',  ( 0.7874015748031503170, -0.1870078740157480601, -0.3641732283464567677 ) ) ;
#79147 = CARTESIAN_POINT ( 'NONE',  ( 1.541994750656168645, -0.6692913385826771977, 0.1292274648535927661 ) ) ;
#79148 = CARTESIAN_POINT ( 'NONE',  ( -1.430446194225721390, -0.3690944881889763329, 0.3153832671262228327 ) ) ;
#79149 = CARTESIAN_POINT ( 'NONE',  ( 0.9776902887139113929, -0.6692913385826773087, -0.1292274648535924053 ) ) ;
#79150 = CARTESIAN_POINT ( 'NONE',  ( -1.095800524934382292, -0.08942795157527998196, 0.3641732283464567121 ) ) ;
#79151 = B_SPLINE_CURVE_WITH_KNOTS ( 'NONE', 3,
 ( #4348, #30015, #55678, #77552 ),
 .UNSPECIFIED., .F., .F.,
 ( 4, 4 ),
 ( 2.888536477662776634E-07, 0.001436607511248048788 ),
 .UNSPECIFIED. ) ;
#79152 = CARTESIAN_POINT ( 'NONE',  ( -0.3674540682414692561, -0.6046776061558809534, -0.2411417322834644161 ) ) ;
#79153 = CARTESIAN_POINT ( 'NONE',  ( 0.3149606299212606708, -0.1870078740157480601, -0.3641732283464567677 ) ) ;
#79154 = CARTESIAN_POINT ( 'NONE',  ( 0.7283464566929140904, -0.4536011799217368745, -0.2665933059059886201 ) ) ;
#79155 = CARTESIAN_POINT ( 'NONE',  ( 0.1902887139107617975, -0.6692913385826773087, -0.1292274648535924053 ) ) ;
#79156 = CARTESIAN_POINT ( 'NONE',  ( -0.3996062992125986590, 0.1070741851644051723, -0.2670603674540683037 ) ) ;
#79157 = CARTESIAN_POINT ( 'NONE',  ( -0.6299212598425188991, -0.1870078740157479769, 0.4822834645669291653 ) ) ;
#79158 = CARTESIAN_POINT ( 'NONE',  ( -0.2867679344610365999, 0.2867679344610364889, -1.364173228346456268 ) ) ;
#79159 = CARTESIAN_POINT ( 'NONE',  ( 1.023622047244095112, -0.1870078740157480601, -0.3641732283464567677 ) ) ;
#79160 = CARTESIAN_POINT ( 'NONE',  ( 0.5905511811023629321, 0.2952755905511811885, 0.000000000000000000 ) ) ;
#79161 = CARTESIAN_POINT ( 'NONE',  ( -0.1574803149606292529, -0.1870078740157480879, -0.4822834645669291653 ) ) ;
#79162 = CARTESIAN_POINT ( 'NONE',  ( -0.3280839895013117347, -0.004921259842519870586, -0.3153832671262229437 ) ) ;
#79163 = CARTESIAN_POINT ( 'NONE',  ( 0.000000000000000000, 0.000000000000000000, -1.250000000000000000 ) ) ;
#79164 = CARTESIAN_POINT ( 'NONE',  ( -0.08530183727034056085, -0.2845877964562159024, 0.3641732283464567677 ) ) ;
#79165 = CARTESIAN_POINT ( 'NONE',  ( 0.1574803149606306130, -0.1870078740157480879, -0.4822834645669291653 ) ) ;
#79166 = CARTESIAN_POINT ( 'NONE',  ( -0.7020997375328076329, -0.2845877964562161244, -0.3641732283464567121 ) ) ;
#79167 = CARTESIAN_POINT ( 'NONE',  ( 0.3460692066303959202, -0.1998031496062991630, -1.126640419947506633 ) ) ;
#79168 = CARTESIAN_POINT ( 'NONE',  ( -0.9383202099737524282, -0.3162353388693409650, -0.4822834645669289433 ) ) ;
#79169 = FACE_OUTER_BOUND ( 'NONE', #23910, .T. ) ;
#79170 = EDGE_LOOP ( 'NONE', ( #43041, #72358 ) ) ;
#79171 = CARTESIAN_POINT ( 'NONE',  ( -0.9711286089238838626, -0.5023911411419708095, 0.1820866141732285504 ) ) ;
#79172 = CARTESIAN_POINT ( 'NONE',  ( 0.06561679790026316017, 0.05413385826771626580, -0.4176697321401330321 ) ) ;
#79173 = B_SPLINE_CURVE_WITH_KNOTS ( 'NONE', 1,
 ( #82986, #25306 ),
 .UNSPECIFIED., .F., .F.,
 ( 2, 2 ),
 ( 0.000000000000000000, 0.001849999999999997480 ),
 .UNSPECIFIED. ) ;
#79174 = CARTESIAN_POINT ( 'NONE',  ( -1.568241469816272105, -0.05778040916215522460, 0.4822834645669289988 ) ) ;
#79175 = CARTESIAN_POINT ( 'NONE',  ( -0.7939632545931750718, -0.05778040916215560624, -0.4822834645669293319 ) ) ;
#79176 =( BOUNDED_CURVE ( )  B_SPLINE_CURVE ( 2, ( #14724, #59726, #2081, #16378, #2502, #3321, #73200, #36129, #67718, #35308, #80767, #79950, #15968 ),
 .UNSPECIFIED., .F., .F. ) 
 B_SPLINE_CURVE_WITH_KNOTS ( ( 3, 2, 2, 2, 2, 2, 3 ),
 ( 0.6278765491802553722, 0.6287878787878787845, 0.6325757575757575690, 0.6363636363636363535, 0.6401515151515151381, 0.6439393939393939226, 0.6448507235470174459 ),
 .UNSPECIFIED. ) 
 CURVE ( )  GEOMETRIC_REPRESENTATION_ITEM ( )  RATIONAL_B_SPLINE_CURVE ( ( 0.9875488213027523443, 0.9918020599134680371, 1.000000000000000000, 0.9659258262890683122, 1.000000000000000000, 0.9659258262890683122, 1.000000000000000000, 0.9659258262890683122, 1.000000000000000000, 0.9659258262890683122, 1.000000000000000000, 0.9918020599134671489, 0.9875488213027514561 ) ) 
 REPRESENTATION_ITEM ( '' )  );
#79177 = CARTESIAN_POINT ( 'NONE',  ( 1.141392835773559211, 0.3937007874015748254, 1.456353465694822491 ) ) ;
#79179 = CARTESIAN_POINT ( 'NONE',  ( 0.9580052493438326877, 0.05413385826771666132, 0.4176697321401328100 ) ) ;
#79178 = CARTESIAN_POINT ( 'NONE',  ( -0.8923884514435688198, 0.2306618581243847221, -0.2411417322834647770 ) ) ;
#79180 = CARTESIAN_POINT ( 'NONE',  ( 1.030183727034121421, -0.05778040916215522460, 0.4822834645669289988 ) ) ;
#79181 = FACE_OUTER_BOUND ( 'NONE', #2443, .T. ) ;
#79182 = FACE_OUTER_BOUND ( 'NONE', #45819, .T. ) ;
#79183 = CARTESIAN_POINT ( 'NONE',  ( -1.391076115485563758, 0.2306618581243848609, 0.2411417322834645549 ) ) ;
#79184 = CARTESIAN_POINT ( 'NONE',  ( 0.3996062992125986035, 0.1070741851644054776, -0.2821522309711286258 ) ) ;
#79185 = ORIENTED_EDGE ( 'NONE', *, *, #47021, .T. ) ;
#79186 = CARTESIAN_POINT ( 'NONE',  ( -0.4461942257217840213, -0.5023911411419708095, -0.1820866141732282451 ) ) ;
#79187 = CARTESIAN_POINT ( 'NONE',  ( 0.1049643490035303689, 0.3917322834645670104, -2.347769028871391050 ) ) ;
#79188 = VERTEX_POINT ( 'NONE', #21497 ) ;
#79189 = CARTESIAN_POINT ( 'NONE',  ( 0.8858267716535438430, -0.5400638737290845981, -0.3530559997133363437 ) ) ;
#79190 = CARTESIAN_POINT ( 'NONE',  ( -0.1181102362204717315, 0.2952755905511811885, 0.000000000000000000 ) ) ;
#79191 = CARTESIAN_POINT ( 'NONE',  ( -0.8267716535433065062, 0.2952755905511811885, 0.000000000000000000 ) ) ;
#79192 = CARTESIAN_POINT ( 'NONE',  ( 1.607611548556431069, -0.6692913385826773087, -0.1292274648535924053 ) ) ;
#79193 = CARTESIAN_POINT ( 'NONE',  ( -0.8136482939632537770, 0.1283753931104746893, -0.1820866141732285504 ) ) ;
#79194 = CARTESIAN_POINT ( 'NONE',  ( 0.4091458600556404646, -0.2362204724409448231, -2.071522309711285814 ) ) ;
#79195 = CARTESIAN_POINT ( 'NONE',  ( 0.4199475065616805614, 0.2306618581243848609, 0.2411417322834645549 ) ) ;
#79196 = CARTESIAN_POINT ( 'NONE',  ( 0.6889763779527563470, 0.07958543189024071263, -0.2665933059059888421 ) ) ;
#79197 = CARTESIAN_POINT ( 'NONE',  ( -0.5708661417322825615, -0.5400638737290844871, 0.3530559997133364547 ) ) ;
#79198 = CARTESIAN_POINT ( 'NONE',  ( 0.3392501089628018329, -0.1958661417322834497, -1.759823203903200017 ) ) ;
#79199 = CARTESIAN_POINT ( 'NONE',  ( -1.345144356955379816, -0.3162353388693405765, 0.4822834645669290543 ) ) ;
#79200 = FACE_OUTER_BOUND ( 'NONE', #18108, .T. ) ;
#79201 = CARTESIAN_POINT ( 'NONE',  ( 1.233595800524935227, 0.2306618581243847221, -0.2411417322834647770 ) ) ;
#79202 = CARTESIAN_POINT ( 'NONE',  ( 1.463254593175853824, -0.5511811023622046335, 0.09757992244046803654 ) ) ;
#79203 = ORIENTED_EDGE ( 'NONE', *, *, #2022, .F. ) ;
#79204 = CARTESIAN_POINT ( 'NONE',  ( 0.1049643490035304799, -0.3917322834645670104, -2.759205667487876656 ) ) ;
#79205 = CARTESIAN_POINT ( 'NONE',  ( -0.3937007874015740483, -0.1870078740157479769, 0.4822834645669291653 ) ) ;
#79206 = VERTEX_POINT ( 'NONE', #33713 ) ;
#79207 = CARTESIAN_POINT ( 'NONE',  ( 0.6102362204724416372, -0.4536011799217367080, 0.2665933059059888421 ) ) ;
#79208 = CARTESIAN_POINT ( 'NONE',  ( -1.023622047244094002, -0.1870078740157480879, -0.4822834645669291653 ) ) ;
#79209 = CARTESIAN_POINT ( 'NONE',  ( 1.003937007874016185, 0.1660481256975883668, -0.3530559997133364547 ) ) ;
#79210 = CARTESIAN_POINT ( 'NONE',  ( 0.6364829396325465405, -0.05778040916215522460, 0.4822834645669289988 ) ) ;
#79211 = CARTESIAN_POINT ( 'NONE',  ( 0.1509186351706042484, -0.3162353388693405765, 0.4822834645669290543 ) ) ;
#79212 = CARTESIAN_POINT ( 'NONE',  ( -0.5380577427821514602, 0.05413385826771666132, 0.4176697321401328100 ) ) ;
#79213 = CARTESIAN_POINT ( 'NONE',  ( 0.3917322834645670104, -0.1049643490035303411, -1.770997375328083656 ) ) ;
#79214 = CARTESIAN_POINT ( 'NONE',  ( 1.548556430446194954, -0.5023911411419708095, 0.1820866141732285504 ) ) ;
#79215 = CARTESIAN_POINT ( 'NONE',  ( -0.7283464566929126471, -0.5400638737290844871, 0.3530559997133364547 ) ) ;
#79216 = CARTESIAN_POINT ( 'NONE',  ( -0.6233595800524928121, -0.2845877964562161244, -0.3641732283464567121 ) ) ;
#79217 = CARTESIAN_POINT ( 'NONE',  ( 1.646981627296588035, -0.3162353388693405765, 0.4822834645669290543 ) ) ;
#79218 = CARTESIAN_POINT ( 'NONE',  ( 3.937007874015748143, 2.755905511811024056, -0.5314960629921260393 ) ) ;
#79219 = CARTESIAN_POINT ( 'NONE',  ( -0.3674540682414692561, -0.6046776061558809534, -0.2411417322834644161 ) ) ;
#79220 = CARTESIAN_POINT ( 'NONE',  ( 0.2624671916010504757, 0.1539470093639523085, 0.1968503937007873850 ) ) ;
#79221 = CARTESIAN_POINT ( 'NONE',  ( 0.7217847769028878924, -0.4281496062992127816, -0.4176697321401328100 ) ) ;
#79222 = CARTESIAN_POINT ( 'NONE',  ( 0.2925321140481932369, -0.2925321140481932369, -1.830708661417322913 ) ) ;
#79223 = CARTESIAN_POINT ( 'NONE',  ( 3.931500874951350255, 1.110937023017455783, 0.2101396702808374650 ) ) ;
#79224 = CARTESIAN_POINT ( 'NONE',  ( -0.08530183727034056085, -0.3162353388693405765, 0.4822834645669290543 ) ) ;
#79226 = CARTESIAN_POINT ( 'NONE',  ( 1.141392835773559211, 0.4110443821404751730, 1.141392835773562764 ) ) ;
#79225 = CARTESIAN_POINT ( 'NONE',  ( 0.9186351706036752773, 0.1283753931104746893, -0.1820866141732285504 ) ) ;
#79227 = CARTESIAN_POINT ( 'NONE',  ( -0.4091458600556405756, 0.2362204724409446288, -0.5754593175853018883 ) ) ;
#79228 = CARTESIAN_POINT ( 'NONE',  ( 1.286089238845145033, -0.5023911411419708095, -0.1820866141732282451 ) ) ;
#79229 = CIRCLE ( 'NONE', #65764, 0.2952755905511810774 ) ;
#79230 = CARTESIAN_POINT ( 'NONE',  ( 1.017060367454068581, -0.05778040916215560624, -0.4822834645669293319 ) ) ;
#79231 = CARTESIAN_POINT ( 'NONE',  ( -0.3420746716998662729, 0.1974969037888702206, -0.2604986876640420501 ) ) ;
#79232 = CARTESIAN_POINT ( 'NONE',  ( -0.1902887139107604098, -0.6692913385826771977, 0.1292274648535927661 ) ) ;
#79233 = CARTESIAN_POINT ( 'NONE',  ( -1.640419947506561060, 0.05413385826771666132, 0.4176697321401328100 ) ) ;
#79234 = CARTESIAN_POINT ( 'NONE',  ( -1.719160104986876103, 0.05413385826771666132, 0.4176697321401328100 ) ) ;
#79235 = CARTESIAN_POINT ( 'NONE',  ( -0.07874015748031421014, -0.1870078740157480879, -0.4822834645669291653 ) ) ;
#79236 = CARTESIAN_POINT ( 'NONE',  ( 0.1974969037888706092, -0.3420746716998660508, -0.3261154855643044748 ) ) ;
#79237 = CARTESIAN_POINT ( 'NONE',  ( 1.089238845144357759, 0.05413385826771626580, -0.4176697321401330321 ) ) ;
#79238 = CARTESIAN_POINT ( 'NONE',  ( 0.3937007874015754361, -0.1870078740157480879, -0.4822834645669291653 ) ) ;
#79239 = CARTESIAN_POINT ( 'NONE',  ( 0.5839895013123367340, 0.1771653543307087630, 0.09757992244046791164 ) ) ;
#79240 = CARTESIAN_POINT ( 'NONE',  ( -0.4744094488188934089, 1.537401574803149984, -1.016821367227985551 ) ) ;
#79241 = CARTESIAN_POINT ( 'NONE',  ( 0.4461942257217856311, 0.1283753931104746893, -0.1820866141732285504 ) ) ;
#79242 = CARTESIAN_POINT ( 'NONE',  ( -1.036394771582349383, 0.004960608223777852183, -0.3437734562760195733 ) ) ;
#79243 = CARTESIAN_POINT ( 'NONE',  ( -0.3460692066303957537, -0.1998031496062994405, -1.231627296587926690 ) ) ;
#79244 = CARTESIAN_POINT ( 'NONE',  ( 0.7874015748031503170, -0.1870078740157480879, -0.4822834645669291653 ) ) ;
#79245 = CARTESIAN_POINT ( 'NONE',  ( -0.1958661417322836718, 0.3392501089628017219, -1.265091863517060489 ) ) ;
#79246 = CARTESIAN_POINT ( 'NONE',  ( 0.8923884514435703741, 0.2306618581243848609, 0.2411417322834645549 ) ) ;
#79247 = CARTESIAN_POINT ( 'NONE',  ( -0.3412073490813641308, 0.1539470093639521697, -0.1968503937007875793 ) ) ;
#79248 = CARTESIAN_POINT ( 'NONE',  ( 0.1377952755905518800, -0.4536011799217367080, 0.2665933059059888421 ) ) ;
#79249 = CARTESIAN_POINT ( 'NONE',  ( -0.06561679790026180015, 0.05413385826771666132, 0.4176697321401328100 ) ) ;
#79250 = CARTESIAN_POINT ( 'NONE',  ( 1.207349081364829990, 0.1283753931104748280, 0.1820866141732283561 ) ) ;
#79251 = CARTESIAN_POINT ( 'NONE',  ( -1.220472440944881054, 0.1771653543307087630, 0.000000000000000000 ) ) ;
#79252 = CARTESIAN_POINT ( 'NONE',  ( -1.043307086614172707, 0.1660481256975883668, -0.3530559997133364547 ) ) ;
#79253 = CARTESIAN_POINT ( 'NONE',  ( -1.692913385826770645, 0.2952755905511811885, 0.000000000000000000 ) ) ;
#79254 = CARTESIAN_POINT ( 'NONE',  ( 0.7349081364829403995, 0.2306618581243848609, 0.2411417322834645549 ) ) ;
#79255 = CARTESIAN_POINT ( 'NONE',  ( 1.404199475065617708, 0.05413385826771626580, -0.4176697321401330321 ) ) ;
#79256 = CARTESIAN_POINT ( 'NONE',  ( -0.9285414500055708675, 0.000000000000000000, -0.6299212598425202314 ) ) ;
#79257 = CARTESIAN_POINT ( 'NONE',  ( 0.7020997375328090762, -0.05778040916215560624, -0.4822834645669293319 ) ) ;
#79258 = CARTESIAN_POINT ( 'NONE',  ( 0.3458507752293908943, -0.3458507752293908943, -2.852362204724409711 ) ) ;
#79259 = CARTESIAN_POINT ( 'NONE',  ( 0.4262708303801458487, 1.326867047802282373, 3.913881452109020831 ) ) ;
#79260 = CARTESIAN_POINT ( 'NONE',  ( 1.233595800524935227, 0.2306618581243847221, -0.2411417322834647770 ) ) ;
#79261 = CARTESIAN_POINT ( 'NONE',  ( -1.450131233595799651, -0.5511811023622046335, 0.09757992244046803654 ) ) ;
#79262 = CARTESIAN_POINT ( 'NONE',  ( 1.056430446194226658, 0.1771653543307087630, 0.09757992244046791164 ) ) ;
#79263 = CARTESIAN_POINT ( 'NONE',  ( -1.371391076115484609, -0.5511811023622046335, 0.09757992244046803654 ) ) ;
#79264 = CARTESIAN_POINT ( 'NONE',  ( -0.7349081364829387342, -0.5023911411419708095, 0.1820866141732285504 ) ) ;
#79265 = DIRECTION ( 'NONE',  ( 1.000000000000000000, 8.805702923740138355E-17, -0.000000000000000000 ) ) ;
#79266 = CARTESIAN_POINT ( 'NONE',  ( 0.5774278215223103139, -0.5023911411419708095, -0.1820866141732282451 ) ) ;
#79267 = CARTESIAN_POINT ( 'NONE',  ( 0.1902887139107617975, -0.6692913385826773087, -0.1292274648535924053 ) ) ;
#79268 = CARTESIAN_POINT ( 'NONE',  ( 1.292650918635171564, 0.2952755905511811885, 0.1292274648535926551 ) ) ;
#79269 = CARTESIAN_POINT ( 'NONE',  ( -0.03937007874015669567, 0.2952755905511811885, 0.000000000000000000 ) ) ;
#79270 = EDGE_CURVE ( 'NONE', #48838, #22548, #54439, .T. ) ;
#79271 = CARTESIAN_POINT ( 'NONE',  ( 0.006561679790026889343, -0.08942795157527998196, 0.3641732283464567121 ) ) ;
#79272 = CARTESIAN_POINT ( 'NONE',  ( 1.062992125984252745, -0.6692913385826771977, 8.415575281601705876E-17 ) ) ;
#79273 = DIRECTION ( 'NONE',  ( 3.096699300667737957E-16, -1.000000000000000000, 0.000000000000000000 ) ) ;
#79274 = CARTESIAN_POINT ( 'NONE',  ( -1.023622047244094002, -0.1870078740157480879, -0.4822834645669291653 ) ) ;
#79275 = CARTESIAN_POINT ( 'NONE',  ( 0.2925321140481932369, 0.2925321140481932369, -0.7677165354330708347 ) ) ;
#79276 = CARTESIAN_POINT ( 'NONE',  ( -0.4724409448818898682, 5.785732909357575061E-17, -2.755905511811024056 ) ) ;
#79277 = CARTESIAN_POINT ( 'NONE',  ( -0.8595800524934373854, -0.05778040916215522460, 0.4822834645669289988 ) ) ;
#79278 = CARTESIAN_POINT ( 'NONE',  ( -0.2690288713910754526, 0.2952755905511810774, -0.1292274648535930714 ) ) ;
#79279 = CARTESIAN_POINT ( 'NONE',  ( -0.3460692066303958092, -0.1998031496062994683, -2.729658792650918375 ) ) ;
#79280 = CARTESIAN_POINT ( 'NONE',  ( -0.1058382717557503211, 0.3949938075777409408, -2.211286089238845065 ) ) ;
#79281 = VERTEX_POINT ( 'NONE', #60213 ) ;
#79282 = CARTESIAN_POINT ( 'NONE',  ( 0.2867679344610365999, 0.2867679344610365999, -1.074803149606299080 ) ) ;
#79283 = CARTESIAN_POINT ( 'NONE',  ( -1.614173228346456712, 2.401574803149606474, 0.1372047244094477536 ) ) ;
#79284 = CARTESIAN_POINT ( 'NONE',  ( -1.469816272965878357, -0.5023911411419708095, -0.1820866141732282451 ) ) ;
#79285 = CARTESIAN_POINT ( 'NONE',  ( 0.3917322834645669549, 0.1049643490035304660, -1.219160104986876325 ) ) ;
#79286 = CARTESIAN_POINT ( 'NONE',  ( 1.587926509186352142, -0.004921259842519576551, 0.3153832671262227771 ) ) ;
#79287 = CARTESIAN_POINT ( 'NONE',  ( -0.2867679344610366554, 0.2867679344610365444, 0.05776209793407005577 ) ) ;
#79288 = CARTESIAN_POINT ( 'NONE',  ( -0.1509186351706028884, -0.3162353388693409650, -0.4822834645669289433 ) ) ;
#79289 = CARTESIAN_POINT ( 'NONE',  ( -0.5183727034120726440, -0.5511811023622048555, -0.09757992244046775898 ) ) ;
#79291 = EDGE_CURVE ( 'NONE', #41808, #29808, #46234, .T. ) ;
#79290 = CARTESIAN_POINT ( 'NONE',  ( 0.6955380577427828781, 0.05413385826771626580, -0.4176697321401330321 ) ) ;
#79292 = CARTESIAN_POINT ( 'NONE',  ( 0.3543307086614179147, 0.2952755905511811885, 0.000000000000000000 ) ) ;
#79293 = CYLINDRICAL_SURFACE ( 'NONE', #26003, 0.5118110236220472231 ) ;
#79294 = CARTESIAN_POINT ( 'NONE',  ( -0.3392501089628019995, 0.1958661417322831999, -1.125347399771340573 ) ) ;
#79295 = CARTESIAN_POINT ( 'NONE',  ( 1.450131233595801428, -0.6692913385826773087, -0.1292274648535924053 ) ) ;
#79296 = CARTESIAN_POINT ( 'NONE',  ( 0.1902887139107617975, 0.2952755905511811885, 0.1292274648535926551 ) ) ;
#79297 = CARTESIAN_POINT ( 'NONE',  ( -0.8267716535433065062, 0.2952755905511811885, 0.000000000000000000 ) ) ;
#79298 = CARTESIAN_POINT ( 'NONE',  ( 1.364829396325459854, -0.6046776061558809534, -0.2411417322834644161 ) ) ;
#79299 = CARTESIAN_POINT ( 'NONE',  ( 0.8202099737532814183, -0.6692913385826773087, -0.1292274648535924053 ) ) ;
#79300 = CARTESIAN_POINT ( 'NONE',  ( 0.3392501089628018329, 0.1958661417322835607, -0.5308398950131234528 ) ) ;
#79301 = CARTESIAN_POINT ( 'NONE',  ( -0.04593175853018302557, -0.6692913385826773087, -0.1292274648535924053 ) ) ;
#79302 = CARTESIAN_POINT ( 'NONE',  ( 0.6627296587926517768, -0.6692913385826773087, -0.1292274648535924053 ) ) ;
#79303 = CARTESIAN_POINT ( 'NONE',  ( -0.006561679790025524116, -0.05778040916215560624, -0.4822834645669293319 ) ) ;
#79304 = CARTESIAN_POINT ( 'NONE',  ( 0.6430446194225729606, -0.3690944881889765550, -0.3153832671262227771 ) ) ;
#79305 = CARTESIAN_POINT ( 'NONE',  ( -1.509186351706035767, 0.05413385826771626580, -0.4176697321401330321 ) ) ;
#79306 = CARTESIAN_POINT ( 'NONE',  ( -1.463254593175852492, -0.6692913385826773087, -0.1292274648535924053 ) ) ;
#79307 = CARTESIAN_POINT ( 'NONE',  ( 0.6167979002624678353, -0.4281496062992124485, 0.4176697321401328655 ) ) ;
#79308 = CARTESIAN_POINT ( 'NONE',  ( -1.157146581871515012E-16, 0.4724409448818898682, -0.5492125984251968740 ) ) ;
#79309 = CARTESIAN_POINT ( 'NONE',  ( -0.1049643490035302024, -0.3917322834645671215, -2.269028871391075786 ) ) ;
#79310 = ORIENTED_EDGE ( 'NONE', *, *, #8336, .T. ) ;
#79311 = CARTESIAN_POINT ( 'NONE',  ( -0.3460692066303960868, 0.1998031496062990242, -0.4986876640419947715 ) ) ;
#79312 = ORIENTED_EDGE ( 'NONE', *, *, #41641, .T. ) ;
#79313 = CARTESIAN_POINT ( 'NONE',  ( 1.108923884514436686, -0.3162353388693409650, -0.4822834645669289433 ) ) ;
#79314 = CARTESIAN_POINT ( 'NONE',  ( 0.6627296587926515548, 0.1771653543307087630, 0.09757992244046791164 ) ) ;
#79315 = CARTESIAN_POINT ( 'NONE',  ( 3.264097702071373064, 2.755905511811024056, -0.5314960629921260393 ) ) ;
#79316 = CARTESIAN_POINT ( 'NONE',  ( -0.8561328129276786214, -2.191421614605370878E-15, 0.4445507791589071167 ) ) ;
#79317 = CARTESIAN_POINT ( 'NONE',  ( 1.614173228346457378, 1.330640075373405118, 0.1372047244094478369 ) ) ;
#79318 = CARTESIAN_POINT ( 'NONE',  ( 0.2867679344610365999, -0.2867679344610365444, -1.442913385826771755 ) ) ;
#79319 = CARTESIAN_POINT ( 'NONE',  ( -1.561679790026246017, -0.4281496062992127816, -0.4176697321401328100 ) ) ;
#79320 = CARTESIAN_POINT ( 'NONE',  ( -0.2559055118110230564, 0.1660481256975883668, -0.3530559997133364547 ) ) ;
#79321 = CARTESIAN_POINT ( 'NONE',  ( 0.9120734908136489683, -0.6692913385826771977, 0.1292274648535927661 ) ) ;
#79322 = ORIENTED_EDGE ( 'NONE', *, *, #76828, .F. ) ;
#79323 = ADVANCED_FACE ( 'NONE', ( #7634 ), #24495, .F. ) ;
#79324 = CARTESIAN_POINT ( 'NONE',  ( -1.417322834645668772, -0.1870078740157479769, 0.4822834645669291653 ) ) ;
#79325 = CARTESIAN_POINT ( 'NONE',  ( -1.171093442848938793, -2.191421614605370878E-15, 0.4445507791589071167 ) ) ;
#79326 = DIRECTION ( 'NONE',  ( 0.000000000000000000, -0.000000000000000000, 1.000000000000000000 ) ) ;
#79327 = DIRECTION ( 'NONE',  ( 0.000000000000000000, -1.734723475976808327E-16, 1.000000000000000000 ) ) ;
#79328 = CARTESIAN_POINT ( 'NONE',  ( -1.194225721784776262, -0.3690944881889763329, 0.3153832671262228327 ) ) ;
#79329 = CARTESIAN_POINT ( 'NONE',  ( -1.607611548556429737, 0.2952755905511810774, -0.1292274648535930714 ) ) ;
#79330 = CARTESIAN_POINT ( 'NONE',  ( 0.2624671916010504757, 0.2306618581243848609, 0.2411417322834645549 ) ) ;
#79331 = ORIENTED_EDGE ( 'NONE', *, *, #61119, .T. ) ;
#79333 = CARTESIAN_POINT ( 'NONE',  ( -0.4396325459317579343, 0.2066929133858267931, 0.1054918080437490802 ) ) ;
#79332 = CARTESIAN_POINT ( 'NONE',  ( 1.633858267716535639, -0.5400638737290844871, 0.3530559997133364547 ) ) ;
#79334 = CARTESIAN_POINT ( 'NONE',  ( -0.8792650918635160906, -0.004921259842519870586, -0.3153832671262229437 ) ) ;
#79335 = CARTESIAN_POINT ( 'NONE',  ( 0.7152230971128616943, -0.05778040916215522460, 0.4822834645669289988 ) ) ;
#79336 = CARTESIAN_POINT ( 'NONE',  ( 1.351706036745407458, -0.3690944881889765550, -0.3153832671262227771 ) ) ;
#79337 = CARTESIAN_POINT ( 'NONE',  ( -0.1958661417322834497, -0.3392501089628018884, -1.248012180281152794 ) ) ;
#79338 = CARTESIAN_POINT ( 'NONE',  ( -0.7152230971128602510, -0.08942795157528024563, -0.3641732283464568787 ) ) ;
#79339 = CARTESIAN_POINT ( 'NONE',  ( -1.482939632545930975, -0.004921259842519576551, 0.3153832671262227771 ) ) ;
#79340 = DIRECTION ( 'NONE',  ( 0.7071067811865474617, 8.659560562354932858E-17, 0.7071067811865474617 ) ) ;
#79341 = CARTESIAN_POINT ( 'NONE',  ( 0.5446194225721792126, -0.05778040916215560624, -0.4822834645669293319 ) ) ;
#79342 = CARTESIAN_POINT ( 'NONE',  ( -1.003937007874014853, 0.07958543189024085140, 0.2665933059059887866 ) ) ;
#79343 = CARTESIAN_POINT ( 'NONE',  ( -0.4002624671916004129, -0.08942795157528024563, -0.3641732283464568787 ) ) ;
#79344 = CARTESIAN_POINT ( 'NONE',  ( -0.3018372703412066094, 0.05413385826771666132, 0.4176697321401328100 ) ) ;
#79345 = CARTESIAN_POINT ( 'NONE',  ( -1.522309711286088607, -0.5023911411419708095, 0.1820866141732285504 ) ) ;
#79346 = CARTESIAN_POINT ( 'NONE',  ( -0.3917322834645670659, -7.196005306013484475E-17, 0.1213717603336463974 ) ) ;
#79347 = CARTESIAN_POINT ( 'NONE',  ( 0.5380577427821529035, 0.05413385826771626580, -0.4176697321401330321 ) ) ;
#79348 = SHAPE_REPRESENTATION ( 'MAS-416', ( #66511, #15446, #30192, #11409, #75935, #24836, #69201, #43631, #54405, #4661, #6042, #82658, #18137, #22161, #32909, #63832, #38301, #10093, #35619, #71911, #55784 ), #67889 ) ;
#79349 = EDGE_CURVE ( 'NONE', #37370, #51716, #66391, .T. ) ;
#79350 = CARTESIAN_POINT ( 'NONE',  ( -0.1265901696524986964, -0.4724409448818899238, -0.2296587926509186250 ) ) ;
#79351 = CARTESIAN_POINT ( 'NONE',  ( 0.2362204724409451007, -0.4091458600556402980, -1.585958005249344049 ) ) ;
#79352 = CARTESIAN_POINT ( 'NONE',  ( -0.6364829396325453192, -0.3162353388693405765, 0.4822834645669290543 ) ) ;
#79353 = CARTESIAN_POINT ( 'NONE',  ( -0.1443569553805768291, -0.004921259842519576551, 0.3153832671262227771 ) ) ;
#79354 = CARTESIAN_POINT ( 'NONE',  ( -1.253280839895012377, -0.3162353388693409650, -0.4822834645669289433 ) ) ;
#79355 = CARTESIAN_POINT ( 'NONE',  ( 0.6167979002624679463, -0.004921259842519870586, -0.3153832671262229437 ) ) ;
#79356 = CARTESIAN_POINT ( 'NONE',  ( -0.7349081364829390672, 0.1283753931104746893, -0.1820866141732285504 ) ) ;
#79357 = CARTESIAN_POINT ( 'NONE',  ( -1.266404199475064773, -0.3162353388693405765, 0.4822834645669290543 ) ) ;
#79358 = CARTESIAN_POINT ( 'NONE',  ( -1.732283464566928277, -0.1870078740157479769, 0.4822834645669291653 ) ) ;
#79359 = CARTESIAN_POINT ( 'NONE',  ( 1.240157480314961314, 0.1660481256975883668, -0.3530559997133364547 ) ) ;
#79360 = CARTESIAN_POINT ( 'NONE',  ( -0.6575345472713096662, 1.929133858267489954, 0.5309055118110236338 ) ) ;
#79361 = CARTESIAN_POINT ( 'NONE',  ( 1.003937007874016407, -0.4536011799217367080, 0.2665933059059888421 ) ) ;
#79362 = CARTESIAN_POINT ( 'NONE',  ( 0.2624671916010504757, 0.2306618581243848609, 0.2411417322834645549 ) ) ;
#79363 = CARTESIAN_POINT ( 'NONE',  ( -1.581364829396324945, -0.05778040916215560624, -0.4822834645669293319 ) ) ;
#79364 = CARTESIAN_POINT ( 'NONE',  ( 1.220472440944882386, -0.5511811023622047445, 6.969142054262312111E-17 ) ) ;
#79365 = ORIENTED_EDGE ( 'NONE', *, *, #68902, .F. ) ;
#79366 = CARTESIAN_POINT ( 'NONE',  ( -0.2925321140481932369, 0.2925321140481931259, -2.773622047244094002 ) ) ;
#79367 = CARTESIAN_POINT ( 'NONE',  ( -1.345144356955379816, -0.2845877964562159024, 0.3641732283464567677 ) ) ;
#79368 = CARTESIAN_POINT ( 'NONE',  ( -0.3346456692913377662, 0.1660481256975883668, -0.3530559997133364547 ) ) ;
#79369 = CARTESIAN_POINT ( 'NONE',  ( 0.1837270341207354329, 0.2306618581243848609, 0.2411417322834645549 ) ) ;
#79370 = CARTESIAN_POINT ( 'NONE',  ( -1.601049868766403650, -0.5023911411419708095, 0.1820866141732285504 ) ) ;
#79371 = CARTESIAN_POINT ( 'NONE',  ( -0.3996062992125985480, -7.340648628747423112E-17, -1.848425196850393748 ) ) ;
#79372 = CARTESIAN_POINT ( 'NONE',  ( -1.456692913385826182, -0.6692913385826771977, 8.415575281601705876E-17 ) ) ;
#79373 = CARTESIAN_POINT ( 'NONE',  ( 0.3149606299212606708, -0.1870078740157480879, -0.4822834645669291653 ) ) ;
#79374 = CARTESIAN_POINT ( 'NONE',  ( -0.05249343832020911260, 0.2306618581243848609, 0.2411417322834645549 ) ) ;
#79375 = CARTESIAN_POINT ( 'NONE',  ( 1.286089238845145033, 0.2306618581243848609, 0.2411417322834645549 ) ) ;
#79376 = CARTESIAN_POINT ( 'NONE',  ( -0.3460692066303960313, 0.1998031496062989965, -0.8904199475065617264 ) ) ;
#79377 = CARTESIAN_POINT ( 'NONE',  ( 0.1070741851644054915, -0.3996062992125986035, -1.187664041994750619 ) ) ;
#79378 = CARTESIAN_POINT ( 'NONE',  ( -0.3949938075777411628, 0.1058382717557497937, -1.135170603674540812 ) ) ;
#79379 = CARTESIAN_POINT ( 'NONE',  ( -0.2925321140481932924, 0.2925321140481931814, -2.539370078740157410 ) ) ;
#79380 = CARTESIAN_POINT ( 'NONE',  ( 0.3917322834645669549, 0.1049643490035304660, -0.2742782152230970327 ) ) ;
#79381 = CARTESIAN_POINT ( 'NONE',  ( -0.03280839895013062252, -0.5511811023622046335, 0.09757992244046803654 ) ) ;
#79382 = CARTESIAN_POINT ( 'NONE',  ( -0.4790026246719154557, -0.3162353388693405765, 0.4822834645669290543 ) ) ;
#79383 = CARTESIAN_POINT ( 'NONE',  ( 0.9317585301837276734, -0.4281496062992124485, 0.4176697321401328655 ) ) ;
#79384 = CARTESIAN_POINT ( 'NONE',  ( 0.3949938075777409408, -0.1058382717557499186, -1.605643044619423199 ) ) ;
#79385 = CARTESIAN_POINT ( 'NONE',  ( 0.1640419947506569498, -0.2845877964562161244, -0.3641732283464567121 ) ) ;
#79386 = CARTESIAN_POINT ( 'NONE',  ( -1.253280839895012377, -0.3162353388693409650, -0.4822834645669289433 ) ) ;
#79387 = CARTESIAN_POINT ( 'NONE',  ( 1.541994750656168645, -0.6692913385826771977, 0.1292274648535927661 ) ) ;
#79388 = CARTESIAN_POINT ( 'NONE',  ( -0.4091458600556405756, 0.2362204724409446288, -2.230971128608923770 ) ) ;
#79389 = LINE ( 'NONE', #33513, #77479 ) ;
#79390 = ORIENTED_EDGE ( 'NONE', *, *, #2734, .T. ) ;
#79391 = EDGE_LOOP ( 'NONE', ( #22148, #44129, #50695, #7396, #77720, #40858, #5448 ) ) ;
#79392 = CARTESIAN_POINT ( 'NONE',  ( 1.161417322834646271, 0.1660481256975883668, -0.3530559997133364547 ) ) ;
#79393 = CARTESIAN_POINT ( 'NONE',  ( 1.450131233595801428, 0.1771653543307087630, 0.09757992244046791164 ) ) ;
#79395 = CARTESIAN_POINT ( 'NONE',  ( -1.082677165354329896, -0.5400638737290845981, -0.3530559997133363437 ) ) ;
#79394 = CARTESIAN_POINT ( 'NONE',  ( -1.056430446194224881, -0.5511811023622046335, 0.09757992244046803654 ) ) ;
#79396 = CARTESIAN_POINT ( 'NONE',  ( 0.2867679344610365999, 0.2867679344610365999, -2.265072547735221153 ) ) ;
#79397 = DIRECTION ( 'NONE',  ( 0.000000000000000000, 0.000000000000000000, 1.000000000000000000 ) ) ;
#79398 = CARTESIAN_POINT ( 'NONE',  ( 1.410761154855643795, -0.05778040916215560624, -0.4822834645669293319 ) ) ;
#79399 = CARTESIAN_POINT ( 'NONE',  ( -1.620734908136482577, -0.6692913385826773087, -0.1292274648535924053 ) ) ;
#79400 = CARTESIAN_POINT ( 'NONE',  ( 0.1115485564304467270, -0.6692913385826773087, -0.1292274648535924053 ) ) ;
#79401 = CARTESIAN_POINT ( 'NONE',  ( -0.2099737532808391705, -0.6046776061558809534, -0.2411417322834644161 ) ) ;
#79402 = AXIS2_PLACEMENT_3D ( 'NONE', #31446, #44473, #70164 ) ;
#79403 = CARTESIAN_POINT ( 'NONE',  ( -1.148293963254592542, 0.2952755905511811885, 0.1292274648535926551 ) ) ;
#79404 = CARTESIAN_POINT ( 'NONE',  ( -0.1958661417322836440, 0.3392501089628016664, -2.770321891567242734 ) ) ;
#79405 = CARTESIAN_POINT ( 'NONE',  ( 0.5511811023622054106, -0.1870078740157480879, -0.4822834645669291653 ) ) ;
#79406 = CARTESIAN_POINT ( 'NONE',  ( 0.2867679344610365999, 0.2867679344610365999, -1.862204724409449064 ) ) ;
#79407 = CARTESIAN_POINT ( 'NONE',  ( -1.338582677165353729, -0.1870078740157479769, 0.3641732283464567677 ) ) ;
#79408 = ORIENTED_EDGE ( 'NONE', *, *, #58809, .F. ) ;
#79409 = CARTESIAN_POINT ( 'NONE',  ( -0.1058382717557503211, 0.3949938075777409408, -2.368766404199475595 ) ) ;
#79410 = VERTEX_POINT ( 'NONE', #38587 ) ;
#79411 = CARTESIAN_POINT ( 'NONE',  ( -1.568139075118781589, 1.385950145841912118, 0.4495859454777829112 ) ) ;
#79412 = CARTESIAN_POINT ( 'NONE',  ( -1.384514435695537005, 0.2952755905511811885, 0.1292274648535926551 ) ) ;
#79413 = CARTESIAN_POINT ( 'NONE',  ( -1.128608923884513837, 0.2306618581243847221, -0.2411417322834647770 ) ) ;
#79414 = CARTESIAN_POINT ( 'NONE',  ( 0.1998031496062994405, -0.3460692066303958092, -0.7217847769028871152 ) ) ;
#79415 = CARTESIAN_POINT ( 'NONE',  ( -1.397637795275589623, 0.1660481256975885056, 0.3530559997133364547 ) ) ;
#79416 = CARTESIAN_POINT ( 'NONE',  ( -1.476377952755905110, -0.5400638737290845981, -0.3530559997133363437 ) ) ;
#79417 = CARTESIAN_POINT ( 'NONE',  ( 0.1011035889004530536, -0.3790285851608820034, -2.755905511811024944 ) ) ;
#79418 = CARTESIAN_POINT ( 'NONE',  ( 0.3917322834645670104, 2.398668435337828261E-17, -0.04527559055118119541 ) ) ;
#79419 = CARTESIAN_POINT ( 'NONE',  ( -0.3674540682414689785, 0.1283753931104748280, 0.1820866141732283561 ) ) ;
#79420 = CARTESIAN_POINT ( 'NONE',  ( -0.8661417322834640276, -0.1870078740157480601, -0.3641732283464567677 ) ) ;
#79421 = CARTESIAN_POINT ( 'NONE',  ( -1.135170603674539924, 0.2952755905511810774, -0.1292274648535930714 ) ) ;
#79422 = CARTESIAN_POINT ( 'NONE',  ( 0.7677165354330716118, -0.5400638737290844871, 0.3530559997133364547 ) ) ;
#79423 = CARTESIAN_POINT ( 'NONE',  ( -0.9251968503937002541, -0.5400638737290845981, -0.3530559997133363437 ) ) ;
#79424 = CARTESIAN_POINT ( 'NONE',  ( -0.3392501089628019995, 0.1958661417322832277, -0.01837270341207344546 ) ) ;
#79425 = EDGE_LOOP ( 'NONE', ( #19558, #3624, #51114, #67499 ) ) ;
#79426 = ADVANCED_FACE ( 'NONE', ( #58783 ), #76894, .F. ) ;
#79427 = CARTESIAN_POINT ( 'NONE',  ( -1.332020997375327642, -0.05778040916215522460, 0.4822834645669289988 ) ) ;
#79428 = CARTESIAN_POINT ( 'NONE',  ( -1.377952755905511140, 0.1771653543307087630, 0.000000000000000000 ) ) ;
#79429 = CARTESIAN_POINT ( 'NONE',  ( -1.679790026246718693, 0.2306618581243847221, -0.2411417322834647770 ) ) ;
#79430 = CARTESIAN_POINT ( 'NONE',  ( 0.4724409448818898682, 2.892866454678787531E-17, -1.377952755905511806 ) ) ;
#79431 = CARTESIAN_POINT ( 'NONE',  ( 2.139067083128515900, 1.422987107291906694, -0.4606739315415588898 ) ) ;
#79432 = EDGE_CURVE ( 'NONE', #14187, #5989, #31857, .T. ) ;
#79433 = CARTESIAN_POINT ( 'NONE',  ( 0.1049643490035303689, 0.3917322834645670104, -0.6154855643044617741 ) ) ;
#79434 = CARTESIAN_POINT ( 'NONE',  ( -9.594673741351313045E-17, 0.3917322834645670104, -2.446850393700787496 ) ) ;
#79435 = CARTESIAN_POINT ( 'NONE',  ( -0.4002624671916004129, -0.3162353388693405765, 0.4822834645669290543 ) ) ;
#79436 = CARTESIAN_POINT ( 'NONE',  ( -1.345144356955379816, -0.2845877964562159024, 0.3641732283464567677 ) ) ;
#79437 = CARTESIAN_POINT ( 'NONE',  ( -0.1998031496062994405, 0.3460692066303957537, -0.08989501312335959615 ) ) ;
#79439 = CARTESIAN_POINT ( 'NONE',  ( 0.000000000000000000, 0.000000000000000000, 0.000000000000000000 ) ) ;
#79438 = DIRECTION ( 'NONE',  ( 2.956072690630991733E-16, -1.000000000000000000, -5.002896285981958034E-32 ) ) ;
#79440 = CARTESIAN_POINT ( 'NONE',  ( -1.627296587926508442, -0.6046776061558809534, -0.2411417322834644161 ) ) ;
#79441 = CARTESIAN_POINT ( 'NONE',  ( -0.2952755905511804668, 0.1660481256975885056, 0.3530559997133364547 ) ) ;
#79442 = CARTESIAN_POINT ( 'NONE',  ( 0.1958661417322834497, 0.3392501089628018329, -0.06690981807642862322 ) ) ;
#79443 = CARTESIAN_POINT ( 'NONE',  ( 0.6167979002624678353, -0.3690944881889763329, 0.3153832671262228327 ) ) ;
#79444 = CARTESIAN_POINT ( 'NONE',  ( -0.1958661417322834220, -0.3392501089628018884, -0.1502624671916011345 ) ) ;
#79445 = CARTESIAN_POINT ( 'NONE',  ( 0.2821522309711292364, 0.1771653543307087075, -0.09757992244046823083 ) ) ;
#79446 = CARTESIAN_POINT ( 'NONE',  ( 0.7939632545931766261, -0.08942795157527998196, 0.3641732283464567121 ) ) ;
#79447 = CARTESIAN_POINT ( 'NONE',  ( 0.8136482939632553313, 0.2306618581243848609, 0.2411417322834645549 ) ) ;
#79448 = CARTESIAN_POINT ( 'NONE',  ( -0.1377952755905504645, -0.4536011799217368745, -0.2665933059059886201 ) ) ;
#79449 = CARTESIAN_POINT ( 'NONE',  ( -0.1049643490035302024, -0.3917322834645671215, -2.111548556430446144 ) ) ;
#79450 = CARTESIAN_POINT ( 'NONE',  ( -1.207349081364828436, -0.6046776061558807314, 0.2411417322834647770 ) ) ;
#79451 = CARTESIAN_POINT ( 'NONE',  ( 0.1115485564304467270, -0.5511811023622048555, -0.09757992244046775898 ) ) ;
#79452 = EDGE_CURVE ( 'NONE', #39742, #80735, #13343, .T. ) ;
#79453 = CARTESIAN_POINT ( 'NONE',  ( -1.332020997375327642, -0.08942795157527998196, 0.3641732283464567121 ) ) ;
#79454 = CARTESIAN_POINT ( 'NONE',  ( 0.4724409448818896462, 0.1265901696524990294, -0.5164041994750655507 ) ) ;
#79455 = CARTESIAN_POINT ( 'NONE',  ( -1.049868766404198794, -0.5023911411419708095, 0.1820866141732285504 ) ) ;
#79456 = EDGE_CURVE ( 'NONE', #57006, #41276, #78159, .T. ) ;
#79457 = DIRECTION ( 'NONE',  ( -0.000000000000000000, 1.000000000000000000, -0.000000000000000000 ) ) ;
#79458 = CARTESIAN_POINT ( 'NONE',  ( -0.06561679790026180015, 0.05413385826771666132, 0.4176697321401328100 ) ) ;
#79459 = FACE_BOUND ( 'NONE', #69943, .T. ) ;
#79460 = CARTESIAN_POINT ( 'NONE',  ( 0.5511811023622054106, -0.1870078740157480601, -0.3641732283464567677 ) ) ;
#79461 = CARTESIAN_POINT ( 'NONE',  ( -0.4330708661417315697, 0.1771653543307087630, 0.000000000000000000 ) ) ;
#79462 = CARTESIAN_POINT ( 'NONE',  ( -0.8727034120734901146, -0.3162353388693405765, 0.4822834645669290543 ) ) ;
#79463 = CYLINDRICAL_SURFACE ( 'NONE', #34468, 0.4724409448818898682 ) ;
#79464 = CARTESIAN_POINT ( 'NONE',  ( -0.9448818897637790704, -0.1870078740157480601, -0.3641732283464567677 ) ) ;
#79465 = CARTESIAN_POINT ( 'NONE',  ( 0.4724409448818898682, 0.000000000000000000, 0.000000000000000000 ) ) ;
#79466 = CARTESIAN_POINT ( 'NONE',  ( 0.3805774278215230400, -0.4281496062992124485, 0.4176697321401328655 ) ) ;
#79467 = AXIS2_PLACEMENT_3D ( 'NONE', #54126, #73931, #16274 ) ;
#79468 = CARTESIAN_POINT ( 'NONE',  ( 0.1070741851644054776, -0.3996062992125984925, -1.579396325459317296 ) ) ;
#79469 = CARTESIAN_POINT ( 'NONE',  ( -1.595398199321656607, 1.309738123151862998, -0.1559797534342480529 ) ) ;
#79470 = CARTESIAN_POINT ( 'NONE',  ( -0.2952755905511804668, 0.07958543189024085140, 0.2665933059059887866 ) ) ;
#79471 = CARTESIAN_POINT ( 'NONE',  ( -0.07217847769028813698, -0.3162353388693409650, -0.4822834645669289433 ) ) ;
#79472 = CARTESIAN_POINT ( 'NONE',  ( -1.515748031496062076, -0.5400638737290844871, 0.3530559997133364547 ) ) ;
#79473 = CARTESIAN_POINT ( 'NONE',  ( -1.568241469816272105, -0.2845877964562161244, -0.3641732283464567121 ) ) ;
#79474 = CARTESIAN_POINT ( 'NONE',  ( 1.240157480314961314, 0.1660481256975883668, -0.3530559997133364547 ) ) ;
#79475 = CARTESIAN_POINT ( 'NONE',  ( -0.6102362204724400829, 0.07958543189024085140, 0.2665933059059887866 ) ) ;
#79476 = CARTESIAN_POINT ( 'NONE',  ( -0.7749820319012115100, 0.000000000000000000, 0.3464511005275205946 ) ) ;
#79477 = CARTESIAN_POINT ( 'NONE',  ( 0.1070741851644053527, 0.3996062992125986590, -0.1509186351706036655 ) ) ;
#79478 = CARTESIAN_POINT ( 'NONE',  ( -0.2867679344610365444, -0.2867679344610367664, -2.417998318406511249 ) ) ;
#79479 = EDGE_CURVE ( 'NONE', #11346, #47146, #25531, .T. ) ;
#79480 = VECTOR ( 'NONE', #4660, 39.37007874015748143 ) ;
#79481 = LINE ( 'NONE', #1622, #67382 ) ;
#79482 = CARTESIAN_POINT ( 'NONE',  ( 0.9580052493438326877, -0.004921259842519576551, 0.3153832671262227771 ) ) ;
#79483 = CARTESIAN_POINT ( 'NONE',  ( -1.620734908136482577, -0.6692913385826773087, -0.1292274648535924053 ) ) ;
#79484 = CARTESIAN_POINT ( 'NONE',  ( 0.8464566929133865436, 0.1660481256975883668, -0.3530559997133364547 ) ) ;
#79485 = CARTESIAN_POINT ( 'NONE',  ( 0.2867679344610365999, 0.2867679344610365999, -2.584645669291338876 ) ) ;
#79486 = CARTESIAN_POINT ( 'NONE',  ( 1.371391076115485941, 0.1771653543307087630, 0.09757992244046791164 ) ) ;
#79487 = CARTESIAN_POINT ( 'NONE',  ( 0.2952755905511819101, 0.1660481256975883668, -0.3530559997133364547 ) ) ;
#79488 = CARTESIAN_POINT ( 'NONE',  ( -0.5380577427821514602, 0.05413385826771666132, 0.4176697321401328100 ) ) ;
#79489 = CARTESIAN_POINT ( 'NONE',  ( 1.601049868766404982, -0.6046776061558809534, -0.2411417322834644161 ) ) ;
#79490 = CARTESIAN_POINT ( 'NONE',  ( 0.4724409448818897572, -0.1265901696524988906, -0.8989501312335956840 ) ) ;
#79491 = CARTESIAN_POINT ( 'NONE',  ( -0.3996062992125986590, 0.1070741851644051862, -2.080052493438320216 ) ) ;
#79492 = CARTESIAN_POINT ( 'NONE',  ( 0.5380577427821529035, -0.004921259842519870586, -0.3153832671262229437 ) ) ;
#79493 = ORIENTED_EDGE ( 'NONE', *, *, #45942, .T. ) ;
#79494 = CARTESIAN_POINT ( 'NONE',  ( -0.1049643490035307158, 0.3917322834645670104, -0.1607804706374822146 ) ) ;
#79495 = ORIENTED_EDGE ( 'NONE', *, *, #10296, .F. ) ;
#79496 = CARTESIAN_POINT ( 'NONE',  ( -0.5708661417322828946, 0.1660481256975883668, -0.3530559997133364547 ) ) ;
#79497 = CARTESIAN_POINT ( 'NONE',  ( 1.181102362204724976, -0.1870078740157480879, -0.4822834645669291653 ) ) ;
#79498 = CARTESIAN_POINT ( 'NONE',  ( 0.05249343832021075018, -0.6046776061558807314, 0.2411417322834647770 ) ) ;
#79499 = CARTESIAN_POINT ( 'NONE',  ( -0.5446194225721777693, -0.08942795157527998196, 0.3641732283464567121 ) ) ;
#79500 = CARTESIAN_POINT ( 'NONE',  ( 0.7677165354330716118, 0.1660481256975883668, -0.3530559997133364547 ) ) ;
#79501 = CARTESIAN_POINT ( 'NONE',  ( -0.8136482939632537770, 0.2306618581243847221, -0.2411417322834647770 ) ) ;
#79502 = CARTESIAN_POINT ( 'NONE',  ( -0.4396325459317579898, 0.2952755905511811885, 0.1292274648535926551 ) ) ;
#79503 = CARTESIAN_POINT ( 'NONE',  ( -0.7545931758530177724, 0.2952755905511811885, 0.1292274648535926551 ) ) ;
#79504 = CARTESIAN_POINT ( 'NONE',  ( 1.227034120734908917, -0.6692913385826771977, 0.1292274648535927661 ) ) ;
#79505 = CARTESIAN_POINT ( 'NONE',  ( 0.8595800524934390507, -0.05778040916215560624, -0.4822834645669293319 ) ) ;
#79506 = EDGE_CURVE ( 'NONE', #71072, #75665, #9292, .T. ) ;
#79507 = CARTESIAN_POINT ( 'NONE',  ( 0.9055118110236227702, 0.2952755905511811885, 0.000000000000000000 ) ) ;
#79508 = CARTESIAN_POINT ( 'NONE',  ( 0.3917322834645670104, -0.1049643490035303411, -0.4186351706036745557 ) ) ;
#79509 = CARTESIAN_POINT ( 'NONE',  ( 0.1246719160104994284, 0.1771653543307087075, -0.09757992244046823083 ) ) ;
#79510 = ORIENTED_EDGE ( 'NONE', *, *, #8432, .T. ) ;
#79511 = CARTESIAN_POINT ( 'NONE',  ( -0.1974969037888703871, -0.3420746716998661063, -1.167979002624671914 ) ) ;
#79512 = ORIENTED_EDGE ( 'NONE', *, *, #37312, .T. ) ;
#79513 = CARTESIAN_POINT ( 'NONE',  ( -0.8333333333333323711, -0.5511811023622048555, -0.09757992244046775898 ) ) ;
#79514 = ADVANCED_BREP_SHAPE_REPRESENTATION ( '', ( #33697, #22098 ), #5981 ) ;
#79515 = CARTESIAN_POINT ( 'NONE',  ( -0.09842519685039295696, -0.5400638737290844871, 0.3530559997133364547 ) ) ;
#79516 = CARTESIAN_POINT ( 'NONE',  ( -1.614173228346456712, 0.000000000000000000, -0.1372047244094478091 ) ) ;
#79517 = CARTESIAN_POINT ( 'NONE',  ( -0.4068241469816267775, 0.05413385826771626580, -0.4176697321401330321 ) ) ;
#79518 = CARTESIAN_POINT ( 'NONE',  ( -0.5446194225721777693, -0.3162353388693409650, -0.4822834645669289433 ) ) ;
#79519 = CARTESIAN_POINT ( 'NONE',  ( -1.404199475065615932, -0.4281496062992127816, -0.4176697321401328100 ) ) ;
#79520 = CARTESIAN_POINT ( 'NONE',  ( -1.227034120734907585, 0.2952755905511811885, 0.1292274648535926551 ) ) ;
#79521 = CARTESIAN_POINT ( 'NONE',  ( 1.384514435695538559, 0.1771653543307087075, -0.09757992244046823083 ) ) ;
#79522 = CARTESIAN_POINT ( 'NONE',  ( 0.3458507752293908943, -0.3458507752293908943, -1.043307086614173151 ) ) ;
#79523 = CARTESIAN_POINT ( 'NONE',  ( 0.2405540237485361554, 0.1712599301372657035, 5.748856329247439945 ) ) ;
#79524 = CARTESIAN_POINT ( 'NONE',  ( 0.4658792650918640033, -0.2845877964562159024, 0.3641732283464567677 ) ) ;
#79525 = CARTESIAN_POINT ( 'NONE',  ( 0.2493438320209980519, 0.05413385826771666132, 0.4176697321401328100 ) ) ;
#79526 = CARTESIAN_POINT ( 'NONE',  ( 0.3937007874015754361, -0.1870078740157479769, 0.4822834645669291653 ) ) ;
#79527 = ORIENTED_EDGE ( 'NONE', *, *, #76941, .T. ) ;
#79528 = AXIS2_PLACEMENT_3D ( 'NONE', #15441, #66790, #2806 ) ;
#79529 = CARTESIAN_POINT ( 'NONE',  ( 0.3996062992125986590, -0.1070741851644053111, -1.528871391076114916 ) ) ;
#79530 = CARTESIAN_POINT ( 'NONE',  ( -0.9348729704079935532, -2.191421614605370878E-15, 0.4445507791589071167 ) ) ;
#79531 = ORIENTED_EDGE ( 'NONE', *, *, #25250, .F. ) ;
#79532 = CARTESIAN_POINT ( 'NONE',  ( -0.3460692066303957537, -0.1998031496062994405, -1.074146981627296604 ) ) ;
#79533 = CARTESIAN_POINT ( 'NONE',  ( 0.3460692066303958092, 0.1998031496062993018, -0.5229658792650918597 ) ) ;
#79534 = CARTESIAN_POINT ( 'NONE',  ( -0.4133858267716528645, 0.1660481256975883668, -0.3530559997133364547 ) ) ;
#79535 = CARTESIAN_POINT ( 'NONE',  ( 5.785732909357575061E-17, -0.4724409448818898682, 0.07874015748031495954 ) ) ;
#79536 = EDGE_CURVE ( 'NONE', #40470, #32861, #64423, .T. ) ;
#79537 = CARTESIAN_POINT ( 'NONE',  ( 0.3392501089628018329, 0.1958661417322835607, -2.420603674540682260 ) ) ;
#79538 = CARTESIAN_POINT ( 'NONE',  ( -1.437007874015747477, 0.07958543189024071263, -0.2665933059059888421 ) ) ;
#79539 = CARTESIAN_POINT ( 'NONE',  ( 0.9186351706036751663, -0.6046776061558807314, 0.2411417322834647770 ) ) ;
#79540 = CARTESIAN_POINT ( 'NONE',  ( 0.7414698162729663755, 0.2952755905511811885, 0.1292274648535926551 ) ) ;
#79541 = CARTESIAN_POINT ( 'NONE',  ( -0.1968503937007867743, 0.1771653543307087630, 0.000000000000000000 ) ) ;
#79542 = CARTESIAN_POINT ( 'NONE',  ( 0.1181102362204730916, -0.6692913385826771977, 8.415575281601705876E-17 ) ) ;
#79543 = CARTESIAN_POINT ( 'NONE',  ( 0.2362204724409449064, 0.4091458600556404646, -1.953412073490813805 ) ) ;
#79544 = CARTESIAN_POINT ( 'NONE',  ( 0.006561679790026889343, -0.2845877964562161244, -0.3641732283464567121 ) ) ;
#79545 = CARTESIAN_POINT ( 'NONE',  ( -0.5380577427821514602, -0.4281496062992127816, -0.4176697321401328100 ) ) ;
#79546 = CARTESIAN_POINT ( 'NONE',  ( 0.3949938075777409963, 2.418639510665530743E-17, -1.769685039370078927 ) ) ;
#79547 = CARTESIAN_POINT ( 'NONE',  ( -1.555118110236219930, 0.1660481256975885056, 0.3530559997133364547 ) ) ;
#79548 = CARTESIAN_POINT ( 'NONE',  ( 0.01312335958005323398, -0.004921259842519576551, 0.3153832671262227771 ) ) ;
#79549 = CARTESIAN_POINT ( 'NONE',  ( 0.9548908091195654757, -4.927456884911482678E-16, 0.4445507791589062840 ) ) ;
#79550 = CARTESIAN_POINT ( 'NONE',  ( -1.161417322834644716, -0.5400638737290845981, -0.3530559997133363437 ) ) ;
#79551 = CARTESIAN_POINT ( 'NONE',  ( -0.7480314960629914633, -0.5511811023622047445, 6.969142054262312111E-17 ) ) ;
#79552 = DIRECTION ( 'NONE',  ( 0.000000000000000000, 0.000000000000000000, 1.000000000000000000 ) ) ;
#79553 = CARTESIAN_POINT ( 'NONE',  ( -1.010498687664041384, -0.4281496062992127816, -0.4176697321401328100 ) ) ;
#79554 = CARTESIAN_POINT ( 'NONE',  ( -0.6167979002624665030, -0.4281496062992127816, -0.4176697321401328100 ) ) ;
#79555 = CARTESIAN_POINT ( 'NONE',  ( 0.1246719160104994284, 0.2952755905511810774, -0.1292274648535930714 ) ) ;
#79556 = CARTESIAN_POINT ( 'NONE',  ( -9.787531504996566615E-17, 0.3996062992125985480, -2.596456692913385655 ) ) ;
#79557 = CARTESIAN_POINT ( 'NONE',  ( 0.1049643490035304522, -0.3917322834645668994, -2.370059424375641211 ) ) ;
#79558 = CARTESIAN_POINT ( 'NONE',  ( 0.5314960629920852941, 2.716724272663528783, 3.890406373195420375 ) ) ;
#79559 = CARTESIAN_POINT ( 'NONE',  ( 0.3608923884514443348, -0.5511811023622046335, 0.09757992244046803654 ) ) ;
#79560 = CARTESIAN_POINT ( 'NONE',  ( 1.174540682414699111, -0.05778040916215560624, -0.4822834645669293319 ) ) ;
#79561 = CARTESIAN_POINT ( 'NONE',  ( -1.377952755905511140, 0.1771653543307087630, 0.000000000000000000 ) ) ;
#79562 = CARTESIAN_POINT ( 'NONE',  ( 1.338582677165355062, -0.1870078740157479769, 0.4822834645669291653 ) ) ;
#79563 = CARTESIAN_POINT ( 'NONE',  ( -1.541994750656167090, 0.1771653543307087630, 0.09757992244046791164 ) ) ;
#79564 = CARTESIAN_POINT ( 'NONE',  ( -0.3937007874015740483, -0.1870078740157480879, -0.4822834645669291653 ) ) ;
#79565 = CARTESIAN_POINT ( 'NONE',  ( 0.3280839895013130669, -0.3690944881889765550, -0.3153832671262227771 ) ) ;
#79566 = DIRECTION ( 'NONE',  ( 0.000000000000000000, 0.000000000000000000, -1.000000000000000000 ) ) ;
#79567 = CARTESIAN_POINT ( 'NONE',  ( 0.5643044619422579178, -0.3690944881889765550, -0.3153832671262227771 ) ) ;
#79568 = CARTESIAN_POINT ( 'NONE',  ( 0.08530183727034192087, -0.05778040916215522460, 0.4822834645669289988 ) ) ;
#79569 = CARTESIAN_POINT ( 'NONE',  ( -0.1998031496062994405, 0.3460692066303957537, -0.4048556430446194621 ) ) ;
#79570 = CARTESIAN_POINT ( 'NONE',  ( -0.6561679790026240244, -0.6046776061558807314, 0.2411417322834647770 ) ) ;
#79571 = CARTESIAN_POINT ( 'NONE',  ( -0.3917322834645669549, -0.1049643490035306603, -2.020341207349081181 ) ) ;
#79572 = CARTESIAN_POINT ( 'NONE',  ( 1.089238845144357537, -0.3690944881889763329, 0.3153832671262228327 ) ) ;
#79573 = CARTESIAN_POINT ( 'NONE',  ( 0.03937007874015833325, -0.6692913385826771977, 8.415575281601705876E-17 ) ) ;
#79574 = CARTESIAN_POINT ( 'NONE',  ( -0.2034120734908128059, 0.2952755905511811885, 0.1292274648535926551 ) ) ;
#79575 = CARTESIAN_POINT ( 'NONE',  ( -0.3083989501312330295, -0.2845877964562161244, -0.3641732283464567121 ) ) ;
#79576 = CARTESIAN_POINT ( 'NONE',  ( 0.9573014326657177664, 0.000000000000000000, 0.3464511005275205946 ) ) ;
#79577 = CARTESIAN_POINT ( 'NONE',  ( -0.6036745406824141069, -0.5023911411419708095, -0.1820866141732282451 ) ) ;
#79578 = CARTESIAN_POINT ( 'NONE',  ( 0.5511811023622055217, -0.1870078740157479769, 0.4822834645669291653 ) ) ;
#79579 = EDGE_CURVE ( 'NONE', #30272, #80363, #78532, .T. ) ;
#79580 = CARTESIAN_POINT ( 'NONE',  ( -0.8333333333333323711, -0.5511811023622048555, -0.09757992244046775898 ) ) ;
#79581 = CARTESIAN_POINT ( 'NONE',  ( -0.3996062992125984925, -0.1070741851644056858, -0.9101049868766404316 ) ) ;
#79582 = CARTESIAN_POINT ( 'NONE',  ( -0.9317585301837263412, -0.4281496062992127816, -0.4176697321401328100 ) ) ;
#79583 = CARTESIAN_POINT ( 'NONE',  ( -0.9881811337016640495, 0.000000000000000000, -0.5314960629921260393 ) ) ;
#79584 = EDGE_LOOP ( 'NONE', ( #2879, #34382, #26589, #67392 ) ) ;
#79585 = EDGE_CURVE ( 'NONE', #7120, #34463, #60032, .T. ) ;
#79586 = CARTESIAN_POINT ( 'NONE',  ( -1.089238845144356427, -0.004921259842519576551, 0.3153832671262227771 ) ) ;
#79587 = AXIS2_PLACEMENT_3D ( 'NONE', #49322, #48491, #56044 ) ;
#79588 = CARTESIAN_POINT ( 'NONE',  ( -0.2099737532808391705, -0.6046776061558809534, -0.2411417322834644161 ) ) ;
#79589 = CARTESIAN_POINT ( 'NONE',  ( -1.725721784776902190, -0.05778040916215522460, 0.4822834645669289988 ) ) ;
#79590 = CARTESIAN_POINT ( 'NONE',  ( -0.7874015748031489847, -0.1870078740157480879, -0.4822834645669291653 ) ) ;
#79591 = DIRECTION ( 'NONE',  ( 0.000000000000000000, -1.000000000000000000, 0.000000000000000000 ) ) ;
#79592 = CARTESIAN_POINT ( 'NONE',  ( 1.364829396325460076, 0.2306618581243848609, 0.2411417322834645549 ) ) ;
#79593 = CARTESIAN_POINT ( 'NONE',  ( 0.7939632545931766261, -0.3162353388693409650, -0.4822834645669289433 ) ) ;
#79594 = CARTESIAN_POINT ( 'NONE',  ( -0.1958661417322834220, -0.3392501089628018884, -2.734908136482939511 ) ) ;
#79595 = CARTESIAN_POINT ( 'NONE',  ( -1.586052503253847501, 1.299212598425198095, 0.1653254495020568260 ) ) ;
#79596 = CARTESIAN_POINT ( 'NONE',  ( 0.2943720246490709180, -0.02382778696830936682, 5.526312367533045666 ) ) ;
#79597 = CARTESIAN_POINT ( 'NONE',  ( -1.646981627296586703, -0.3162353388693409650, -0.4822834645669289433 ) ) ;
#79598 = CARTESIAN_POINT ( 'NONE',  ( 0.2925321140481932369, 0.2925321140481932369, -0.4527559055118109965 ) ) ;
#79599 = ORIENTED_EDGE ( 'NONE', *, *, #38721, .F. ) ;
#79600 = CARTESIAN_POINT ( 'NONE',  ( -0.5839895013123351797, -0.5511811023622046335, 0.09757992244046803654 ) ) ;
#79601 = CARTESIAN_POINT ( 'NONE',  ( 0.1049643490035304938, -0.3917322834645669549, -2.124671916010498762 ) ) ;
#79602 = ORIENTED_EDGE ( 'NONE', *, *, #41314, .T. ) ;
#79603 = CARTESIAN_POINT ( 'NONE',  ( 0.8398950131233602345, 0.2306618581243847221, -0.2411417322834647770 ) ) ;
#79604 = CARTESIAN_POINT ( 'NONE',  ( 0.1706036745406830368, 0.05413385826771666132, 0.4176697321401328100 ) ) ;
#79605 = CARTESIAN_POINT ( 'NONE',  ( -0.5577427821522301654, -0.3162353388693405765, 0.4822834645669290543 ) ) ;
#79606 = CARTESIAN_POINT ( 'NONE',  ( 1.430446194225722500, -0.4281496062992127816, -0.4176697321401328100 ) ) ;
#79607 = CARTESIAN_POINT ( 'NONE',  ( -0.6889763779527552368, 0.07958543189024085140, 0.2665933059059887866 ) ) ;
#79608 = CARTESIAN_POINT ( 'NONE',  ( 0.000000000000000000, 0.000000000000000000, -2.755905511811024056 ) ) ;
#79609 = CARTESIAN_POINT ( 'NONE',  ( 0.4855643044619430415, -0.4281496062992127816, -0.4176697321401328100 ) ) ;
#79610 = CARTESIAN_POINT ( 'NONE',  ( 0.4133858267716541968, -0.4536011799217368745, -0.2665933059059886201 ) ) ;
#79611 = CARTESIAN_POINT ( 'NONE',  ( -0.6364829396325453192, -0.05778040916215560624, -0.4822834645669293319 ) ) ;
#79612 = CARTESIAN_POINT ( 'NONE',  ( 0.3917322834645669549, 2.398668435337827645E-17, -1.457985933561992686 ) ) ;
#79613 = CARTESIAN_POINT ( 'NONE',  ( -1.253280839895012377, -0.3162353388693409650, -0.4822834645669289433 ) ) ;
#79614 = ADVANCED_BREP_SHAPE_REPRESENTATION ( '', ( #31714, #22098 ), #649 ) ;
#79615 = CARTESIAN_POINT ( 'NONE',  ( -1.646981627296586703, -0.2845877964562161244, -0.3641732283464567121 ) ) ;
#79616 = CARTESIAN_POINT ( 'NONE',  ( 1.043307086614173818, 0.1660481256975885056, 0.3530559997133364547 ) ) ;
#79617 = CARTESIAN_POINT ( 'NONE',  ( 1.102362204724410155, -0.1870078740157480601, -0.3641732283464567677 ) ) ;
#79618 = ORIENTED_EDGE ( 'NONE', *, *, #48636, .F. ) ;
#79619 = CARTESIAN_POINT ( 'NONE',  ( -0.3917322834645670104, -0.1049643490035307020, -2.719835588747718802 ) ) ;
#79620 = CARTESIAN_POINT ( 'NONE',  ( -0.5380577427821514602, 0.05413385826771666132, 0.4176697321401328100 ) ) ;
#79621 = EDGE_LOOP ( 'NONE', ( #34046, #40672, #56675, #51798 ) ) ;
#79622 = CARTESIAN_POINT ( 'NONE',  ( 0.2952755905511816326, -0.4536011799217367080, 0.2665933059059888421 ) ) ;
#79623 = CARTESIAN_POINT ( 'NONE',  ( -1.036745406824146176, 0.05413385826771626580, -0.4176697321401330321 ) ) ;
#79624 = CARTESIAN_POINT ( 'NONE',  ( 1.076115485564305141, -0.6046776061558807314, 0.2411417322834647770 ) ) ;
#79625 = CARTESIAN_POINT ( 'NONE',  ( 1.030183727034121421, -0.3162353388693409650, -0.4822834645669289433 ) ) ;
#79626 = CARTESIAN_POINT ( 'NONE',  ( -0.04593175853018302557, -0.6692913385826773087, -0.1292274648535924053 ) ) ;
#79627 = CARTESIAN_POINT ( 'NONE',  ( -0.4396325459317577122, -0.6692913385826773087, -0.1292274648535924053 ) ) ;
#79628 = CARTESIAN_POINT ( 'NONE',  ( 0.2867679344610365999, -0.2867679344610365444, -2.072834645669291209 ) ) ;
#79629 = CARTESIAN_POINT ( 'NONE',  ( 1.614173228346457378, 0.1771653543307087630, 0.000000000000000000 ) ) ;
#79630 = CARTESIAN_POINT ( 'NONE',  ( -0.4133858267716528645, -0.5400638737290844871, 0.3530559997133364547 ) ) ;
#79631 = CARTESIAN_POINT ( 'NONE',  ( -0.4593175853018364174, -0.3690944881889765550, -0.3153832671262227771 ) ) ;
#79632 = CARTESIAN_POINT ( 'NONE',  ( 1.515748031496063408, 0.1660481256975885056, 0.3530559997133364547 ) ) ;
#79633 = CARTESIAN_POINT ( 'NONE',  ( 1.489501312335958172, -0.3162353388693405765, 0.4822834645669290543 ) ) ;
#79634 = CARTESIAN_POINT ( 'NONE',  ( -0.8792650918635160906, 0.05413385826771626580, -0.4176697321401330321 ) ) ;
#79635 = FACE_OUTER_BOUND ( 'NONE', #16162, .T. ) ;
#79636 = CARTESIAN_POINT ( 'NONE',  ( 0.5380577427821529035, 0.05413385826771626580, -0.4176697321401330321 ) ) ;
#79637 = CARTESIAN_POINT ( 'NONE',  ( -0.2925321140481932924, 0.2925321140481931814, -2.066929133858267154 ) ) ;
#79638 = CARTESIAN_POINT ( 'NONE',  ( 3.926431222168898838, 1.160582578298199108, 0.2886442948464663094 ) ) ;
#79639 = CARTESIAN_POINT ( 'NONE',  ( -0.2493438320209966919, -0.4281496062992124485, 0.4176697321401328655 ) ) ;
#79640 = CARTESIAN_POINT ( 'NONE',  ( -1.351706036745406347, -0.3690944881889763329, 0.3153832671262228327 ) ) ;
#79642 = FACE_OUTER_BOUND ( 'NONE', #98, .T. ) ;
#79641 = CARTESIAN_POINT ( 'NONE',  ( 1.030183727034121421, -0.08942795157527998196, 0.3641732283464567121 ) ) ;
#79643 = CARTESIAN_POINT ( 'NONE',  ( -1.157146581871515012E-16, 0.4724409448818898682, -0.8641732283464567121 ) ) ;
#79644 = CARTESIAN_POINT ( 'NONE',  ( 1.181102362204725198, -0.1870078740157479769, 0.3641732283464567677 ) ) ;
#79645 = CARTESIAN_POINT ( 'NONE',  ( 0.6955380577427828781, 0.05413385826771626580, -0.4176697321401330321 ) ) ;
#79646 = CARTESIAN_POINT ( 'NONE',  ( 0.3949938075777408852, 0.1058382717557500435, -0.3589238845144356871 ) ) ;
#79647 = CARTESIAN_POINT ( 'NONE',  ( -0.2821522309711278487, 0.2952755905511811885, 0.1292274648535926551 ) ) ;
#79648 = DIRECTION ( 'NONE',  ( 1.000000000000000000, -0.000000000000000000, 3.491481338843132961E-15 ) ) ;
#79649 = CARTESIAN_POINT ( 'NONE',  ( 1.187664041994751285, -0.2845877964562161244, -0.3641732283464567121 ) ) ;
#79650 = CARTESIAN_POINT ( 'NONE',  ( -0.7283464566929126471, 0.1660481256975883668, -0.3530559997133364547 ) ) ;
#79651 = CARTESIAN_POINT ( 'NONE',  ( 0.3949938075777409963, 2.418639510665530743E-17, -0.5098425196850394636 ) ) ;
#79652 = CARTESIAN_POINT ( 'NONE',  ( 1.154855643044620184, -0.6046776061558807314, 0.2411417322834647770 ) ) ;
#79653 = CARTESIAN_POINT ( 'NONE',  ( 0.1115485564304467270, -0.6692913385826773087, -0.1292274648535924053 ) ) ;
#79654 = AXIS2_PLACEMENT_3D ( 'NONE', #59059, #40538, #28315 ) ;
#79655 = CARTESIAN_POINT ( 'NONE',  ( 0.6102362204724416372, 0.07958543189024071263, -0.2665933059059888421 ) ) ;
#79656 = DIRECTION ( 'NONE',  ( 0.000000000000000000, -0.000000000000000000, 1.000000000000000000 ) ) ;
#79657 = CARTESIAN_POINT ( 'NONE',  ( 0.3674540682414705883, -0.5023911411419708095, 0.1820866141732285504 ) ) ;
#79658 = CYLINDRICAL_SURFACE ( 'NONE', #73986, 0.2165354330708660624 ) ;
#79659 = CARTESIAN_POINT ( 'NONE',  ( -9.787531504996566615E-17, 0.3996062992125985480, -1.336614173228346525 ) ) ;
#79660 = CARTESIAN_POINT ( 'NONE',  ( 0.7742782152230979209, 0.05413385826771626580, -0.4176697321401330321 ) ) ;
#79661 = CARTESIAN_POINT ( 'NONE',  ( 4.797336870675656522E-17, -0.3917322834645670104, -1.015748031496062964 ) ) ;
#79662 = CARTESIAN_POINT ( 'NONE',  ( 1.679790026246720025, 0.1283753931104748280, 0.1820866141732283561 ) ) ;
#79663 = CARTESIAN_POINT ( 'NONE',  ( -0.3496712940256294089, -0.1778467755331540612, -5.947530023412595687E-17 ) ) ;
#79664 = CARTESIAN_POINT ( 'NONE',  ( -0.09842519685039295696, 0.07958543189024071263, -0.2665933059059888421 ) ) ;
#79665 = CARTESIAN_POINT ( 'NONE',  ( 0.1640419947506569498, -0.3162353388693409650, -0.4822834645669289433 ) ) ;
#79666 = CARTESIAN_POINT ( 'NONE',  ( 1.607611548556431069, -0.5511811023622048555, -0.09757992244046775898 ) ) ;
#79667 = CARTESIAN_POINT ( 'NONE',  ( -1.338582677165353729, -0.1870078740157480601, -0.3641732283464567677 ) ) ;
#79668 = CARTESIAN_POINT ( 'NONE',  ( -1.482939632545930975, -0.4281496062992127816, -0.4176697321401328100 ) ) ;
#79669 = CARTESIAN_POINT ( 'NONE',  ( 0.7152230971128616943, -0.05778040916215522460, 0.4822834645669289988 ) ) ;
#79670 = CARTESIAN_POINT ( 'NONE',  ( 1.384514435695538559, 0.2952755905511810774, -0.1292274648535930714 ) ) ;
#79671 =( BOUNDED_CURVE ( )  B_SPLINE_CURVE ( 1, ( #72266, #39853 ),
 .UNSPECIFIED., .F., .F. ) 
 B_SPLINE_CURVE_WITH_KNOTS ( ( 2, 2 ),
 ( 0.000000000000000000, 0.001849999999999997480 ),
 .UNSPECIFIED. ) 
 CURVE ( )  GEOMETRIC_REPRESENTATION_ITEM ( )  RATIONAL_B_SPLINE_CURVE ( ( 0.9911642120908024101, 0.9911642120908024101 ) ) 
 REPRESENTATION_ITEM ( '' )  );
#79672 = CARTESIAN_POINT ( 'NONE',  ( -0.4091458600556405756, 0.2362204724409446288, -0.2604986876640419946 ) ) ;
#79673 = CARTESIAN_POINT ( 'NONE',  ( 0.3674540682414705883, 0.2306618581243847221, -0.2411417322834647770 ) ) ;
#79674 = CARTESIAN_POINT ( 'NONE',  ( 1.279527559055118724, -0.5400638737290845981, -0.3530559997133363437 ) ) ;
#79675 = CARTESIAN_POINT ( 'NONE',  ( 0.8661417322834653598, -0.1870078740157479769, 0.4822834645669291653 ) ) ;
#79676 = CARTESIAN_POINT ( 'NONE',  ( -1.332020997375327642, -0.2845877964562161244, -0.3641732283464567121 ) ) ;
#79677 = CARTESIAN_POINT ( 'NONE',  ( 1.128608923884515169, -0.5023911411419708095, -0.1820866141732282451 ) ) ;
#79678 = CARTESIAN_POINT ( 'NONE',  ( 1.686351706036745890, 0.2952755905511811885, 0.1292274648535926551 ) ) ;
#79679 = CARTESIAN_POINT ( 'NONE',  ( -0.7414698162729651543, -0.5511811023622046335, 0.09757992244046803654 ) ) ;
#79680 = EDGE_CURVE ( 'NONE', #33309, #43739, #34366, .T. ) ;
#79681 = CARTESIAN_POINT ( 'NONE',  ( 0.4724409448818897017, 0.1265901696524990294, -2.014435695538057125 ) ) ;
#79682 = CARTESIAN_POINT ( 'NONE',  ( 0.6889763779527563470, 0.07958543189024071263, -0.2665933059059888421 ) ) ;
#79683 = CARTESIAN_POINT ( 'NONE',  ( 0.09186351706036827158, 0.05413385826771666132, 0.4176697321401328100 ) ) ;
#79684 = CARTESIAN_POINT ( 'NONE',  ( 0.8464566929133865436, 0.1660481256975883668, -0.3530559997133364547 ) ) ;
#79685 = CARTESIAN_POINT ( 'NONE',  ( -0.4265091863517051496, -0.6692913385826771977, 0.1292274648535927661 ) ) ;
#79686 = CARTESIAN_POINT ( 'NONE',  ( 0.1574803149606306130, -0.1870078740157479769, 0.3641732283464567677 ) ) ;
#79687 = CARTESIAN_POINT ( 'NONE',  ( 1.325459317585302665, 0.05413385826771626580, -0.4176697321401330321 ) ) ;
#79688 = CARTESIAN_POINT ( 'NONE',  ( 0.000000000000000000, 1.446433227339393149E-17, -0.1181102362204724116 ) ) ;
#79689 = CARTESIAN_POINT ( 'NONE',  ( -0.8923884514435688198, 0.2306618581243847221, -0.2411417322834647770 ) ) ;
#79691 = CARTESIAN_POINT ( 'NONE',  ( 0.3996062992125985480, 0.1070741851644054637, -0.7545931758530182165 ) ) ;
#79690 = DIRECTION ( 'NONE',  ( 0.000000000000000000, 0.000000000000000000, 1.000000000000000000 ) ) ;
#79692 = LINE ( 'NONE', #79276, #65072 ) ;
#79693 = CARTESIAN_POINT ( 'NONE',  ( -0.7086614173228339419, -0.1870078740157479769, 0.4822834645669291653 ) ) ;
#79694 = CARTESIAN_POINT ( 'NONE',  ( -0.5708661417322828946, 0.1660481256975883668, -0.3530559997133364547 ) ) ;
#79695 = CARTESIAN_POINT ( 'NONE',  ( 0.4724409448818897572, -0.1265901696524988906, 0.04593175853018372640 ) ) ;
#79696 = CARTESIAN_POINT ( 'NONE',  ( -0.3420746716998659953, -0.1974969037888706647, -2.257217847769029007 ) ) ;
#79697 = ORIENTED_EDGE ( 'NONE', *, *, #46085, .T. ) ;
#79698 = CARTESIAN_POINT ( 'NONE',  ( 0.8202099737532814183, -0.5511811023622048555, -0.09757992244046775898 ) ) ;
#79700 = CARTESIAN_POINT ( 'NONE',  ( 0.3392501089628018884, -0.1958661417322834220, -1.041994750656167756 ) ) ;
#79699 = AXIS2_PLACEMENT_3D ( 'NONE', #10553, #55964, #23161 ) ;
#79701 = CARTESIAN_POINT ( 'NONE',  ( 1.036745406824147508, -0.4281496062992127816, -0.4176697321401328100 ) ) ;
#79702 = CYLINDRICAL_SURFACE ( 'NONE', #66851, 0.4744094488188972947 ) ;
#79703 = CARTESIAN_POINT ( 'NONE',  ( -1.528871391076114250, 0.1771653543307087075, -0.09757992244046823083 ) ) ;
#79704 = CARTESIAN_POINT ( 'NONE',  ( 1.469816272965879911, -0.6046776061558807314, 0.2411417322834647770 ) ) ;
#79705 = CARTESIAN_POINT ( 'NONE',  ( -1.653543307086613234, -0.1870078740157480879, -0.4822834645669291653 ) ) ;
#79706 = CARTESIAN_POINT ( 'NONE',  ( 0.3917322834645668994, -0.1049643490035303134, -0.5065423640081871959 ) ) ;
#79707 = CARTESIAN_POINT ( 'NONE',  ( -0.09186351706036663400, -0.4281496062992124485, 0.4176697321401328655 ) ) ;
#79708 = CARTESIAN_POINT ( 'NONE',  ( -0.3215223097112853146, -0.2845877964562159024, 0.3641732283464567677 ) ) ;
#79709 = CARTESIAN_POINT ( 'NONE',  ( 1.010498687664042716, 0.05413385826771626580, -0.4176697321401330321 ) ) ;
#79710 = CARTESIAN_POINT ( 'NONE',  ( 0.1312335958005255154, -0.6046776061558807314, 0.2411417322834647770 ) ) ;
#79711 = DIRECTION ( 'NONE',  ( 0.000000000000000000, 1.000000000000000000, -0.000000000000000000 ) ) ;
#79712 = CARTESIAN_POINT ( 'NONE',  ( -1.614173228346457378, 0.5038684218300931716, 0.1372047244094476981 ) ) ;
#79713 = CARTESIAN_POINT ( 'NONE',  ( 0.1049643490035304799, -0.3917322834645670104, -1.814323777724096809 ) ) ;
#79714 = CARTESIAN_POINT ( 'NONE',  ( 0.8661417322834653598, -0.1870078740157479769, 0.4822834645669291653 ) ) ;
#79715 = CARTESIAN_POINT ( 'NONE',  ( 0.1049868766404206816, -0.6046776061558809534, -0.2411417322834644161 ) ) ;
#79716 = CARTESIAN_POINT ( 'NONE',  ( -1.017060367454067249, -0.05778040916215522460, 0.4822834645669289988 ) ) ;
#79717 = CARTESIAN_POINT ( 'NONE',  ( 0.8923884514435701520, -0.6046776061558809534, -0.2411417322834644161 ) ) ;
#79718 = CARTESIAN_POINT ( 'NONE',  ( 1.056430446194226658, 0.2952755905511811885, 0.1292274648535926551 ) ) ;
#79719 = CARTESIAN_POINT ( 'NONE',  ( 0.2867679344610365999, -0.2867679344610365444, -0.9704724409448820532 ) ) ;
#79720 = CARTESIAN_POINT ( 'NONE',  ( -0.2690288713910754526, 0.2952755905511810774, -0.1292274648535930714 ) ) ;
#79721 = CARTESIAN_POINT ( 'NONE',  ( 0.7611548556430454138, 0.2306618581243847221, -0.2411417322834647770 ) ) ;
#79722 = CARTESIAN_POINT ( 'NONE',  ( 0.07217847769028949700, -0.3162353388693405765, 0.4822834645669290543 ) ) ;
#79723 = CARTESIAN_POINT ( 'NONE',  ( 0.5183727034120741983, -0.5511811023622046335, 0.09757992244046803654 ) ) ;
#79724 = CARTESIAN_POINT ( 'NONE',  ( -1.194225721784776262, 0.05413385826771626580, -0.4176697321401330321 ) ) ;
#79725 = CARTESIAN_POINT ( 'NONE',  ( -0.2887997841774402885, 1.160717306711473107, -2.785006778007305783 ) ) ;
#79726 = CARTESIAN_POINT ( 'NONE',  ( 0.3937007874015754361, -0.1870078740157480879, -0.4822834645669291653 ) ) ;
#79727 = DIRECTION ( 'NONE',  ( -1.000000000000000000, 0.000000000000000000, 0.000000000000000000 ) ) ;
#79728 = CARTESIAN_POINT ( 'NONE',  ( 4.797336870675656522E-17, -0.3917322834645670104, -2.433070866141732402 ) ) ;
#79729 = EDGE_LOOP ( 'NONE', ( #805, #17938, #34346, #53798, #46161, #34898, #17871, #41613, #31008, #66865, #30527, #20275, #65026, #51801, #25967, #59176, #24695, #77415, #81176, #81851, #24641, #22990, #78898, #66148, #24924, #294, #26892, #22166, #37657, #27411, #12944, #1866, #8790, #24726, #35091, #60649 ) ) ;
#79730 = VERTEX_POINT ( 'NONE', #16267 ) ;
#79731 = CARTESIAN_POINT ( 'NONE',  ( 1.076115485564305141, 0.2306618581243847221, -0.2411417322834647770 ) ) ;
#79732 = CARTESIAN_POINT ( 'NONE',  ( 0.5774278215223103139, -0.5023911411419708095, -0.1820866141732282451 ) ) ;
#79733 = DIRECTION ( 'NONE',  ( 0.000000000000000000, 1.000000000000000000, -0.000000000000000000 ) ) ;
#79734 = CARTESIAN_POINT ( 'NONE',  ( -0.7426113562972000981, 2.793565526369265584, -0.5309055118110234117 ) ) ;
#79735 = DIRECTION ( 'NONE',  ( 0.000000000000000000, 0.000000000000000000, 1.000000000000000000 ) ) ;
#79736 = CARTESIAN_POINT ( 'NONE',  ( -0.3917322834645669549, -0.1049643490035306603, -1.232939632545931863 ) ) ;
#79737 = CARTESIAN_POINT ( 'NONE',  ( -0.2925321140481930149, -0.2925321140481933480, -2.183070866141731958 ) ) ;
#79738 = CARTESIAN_POINT ( 'NONE',  ( -0.8464566929133852113, 0.1660481256975885056, 0.3530559997133364547 ) ) ;
#79739 = VECTOR ( 'NONE', #79985, 39.37007874015748143 ) ;
#79740 = CARTESIAN_POINT ( 'NONE',  ( -0.8333333333333323711, -0.6692913385826773087, -0.1292274648535924053 ) ) ;
#79741 = CARTESIAN_POINT ( 'NONE',  ( 1.148293963254593653, 0.2952755905511810774, -0.1292274648535930714 ) ) ;
#79742 = ORIENTED_EDGE ( 'NONE', *, *, #81513, .F. ) ;
#79743 = CARTESIAN_POINT ( 'NONE',  ( 1.601049868766404982, 0.2306618581243848609, 0.2411417322834645549 ) ) ;
#79744 = CARTESIAN_POINT ( 'NONE',  ( -1.016821367227983774, 1.505793896356053096, 0.4744094488188971281 ) ) ;
#79745 = CONTEXT_DEPENDENT_SHAPE_REPRESENTATION ( #65913, #66174 ) ;
#79746 = LINE ( 'NONE', #59113, #47932 ) ;
#79747 = CARTESIAN_POINT ( 'NONE',  ( -0.3996062992125984925, -0.1070741851644056719, -2.012467191601049699 ) ) ;
#79748 = CARTESIAN_POINT ( 'NONE',  ( -1.345144356955379816, -0.2845877964562159024, 0.3641732283464567677 ) ) ;
#79749 = CARTESIAN_POINT ( 'NONE',  ( 0.4177787735907000366, 0.3937007874015748254, -1.559171609364239375 ) ) ;
#79750 = CARTESIAN_POINT ( 'NONE',  ( 0.3149606299212606708, -0.1870078740157480879, -0.4822834645669291653 ) ) ;
#79752 = DIRECTION ( 'NONE',  ( -0.000000000000000000, -1.000000000000000000, -0.000000000000000000 ) ) ;
#79751 = CARTESIAN_POINT ( 'NONE',  ( 1.692913385826772421, 0.2952755905511811885, 0.000000000000000000 ) ) ;
#79753 = CARTESIAN_POINT ( 'NONE',  ( -0.6955380577427815458, -0.3690944881889765550, -0.3153832671262227771 ) ) ;
#79754 = CARTESIAN_POINT ( 'NONE',  ( 0.8989501312335964611, 0.2952755905511811885, 0.1292274648535926551 ) ) ;
#79755 = CARTESIAN_POINT ( 'NONE',  ( 1.377952755905512472, -0.5511811023622047445, 6.969142054262312111E-17 ) ) ;
#79756 = CARTESIAN_POINT ( 'NONE',  ( -9.594673741351310580E-17, 0.3917322834645669549, -1.182395382380890592 ) ) ;
#79757 = CONICAL_SURFACE ( 'NONE', #27277, 0.09842519685039351207, 1.029744258676651647 ) ;
#79758 = CARTESIAN_POINT ( 'NONE',  ( -0.7414698162729651543, 0.1771653543307087075, -0.09757992244046823083 ) ) ;
#79759 = CARTESIAN_POINT ( 'NONE',  ( 1.167979002624672580, -0.4281496062992124485, 0.4176697321401328655 ) ) ;
#79760 = CARTESIAN_POINT ( 'NONE',  ( 0.03185741929354787838, 1.953955006892923674, 0.3117665279056321959 ) ) ;
#79761 = CARTESIAN_POINT ( 'NONE',  ( -0.3083989501312330295, -0.05778040916215522460, 0.4822834645669289988 ) ) ;
#79762 = CARTESIAN_POINT ( 'NONE',  ( -0.9251968503937002541, -0.4536011799217368745, -0.2665933059059886201 ) ) ;
#79763 = CARTESIAN_POINT ( 'NONE',  ( -0.3543307086614165824, -0.5511811023622047445, 6.969142054262312111E-17 ) ) ;
#79764 = CARTESIAN_POINT ( 'NONE',  ( -0.4133858267716528645, 0.1660481256975883668, -0.3530559997133364547 ) ) ;
#79765 = CARTESIAN_POINT ( 'NONE',  ( 1.679790026246720025, 0.2306618581243848609, 0.2411417322834645549 ) ) ;
#79766 = CARTESIAN_POINT ( 'NONE',  ( 0.3917322834645670659, -0.1049643490035303273, -0.5807279771991620265 ) ) ;
#79767 = CARTESIAN_POINT ( 'NONE',  ( 0.4330708661417329575, -0.6692913385826771977, 8.415575281601705876E-17 ) ) ;
#79768 = EDGE_CURVE ( 'NONE', #40586, #78998, #28766, .T. ) ;
#79769 = CARTESIAN_POINT ( 'NONE',  ( -0.3458507752293906723, -0.3458507752293910609, -0.2165354330708661734 ) ) ;
#79770 = CARTESIAN_POINT ( 'NONE',  ( 0.1265901696524990294, -0.4724409448818896462, -1.579396325459317296 ) ) ;
#79771 = CARTESIAN_POINT ( 'NONE',  ( -0.8005249343832013809, -0.4281496062992124485, 0.4176697321401328655 ) ) ;
#79772 = CARTESIAN_POINT ( 'NONE',  ( -0.1181102362204717315, 0.1771653543307087630, 0.000000000000000000 ) ) ;
#79773 = CARTESIAN_POINT ( 'NONE',  ( -1.148293963254592542, 0.2952755905511811885, 0.1292274648535926551 ) ) ;
#79774 = CARTESIAN_POINT ( 'NONE',  ( -0.1115485564304453947, -0.6692913385826771977, 0.1292274648535927661 ) ) ;
#79775 = CARTESIAN_POINT ( 'NONE',  ( 0.5314960629921267055, -0.4536011799217367080, 0.2665933059059888421 ) ) ;
#79776 = CARTESIAN_POINT ( 'NONE',  ( -0.8005249343832013809, -0.3690944881889763329, 0.3153832671262228327 ) ) ;
#79777 = CARTESIAN_POINT ( 'NONE',  ( -0.9186351706036736120, 0.2306618581243848609, 0.2411417322834645549 ) ) ;
#79778 = CARTESIAN_POINT ( 'NONE',  ( -1.489501312335957062, -0.3162353388693409650, -0.4822834645669289433 ) ) ;
#79779 = EDGE_CURVE ( 'NONE', #21435, #69331, #3625, .T. ) ;
#79780 = CARTESIAN_POINT ( 'NONE',  ( 1.181102362204725198, -0.1870078740157479769, 0.4822834645669291653 ) ) ;
#79781 = DIRECTION ( 'NONE',  ( 0.000000000000000000, 0.000000000000000000, 1.000000000000000000 ) ) ;
#79782 = CARTESIAN_POINT ( 'NONE',  ( 0.7217847769028878924, -0.004921259842519576551, 0.3153832671262227771 ) ) ;
#79783 = CARTESIAN_POINT ( 'NONE',  ( 0.9776902887139113929, -0.6692913385826773087, -0.1292274648535924053 ) ) ;
#79784 = DIRECTION ( 'NONE',  ( 1.000000000000000000, 0.000000000000000000, 0.000000000000000000 ) ) ;
#79785 = CARTESIAN_POINT ( 'NONE',  ( 1.358267716535433323, -0.4536011799217368745, -0.2665933059059886201 ) ) ;
#79786 = ORIENTED_EDGE ( 'NONE', *, *, #15246, .F. ) ;
#79787 = CARTESIAN_POINT ( 'NONE',  ( -0.8005249343832011588, 0.05413385826771626580, -0.4176697321401330321 ) ) ;
#79788 = CARTESIAN_POINT ( 'NONE',  ( -0.2925321140481930149, -0.2925321140481933480, -2.812992125984251857 ) ) ;
#79789 = CARTESIAN_POINT ( 'NONE',  ( -1.305774278215222184, 0.1771653543307087630, 0.09757992244046791164 ) ) ;
#79790 = CARTESIAN_POINT ( 'NONE',  ( -0.5249343832020990641, 0.2306618581243848609, 0.2411417322834645549 ) ) ;
#79791 = CARTESIAN_POINT ( 'NONE',  ( 0.4724409448818904789, -0.1870078740157479769, 0.4822834645669291653 ) ) ;
#79792 = CARTESIAN_POINT ( 'NONE',  ( -1.568241469816272105, -0.08942795157527998196, 0.3641732283464567121 ) ) ;
#79793 = CARTESIAN_POINT ( 'NONE',  ( -9.787531504996566615E-17, 0.3996062992125985480, -2.281496062992125928 ) ) ;
#79794 = CARTESIAN_POINT ( 'NONE',  ( -1.541994750656167090, 0.2952755905511811885, 0.1292274648535926551 ) ) ;
#79795 = CARTESIAN_POINT ( 'NONE',  ( 0.3805774278215230400, -0.4281496062992124485, 0.4176697321401328655 ) ) ;
#79796 = CARTESIAN_POINT ( 'NONE',  ( 0.1115485564304470323, 0.2952755905511811885, 0.1292274648535926551 ) ) ;
#79797 = CARTESIAN_POINT ( 'NONE',  ( 0.9908136482939640111, 0.2952755905511810774, -0.1292274648535930714 ) ) ;
#79798 = CARTESIAN_POINT ( 'NONE',  ( 1.673228346456693494, 0.1660481256975885056, 0.3530559997133364547 ) ) ;
#79799 = CARTESIAN_POINT ( 'NONE',  ( 0.2925321140481932369, -0.2925321140481932369, -1.988188976377952777 ) ) ;
#79800 = CARTESIAN_POINT ( 'NONE',  ( 0.2891555358219910499, 0.2891555358219910499, -0.9251968503937008093 ) ) ;
#79801 = CARTESIAN_POINT ( 'NONE',  ( -0.1998031496062991907, -0.3460692066303959757, -2.585301837270341352 ) ) ;
#79802 = CARTESIAN_POINT ( 'NONE',  ( 0.3458507752293908943, 0.3458507752293908943, -0.6102362204724408601 ) ) ;
#79803 = CARTESIAN_POINT ( 'NONE',  ( -0.3392501089628017219, -0.1958661417322836718, -0.3595800524934382736 ) ) ;
#79804 = CARTESIAN_POINT ( 'NONE',  ( 0.01968503937007930540, 0.07958543189024085140, 0.2665933059059887866 ) ) ;
#79805 = CARTESIAN_POINT ( 'NONE',  ( -0.2230971128608915943, -0.4281496062992127816, -0.4176697321401328100 ) ) ;
#79806 = CARTESIAN_POINT ( 'NONE',  ( 0.8661417322834652488, -0.1870078740157480879, -0.4822834645669291653 ) ) ;
#79807 = CARTESIAN_POINT ( 'NONE',  ( 4.837279021331061486E-17, -0.3949938075777409963, -2.045275590551181022 ) ) ;
#79808 = CARTESIAN_POINT ( 'NONE',  ( 0.05905511811023709395, -0.4536011799217367080, 0.2665933059059888421 ) ) ;
#79809 = CARTESIAN_POINT ( 'NONE',  ( -1.076115485564303809, -0.6046776061558809534, -0.2411417322834644161 ) ) ;
#79810 = CARTESIAN_POINT ( 'NONE',  ( -1.535433070866141225, -0.6692913385826771977, 8.415575281601705876E-17 ) ) ;
#79811 = CARTESIAN_POINT ( 'NONE',  ( -0.3458507752293906723, -0.3458507752293910609, -2.106299212598425452 ) ) ;
#79812 = DIRECTION ( 'NONE',  ( -0.000000000000000000, -1.000000000000000000, -0.000000000000000000 ) ) ;
#79813 = VERTEX_POINT ( 'NONE', #41912 ) ;
#79814 = ORIENTED_EDGE ( 'NONE', *, *, #7406, .T. ) ;
#79815 = CARTESIAN_POINT ( 'NONE',  ( 0.9055118110236227702, -0.6692913385826771977, 8.415575281601705876E-17 ) ) ;
#79816 = CONICAL_SURFACE ( 'NONE', #8550, 1.889763779527559251, 0.7853981633974500554 ) ;
#79817 = CARTESIAN_POINT ( 'NONE',  ( 1.601049868766404982, 0.1283753931104748280, 0.1820866141732283561 ) ) ;
#79819 = CARTESIAN_POINT ( 'NONE',  ( -1.200787401574802349, -0.5400638737290844871, 0.3530559997133364547 ) ) ;
#79818 = CARTESIAN_POINT ( 'NONE',  ( -1.410761154855641575, -0.2845877964562161244, -0.3641732283464567121 ) ) ;
#79820 = CARTESIAN_POINT ( 'NONE',  ( 0.3392501089628018329, -0.1958661417322834497, -2.232264148785090274 ) ) ;
#79821 = DIRECTION ( 'NONE',  ( 0.000000000000000000, 8.673617379884035472E-16, -1.000000000000000000 ) ) ;
#79822 = CARTESIAN_POINT ( 'NONE',  ( 1.305774278215223960, -0.6692913385826771977, 0.1292274648535927661 ) ) ;
#79823 = CARTESIAN_POINT ( 'NONE',  ( -1.568241469816272105, -0.05778040916215522460, 0.4822834645669289988 ) ) ;
#79824 = CARTESIAN_POINT ( 'NONE',  ( -0.1706036745406816491, -0.4281496062992124485, 0.4176697321401328655 ) ) ;
#79825 = CARTESIAN_POINT ( 'NONE',  ( 0.03280839895013198948, 0.2952755905511811885, 0.1292274648535926551 ) ) ;
#79826 = CARTESIAN_POINT ( 'NONE',  ( -1.102362204724408601, -0.1870078740157480879, -0.4822834645669291653 ) ) ;
#79827 = CARTESIAN_POINT ( 'NONE',  ( -0.2867679344610364334, -0.2867679344610367109, 0.01377952755905502598 ) ) ;
#79828 = CARTESIAN_POINT ( 'NONE',  ( 0.1902887139107617975, 0.2952755905511811885, 0.1292274648535926551 ) ) ;
#79829 = CARTESIAN_POINT ( 'NONE',  ( 0.2867679344610365999, -0.2867679344610365444, -1.980314960629921073 ) ) ;
#79830 = CARTESIAN_POINT ( 'NONE',  ( -1.345144356955379816, -0.2845877964562159024, 0.3641732283464567677 ) ) ;
#79831 = VERTEX_POINT ( 'NONE', #9525 ) ;
#79832 = CARTESIAN_POINT ( 'NONE',  ( -0.3949938075777409408, -0.1058382717557502933, -2.250656167979002920 ) ) ;
#79833 = VERTEX_POINT ( 'NONE', #29292 ) ;
#79834 = CARTESIAN_POINT ( 'NONE',  ( -2.142213561789869658, 0.02617651024168207372, -0.4623158380715769455 ) ) ;
#79835 = CARTESIAN_POINT ( 'NONE',  ( -1.561679790026246017, 0.05413385826771666132, 0.4176697321401328100 ) ) ;
#79836 = CARTESIAN_POINT ( 'NONE',  ( 0.1070741851644054915, -0.3996062992125986035, -0.8727034120734907807 ) ) ;
#79837 = CARTESIAN_POINT ( 'NONE',  ( -1.581364829396324945, -0.3162353388693405765, 0.4822834645669290543 ) ) ;
#79838 = CARTESIAN_POINT ( 'NONE',  ( 1.033875059083676717, 1.724409448818897905, -0.4359958488159719758 ) ) ;
#79839 = CARTESIAN_POINT ( 'NONE',  ( -1.003937007874014853, 0.1660481256975885056, 0.3530559997133364547 ) ) ;
#79840 = CARTESIAN_POINT ( 'NONE',  ( 0.9345427628023850186, -1.711642917916620527E-15, -0.4281989832122460871 ) ) ;
#79841 = CARTESIAN_POINT ( 'NONE',  ( 0.3917322834645669549, 0.1049643490035304660, 0.1056430446194224632 ) ) ;
#79842 = CARTESIAN_POINT ( 'NONE',  ( -0.1574803149606292529, -0.1870078740157480601, -0.3641732283464567677 ) ) ;
#79843 = EDGE_CURVE ( 'NONE', #12831, #19838, #33946, .T. ) ;
#79844 = CARTESIAN_POINT ( 'NONE',  ( -0.8595800524934373854, -0.2845877964562161244, -0.3641732283464567121 ) ) ;
#79845 = CARTESIAN_POINT ( 'NONE',  ( -1.161417322834644716, 0.1660481256975885056, 0.3530559997133364547 ) ) ;
#79846 = CARTESIAN_POINT ( 'NONE',  ( 0.4921259842519691285, 0.1660481256975885056, 0.3530559997133364547 ) ) ;
#79847 = CARTESIAN_POINT ( 'NONE',  ( -0.7742782152230962556, -0.4281496062992127816, -0.4176697321401328100 ) ) ;
#79848 = CARTESIAN_POINT ( 'NONE',  ( 0.5314960629921395840, 2.677165354330708791, -3.900966923095588346 ) ) ;
#79849 = VERTEX_POINT ( 'NONE', #80662 ) ;
#79850 = CARTESIAN_POINT ( 'NONE',  ( -1.456692913385826182, 0.2952755905511811885, 0.000000000000000000 ) ) ;
#79851 = FACE_BOUND ( 'NONE', #60012, .T. ) ;
#79852 = CARTESIAN_POINT ( 'NONE',  ( 0.1265901696524989462, 0.4724409448818897572, -1.095800524934382958 ) ) ;
#79853 = CARTESIAN_POINT ( 'NONE',  ( 0.2952755905511810774, 0.000000000000000000, -1.929133858267716661 ) ) ;
#79854 =( BOUNDED_SURFACE ( )  B_SPLINE_SURFACE ( 1, 2, ( 
 ( #32651, #83174, #31820, #30988, #12891, #32236, #13309, #38550, #26336, #82760, #76455, #70120, #57894, #56656, #38133, #5730, #24675, #25494, #77702, #69719, #63807, #45683, #20032, #261, #18782, #76856, #44426, #44837, #64230, #25914, #77276, #45268, #54082, #78121, #34752, #34331, #27173, #7832, #78547, #33499, #73046, #46940, #15823, #14980, #15395, #65909, #60412, #41472, #53668, #1931, #79375, #58744, #66321, #2763, #28008, #40639, #41057, #1106, #65500, #72632, #78966, #33911, #72225, #47357, #26757, #52412, #8660, #59575, #20872, #22113, #20454, #46107, #71800, #21286, #59161, #66745, #59996, #53254, #14575, #14153, #7407, #2352, #1519, #39810, #47773, #46525, #73474, #52835, #21694, #40227, #8246, #27594, #9081, #28422, #33077, #79797, #17880, #75540, #3172, #4816, #55327, #67157, #49019, #68801, #28836, #36805, #68399, #30076, #4001, #9486, #10738, #23348, #24172, #62481, #16645, #35161, #42702, #49841, #60821, #80213, #9900, #54500, #42285, #10328, #17065, #4408, #43105, #22528, #48190, #73887, #35572, #16227, #67983, #35990, #36395, #55739, #11146, #41874, #75129, #61660, #29665, #67568, #74716, #62069, #23764, #81447, #30494, #61235, #3590, #22937, #49435, #29255, #48603, #54919, #80625, #81036, #17474, #74299, #56157, #81860, #45165, #70439, #64547, #38038, #43514, #26238, #51065, #82266, #19095, #24985, #6884, #30898, #70871, #12796, #63303, #43933, #31308, #69627, #25817, #83080, #51899, #76765, #51477, #18693, #13220, #77606, #6470, #63713, #32140, #11563, #44744, #38866, #64138, #38452, #77180, #37222, #18288, #25401, #31725, #70027, #50661, #164, #62899, #5234, #57797, #12380, #56972, #58217, #56565, #24584, #50251, #57388, #11972, #19511, #32554, #6053, #76361, #75947, #69214, #583, #37627, #5641, #82670, #44336, #34649, #58642, #65815, #65400, #46004, #20352, #40543, #1010, #19939, #66223, #53982, #28321, #39282, #40957, #8148, #45588, #1831, #21593, #64969, #72944, #21187, #8561, #40129, #71281, #46841, #59478, #60313, #15296, #52735, #13630, #78861, #66638, #39709, #72535, #20772, #7737, #14476, #33403, #33813, #47255, #8975, #26663, #14883, #7305, #52317, #59065, #27492, #53149, #34229, #59892, #32975, #2244, #71700, #27910, #2662, #78024, #14054, #1420, #27076, #53569, #78446, #46426, #72117, #79278, #73787, #48494, #43002, #4708, #36290, #49325, #10219, #48913, #61132, #74195, #17372, #54397, #54819, #68695, #60721, #68299, #29966, #74613, #16958, #61963, #10635, #67881, #55221, #11037, #47671, #16541, #42186, #35468, #3484, #35886, #30382, #61556, #3899, #36695, #62370, #29558, #42597, #35055, #80928, #23243, #4303, #55631, #73366, #81340, #23655, #79694, #75027, #22011, #15714, #41371, #41769, #67052, #9385, #3070, #16123, #28737, #80110, #22428, #48086, #67462, #9796, #29150, #80520, #22835, #57696, #50961, #82163, #76658, #58, #69521, #31203, #43817, #11871, #6365, #12277, #37934, #75435, #17775, #43408, #82564, #32037, #64025, #18991, #56869, #76255, #37113, #63611, #25712, #6778, #69107, #11455, #62796, #75842, #24479, #51372, #37523, #70763, #5131, #18590, #18184, #50145, #56461, #44639, #30795, #56048, #70335, #81757, #64442, #63197, #77075, #44232, #24067, #5948, #19409, #5538, #45060, #57279, #12691, #69922, #49736, #82976, #31617, #13112, #38765, #24883, #50552, #25295, #38350, #26133, #45484, #58541, #77500, #7635, #58967, #65720, #53051, #8461, #13523, #40444, #1324, #33306, #32450, #14376, #8052, #72438, #40033, #27813, #908, #26564, #71598, #33714, #40856, #13950, #64863, #58112, #26973, #66124, #66540, #39608, #47157, #34130, #59376, #53473, #52638, #478, #15197, #1734, #71181, #27390, #65296, #79183, #19835, #59791, #78763, #52218, #32873, #20252, #77921, #14788, #72020, #51795, #21087, #2146, #78343, #21498, #39179, #46746, #20674, #72848, #7202, #45901, #46327, #29465, #42090, #16861, #60215, #66960, #48399, #80429, #35374, #73691, #48815, #28224, #2565, #10123, #61039, #22331, #23557, #53882, #79597, #21912, #22739, #60626, #42499, #74099, #54724, #16031, #47574, #42904, #16445, #2976, #73268, #49227 ),
 ( #3803, #74514, #80832, #67785, #35787, #29870, #15617, #3389, #29053, #47992, #41677, #61455, #17276, #55123, #23146, #74931, #81241, #68200, #10538, #41274, #36195, #61865, #4206, #55532, #9293, #8873, #34549, #34963, #28642, #54300, #80013, #67370, #9704, #44140, #76160, #55949, #62697, #31523, #75332, #6263, #69832, #17679, #11358, #82067, #12591, #24380, #70236, #63517, #37016, #5847, #38249, #50052, #43722, #56368, #75746, #18896, #24787, #50456, #4611, #30283, #81661, #11779, #44545, #76568, #57180, #69426, #5444, #49639, #18497, #63927, #19308, #23972, #43309, #69007, #5036, #30704, #31939, #57600, #18087, #12181, #37432, #63105, #31105, #56772, #82472, #83290, #25613, #37839, #82882, #10939, #25202, #50868, #51276, #76978, #68599, #36596, #62274, #33203, #13426, #26875, #2044, #70656, #27709, #59689, #39082, #78243, #53375, #79083, #52115, #64345, #64763, #13848, #8361, #44960, #6681, #32353, #58014, #7102, #71083, #72339, #66024, #32772, #46226, #45803, #58439, #39506, #801, #65194, #46646, #34028, #51694, #20575, #13013, #77397, #26464, #58868, #1226, #7530, #52535, #38667, #71922, #77823, #14272, #379, #26034, #19731, #45386, #20153, #39933, #71500, #65620, #7951, #33613, #59276, #1632, #27291, #52949, #78663, #14687, #20984, #40344, #2875, #73590, #42397, #79492, #79911, #10441, #2466, #10018, #55026, #16345, #41988, #61349, #35684, #9603, #80327, #68095, #72747, #15933, #41580, #60526, #28538, #60936, #29774, #3286, #28951, #61768, #36097, #67270, #67682, #60115, #35271, #54616, #22641, #80734, #15095, #48301, #3703, #55435, #74413, #4108, #21400, #40752, #66862, #73998, #29366, #8772, #15513, #23048, #28124, #47055, #48715, #53779, #47471, #34864, #16757, #54195, #66436, #34446, #73163, #21807, #41171, #22228, #47883, #9192, #36918, #31419, #37336, #63008, #17175, #42808, #68502, #24281, #58228, #5748, #18402, #56270, #17990, #62178, #5347, #595, #10842, #19950, #69329, #7317, #31006, #26251, #36502, #51910, #82374, #44045, #43625, #81144, #24693, #56674, #39295, #77617, #30605, #32986, #50361, #64981, #74830, #4516, #23875, #30185, #81966, #49952, #76059, #69737, #45600, #55848, #71294, #75650, #11678, #23459, #12081, #37739, #63413, #13642, #49125, #49541, #75236, #62595, #81556, #17579, #4937, #43212, #68908, #11260, #8990, #67066, #40140, #73379, #60326, #2256, #79708, #53161, #58654, #41385, #66234, #14065, #34242, #65825, #22024, #46017, #2675, #27921, #78457, #59075, #46437, #1430, #40971, #14893, #9398, #8572, #66653, #33823, #28334, #1021, #21607, #78872, #47267, #26674, #59904, #53996, #79289, #53580, #34663, #52329, #33413, #40553, #46851, #1843, #8158, #15308, #78035, #20365, #72957, #27504, #72128, #15729, #71711, #39719, #65410, #72546, #27086, #47684, #7748, #21197, #59489, #52749, #20782, #14486, #29165, #80124, #75452, #22851, #49752, #73802, #80944, #80539, #61147, #35483, #55646, #16138, #35069, #81357, #69122, #43425, #23259, #74629, #60735, #48929, #3499, #16973, #17790, #3087, #28751, #54413, #54834, #68313, #22443, #48104, #42201, #41784, #48511, #3914, #81772, #67477, #75041, #4723, #42613, #4318, #16557, #29575, #56063, #9811, #10235, #24082, #74211, #23669, #68712, #29983, #49341, #17387, #43018, #10650, #36305, #67897, #35902, #55238, #61981, #61571, #11053, #36711, #62386, #30398, #19007, #51813, #497, #63627, #32053, #50162, #82992, #44656, #25313, #45078, #62812, #12707, #51389, #45502, #64460, #32468, #77518, #5146, #56887, #70352, #38366, #82179, #5555, #57713, #18200, #58130, #64042, #43835, #37539, #24899, #38783, #50568, #13132, #6381, #63215, #76, #6797, #76272, #69938, #82580, #18606, #70781, #50977, #76675, #30811, #56476, #24496, #37950, #26152, #19426, #25729, #12294, #31634, #75858, #77094, #19853, #11471, #69537, #11887, #31219, #44249, #5964, #37128, #57294, #7654, #72456, #72037, #58986, #65737, #33324, #8070, #72866, #34567, #77939, #46763, #13542, #20269, #1341, #59393, #1751, #79615, #7220, #8890, #27408, #21931, #53069, #15215, #32891, #40875, #14805, #34148, #33732, #71199, #40463 ) ),
 .UNSPECIFIED., .F., .F., .F. ) 
 B_SPLINE_SURFACE_WITH_KNOTS ( ( 2, 2 ),
 ( 3, 2, 2, 2, 2, 2, 2, 2, 2, 2, 2, 2, 2, 2, 2, 2, 2, 2, 2, 2, 2, 2, 2, 2, 2, 2, 2, 2, 2, 2, 2, 2, 2, 2, 2, 2, 2, 2, 2, 2, 2, 2, 2, 2, 2, 2, 2, 2, 2, 2, 2, 2, 2, 2, 2, 2, 2, 2, 2, 2, 2, 2, 2, 2, 2, 2, 2, 2, 2, 2, 2, 2, 2, 2, 2, 2, 2, 2, 2, 2, 2, 2, 2, 2, 2, 2, 2, 2, 2, 2, 2, 2, 2, 2, 2, 2, 2, 2, 2, 2, 2, 2, 2, 2, 2, 2, 2, 2, 2, 2, 2, 2, 2, 2, 2, 2, 2, 2, 2, 2, 2, 2, 2, 2, 2, 2, 2, 2, 2, 2, 2, 2, 2, 2, 2, 2, 2, 2, 2, 2, 2, 2, 2, 2, 2, 2, 2, 2, 2, 2, 2, 2, 2, 2, 2, 2, 2, 2, 2, 2, 2, 2, 2, 2, 2, 2, 2, 2, 2, 2, 2, 2, 2, 2, 2, 2, 2, 2, 2, 2, 2, 2, 2, 2, 2, 2, 2, 2, 2, 2, 2, 2, 2, 2, 2, 2, 2, 2, 2, 2, 2, 2, 2, 2, 2, 2, 2, 2, 2, 2, 2, 2, 2, 2, 2, 2, 2, 2, 2, 2, 2, 2, 2, 2, 2, 2, 2, 2, 2, 2, 2, 2, 2, 2, 2, 2, 2, 2, 2, 2, 2, 2, 2, 2, 2, 2, 2, 2, 2, 2, 2, 2, 2, 2, 2, 3 ),
 ( 0.000000000000000000, 1.000000000000000000 ),
 ( 0.000000000000000000, 0.003787878787878787984, 0.007575757575757575968, 0.01136363636363636395, 0.01515151515151515194, 0.01893939393939393992, 0.02272727272727272790, 0.02651515151515151589, 0.03030303030303030387, 0.03409090909090908839, 0.03787878787878787984, 0.04166666666666666435, 0.04545454545454545581, 0.04924242424242424032, 0.05303030303030303177, 0.05681818181818181629, 0.06060606060606060774, 0.06439393939393939226, 0.06818181818181817677, 0.07196969696969697516, 0.07575757575757575968, 0.07954545454545454419, 0.08333333333333332871, 0.08712121212121212710, 0.09090909090909091161, 0.09469696969696969613, 0.09848484848484848064, 0.1022727272727272790, 0.1060606060606060635, 0.1098484848484848481, 0.1136363636363636326, 0.1174242424242424310, 0.1212121212121212155, 0.1250000000000000000, 0.1287878787878787845, 0.1325757575757575690, 0.1363636363636363535, 0.1401515151515151381, 0.1439393939393939503, 0.1477272727272727348, 0.1515151515151515194, 0.1553030303030303039, 0.1590909090909090884, 0.1628787878787878729, 0.1666666666666666574, 0.1704545454545454419, 0.1742424242424242542, 0.1780303030303030387, 0.1818181818181818232, 0.1856060606060606077, 0.1893939393939393923, 0.1931818181818181768, 0.1969696969696969613, 0.2007575757575757458, 0.2045454545454545581, 0.2083333333333333426, 0.2121212121212121271, 0.2159090909090909116, 0.2196969696969696961, 0.2234848484848484806, 0.2272727272727272652, 0.2310606060606060497, 0.2348484848484848619, 0.2386363636363636465, 0.2424242424242424310, 0.2462121212121212155, 0.2500000000000000000, 0.2537878787878787845, 0.2575757575757575690, 0.2613636363636363535, 0.2651515151515151381, 0.2689393939393939226, 0.2727272727272727071, 0.2765151515151514916, 0.2803030303030302761, 0.2840909090909091161, 0.2878787878787879007, 0.2916666666666666852, 0.2954545454545454697, 0.2992424242424242542, 0.3030303030303030387, 0.3068181818181818232, 0.3106060606060606077, 0.3143939393939393923, 0.3181818181818181768, 0.3219696969696969613, 0.3257575757575757458, 0.3295454545454545303, 0.3333333333333333148, 0.3371212121212120993, 0.3409090909090908839, 0.3446969696969697239, 0.3484848484848485084, 0.3522727272727272929, 0.3560606060606060774, 0.3598484848484848619, 0.3636363636363636465, 0.3674242424242424310, 0.3712121212121212155, 0.3750000000000000000, 0.3787878787878787845, 0.3825757575757575690, 0.3863636363636363535, 0.3901515151515151381, 0.3939393939393939226, 0.3977272727272727071, 0.4015151515151514916, 0.4053030303030302761, 0.4090909090909091161, 0.4128787878787879007, 0.4166666666666666852, 0.4204545454545454697, 0.4242424242424242542, 0.4280303030303030387, 0.4318181818181818232, 0.4356060606060606077, 0.4393939393939393923, 0.4431818181818181768, 0.4469696969696969613, 0.4507575757575757458, 0.4545454545454545303, 0.4583333333333333148, 0.4621212121212120993, 0.4659090909090908839, 0.4696969696969697239, 0.4734848484848485084, 0.4772727272727272929, 0.4810606060606060774, 0.4848484848484848619, 0.4886363636363636465, 0.4924242424242424310, 0.4962121212121212155, 0.5000000000000000000, 0.5037878787878787845, 0.5075757575757575690, 0.5113636363636363535, 0.5151515151515151381, 0.5189393939393939226, 0.5227272727272727071, 0.5265151515151514916, 0.5303030303030302761, 0.5340909090909090606, 0.5378787878787878451, 0.5416666666666666297, 0.5454545454545454142, 0.5492424242424241987, 0.5530303030303029832, 0.5568181818181817677, 0.5606060606060605522, 0.5643939393939394478, 0.5681818181818182323, 0.5719696969696970168, 0.5757575757575758013, 0.5795454545454545858, 0.5833333333333333703, 0.5871212121212121549, 0.5909090909090909394, 0.5946969696969697239, 0.5984848484848485084, 0.6022727272727272929, 0.6060606060606060774, 0.6098484848484848619, 0.6136363636363636465, 0.6174242424242424310, 0.6212121212121212155, 0.6250000000000000000, 0.6287878787878787845, 0.6325757575757575690, 0.6363636363636363535, 0.6401515151515151381, 0.6439393939393939226, 0.6477272727272727071, 0.6515151515151514916, 0.6553030303030302761, 0.6590909090909090606, 0.6628787878787878451, 0.6666666666666666297, 0.6704545454545454142, 0.6742424242424241987, 0.6780303030303029832, 0.6818181818181817677, 0.6856060606060605522, 0.6893939393939394478, 0.6931818181818182323, 0.6969696969696970168, 0.7007575757575758013, 0.7045454545454545858, 0.7083333333333333703, 0.7121212121212121549, 0.7159090909090909394, 0.7196969696969697239, 0.7234848484848485084, 0.7272727272727272929, 0.7310606060606060774, 0.7348484848484848619, 0.7386363636363636465, 0.7424242424242424310, 0.7462121212121212155, 0.7500000000000000000, 0.7537878787878787845, 0.7575757575757575690, 0.7613636363636363535, 0.7651515151515151381, 0.7689393939393939226, 0.7727272727272727071, 0.7765151515151514916, 0.7803030303030302761, 0.7840909090909090606, 0.7878787878787878451, 0.7916666666666666297, 0.7954545454545454142, 0.7992424242424241987, 0.8030303030303029832, 0.8068181818181817677, 0.8106060606060605522, 0.8143939393939394478, 0.8181818181818182323, 0.8219696969696970168, 0.8257575757575758013, 0.8295454545454545858, 0.8333333333333333703, 0.8371212121212121549, 0.8409090909090909394, 0.8446969696969697239, 0.8484848484848485084, 0.8522727272727272929, 0.8560606060606060774, 0.8598484848484848619, 0.8636363636363636465, 0.8674242424242424310, 0.8712121212121212155, 0.8750000000000000000, 0.8787878787878787845, 0.8825757575757575690, 0.8863636363636363535, 0.8901515151515151381, 0.8939393939393939226, 0.8977272727272727071, 0.9015151515151514916, 0.9053030303030302761, 0.9090909090909090606, 0.9128787878787878451, 0.9166666666666666297, 0.9204545454545454142, 0.9242424242424241987, 0.9280303030303029832, 0.9318181818181817677, 0.9356060606060605522, 0.9393939393939394478, 0.9431818181818182323, 0.9469696969696970168, 0.9507575757575758013, 0.9545454545454545858, 0.9583333333333333703, 0.9621212121212121549, 0.9659090909090909394 ),
 .UNSPECIFIED. ) 
 GEOMETRIC_REPRESENTATION_ITEM ( )  RATIONAL_B_SPLINE_SURFACE ( (
 ( 1.000000000000000000, 0.9659258262890683122, 1.000000000000000000, 0.9659258262890683122, 1.000000000000000000, 0.9659258262890683122, 1.000000000000000000, 0.9659258262890683122, 1.000000000000000000, 0.9659258262890683122, 1.000000000000000000, 0.9659258262890683122, 1.000000000000000000, 0.9659258262890683122, 1.000000000000000000, 0.9659258262890683122, 1.000000000000000000, 0.9659258262890683122, 1.000000000000000000, 0.9659258262890683122, 1.000000000000000000, 0.9659258262890683122, 1.000000000000000000, 0.9659258262890683122, 1.000000000000000000, 0.9659258262890683122, 1.000000000000000000, 0.9659258262890683122, 1.000000000000000000, 0.9659258262890683122, 1.000000000000000000, 0.9659258262890683122, 1.000000000000000000, 0.9659258262890683122, 1.000000000000000000, 0.9659258262890683122, 1.000000000000000000, 0.9659258262890683122, 1.000000000000000000, 0.9659258262890683122, 1.000000000000000000, 0.9659258262890683122, 1.000000000000000000, 0.9659258262890683122, 1.000000000000000000, 0.9659258262890683122, 1.000000000000000000, 0.9659258262890683122, 1.000000000000000000, 0.9659258262890683122, 1.000000000000000000, 0.9659258262890683122, 1.000000000000000000, 0.9659258262890683122, 1.000000000000000000, 0.9659258262890683122, 1.000000000000000000, 0.9659258262890683122, 1.000000000000000000, 0.9659258262890683122, 1.000000000000000000, 0.9659258262890683122, 1.000000000000000000, 0.9659258262890683122, 1.000000000000000000, 0.9659258262890683122, 1.000000000000000000, 0.9659258262890683122, 1.000000000000000000, 0.9659258262890683122, 1.000000000000000000, 0.9659258262890683122, 1.000000000000000000, 0.9659258262890683122, 1.000000000000000000, 0.9659258262890683122, 1.000000000000000000, 0.9659258262890683122, 1.000000000000000000, 0.9659258262890683122, 1.000000000000000000, 0.9659258262890683122, 1.000000000000000000, 0.9659258262890683122, 1.000000000000000000, 0.9659258262890683122, 1.000000000000000000, 0.9659258262890683122, 1.000000000000000000, 0.9659258262890683122, 1.000000000000000000, 0.9659258262890683122, 1.000000000000000000, 0.9659258262890683122, 1.000000000000000000, 0.9659258262890683122, 1.000000000000000000, 0.9659258262890683122, 1.000000000000000000, 0.9659258262890683122, 1.000000000000000000, 0.9659258262890683122, 1.000000000000000000, 0.9659258262890683122, 1.000000000000000000, 0.9659258262890683122, 1.000000000000000000, 0.9659258262890683122, 1.000000000000000000, 0.9659258262890683122, 1.000000000000000000, 0.9659258262890683122, 1.000000000000000000, 0.9659258262890683122, 1.000000000000000000, 0.9659258262890683122, 1.000000000000000000, 0.9659258262890683122, 1.000000000000000000, 0.9659258262890683122, 1.000000000000000000, 0.9659258262890683122, 1.000000000000000000, 0.9659258262890683122, 1.000000000000000000, 0.9659258262890683122, 1.000000000000000000, 0.9659258262890683122, 1.000000000000000000, 0.9659258262890683122, 1.000000000000000000, 0.9659258262890683122, 1.000000000000000000, 0.9659258262890683122, 1.000000000000000000, 0.9659258262890683122, 1.000000000000000000, 0.9659258262890683122, 1.000000000000000000, 0.9659258262890683122, 1.000000000000000000, 0.9659258262890683122, 1.000000000000000000, 0.9659258262890683122, 1.000000000000000000, 0.9659258262890683122, 1.000000000000000000, 0.9659258262890683122, 1.000000000000000000, 0.9659258262890683122, 1.000000000000000000, 0.9659258262890683122, 1.000000000000000000, 0.9659258262890683122, 1.000000000000000000, 0.9659258262890683122, 1.000000000000000000, 0.9659258262890683122, 1.000000000000000000, 0.9659258262890683122, 1.000000000000000000, 0.9659258262890683122, 1.000000000000000000, 0.9659258262890683122, 1.000000000000000000, 0.9659258262890683122, 1.000000000000000000, 0.9659258262890683122, 1.000000000000000000, 0.9659258262890683122, 1.000000000000000000, 0.9659258262890683122, 1.000000000000000000, 0.9659258262890683122, 1.000000000000000000, 0.9659258262890683122, 1.000000000000000000, 0.9659258262890683122, 1.000000000000000000, 0.9659258262890683122, 1.000000000000000000, 0.9659258262890683122, 1.000000000000000000, 0.9659258262890683122, 1.000000000000000000, 0.9659258262890683122, 1.000000000000000000, 0.9659258262890683122, 1.000000000000000000, 0.9659258262890683122, 1.000000000000000000, 0.9659258262890683122, 1.000000000000000000, 0.9659258262890683122, 1.000000000000000000, 0.9659258262890683122, 1.000000000000000000, 0.9659258262890683122, 1.000000000000000000, 0.9659258262890683122, 1.000000000000000000, 0.9659258262890683122, 1.000000000000000000, 0.9659258262890683122, 1.000000000000000000, 0.9659258262890683122, 1.000000000000000000, 0.9659258262890683122, 1.000000000000000000, 0.9659258262890683122, 1.000000000000000000, 0.9659258262890683122, 1.000000000000000000, 0.9659258262890683122, 1.000000000000000000, 0.9659258262890683122, 1.000000000000000000, 0.9659258262890683122, 1.000000000000000000, 0.9659258262890683122, 1.000000000000000000, 0.9659258262890683122, 1.000000000000000000, 0.9659258262890683122, 1.000000000000000000, 0.9659258262890683122, 1.000000000000000000, 0.9659258262890683122, 1.000000000000000000, 0.9659258262890683122, 1.000000000000000000, 0.9659258262890683122, 1.000000000000000000, 0.9659258262890683122, 1.000000000000000000, 0.9659258262890683122, 1.000000000000000000, 0.9659258262890683122, 1.000000000000000000, 0.9659258262890683122, 1.000000000000000000, 0.9659258262890683122, 1.000000000000000000, 0.9659258262890683122, 1.000000000000000000, 0.9659258262890683122, 1.000000000000000000, 0.9659258262890683122, 1.000000000000000000, 0.9659258262890683122, 1.000000000000000000, 0.9659258262890683122, 1.000000000000000000, 0.9659258262890683122, 1.000000000000000000, 0.9659258262890683122, 1.000000000000000000, 0.9659258262890683122, 1.000000000000000000, 0.9659258262890683122, 1.000000000000000000, 0.9659258262890683122, 1.000000000000000000, 0.9659258262890683122, 1.000000000000000000, 0.9659258262890683122, 1.000000000000000000, 0.9659258262890683122, 1.000000000000000000, 0.9659258262890683122, 1.000000000000000000, 0.9659258262890683122, 1.000000000000000000, 0.9659258262890683122, 1.000000000000000000, 0.9659258262890683122, 1.000000000000000000, 0.9659258262890683122, 1.000000000000000000, 0.9659258262890683122, 1.000000000000000000, 0.9659258262890683122, 1.000000000000000000, 0.9659258262890683122, 1.000000000000000000, 0.9659258262890683122, 1.000000000000000000, 0.9659258262890683122, 1.000000000000000000, 0.9659258262890683122, 1.000000000000000000, 0.9659258262890683122, 1.000000000000000000, 0.9659258262890683122, 1.000000000000000000, 0.9659258262890683122, 1.000000000000000000, 0.9659258262890683122, 1.000000000000000000, 0.9659258262890683122, 1.000000000000000000, 0.9659258262890683122, 1.000000000000000000, 0.9659258262890683122, 1.000000000000000000, 0.9659258262890683122, 1.000000000000000000, 0.9659258262890683122, 1.000000000000000000, 0.9659258262890683122, 1.000000000000000000, 0.9659258262890683122, 1.000000000000000000, 0.9659258262890683122, 1.000000000000000000, 0.9659258262890683122, 1.000000000000000000, 0.9659258262890683122, 1.000000000000000000, 0.9659258262890683122, 1.000000000000000000, 0.9659258262890683122, 1.000000000000000000, 0.9659258262890683122, 1.000000000000000000, 0.9659258262890683122, 1.000000000000000000, 0.9659258262890683122, 1.000000000000000000, 0.9659258262890683122, 1.000000000000000000, 0.9659258262890683122, 1.000000000000000000, 0.9659258262890683122, 1.000000000000000000, 0.9659258262890683122, 1.000000000000000000, 0.9659258262890683122, 1.000000000000000000, 0.9659258262890683122, 1.000000000000000000, 0.9659258262890683122, 1.000000000000000000, 0.9659258262890683122, 1.000000000000000000, 0.9659258262890683122, 1.000000000000000000, 0.9659258262890683122, 1.000000000000000000, 0.9659258262890683122, 1.000000000000000000, 0.9659258262890683122, 1.000000000000000000, 0.9659258262890683122, 1.000000000000000000, 0.9659258262890683122, 1.000000000000000000, 0.9659258262890683122, 1.000000000000000000, 0.9659258262890683122, 1.000000000000000000, 0.9659258262890683122, 1.000000000000000000, 0.9659258262890683122, 1.000000000000000000, 0.9659258262890683122, 1.000000000000000000, 0.9659258262890683122, 1.000000000000000000, 0.9659258262890683122, 1.000000000000000000, 0.9659258262890683122, 1.000000000000000000, 0.9659258262890683122, 1.000000000000000000, 0.9659258262890683122, 1.000000000000000000, 0.9659258262890683122, 1.000000000000000000, 0.9659258262890683122, 1.000000000000000000, 0.9659258262890683122, 1.000000000000000000, 0.9659258262890683122, 1.000000000000000000, 0.9659258262890683122, 1.000000000000000000, 0.9659258262890683122, 1.000000000000000000, 0.9659258262890683122, 1.000000000000000000, 0.9659258262890683122, 1.000000000000000000, 0.9659258262890683122, 1.000000000000000000, 0.9659258262890683122, 1.000000000000000000, 0.9659258262890683122, 1.000000000000000000, 0.9659258262890683122, 1.000000000000000000, 0.9659258262890683122, 1.000000000000000000, 0.9659258262890683122, 1.000000000000000000, 0.9659258262890683122, 1.000000000000000000, 0.9659258262890683122, 1.000000000000000000, 0.9659258262890683122, 1.000000000000000000, 0.9659258262890683122, 1.000000000000000000, 0.9659258262890683122, 1.000000000000000000, 0.9659258262890683122, 1.000000000000000000, 0.9659258262890683122, 1.000000000000000000, 0.9659258262890683122, 1.000000000000000000, 0.9659258262890683122, 1.000000000000000000, 0.9659258262890683122, 1.000000000000000000, 0.9659258262890683122, 1.000000000000000000, 0.9659258262890683122, 1.000000000000000000, 0.9659258262890683122, 1.000000000000000000, 0.9659258262890683122, 1.000000000000000000, 0.9659258262890683122, 1.000000000000000000, 0.9659258262890683122, 1.000000000000000000, 0.9659258262890683122, 1.000000000000000000, 0.9659258262890683122, 1.000000000000000000, 0.9659258262890683122, 1.000000000000000000, 0.9659258262890683122, 1.000000000000000000, 0.9659258262890683122, 1.000000000000000000, 0.9659258262890683122, 1.000000000000000000, 0.9659258262890683122, 1.000000000000000000, 0.9659258262890683122, 1.000000000000000000, 0.9659258262890683122, 1.000000000000000000, 0.9659258262890683122, 1.000000000000000000, 0.9659258262890683122, 1.000000000000000000, 0.9659258262890683122, 1.000000000000000000, 0.9659258262890683122, 1.000000000000000000, 0.9659258262890683122, 1.000000000000000000, 0.9659258262890683122, 1.000000000000000000, 0.9659258262890683122, 1.000000000000000000, 0.9659258262890683122, 1.000000000000000000, 0.9659258262890683122, 1.000000000000000000, 0.9659258262890683122, 1.000000000000000000, 0.9659258262890683122, 1.000000000000000000, 0.9659258262890683122, 1.000000000000000000, 0.9659258262890683122, 1.000000000000000000, 0.9659258262890683122, 1.000000000000000000, 0.9659258262890683122, 1.000000000000000000, 0.9659258262890683122, 1.000000000000000000, 0.9659258262890683122, 1.000000000000000000, 0.9659258262890683122, 1.000000000000000000, 0.9659258262890683122, 1.000000000000000000, 0.9659258262890683122, 1.000000000000000000, 0.9659258262890683122, 1.000000000000000000, 0.9659258262890683122, 1.000000000000000000, 0.9659258262890683122, 1.000000000000000000, 0.9659258262890683122, 1.000000000000000000, 0.9659258262890683122, 1.000000000000000000, 0.9659258262890683122, 1.000000000000000000, 0.9659258262890683122, 1.000000000000000000, 0.9659258262890683122, 1.000000000000000000),
 ( 1.000000000000000000, 0.9659258262890683122, 1.000000000000000000, 0.9659258262890683122, 1.000000000000000000, 0.9659258262890683122, 1.000000000000000000, 0.9659258262890683122, 1.000000000000000000, 0.9659258262890683122, 1.000000000000000000, 0.9659258262890683122, 1.000000000000000000, 0.9659258262890683122, 1.000000000000000000, 0.9659258262890683122, 1.000000000000000000, 0.9659258262890683122, 1.000000000000000000, 0.9659258262890683122, 1.000000000000000000, 0.9659258262890683122, 1.000000000000000000, 0.9659258262890683122, 1.000000000000000000, 0.9659258262890683122, 1.000000000000000000, 0.9659258262890683122, 1.000000000000000000, 0.9659258262890683122, 1.000000000000000000, 0.9659258262890683122, 1.000000000000000000, 0.9659258262890683122, 1.000000000000000000, 0.9659258262890683122, 1.000000000000000000, 0.9659258262890683122, 1.000000000000000000, 0.9659258262890683122, 1.000000000000000000, 0.9659258262890683122, 1.000000000000000000, 0.9659258262890683122, 1.000000000000000000, 0.9659258262890683122, 1.000000000000000000, 0.9659258262890683122, 1.000000000000000000, 0.9659258262890683122, 1.000000000000000000, 0.9659258262890683122, 1.000000000000000000, 0.9659258262890683122, 1.000000000000000000, 0.9659258262890683122, 1.000000000000000000, 0.9659258262890683122, 1.000000000000000000, 0.9659258262890683122, 1.000000000000000000, 0.9659258262890683122, 1.000000000000000000, 0.9659258262890683122, 1.000000000000000000, 0.9659258262890683122, 1.000000000000000000, 0.9659258262890683122, 1.000000000000000000, 0.9659258262890683122, 1.000000000000000000, 0.9659258262890683122, 1.000000000000000000, 0.9659258262890683122, 1.000000000000000000, 0.9659258262890683122, 1.000000000000000000, 0.9659258262890683122, 1.000000000000000000, 0.9659258262890683122, 1.000000000000000000, 0.9659258262890683122, 1.000000000000000000, 0.9659258262890683122, 1.000000000000000000, 0.9659258262890683122, 1.000000000000000000, 0.9659258262890683122, 1.000000000000000000, 0.9659258262890683122, 1.000000000000000000, 0.9659258262890683122, 1.000000000000000000, 0.9659258262890683122, 1.000000000000000000, 0.9659258262890683122, 1.000000000000000000, 0.9659258262890683122, 1.000000000000000000, 0.9659258262890683122, 1.000000000000000000, 0.9659258262890683122, 1.000000000000000000, 0.9659258262890683122, 1.000000000000000000, 0.9659258262890683122, 1.000000000000000000, 0.9659258262890683122, 1.000000000000000000, 0.9659258262890683122, 1.000000000000000000, 0.9659258262890683122, 1.000000000000000000, 0.9659258262890683122, 1.000000000000000000, 0.9659258262890683122, 1.000000000000000000, 0.9659258262890683122, 1.000000000000000000, 0.9659258262890683122, 1.000000000000000000, 0.9659258262890683122, 1.000000000000000000, 0.9659258262890683122, 1.000000000000000000, 0.9659258262890683122, 1.000000000000000000, 0.9659258262890683122, 1.000000000000000000, 0.9659258262890683122, 1.000000000000000000, 0.9659258262890683122, 1.000000000000000000, 0.9659258262890683122, 1.000000000000000000, 0.9659258262890683122, 1.000000000000000000, 0.9659258262890683122, 1.000000000000000000, 0.9659258262890683122, 1.000000000000000000, 0.9659258262890683122, 1.000000000000000000, 0.9659258262890683122, 1.000000000000000000, 0.9659258262890683122, 1.000000000000000000, 0.9659258262890683122, 1.000000000000000000, 0.9659258262890683122, 1.000000000000000000, 0.9659258262890683122, 1.000000000000000000, 0.9659258262890683122, 1.000000000000000000, 0.9659258262890683122, 1.000000000000000000, 0.9659258262890683122, 1.000000000000000000, 0.9659258262890683122, 1.000000000000000000, 0.9659258262890683122, 1.000000000000000000, 0.9659258262890683122, 1.000000000000000000, 0.9659258262890683122, 1.000000000000000000, 0.9659258262890683122, 1.000000000000000000, 0.9659258262890683122, 1.000000000000000000, 0.9659258262890683122, 1.000000000000000000, 0.9659258262890683122, 1.000000000000000000, 0.9659258262890683122, 1.000000000000000000, 0.9659258262890683122, 1.000000000000000000, 0.9659258262890683122, 1.000000000000000000, 0.9659258262890683122, 1.000000000000000000, 0.9659258262890683122, 1.000000000000000000, 0.9659258262890683122, 1.000000000000000000, 0.9659258262890683122, 1.000000000000000000, 0.9659258262890683122, 1.000000000000000000, 0.9659258262890683122, 1.000000000000000000, 0.9659258262890683122, 1.000000000000000000, 0.9659258262890683122, 1.000000000000000000, 0.9659258262890683122, 1.000000000000000000, 0.9659258262890683122, 1.000000000000000000, 0.9659258262890683122, 1.000000000000000000, 0.9659258262890683122, 1.000000000000000000, 0.9659258262890683122, 1.000000000000000000, 0.9659258262890683122, 1.000000000000000000, 0.9659258262890683122, 1.000000000000000000, 0.9659258262890683122, 1.000000000000000000, 0.9659258262890683122, 1.000000000000000000, 0.9659258262890683122, 1.000000000000000000, 0.9659258262890683122, 1.000000000000000000, 0.9659258262890683122, 1.000000000000000000, 0.9659258262890683122, 1.000000000000000000, 0.9659258262890683122, 1.000000000000000000, 0.9659258262890683122, 1.000000000000000000, 0.9659258262890683122, 1.000000000000000000, 0.9659258262890683122, 1.000000000000000000, 0.9659258262890683122, 1.000000000000000000, 0.9659258262890683122, 1.000000000000000000, 0.9659258262890683122, 1.000000000000000000, 0.9659258262890683122, 1.000000000000000000, 0.9659258262890683122, 1.000000000000000000, 0.9659258262890683122, 1.000000000000000000, 0.9659258262890683122, 1.000000000000000000, 0.9659258262890683122, 1.000000000000000000, 0.9659258262890683122, 1.000000000000000000, 0.9659258262890683122, 1.000000000000000000, 0.9659258262890683122, 1.000000000000000000, 0.9659258262890683122, 1.000000000000000000, 0.9659258262890683122, 1.000000000000000000, 0.9659258262890683122, 1.000000000000000000, 0.9659258262890683122, 1.000000000000000000, 0.9659258262890683122, 1.000000000000000000, 0.9659258262890683122, 1.000000000000000000, 0.9659258262890683122, 1.000000000000000000, 0.9659258262890683122, 1.000000000000000000, 0.9659258262890683122, 1.000000000000000000, 0.9659258262890683122, 1.000000000000000000, 0.9659258262890683122, 1.000000000000000000, 0.9659258262890683122, 1.000000000000000000, 0.9659258262890683122, 1.000000000000000000, 0.9659258262890683122, 1.000000000000000000, 0.9659258262890683122, 1.000000000000000000, 0.9659258262890683122, 1.000000000000000000, 0.9659258262890683122, 1.000000000000000000, 0.9659258262890683122, 1.000000000000000000, 0.9659258262890683122, 1.000000000000000000, 0.9659258262890683122, 1.000000000000000000, 0.9659258262890683122, 1.000000000000000000, 0.9659258262890683122, 1.000000000000000000, 0.9659258262890683122, 1.000000000000000000, 0.9659258262890683122, 1.000000000000000000, 0.9659258262890683122, 1.000000000000000000, 0.9659258262890683122, 1.000000000000000000, 0.9659258262890683122, 1.000000000000000000, 0.9659258262890683122, 1.000000000000000000, 0.9659258262890683122, 1.000000000000000000, 0.9659258262890683122, 1.000000000000000000, 0.9659258262890683122, 1.000000000000000000, 0.9659258262890683122, 1.000000000000000000, 0.9659258262890683122, 1.000000000000000000, 0.9659258262890683122, 1.000000000000000000, 0.9659258262890683122, 1.000000000000000000, 0.9659258262890683122, 1.000000000000000000, 0.9659258262890683122, 1.000000000000000000, 0.9659258262890683122, 1.000000000000000000, 0.9659258262890683122, 1.000000000000000000, 0.9659258262890683122, 1.000000000000000000, 0.9659258262890683122, 1.000000000000000000, 0.9659258262890683122, 1.000000000000000000, 0.9659258262890683122, 1.000000000000000000, 0.9659258262890683122, 1.000000000000000000, 0.9659258262890683122, 1.000000000000000000, 0.9659258262890683122, 1.000000000000000000, 0.9659258262890683122, 1.000000000000000000, 0.9659258262890683122, 1.000000000000000000, 0.9659258262890683122, 1.000000000000000000, 0.9659258262890683122, 1.000000000000000000, 0.9659258262890683122, 1.000000000000000000, 0.9659258262890683122, 1.000000000000000000, 0.9659258262890683122, 1.000000000000000000, 0.9659258262890683122, 1.000000000000000000, 0.9659258262890683122, 1.000000000000000000, 0.9659258262890683122, 1.000000000000000000, 0.9659258262890683122, 1.000000000000000000, 0.9659258262890683122, 1.000000000000000000, 0.9659258262890683122, 1.000000000000000000, 0.9659258262890683122, 1.000000000000000000, 0.9659258262890683122, 1.000000000000000000, 0.9659258262890683122, 1.000000000000000000, 0.9659258262890683122, 1.000000000000000000, 0.9659258262890683122, 1.000000000000000000, 0.9659258262890683122, 1.000000000000000000, 0.9659258262890683122, 1.000000000000000000, 0.9659258262890683122, 1.000000000000000000, 0.9659258262890683122, 1.000000000000000000, 0.9659258262890683122, 1.000000000000000000, 0.9659258262890683122, 1.000000000000000000, 0.9659258262890683122, 1.000000000000000000, 0.9659258262890683122, 1.000000000000000000, 0.9659258262890683122, 1.000000000000000000, 0.9659258262890683122, 1.000000000000000000, 0.9659258262890683122, 1.000000000000000000, 0.9659258262890683122, 1.000000000000000000, 0.9659258262890683122, 1.000000000000000000, 0.9659258262890683122, 1.000000000000000000, 0.9659258262890683122, 1.000000000000000000, 0.9659258262890683122, 1.000000000000000000, 0.9659258262890683122, 1.000000000000000000, 0.9659258262890683122, 1.000000000000000000, 0.9659258262890683122, 1.000000000000000000, 0.9659258262890683122, 1.000000000000000000, 0.9659258262890683122, 1.000000000000000000, 0.9659258262890683122, 1.000000000000000000, 0.9659258262890683122, 1.000000000000000000, 0.9659258262890683122, 1.000000000000000000, 0.9659258262890683122, 1.000000000000000000, 0.9659258262890683122, 1.000000000000000000, 0.9659258262890683122, 1.000000000000000000, 0.9659258262890683122, 1.000000000000000000, 0.9659258262890683122, 1.000000000000000000, 0.9659258262890683122, 1.000000000000000000, 0.9659258262890683122, 1.000000000000000000, 0.9659258262890683122, 1.000000000000000000, 0.9659258262890683122, 1.000000000000000000, 0.9659258262890683122, 1.000000000000000000, 0.9659258262890683122, 1.000000000000000000, 0.9659258262890683122, 1.000000000000000000, 0.9659258262890683122, 1.000000000000000000, 0.9659258262890683122, 1.000000000000000000, 0.9659258262890683122, 1.000000000000000000, 0.9659258262890683122, 1.000000000000000000, 0.9659258262890683122, 1.000000000000000000, 0.9659258262890683122, 1.000000000000000000, 0.9659258262890683122, 1.000000000000000000, 0.9659258262890683122, 1.000000000000000000, 0.9659258262890683122, 1.000000000000000000, 0.9659258262890683122, 1.000000000000000000, 0.9659258262890683122, 1.000000000000000000, 0.9659258262890683122, 1.000000000000000000, 0.9659258262890683122, 1.000000000000000000, 0.9659258262890683122, 1.000000000000000000, 0.9659258262890683122, 1.000000000000000000, 0.9659258262890683122, 1.000000000000000000, 0.9659258262890683122, 1.000000000000000000, 0.9659258262890683122, 1.000000000000000000, 0.9659258262890683122, 1.000000000000000000, 0.9659258262890683122, 1.000000000000000000, 0.9659258262890683122, 1.000000000000000000, 0.9659258262890683122, 1.000000000000000000, 0.9659258262890683122, 1.000000000000000000, 0.9659258262890683122, 1.000000000000000000, 0.9659258262890683122, 1.000000000000000000, 0.9659258262890683122, 1.000000000000000000, 0.9659258262890683122, 1.000000000000000000, 0.9659258262890683122, 1.000000000000000000, 0.9659258262890683122, 1.000000000000000000) ) ) 
 REPRESENTATION_ITEM ( '' )  SURFACE ( )  );
#79855 = CARTESIAN_POINT ( 'NONE',  ( 0.1958661417322834775, 0.3392501089628018884, -0.6089238845144356871 ) ) ;
#79856 = CARTESIAN_POINT ( 'NONE',  ( -0.3917322834645670104, -7.196005306013484475E-17, -2.486220472440944906 ) ) ;
#79857 = CARTESIAN_POINT ( 'NONE',  ( -0.6627296587926501115, 0.2952755905511810774, -0.1292274648535930714 ) ) ;
#79858 = CARTESIAN_POINT ( 'NONE',  ( 1.640419947506562393, -0.4281496062992124485, 0.4176697321401328655 ) ) ;
#79859 = CARTESIAN_POINT ( 'NONE',  ( -0.2925321140481932369, 0.2925321140481931259, -0.09645669291338584972 ) ) ;
#79861 = CARTESIAN_POINT ( 'NONE',  ( -0.4744094488189058989, 1.554943921348593161, 2.554262525012261253 ) ) ;
#79860 = CARTESIAN_POINT ( 'NONE',  ( -1.614173228346456712, 2.401574803149606474, -0.1372047244094478091 ) ) ;
#79862 = CARTESIAN_POINT ( 'NONE',  ( -1.430446194225721390, -0.4281496062992124485, 0.4176697321401328655 ) ) ;
#79863 = CARTESIAN_POINT ( 'NONE',  ( -0.6364829396325453192, -0.3162353388693405765, 0.4822834645669290543 ) ) ;
#79864 = CARTESIAN_POINT ( 'NONE',  ( -0.1049643490035301746, -0.3917322834645670659, -0.1522116553467698086 ) ) ;
#79865 = CARTESIAN_POINT ( 'NONE',  ( 0.3412073490813655186, 0.1283753931104748280, 0.1820866141732283561 ) ) ;
#79866 = CARTESIAN_POINT ( 'NONE',  ( -0.2867679344610366554, 0.2867679344610365444, -0.4192913385826772532 ) ) ;
#79867 = CIRCLE ( 'NONE', #18020, 2.204724409448819422 ) ;
#79868 = CARTESIAN_POINT ( 'NONE',  ( 0.2690288713910767848, 0.1771653543307087630, 0.09757992244046791164 ) ) ;
#79869 = CARTESIAN_POINT ( 'NONE',  ( 1.030183727034121421, -0.2845877964562161244, -0.3641732283464567121 ) ) ;
#79870 = CARTESIAN_POINT ( 'NONE',  ( 1.095800524934383846, -0.3162353388693405765, 0.4822834645669290543 ) ) ;
#79871 = CARTESIAN_POINT ( 'NONE',  ( -0.5052493438320203589, 0.1771653543307087075, -0.09757992244046823083 ) ) ;
#79872 = CARTESIAN_POINT ( 'NONE',  ( -0.2867679344610364334, -0.2867679344610367109, -1.783464566929133577 ) ) ;
#79873 = CARTESIAN_POINT ( 'NONE',  ( -1.122047244094487306, 0.1660481256975883668, -0.3530559997133364547 ) ) ;
#79874 = CARTESIAN_POINT ( 'NONE',  ( -1.259842519685038686, -0.1870078740157480601, -0.3641732283464567677 ) ) ;
#79875 = CARTESIAN_POINT ( 'NONE',  ( -0.1265901696524993347, 0.4724409448818895907, -0.5557742782152230721 ) ) ;
#79876 = CARTESIAN_POINT ( 'NONE',  ( -0.9317585301837263412, -0.3690944881889765550, -0.3153832671262227771 ) ) ;
#79877 = CARTESIAN_POINT ( 'NONE',  ( -0.2821522309711278487, -0.6692913385826773087, -0.1292274648535924053 ) ) ;
#79878 = CARTESIAN_POINT ( 'NONE',  ( 1.601049868766404982, -0.5023911411419708095, -0.1820866141732282451 ) ) ;
#79879 = CONICAL_SURFACE ( 'NONE', #34134, 2.559055118110236560, 0.7853981633974500554 ) ;
#79880 = CARTESIAN_POINT ( 'NONE',  ( 0.4265091863517067039, -0.5511811023622048555, -0.09757992244046775898 ) ) ;
#79881 = CARTESIAN_POINT ( 'NONE',  ( -0.4527559055118102749, 0.07958543189024085140, 0.2665933059059887866 ) ) ;
#79882 = CARTESIAN_POINT ( 'NONE',  ( -0.7217847769028863381, -0.4281496062992124485, 0.4176697321401328655 ) ) ;
#79883 = DIRECTION ( 'NONE',  ( 0.000000000000000000, 0.000000000000000000, -1.000000000000000000 ) ) ;
#79884 = CARTESIAN_POINT ( 'NONE',  ( -2.795275590551183686, 1.299212598425198095, -1.990688069879260956E-16 ) ) ;
#79885 = CARTESIAN_POINT ( 'NONE',  ( 0.2755905511811031494, 0.2952755905511811885, 0.000000000000000000 ) ) ;
#79886 = CARTESIAN_POINT ( 'NONE',  ( -0.3460692066303960313, 0.1998031496062989965, -1.520341207349081181 ) ) ;
#79887 = CARTESIAN_POINT ( 'NONE',  ( 1.614173228346457378, 0.2952755905511811885, 0.000000000000000000 ) ) ;
#79888 = CARTESIAN_POINT ( 'NONE',  ( -0.1312335958005241554, 0.1283753931104748280, 0.1820866141732283561 ) ) ;
#79889 = CARTESIAN_POINT ( 'NONE',  ( -0.006561679790025524116, -0.3162353388693405765, 0.4822834645669290543 ) ) ;
#79890 = CARTESIAN_POINT ( 'NONE',  ( -1.443569553805773564, 0.2306618581243847221, -0.2411417322834647770 ) ) ;
#79891 = CARTESIAN_POINT ( 'NONE',  ( 1.522309711286089939, 0.2306618581243848609, 0.2411417322834645549 ) ) ;
#79892 = CARTESIAN_POINT ( 'NONE',  ( 1.292650918635171564, -0.6692913385826773087, -0.1292274648535924053 ) ) ;
#79893 = CARTESIAN_POINT ( 'NONE',  ( -0.5314960629921254842, -0.4536011799217368745, -0.2665933059059886201 ) ) ;
#79894 = CARTESIAN_POINT ( 'NONE',  ( -0.1070741851644051862, -0.3996062992125986035, -0.3064304461942256586 ) ) ;
#79895 = CARTESIAN_POINT ( 'NONE',  ( -0.2925321140481932924, 0.2925321140481931814, -0.1771653543307086520 ) ) ;
#79896 = CARTESIAN_POINT ( 'NONE',  ( -9.674558042662121740E-17, 0.3949938075777409963, 0.1574803149606298636 ) ) ;
#79897 = CARTESIAN_POINT ( 'NONE',  ( 1.574803149606299746, -0.1870078740157480601, -0.3641732283464567677 ) ) ;
#79898 = EDGE_CURVE ( 'NONE', #15186, #47884, #22974, .T. ) ;
#79899 = CARTESIAN_POINT ( 'NONE',  ( 1.253280839895013710, -0.2845877964562159024, 0.3641732283464567677 ) ) ;
#79900 = DIRECTION ( 'NONE',  ( -1.000000000000000000, 0.000000000000000000, 0.000000000000000000 ) ) ;
#79901 = B_SPLINE_CURVE_WITH_KNOTS ( 'NONE', 3,
 ( #7412, #32656, #64235, #26341, #71385, #13734, #7836, #52002 ),
 .UNSPECIFIED., .F., .F.,
 ( 4, 2, 2, 4 ),
 ( 0.07134069304684192980, 0.07377942048615132586, 0.07499878420580601002, 0.07621814792546070805 ),
 .UNSPECIFIED. ) ;
#79902 = CARTESIAN_POINT ( 'NONE',  ( 0.8005249343832027131, 0.05413385826771666132, 0.4176697321401328100 ) ) ;
#79903 = CARTESIAN_POINT ( 'NONE',  ( 0.3917322834645670104, -0.1049643490035303411, -2.243438320209974357 ) ) ;
#79904 = CARTESIAN_POINT ( 'NONE',  ( 1.272965879265092637, -0.3690944881889765550, -0.3153832671262227771 ) ) ;
#79905 = EDGE_CURVE ( 'NONE', #31620, #3191, #40673, .T. ) ;
#79906 = CARTESIAN_POINT ( 'NONE',  ( 0.1902887139107617975, -0.6692913385826773087, -0.1292274648535924053 ) ) ;
#79907 = CARTESIAN_POINT ( 'NONE',  ( -0.5118110236220466680, 0.2952755905511811885, 0.000000000000000000 ) ) ;
#79908 = CARTESIAN_POINT ( 'NONE',  ( 0.000000000000000000, 0.000000000000000000, -1.512162153811850596 ) ) ;
#79909 = CARTESIAN_POINT ( 'NONE',  ( 5.785732909357575061E-17, -0.4724409448818898682, -0.8661417322834645827 ) ) ;
#79910 = CARTESIAN_POINT ( 'NONE',  ( -0.1998031496062994683, 0.3460692066303958092, -2.060367454068241511 ) ) ;
#79911 = CARTESIAN_POINT ( 'NONE',  ( 0.5314960629921264834, 0.07958543189024071263, -0.2665933059059888421 ) ) ;
#79912 = ORIENTED_EDGE ( 'NONE', *, *, #37828, .T. ) ;
#79913 = CARTESIAN_POINT ( 'NONE',  ( 0.3392501089628018884, -0.1958661417322833942, -0.4166859824485057984 ) ) ;
#79914 = ORIENTED_EDGE ( 'NONE', *, *, #15570, .F. ) ;
#79915 = CARTESIAN_POINT ( 'NONE',  ( -0.6233595800524928121, -0.05778040916215522460, 0.4822834645669289988 ) ) ;
#79916 = CARTESIAN_POINT ( 'NONE',  ( 0.9645669291338588858, 0.1660481256975885056, 0.3530559997133364547 ) ) ;
#79917 = CARTESIAN_POINT ( 'NONE',  ( 0.3018372703412079971, 0.05413385826771626580, -0.4176697321401330321 ) ) ;
#79918 = CARTESIAN_POINT ( 'NONE',  ( -0.1771653543307080136, 0.07958543189024071263, -0.2665933059059888421 ) ) ;
#79919 = VECTOR ( 'NONE', #7670, 39.37007874015748143 ) ;
#79920 = CARTESIAN_POINT ( 'NONE',  ( 0.6364829396325465405, -0.3162353388693409650, -0.4822834645669289433 ) ) ;
#79921 = CARTESIAN_POINT ( 'NONE',  ( -0.8333333333333323711, 0.2952755905511811885, 0.1292274648535926551 ) ) ;
#79922 = CARTESIAN_POINT ( 'NONE',  ( -0.5314960629921254842, -0.5400638737290845981, -0.3530559997133363437 ) ) ;
#79923 = CARTESIAN_POINT ( 'NONE',  ( -0.9908136482939626788, -0.6692913385826773087, -0.1292274648535924053 ) ) ;
#79924 = CARTESIAN_POINT ( 'NONE',  ( 1.036745406824147508, -0.4281496062992127816, -0.4176697321401328100 ) ) ;
#79925 = CARTESIAN_POINT ( 'NONE',  ( 0.7283464566929140904, -0.5400638737290845981, -0.3530559997133363437 ) ) ;
#79926 = CARTESIAN_POINT ( 'NONE',  ( 0.8070866141732289112, -0.5400638737290845981, -0.3530559997133363437 ) ) ;
#79927 = EDGE_CURVE ( 'NONE', #70474, #27584, #53290, .T. ) ;
#79928 = CARTESIAN_POINT ( 'NONE',  ( 0.2867679344610365999, 0.2867679344610365999, -0.4448818897637794589 ) ) ;
#79929 = CARTESIAN_POINT ( 'NONE',  ( -0.1312335958005241554, -0.5023911411419708095, -0.1820866141732282451 ) ) ;
#79930 = ORIENTED_EDGE ( 'NONE', *, *, #68219, .F. ) ;
#79931 = CARTESIAN_POINT ( 'NONE',  ( -0.3949938075777409408, -0.1058382717557502933, -0.8333333333333334814 ) ) ;
#79932 = ORIENTED_EDGE ( 'NONE', *, *, #46613, .F. ) ;
#79933 = CARTESIAN_POINT ( 'NONE',  ( -1.030183727034119867, -0.08942795157528024563, -0.3641732283464568787 ) ) ;
#79934 = CARTESIAN_POINT ( 'NONE',  ( -0.2952755905511803003, -0.5400638737290845981, -0.3530559997133363437 ) ) ;
#79935 = DIRECTION ( 'NONE',  ( 0.000000000000000000, 0.000000000000000000, 1.000000000000000000 ) ) ;
#79936 = CARTESIAN_POINT ( 'NONE',  ( -0.1706036745406816491, -0.4281496062992124485, 0.4176697321401328655 ) ) ;
#79937 = CARTESIAN_POINT ( 'NONE',  ( -0.5118110236220466680, -0.6692913385826771977, 8.415575281601705876E-17 ) ) ;
#79938 = CARTESIAN_POINT ( 'NONE',  ( -1.194225721784776262, -0.4281496062992124485, 0.4176697321401328655 ) ) ;
#79939 = CARTESIAN_POINT ( 'NONE',  ( -1.332020997375327642, -0.3162353388693409650, -0.4822834645669289433 ) ) ;
#79940 = VECTOR ( 'NONE', #38923, 39.37007874015748143 ) ;
#79941 = CARTESIAN_POINT ( 'NONE',  ( 0.7742782152230979209, -0.004921259842519870586, -0.3153832671262229437 ) ) ;
#79942 = CARTESIAN_POINT ( 'NONE',  ( 0.3458507752293908943, 0.3458507752293908943, -0.3720472440944882497 ) ) ;
#79943 = CARTESIAN_POINT ( 'NONE',  ( 0.2597269936800725709, 0.1406511682536830121, 5.810287953473521227 ) ) ;
#79944 = CARTESIAN_POINT ( 'NONE',  ( 0.3280839895013130669, -0.004921259842519576551, 0.3153832671262227771 ) ) ;
#79945 =( REPRESENTATION_RELATIONSHIP ('NONE','NONE', #79348, #33107 ) REPRESENTATION_RELATIONSHIP_WITH_TRANSFORMATION ( #30850 )SHAPE_REPRESENTATION_RELATIONSHIP( ) );
#79946 = CARTESIAN_POINT ( 'NONE',  ( -0.1443569553805765515, -0.4281496062992127816, -0.4176697321401328100 ) ) ;
#79947 = CARTESIAN_POINT ( 'NONE',  ( 0.2296587926509192634, -0.3162353388693405765, 0.4822834645669290543 ) ) ;
#79948 = ORIENTED_EDGE ( 'NONE', *, *, #56687, .F. ) ;
#79949 = CARTESIAN_POINT ( 'NONE',  ( -0.1070741851644051862, -0.3996062992125987146, -1.804461942257217677 ) ) ;
#79950 = CARTESIAN_POINT ( 'NONE',  ( -0.6183353934921174133, 0.02791078216816064370, 0.4328096321851915285 ) ) ;
#79951 = ORIENTED_EDGE ( 'NONE', *, *, #77984, .T. ) ;
#79952 = CARTESIAN_POINT ( 'NONE',  ( -0.1998031496062994405, 0.3460692066303957537, -1.349737532808398921 ) ) ;
#79953 = CARTESIAN_POINT ( 'NONE',  ( -0.3460692066303960313, 0.1998031496062989965, -0.5754593175853018883 ) ) ;
#79954 = CARTESIAN_POINT ( 'NONE',  ( -0.6758530183727028406, -0.5511811023622048555, -0.09757992244046775898 ) ) ;
#79955 = CARTESIAN_POINT ( 'NONE',  ( -0.5774278215223089816, 0.2306618581243847221, -0.2411417322834647770 ) ) ;
#79956 = CARTESIAN_POINT ( 'NONE',  ( -0.1265901696524993347, 0.4724409448818895907, -0.1640419947506561726 ) ) ;
#79957 = CARTESIAN_POINT ( 'NONE',  ( -0.1958661417322836718, 0.3392501089628017219, -2.459973753280839670 ) ) ;
#79958 = CARTESIAN_POINT ( 'NONE',  ( -1.430446194225720724, -0.004921259842519870586, -0.3153832671262229437 ) ) ;
#79959 = CARTESIAN_POINT ( 'NONE',  ( 0.6889763779527563470, 0.1660481256975883668, -0.3530559997133364547 ) ) ;
#79960 = CARTESIAN_POINT ( 'NONE',  ( 0.9251968503937015864, 0.1660481256975883668, -0.3530559997133364547 ) ) ;
#79961 = CARTESIAN_POINT ( 'NONE',  ( -0.6627296587926501115, 0.1771653543307087075, -0.09757992244046823083 ) ) ;
#79962 = CARTESIAN_POINT ( 'NONE',  ( 0.1968503937007881344, 0.2952755905511811885, 0.000000000000000000 ) ) ;
#79963 = CARTESIAN_POINT ( 'NONE',  ( 5.785732909357575061E-17, -0.4724409448818898682, -1.730314960629921517 ) ) ;
#79964 = CARTESIAN_POINT ( 'NONE',  ( -0.1312335958005241554, -0.5023911411419708095, -0.1820866141732282451 ) ) ;
#79965 = CARTESIAN_POINT ( 'NONE',  ( -0.5643044619422565855, 0.05413385826771626580, -0.4176697321401330321 ) ) ;
#79966 = CARTESIAN_POINT ( 'NONE',  ( 0.2891555358219910499, 0.2891555358219910499, -1.631889763779527991 ) ) ;
#79967 = CARTESIAN_POINT ( 'NONE',  ( 1.509186351706037543, -0.3690944881889765550, -0.3153832671262227771 ) ) ;
#79968 = CARTESIAN_POINT ( 'NONE',  ( 0.07217847769028949700, -0.08942795157528024563, -0.3641732283464568787 ) ) ;
#79969 = CARTESIAN_POINT ( 'NONE',  ( 1.581364829396326277, -0.2845877964562161244, -0.3641732283464567121 ) ) ;
#79970 = CARTESIAN_POINT ( 'NONE',  ( -1.102362204724408601, -0.1870078740157479769, 0.4822834645669291653 ) ) ;
#79971 = CARTESIAN_POINT ( 'NONE',  ( -0.6233595800524928121, -0.2845877964562161244, -0.3641732283464567121 ) ) ;
#79972 = LINE ( 'NONE', #47946, #50653 ) ;
#79973 = CARTESIAN_POINT ( 'NONE',  ( -1.076115485564303809, 0.2306618581243848609, 0.2411417322834645549 ) ) ;
#79974 = CARTESIAN_POINT ( 'NONE',  ( -0.2099737532808391705, 0.2306618581243848609, 0.2411417322834645549 ) ) ;
#79975 = CARTESIAN_POINT ( 'NONE',  ( 4.893765752498283308E-17, -0.3996062992125985480, -2.675196850393700920 ) ) ;
#79976 = CARTESIAN_POINT ( 'NONE',  ( -0.1049643490035306742, 0.3917322834645668994, -2.291319266895325946 ) ) ;
#79977 = CARTESIAN_POINT ( 'NONE',  ( -1.939486441909048509, 1.160811571118562702, -0.2889173282905337925 ) ) ;
#79978 = CARTESIAN_POINT ( 'NONE',  ( 0.1968503937007881344, -0.5511811023622047445, 6.969142054262312111E-17 ) ) ;
#79979 = CARTESIAN_POINT ( 'NONE',  ( 1.148293963254593653, 0.2952755905511810774, -0.1292274648535930714 ) ) ;
#79980 = CARTESIAN_POINT ( 'NONE',  ( -1.062992125984250968, 0.1771653543307087630, 0.000000000000000000 ) ) ;
#79981 = CARTESIAN_POINT ( 'NONE',  ( 1.062992125984252745, 0.2952755905511811885, 0.000000000000000000 ) ) ;
#79982 = CARTESIAN_POINT ( 'NONE',  ( -1.568241469816272105, -0.08942795157527998196, 0.3641732283464567121 ) ) ;
#79983 = CARTESIAN_POINT ( 'NONE',  ( -0.6233595800524928121, -0.05778040916215522460, 0.4822834645669289988 ) ) ;
#79984 = CARTESIAN_POINT ( 'NONE',  ( 0.05905511811023709395, -0.4536011799217367080, 0.2665933059059888421 ) ) ;
#79985 = DIRECTION ( 'NONE',  ( 0.000000000000000000, -1.000000000000000000, 0.000000000000000000 ) ) ;
#79986 = CARTESIAN_POINT ( 'NONE',  ( 0.7611548556430451917, -0.5023911411419708095, 0.1820866141732285504 ) ) ;
#79987 = ORIENTED_EDGE ( 'NONE', *, *, #43286, .F. ) ;
#79988 = EDGE_CURVE ( 'NONE', #9295, #3606, #48476, .T. ) ;
#79989 = CARTESIAN_POINT ( 'NONE',  ( -0.08530183727034056085, -0.3162353388693405765, 0.4822834645669290543 ) ) ;
#79990 = CARTESIAN_POINT ( 'NONE',  ( 0.3996062992125985480, 2.446882876249141654E-17, -0.3523622047244094335 ) ) ;
#79991 = CARTESIAN_POINT ( 'NONE',  ( -0.9055118110236215490, 0.2952755905511811885, 0.000000000000000000 ) ) ;
#79992 = CARTESIAN_POINT ( 'NONE',  ( -9.594673741351313045E-17, 0.3917322834645670104, -1.974409448818897683 ) ) ;
#79993 = CARTESIAN_POINT ( 'NONE',  ( 1.017060367454068581, -0.08942795157528024563, -0.3641732283464568787 ) ) ;
#79994 = CARTESIAN_POINT ( 'NONE',  ( -0.1049868766404193215, -0.6046776061558807314, 0.2411417322834647770 ) ) ;
#79995 = CARTESIAN_POINT ( 'NONE',  ( -0.1640419947506553400, -0.05778040916215560624, -0.4822834645669293319 ) ) ;
#79996 = CARTESIAN_POINT ( 'NONE',  ( -0.5511811023622038563, -0.1870078740157479769, 0.3641732283464567677 ) ) ;
#79997 = CARTESIAN_POINT ( 'NONE',  ( 1.213910761154856299, 0.2952755905511811885, 0.1292274648535926551 ) ) ;
#79998 = CARTESIAN_POINT ( 'NONE',  ( -0.2821522309711278487, -0.5511811023622048555, -0.09757992244046775898 ) ) ;
#79999 = CARTESIAN_POINT ( 'NONE',  ( 0.2165354330708668673, -0.5400638737290844871, 0.3530559997133364547 ) ) ;
#80000 = CARTESIAN_POINT ( 'NONE',  ( -0.6561679790026240244, -0.5023911411419708095, 0.1820866141732285504 ) ) ;
#80002 = CARTESIAN_POINT ( 'NONE',  ( -0.1998031496062994405, 0.3460692066303957537, -1.034776902887139194 ) ) ;
#80001 = AXIS2_PLACEMENT_3D ( 'NONE', #31767, #623, #64589 ) ;
#80003 = CARTESIAN_POINT ( 'NONE',  ( -1.318897637795274802, 0.1660481256975885056, 0.3530559997133364547 ) ) ;
#80004 = DIRECTION ( 'NONE',  ( 0.000000000000000000, -1.000000000000000000, 0.000000000000000000 ) ) ;
#80005 = ORIENTED_EDGE ( 'NONE', *, *, #22645, .T. ) ;
#80006 = CARTESIAN_POINT ( 'NONE',  ( -1.200787401574802349, 0.07958543189024071263, -0.2665933059059888421 ) ) ;
#80007 = CARTESIAN_POINT ( 'NONE',  ( -0.5314960629921254842, -0.5400638737290845981, -0.3530559997133363437 ) ) ;
#80008 = CARTESIAN_POINT ( 'NONE',  ( -1.522309711286088607, 0.2306618581243847221, -0.2411417322834647770 ) ) ;
#80009 = CARTESIAN_POINT ( 'NONE',  ( -1.246719160104985846, -0.4281496062992127816, -0.4176697321401328100 ) ) ;
#80010 = CARTESIAN_POINT ( 'NONE',  ( 1.161417322834646493, -0.5400638737290844871, 0.3530559997133364547 ) ) ;
#80011 = CARTESIAN_POINT ( 'NONE',  ( 0.9186351706036752773, 0.2306618581243847221, -0.2411417322834647770 ) ) ;
#80012 = CARTESIAN_POINT ( 'NONE',  ( -0.3917322834645670104, -7.196005306013484475E-17, -2.708661417322834275 ) ) ;
#80013 = CARTESIAN_POINT ( 'NONE',  ( 1.417322834645670104, -0.1870078740157479769, 0.3641732283464567677 ) ) ;
#80014 = CARTESIAN_POINT ( 'NONE',  ( -0.3996062992125987146, 0.1070741851644051862, -0.3477690288713909950 ) ) ;
#80015 = ORIENTED_EDGE ( 'NONE', *, *, #41924, .F. ) ;
#80016 = CARTESIAN_POINT ( 'NONE',  ( -0.4002624671916004129, -0.2845877964562159024, 0.3641732283464567677 ) ) ;
#80017 = CARTESIAN_POINT ( 'NONE',  ( -0.1049643490035307020, 0.3917322834645669549, -2.360892388451444113 ) ) ;
#80018 = ORIENTED_EDGE ( 'NONE', *, *, #71612, .T. ) ;
#80019 = CARTESIAN_POINT ( 'NONE',  ( 0.7349081364829402885, -0.6046776061558809534, -0.2411417322834644161 ) ) ;
#80020 = CARTESIAN_POINT ( 'NONE',  ( -0.3018372703412066094, 0.05413385826771666132, 0.4176697321401328100 ) ) ;
#80021 = CARTESIAN_POINT ( 'NONE',  ( -0.6955380577427815458, 0.05413385826771666132, 0.4176697321401328100 ) ) ;
#80022 = CARTESIAN_POINT ( 'NONE',  ( 1.463254593175853824, -0.6692913385826771977, 0.1292274648535927661 ) ) ;
#80023 = CARTESIAN_POINT ( 'NONE',  ( -1.207349081364828436, -0.5023911411419708095, 0.1820866141732285504 ) ) ;
#80024 = CARTESIAN_POINT ( 'NONE',  ( 0.04801148344178311073, 1.065401592510863971, -1.490017649659075571 ) ) ;
#80025 = CARTESIAN_POINT ( 'NONE',  ( 0.3018372703412079971, 0.05413385826771626580, -0.4176697321401330321 ) ) ;
#80026 = CARTESIAN_POINT ( 'NONE',  ( -0.8530183727034112984, 0.05413385826771666132, 0.4176697321401328100 ) ) ;
#80027 = CARTESIAN_POINT ( 'NONE',  ( 0.3392501089628018329, 0.1958661417322835052, -1.628589608102675390 ) ) ;
#80028 = CARTESIAN_POINT ( 'NONE',  ( -1.095800524934382292, -0.3162353388693409650, -0.4822834645669289433 ) ) ;
#80029 = CARTESIAN_POINT ( 'NONE',  ( 2.787279214012418738, 0.000000000000000000, 0.000000000000000000 ) ) ;
#80030 = CARTESIAN_POINT ( 'NONE',  ( 0.8727034120734913358, -0.05778040916215522460, 0.4822834645669289988 ) ) ;
#80031 = CARTESIAN_POINT ( 'NONE',  ( 1.377952755905512472, 0.1771653543307087630, 0.000000000000000000 ) ) ;
#80032 = ORIENTED_EDGE ( 'NONE', *, *, #79536, .F. ) ;
#80033 = CARTESIAN_POINT ( 'NONE',  ( 0.3392501089628018884, -0.1958661417322833942, -2.778890706857954473 ) ) ;
#80034 = CARTESIAN_POINT ( 'NONE',  ( -0.2559055118110227234, -0.5400638737290844871, 0.3530559997133364547 ) ) ;
#80035 = ORIENTED_EDGE ( 'NONE', *, *, #59891, .F. ) ;
#80036 = CARTESIAN_POINT ( 'NONE',  ( 0.4068241469816279987, -0.3690944881889765550, -0.3153832671262227771 ) ) ;
#80037 = CARTESIAN_POINT ( 'NONE',  ( -1.240157480314959759, 0.1660481256975885056, 0.3530559997133364547 ) ) ;
#80038 = CARTESIAN_POINT ( 'NONE',  ( 1.108923884514436242, -0.05778040916215522460, 0.4822834645669289988 ) ) ;
#80039 = CARTESIAN_POINT ( 'NONE',  ( 0.9908136482939640111, 0.2952755905511810774, -0.1292274648535930714 ) ) ;
#80040 =( BOUNDED_CURVE ( )  B_SPLINE_CURVE ( 2, ( #16669, #27615, #46961, #28031, #3197, #68006, #35184, #9511, #16252, #9924, #15003, #66770, #28861 ),
 .UNSPECIFIED., .F., .F. ) 
 B_SPLINE_CURVE_WITH_KNOTS ( ( 3, 2, 2, 2, 2, 2, 3 ),
 ( 0.7649423569342326257, 0.7651515151515151381, 0.7689393939393939226, 0.7727272727272727071, 0.7765151515151514916, 0.7803030303030302761, 0.7805121885203127885 ),
 .UNSPECIFIED. ) 
 CURVE ( )  GEOMETRIC_REPRESENTATION_ITEM ( )  RATIONAL_B_SPLINE_CURVE ( ( 0.9964447847208419695, 0.9981185001348091834, 1.000000000000000000, 0.9659258262890683122, 1.000000000000000000, 0.9659258262890683122, 1.000000000000000000, 0.9659258262890683122, 1.000000000000000000, 0.9659258262890683122, 1.000000000000000000, 0.9981185001348091834, 0.9964447847208420805 ) ) 
 REPRESENTATION_ITEM ( '' )  );
#80041 = CARTESIAN_POINT ( 'NONE',  ( -0.03937007874015669567, -0.6692913385826771977, 8.415575281601705876E-17 ) ) ;
#80042 = CARTESIAN_POINT ( 'NONE',  ( 0.2867679344610366554, -0.2867679344610365999, -1.355006192422259170 ) ) ;
#80043 = CARTESIAN_POINT ( 'NONE',  ( -0.7217847769028863381, -0.4281496062992124485, 0.4176697321401328655 ) ) ;
#80044 = CARTESIAN_POINT ( 'NONE',  ( 0.2867679344610365999, -0.2867679344610365444, -2.387795275590551380 ) ) ;
#80045 = CARTESIAN_POINT ( 'NONE',  ( -1.581364829396324945, -0.3162353388693405765, 0.4822834645669290543 ) ) ;
#80046 = CARTESIAN_POINT ( 'NONE',  ( -0.5380577427821514602, 0.05413385826771666132, 0.4176697321401328100 ) ) ;
#80047 = CARTESIAN_POINT ( 'NONE',  ( -0.3871391076115476282, -0.08942795157527998196, 0.3641732283464567121 ) ) ;
#80048 = CARTESIAN_POINT ( 'NONE',  ( 1.410761154855643795, -0.05778040916215560624, -0.4822834645669293319 ) ) ;
#80049 = CARTESIAN_POINT ( 'NONE',  ( 1.666666666666667185, 0.05413385826771666132, 0.4176697321401328100 ) ) ;
#80050 = CARTESIAN_POINT ( 'NONE',  ( -1.089238845144356427, 0.05413385826771666132, 0.4176697321401328100 ) ) ;
#80051 = CARTESIAN_POINT ( 'NONE',  ( -0.1070741851644056997, 0.3996062992125984925, 0.2316272965879264956 ) ) ;
#80052 = CARTESIAN_POINT ( 'NONE',  ( 0.8858267716535438430, -0.5400638737290845981, -0.3530559997133363437 ) ) ;
#80053 = CARTESIAN_POINT ( 'NONE',  ( -0.3460692066303958092, -0.1998031496062994683, -1.942257217847769057 ) ) ;
#80054 = CARTESIAN_POINT ( 'NONE',  ( 1.614173228346457378, 1.055049524192302357, 0.1372047244094478369 ) ) ;
#80055 = CARTESIAN_POINT ( 'NONE',  ( -0.09186351706036663400, -0.4281496062992124485, 0.4176697321401328655 ) ) ;
#80056 = VECTOR ( 'NONE', #5108, 39.37007874015748143 ) ;
#80057 = CARTESIAN_POINT ( 'NONE',  ( -0.9973753280839886548, 0.1283753931104748280, 0.1820866141732283561 ) ) ;
#80058 = CARTESIAN_POINT ( 'NONE',  ( 0.5839895013123367340, 0.1771653543307087630, 0.09757992244046791164 ) ) ;
#80059 = CARTESIAN_POINT ( 'NONE',  ( -0.4724409448818895907, -0.1265901696524993070, -0.7526246719160103460 ) ) ;
#80060 = CARTESIAN_POINT ( 'NONE',  ( 1.102362204724410155, -0.1870078740157480601, -0.3641732283464567677 ) ) ;
#80061 = EDGE_CURVE ( 'NONE', #64262, #6368, #62345, .T. ) ;
#80062 = CARTESIAN_POINT ( 'NONE',  ( 0.9186351706036751663, -0.6046776061558807314, 0.2411417322834647770 ) ) ;
#80063 = CARTESIAN_POINT ( 'NONE',  ( -0.3420746716998662729, 0.1974969037888702206, -0.5754593175853018883 ) ) ;
#80064 = CARTESIAN_POINT ( 'NONE',  ( -0.2690288713910754526, 0.2952755905511810774, -0.1292274648535930714 ) ) ;
#80065 = CARTESIAN_POINT ( 'NONE',  ( 0.3149606299212737159, 2.165354330708661568, -3.924389226575467404 ) ) ;
#80066 = CARTESIAN_POINT ( 'NONE',  ( 1.246719160104987623, -0.3690944881889763329, 0.3153832671262228327 ) ) ;
#80067 = CARTESIAN_POINT ( 'NONE',  ( -0.3805774278215216522, -0.4281496062992127816, -0.4176697321401328100 ) ) ;
#80068 = EDGE_CURVE ( 'NONE', #78176, #27965, #36410, .T. ) ;
#80069 = CARTESIAN_POINT ( 'NONE',  ( -0.2891555358219909388, -0.2891555358219912164, -0.4507874015748032925 ) ) ;
#80070 = CARTESIAN_POINT ( 'NONE',  ( 1.305774278215223960, -0.6692913385826771977, 0.1292274648535927661 ) ) ;
#80071 = CARTESIAN_POINT ( 'NONE',  ( 0.006561679790026889343, -0.05778040916215522460, 0.4822834645669289988 ) ) ;
#80072 = CARTESIAN_POINT ( 'NONE',  ( 0.4330708661417329575, 0.1771653543307087630, 0.000000000000000000 ) ) ;
#80073 = CARTESIAN_POINT ( 'NONE',  ( -0.2120393137889660107, 1.111861684530155658, -1.102218936792509485 ) ) ;
#80074 = CARTESIAN_POINT ( 'NONE',  ( 0.4593175853018380828, -0.004921259842519870586, -0.3153832671262229437 ) ) ;
#80075 = CARTESIAN_POINT ( 'NONE',  ( -1.062992125984250968, 0.2066929133858268208, 0.000000000000000000 ) ) ;
#80076 = CARTESIAN_POINT ( 'NONE',  ( 0.1070741851644053388, 0.3996062992125986035, -1.172572178477690352 ) ) ;
#80077 = CARTESIAN_POINT ( 'NONE',  ( 0.6758530183727039509, -0.6692913385826771977, 0.1292274648535927661 ) ) ;
#80078 = CARTESIAN_POINT ( 'NONE',  ( 4.797336870675656522E-17, -0.3917322834645670104, -1.173228346456692828 ) ) ;
#80079 = CARTESIAN_POINT ( 'NONE',  ( 1.450131233595801428, -0.5511811023622048555, -0.09757992244046775898 ) ) ;
#80080 = CARTESIAN_POINT ( 'NONE',  ( -0.2263583204867699317, -0.3204081651523066343, -2.110585413283051508E-17 ) ) ;
#80081 = CARTESIAN_POINT ( 'NONE',  ( 0.09186351706036799403, -0.3690944881889765550, -0.3153832671262227771 ) ) ;
#80082 = CARTESIAN_POINT ( 'NONE',  ( 0.06561679790026316017, -0.4281496062992124485, 0.4176697321401328655 ) ) ;
#80083 = CARTESIAN_POINT ( 'NONE',  ( 1.423884514435696413, -0.2845877964562161244, -0.3641732283464567121 ) ) ;
#80084 = CARTESIAN_POINT ( 'NONE',  ( -1.391076115485563758, 0.1283753931104748280, 0.1820866141732283561 ) ) ;
#80085 = CARTESIAN_POINT ( 'NONE',  ( -1.535433070866141225, 0.2952755905511811885, 0.000000000000000000 ) ) ;
#80086 = CARTESIAN_POINT ( 'NONE',  ( 0.5971128608923891301, 0.2952755905511810774, -0.1292274648535930714 ) ) ;
#80087 = CARTESIAN_POINT ( 'NONE',  ( 1.200787401574803681, 0.1660481256975885056, 0.3530559997133364547 ) ) ;
#80088 = DIRECTION ( 'NONE',  ( 1.000000000000000000, -0.000000000000000000, -0.000000000000000000 ) ) ;
#80089 = CARTESIAN_POINT ( 'NONE',  ( 0.4461942257217855201, -0.6046776061558807314, 0.2411417322834647770 ) ) ;
#80090 = CARTESIAN_POINT ( 'NONE',  ( 1.253280839895013710, -0.05778040916215560624, -0.4822834645669293319 ) ) ;
#80091 = CARTESIAN_POINT ( 'NONE',  ( 1.023622047244095334, -0.1870078740157479769, 0.4822834645669291653 ) ) ;
#80092 = LINE ( 'NONE', #9368, #54765 ) ;
#80093 = CARTESIAN_POINT ( 'NONE',  ( 0.7677165354330716118, 0.07958543189024071263, -0.2665933059059888421 ) ) ;
#80094 = CARTESIAN_POINT ( 'NONE',  ( 1.581364829396326277, -0.3162353388693409650, -0.4822834645669289433 ) ) ;
#80095 = CARTESIAN_POINT ( 'NONE',  ( -0.9842519685039360366, 0.1771653543307087630, 0.000000000000000000 ) ) ;
#80096 = EDGE_CURVE ( 'NONE', #67621, #57422, #42735, .T. ) ;
#80097 = CARTESIAN_POINT ( 'NONE',  ( 0.3871391076115492380, -0.08942795157528024563, -0.3641732283464568787 ) ) ;
#80098 = CARTESIAN_POINT ( 'NONE',  ( 0.2296587926509192634, -0.3162353388693405765, 0.4822834645669290543 ) ) ;
#80099 = CARTESIAN_POINT ( 'NONE',  ( 0.6824146981627303710, 0.2306618581243847221, -0.2411417322834647770 ) ) ;
#80100 = CARTESIAN_POINT ( 'NONE',  ( -0.4986876640419939388, 0.2306618581243847221, -0.2411417322834647770 ) ) ;
#80101 = CARTESIAN_POINT ( 'NONE',  ( 0.2165354330708668673, 0.07958543189024071263, -0.2665933059059888421 ) ) ;
#80102 = CARTESIAN_POINT ( 'NONE',  ( 0.7677165354330716118, -0.5400638737290844871, 0.3530559997133364547 ) ) ;
#80103 = DIRECTION ( 'NONE',  ( 1.000000000000000000, 0.000000000000000000, -0.000000000000000000 ) ) ;
#80104 = CARTESIAN_POINT ( 'NONE',  ( -0.7677165354330699465, 0.1660481256975885056, 0.3530559997133364547 ) ) ;
#80106 = CARTESIAN_POINT ( 'NONE',  ( 0.3460692066303959202, 0.1998031496062993295, -0.6036745406824146620 ) ) ;
#80105 = FACE_BOUND ( 'NONE', #4225, .T. ) ;
#80107 = CARTESIAN_POINT ( 'NONE',  ( 1.011202504342157527, 9.477779430591278127E-17, -0.3464511005275205946 ) ) ;
#80109 = AXIS2_PLACEMENT_3D ( 'NONE', #66682, #79733, #27113 ) ;
#80108 = CARTESIAN_POINT ( 'NONE',  ( -0.7742782152230962556, -0.4281496062992127816, -0.4176697321401328100 ) ) ;
#80110 = CARTESIAN_POINT ( 'NONE',  ( -0.6430446194225716283, -0.4281496062992124485, 0.4176697321401328655 ) ) ;
#80111 = CARTESIAN_POINT ( 'NONE',  ( -0.2362204724409451284, 0.4091458600556402425, -0.01312335958005249326 ) ) ;
#80112 = CARTESIAN_POINT ( 'NONE',  ( -0.3949938075777409408, -0.1058382717557502933, -2.250656167979002920 ) ) ;
#80113 = ORIENTED_EDGE ( 'NONE', *, *, #55755, .F. ) ;
#80114 = CARTESIAN_POINT ( 'NONE',  ( 0.7545931758530189937, 0.1771653543307087075, -0.09757992244046823083 ) ) ;
#80115 = CARTESIAN_POINT ( 'NONE',  ( 0.1049643490035303689, 0.3917322834645670104, -0.7729658792650916377 ) ) ;
#80116 = CARTESIAN_POINT ( 'NONE',  ( 1.181102362204724976, -0.1870078740157480879, -0.4822834645669291653 ) ) ;
#80117 = CARTESIAN_POINT ( 'NONE',  ( 1.191111281560510715, -4.927456884911482678E-16, 0.4445507791589062840 ) ) ;
#80118 = CARTESIAN_POINT ( 'NONE',  ( -1.345144356955379816, -0.08942795157528024563, -0.3641732283464568787 ) ) ;
#80119 = CARTESIAN_POINT ( 'NONE',  ( 1.456692913385827515, -0.6692913385826771977, 8.415575281601705876E-17 ) ) ;
#80120 = CARTESIAN_POINT ( 'NONE',  ( -1.463254593175852492, -0.6692913385826773087, -0.1292274648535924053 ) ) ;
#80121 = CARTESIAN_POINT ( 'NONE',  ( 0.3543307086614181922, -0.6692913385826771977, 8.415575281601705876E-17 ) ) ;
#80122 = CARTESIAN_POINT ( 'NONE',  ( 0.3917322834645668994, 0.1049643490035304522, -0.2047050936669798094 ) ) ;
#80123 = CARTESIAN_POINT ( 'NONE',  ( 0.05905511811023709395, -0.5400638737290844871, 0.3530559997133364547 ) ) ;
#80124 = CARTESIAN_POINT ( 'NONE',  ( -0.7086614173228339419, -0.1870078740157480601, -0.3641732283464567677 ) ) ;
#80125 = CARTESIAN_POINT ( 'NONE',  ( 1.043307086614173818, -0.5400638737290845981, -0.3530559997133363437 ) ) ;
#80126 = CARTESIAN_POINT ( 'NONE',  ( -0.01968503937007793844, -0.5400638737290844871, 0.3530559997133364547 ) ) ;
#80127 = PLANE ( 'NONE',  #50214 ) ;
#80128 = CARTESIAN_POINT ( 'NONE',  ( -0.01033912696139454093, 1.702998256715020864E-15, -0.4281989832122450323 ) ) ;
#80129 = CARTESIAN_POINT ( 'NONE',  ( -0.2867679344610365444, -0.2867679344610367664, -1.473116428642731401 ) ) ;
#80130 = CARTESIAN_POINT ( 'NONE',  ( 1.036745406824147731, 0.05413385826771666132, 0.4176697321401328100 ) ) ;
#80131 = CARTESIAN_POINT ( 'NONE',  ( 0.2755905511811031494, -0.6692913385826771977, 8.415575281601705876E-17 ) ) ;
#80132 = CARTESIAN_POINT ( 'NONE',  ( -1.135170603674539924, 0.2952755905511810774, -0.1292274648535930714 ) ) ;
#80133 = CARTESIAN_POINT ( 'NONE',  ( 1.240157480314961314, -0.5400638737290844871, 0.3530559997133364547 ) ) ;
#80134 = CARTESIAN_POINT ( 'NONE',  ( 0.2755905511811031494, 0.2952755905511811885, 0.000000000000000000 ) ) ;
#80135 = CARTESIAN_POINT ( 'NONE',  ( 4.797336870675656522E-17, -0.3917322834645670104, -0.7933070866141732624 ) ) ;
#80136 = CARTESIAN_POINT ( 'NONE',  ( -0.2755905511811018171, 0.2952755905511811885, 0.000000000000000000 ) ) ;
#80137 = CARTESIAN_POINT ( 'NONE',  ( 0.7020997375328090762, -0.3162353388693405765, 0.4822834645669290543 ) ) ;
#80138 = CARTESIAN_POINT ( 'NONE',  ( 0.05249343832021075018, -0.6046776061558807314, 0.2411417322834647770 ) ) ;
#80139 = CARTESIAN_POINT ( 'NONE',  ( 0.8661417322834653598, -0.1870078740157479769, 0.3641732283464567677 ) ) ;
#80140 = CARTESIAN_POINT ( 'NONE',  ( -1.220472440944881054, 0.2952755905511811885, 0.000000000000000000 ) ) ;
#80141 = CARTESIAN_POINT ( 'NONE',  ( -0.08529443231573714812, 1.070420337342310235, -2.867136178046102657 ) ) ;
#80142 = CARTESIAN_POINT ( 'NONE',  ( 0.2165354330708668673, 0.1660481256975883668, -0.3530559997133364547 ) ) ;
#80143 =( NAMED_UNIT ( * ) SI_UNIT ( $, .STERADIAN. ) SOLID_ANGLE_UNIT ( ) );
#80144 = CARTESIAN_POINT ( 'NONE',  ( 0.3917322834645670104, -0.1049643490035303411, -2.150918635170603554 ) ) ;
#80145 = EDGE_LOOP ( 'NONE', ( #9422, #24299, #23559, #55057 ) ) ;
#80146 = ORIENTED_EDGE ( 'NONE', *, *, #71791, .F. ) ;
#80147 = AXIS2_PLACEMENT_3D ( 'NONE', #30957, #71341, #76008 ) ;
#80148 = CARTESIAN_POINT ( 'NONE',  ( 1.082677165354331228, 0.1660481256975883668, -0.3530559997133364547 ) ) ;
#80149 = CARTESIAN_POINT ( 'NONE',  ( 0.4855643044619428750, -0.004921259842519576551, 0.3153832671262227771 ) ) ;
#80150 = VECTOR ( 'NONE', #22572, 39.37007874015748143 ) ;
#80151 = AXIS2_PLACEMENT_3D ( 'NONE', #68366, #35956, #10704 ) ;
#80153 = DIRECTION ( 'NONE',  ( 0.000000000000000000, 0.000000000000000000, -1.000000000000000000 ) ) ;
#80152 = LINE ( 'NONE', #15757, #1466 ) ;
#80154 = CARTESIAN_POINT ( 'NONE',  ( 0.4177787735907000921, 0.3937007874015748254, -1.244210979442979648 ) ) ;
#80155 = CARTESIAN_POINT ( 'NONE',  ( 0.3392501089628018884, -0.1958661417322834220, -1.291994750656167978 ) ) ;
#80156 = EDGE_CURVE ( 'NONE', #25851, #34321, #38991, .T. ) ;
#80157 = CARTESIAN_POINT ( 'NONE',  ( 0.1070741851644053388, 0.3996062992125986035, -2.432414698162729039 ) ) ;
#80158 = CARTESIAN_POINT ( 'NONE',  ( -0.9514435695538050464, -0.05778040916215560624, -0.4822834645669293319 ) ) ;
#80159 = CARTESIAN_POINT ( 'NONE',  ( -0.6889763779527552368, -0.5400638737290845981, -0.3530559997133363437 ) ) ;
#80160 = CARTESIAN_POINT ( 'NONE',  ( 0.6889763779527563470, 0.1660481256975883668, -0.3530559997133364547 ) ) ;
#80161 = ORIENTED_EDGE ( 'NONE', *, *, #79009, .T. ) ;
#80162 = CARTESIAN_POINT ( 'NONE',  ( 1.535433070866142335, -0.6692913385826771977, 8.415575281601705876E-17 ) ) ;
#80163 = CARTESIAN_POINT ( 'NONE',  ( 1.660104986876641320, -0.08942795157527998196, 0.3641732283464567121 ) ) ;
#80164 = ITEM_DEFINED_TRANSFORMATION ( 'NONE', 'NONE', #11409,  #22098 ) ;
#80165 = PLANE ( 'NONE',  #43886 ) ;
#80166 = CARTESIAN_POINT ( 'NONE',  ( 0.000000000000000000, 0.7086614173228346081, 0.000000000000000000 ) ) ;
#80167 = CARTESIAN_POINT ( 'NONE',  ( -1.240157480314959759, -0.4536011799217368745, -0.2665933059059886201 ) ) ;
#80168 =( BOUNDED_CURVE ( )  B_SPLINE_CURVE ( 2, ( #42166, #73346, #3464, #67861, #60290, #3878, #16102, #16521, #80500, #2640, #79672, #15693, #10198 ),
 .UNSPECIFIED., .F., .F. ) 
 B_SPLINE_CURVE_WITH_KNOTS ( ( 3, 2, 2, 2, 2, 2, 3 ),
 ( 0.1375000000000000111, 0.1416666666666666630, 0.1458333333333333426, 0.1499999999999999944, 0.1541666666666666741, 0.1583333333333333259, 0.1625000000000000056 ),
 .UNSPECIFIED. ) 
 CURVE ( )  GEOMETRIC_REPRESENTATION_ITEM ( )  RATIONAL_B_SPLINE_CURVE ( ( 1.000000000000000000, 0.9659258262890683122, 1.000000000000000000, 0.9659258262890683122, 1.000000000000000000, 0.9659258262890683122, 1.000000000000000000, 0.9659258262890683122, 1.000000000000000000, 0.9659258262890683122, 1.000000000000000000, 0.9659258262890683122, 1.000000000000000000 ) ) 
 REPRESENTATION_ITEM ( '' )  );
#80169 = CARTESIAN_POINT ( 'NONE',  ( 0.4849061582275016602, 2.793565526369266028, -0.4921425059946356595 ) ) ;
#80170 = CARTESIAN_POINT ( 'NONE',  ( 0.04593175853018440641, -0.6692913385826771977, 0.1292274648535927661 ) ) ;
#80171 = AXIS2_PLACEMENT_3D ( 'NONE', #48143, #9437, #9854 ) ;
#80173 = CYLINDRICAL_SURFACE ( 'NONE', #54633, 0.2165354330708661457 ) ;
#80172 = CARTESIAN_POINT ( 'NONE',  ( 1.371391076115485941, 0.2952755905511811885, 0.1292274648535926551 ) ) ;
#80174 = CARTESIAN_POINT ( 'NONE',  ( -1.299212598425196097, -0.5511811023622047445, 6.969142054262312111E-17 ) ) ;
#80175 = CARTESIAN_POINT ( 'NONE',  ( 0.9645669291338591078, -0.5400638737290845981, -0.3530559997133363437 ) ) ;
#80176 = CARTESIAN_POINT ( 'NONE',  ( 1.272965879265092637, -0.004921259842519576551, 0.3153832671262227771 ) ) ;
#80177 = CARTESIAN_POINT ( 'NONE',  ( -0.2867679344610366554, 0.2867679344610365444, -1.359560736711598938 ) ) ;
#80178 = CARTESIAN_POINT ( 'NONE',  ( -1.154855643044618851, -0.5023911411419708095, -0.1820866141732282451 ) ) ;
#80179 = CARTESIAN_POINT ( 'NONE',  ( 1.299212598425197429, -0.6692913385826771977, 8.415575281601705876E-17 ) ) ;
#80180 = CARTESIAN_POINT ( 'NONE',  ( 0.3116086372737535415, 1.665959576555773314, 0.02998912175037303507 ) ) ;
#80181 = CARTESIAN_POINT ( 'NONE',  ( -0.1312335958005241554, 0.2306618581243848609, 0.2411417322834645549 ) ) ;
#80182 = CARTESIAN_POINT ( 'NONE',  ( -1.141732283464566011, 0.1771653543307087630, 0.000000000000000000 ) ) ;
#80183 = CARTESIAN_POINT ( 'NONE',  ( -0.3280839895013117347, -0.3690944881889763329, 0.3153832671262228327 ) ) ;
#80184 = CARTESIAN_POINT ( 'NONE',  ( -0.6758530183727028406, -0.6692913385826773087, -0.1292274648535924053 ) ) ;
#80185 = CARTESIAN_POINT ( 'NONE',  ( -1.620734908136482577, 0.1771653543307087630, 0.09757992244046791164 ) ) ;
#80186 = CARTESIAN_POINT ( 'NONE',  ( 0.1958661417322836718, -0.3392501089628017219, -0.5610429378290832103 ) ) ;
#80187 = CARTESIAN_POINT ( 'NONE',  ( 0.2755905511811031494, -0.6692913385826771977, 8.415575281601705876E-17 ) ) ;
#80188 = CARTESIAN_POINT ( 'NONE',  ( -0.4724409448818898682, -8.678599364036362592E-17, -0.1968503937007874127 ) ) ;
#80189 = CARTESIAN_POINT ( 'NONE',  ( -0.1265901696524993347, 0.4724409448818895907, -1.500656167979002031 ) ) ;
#80190 = CARTESIAN_POINT ( 'NONE',  ( -1.325459317585300889, -0.4281496062992127816, -0.4176697321401328100 ) ) ;
#80191 = CARTESIAN_POINT ( 'NONE',  ( -0.6233595800524928121, -0.08942795157527998196, 0.3641732283464567121 ) ) ;
#80192 = CARTESIAN_POINT ( 'NONE',  ( -0.01312335958005186876, 0.05413385826771626580, -0.4176697321401330321 ) ) ;
#80193 = CARTESIAN_POINT ( 'NONE',  ( 0.4330708661417329575, 0.1771653543307087630, 0.000000000000000000 ) ) ;
#80194 = CARTESIAN_POINT ( 'NONE',  ( -0.9120734908136475250, 0.1771653543307087630, 0.09757992244046791164 ) ) ;
#80195 = CARTESIAN_POINT ( 'NONE',  ( -1.292650918635170010, -0.6692913385826771977, 0.1292274648535927661 ) ) ;
#80196 = CARTESIAN_POINT ( 'NONE',  ( -1.719160104986876103, 0.05413385826771666132, 0.4176697321401328100 ) ) ;
#80197 = CARTESIAN_POINT ( 'NONE',  ( 1.568241469816273659, -0.05778040916215560624, -0.4822834645669293319 ) ) ;
#80198 = CARTESIAN_POINT ( 'NONE',  ( 0.4257672537616556951, 1.326168777627702244, 2.077356831852779528 ) ) ;
#80199 = CARTESIAN_POINT ( 'NONE',  ( 0.9383202099737538715, -0.08942795157528024563, -0.3641732283464568787 ) ) ;
#80200 = CARTESIAN_POINT ( 'NONE',  ( 0.9120734908136490793, 0.2952755905511810774, -0.1292274648535930714 ) ) ;
#80201 = CARTESIAN_POINT ( 'NONE',  ( -0.5387615594602663815, -2.294479370626195693E-15, 0.3464511005275217603 ) ) ;
#80202 = CARTESIAN_POINT ( 'NONE',  ( 1.423884514435696191, -0.08942795157527998196, 0.3641732283464567121 ) ) ;
#80203 = ORIENTED_EDGE ( 'NONE', *, *, #10428, .T. ) ;
#80204 = CARTESIAN_POINT ( 'NONE',  ( -0.6824146981627288167, 0.2306618581243848609, 0.2411417322834645549 ) ) ;
#80205 = CARTESIAN_POINT ( 'NONE',  ( -0.7414698162729651543, -0.6692913385826771977, 0.1292274648535927661 ) ) ;
#80206 = CARTESIAN_POINT ( 'NONE',  ( 0.4855643044619428750, 0.05413385826771666132, 0.4176697321401328100 ) ) ;
#80207 = VECTOR ( 'NONE', #14436, 39.37007874015748143 ) ;
#80208 = CARTESIAN_POINT ( 'NONE',  ( -1.496062992125983815, -0.1870078740157480601, -0.3641732283464567677 ) ) ;
#80209 = CARTESIAN_POINT ( 'NONE',  ( 0.3460692066303958092, 0.1998031496062993018, -2.412729658792650778 ) ) ;
#80210 = CARTESIAN_POINT ( 'NONE',  ( -1.633858267716534529, -0.5400638737290845981, -0.3530559997133363437 ) ) ;
#80211 = CONICAL_SURFACE ( 'NONE', #15683, 1.181102362204724310, 0.7853981633974552734 ) ;
#80212 = CARTESIAN_POINT ( 'NONE',  ( 0.2821522309711292364, 0.2952755905511810774, -0.1292274648535930714 ) ) ;
#80213 = CARTESIAN_POINT ( 'NONE',  ( 0.8333333333333340365, 0.2952755905511810774, -0.1292274648535930714 ) ) ;
#80214 = CARTESIAN_POINT ( 'NONE',  ( -1.595398199321656385, 1.288687073698533414, -0.1559797534342482195 ) ) ;
#80215 = CARTESIAN_POINT ( 'NONE',  ( 0.1998031496062992740, 0.3460692066303959757, -1.719160104986876769 ) ) ;
#80216 = CARTESIAN_POINT ( 'NONE',  ( -0.1058382717557503211, 0.3949938075777409408, -1.266404199475065440 ) ) ;
#80217 = CARTESIAN_POINT ( 'NONE',  ( -0.1070741851644051862, -0.3996062992125987146, -2.591863517060367439 ) ) ;
#80218 = DIRECTION ( 'NONE',  ( -0.000000000000000000, 1.000000000000000000, -0.000000000000000000 ) ) ;
#80219 = CARTESIAN_POINT ( 'NONE',  ( 0.1958661417322834775, 0.3392501089628018884, -0.2939632545931757934 ) ) ;
#80220 = CARTESIAN_POINT ( 'NONE',  ( 0.05905511811023681640, 0.07958543189024071263, -0.2665933059059888421 ) ) ;
#80221 = CARTESIAN_POINT ( 'NONE',  ( -0.3412073490813641308, -0.6046776061558807314, 0.2411417322834647770 ) ) ;
#80222 = CARTESIAN_POINT ( 'NONE',  ( 0.6889763779527563470, 0.1660481256975883668, -0.3530559997133364547 ) ) ;
#80223 = CARTESIAN_POINT ( 'NONE',  ( -0.3420746716998662729, 0.1974969037888702206, -1.992782152230971882 ) ) ;
#80224 = CARTESIAN_POINT ( 'NONE',  ( 0.02624671916010564918, -0.5023911411419708095, -0.1820866141732282451 ) ) ;
#80225 = CARTESIAN_POINT ( 'NONE',  ( -1.358267716535432434, -0.5400638737290844871, 0.3530559997133364547 ) ) ;
#80226 = CARTESIAN_POINT ( 'NONE',  ( 1.181102362204724976, -0.1870078740157480879, -0.4822834645669291653 ) ) ;
#80227 = CARTESIAN_POINT ( 'NONE',  ( 0.3458507752293908943, 0.3458507752293908943, -2.342519685039369914 ) ) ;
#80228 = CARTESIAN_POINT ( 'NONE',  ( -0.2925321140481932924, 0.2925321140481931814, -1.594488188976378229 ) ) ;
#80229 = CARTESIAN_POINT ( 'NONE',  ( 0.08874907683610111508, -2.191421614605370878E-15, 0.4445507791589071167 ) ) ;
#80230 = AXIS2_PLACEMENT_3D ( 'NONE', #40178, #73421, #54453 ) ;
#80231 = EDGE_LOOP ( 'NONE', ( #37843, #76487, #53817, #18106 ) ) ;
#80232 = ORIENTED_EDGE ( 'NONE', *, *, #49009, .T. ) ;
#80233 = CARTESIAN_POINT ( 'NONE',  ( 0.8464566929133865436, 0.1660481256975883668, -0.3530559997133364547 ) ) ;
#80234 = CARTESIAN_POINT ( 'NONE',  ( -1.515748031496062076, 0.1660481256975883668, -0.3530559997133364547 ) ) ;
#80236 = CARTESIAN_POINT ( 'NONE',  ( 1.489501312335958172, -0.05778040916215560624, -0.4822834645669293319 ) ) ;
#80235 = CARTESIAN_POINT ( 'NONE',  ( -1.272965879265091305, -0.004921259842519870586, -0.3153832671262229437 ) ) ;
#80237 = CARTESIAN_POINT ( 'NONE',  ( -0.2867679344610364334, -0.2867679344610368219, -2.816253650097426231 ) ) ;
#80238 = CARTESIAN_POINT ( 'NONE',  ( 1.220472440944882164, -0.1870078740157480046, 1.254653134982923898E-17 ) ) ;
#80239 = CARTESIAN_POINT ( 'NONE',  ( 1.437007874015748810, -0.5400638737290845981, -0.3530559997133363437 ) ) ;
#80240 = CARTESIAN_POINT ( 'NONE',  ( -1.679790026246718693, 0.2306618581243847221, -0.2411417322834647770 ) ) ;
#80241 = CARTESIAN_POINT ( 'NONE',  ( 0.01312335958005323398, 0.05413385826771666132, 0.4176697321401328100 ) ) ;
#80242 = CARTESIAN_POINT ( 'NONE',  ( -0.6561679790026240244, -0.6046776061558807314, 0.2411417322834647770 ) ) ;
#80243 = CARTESIAN_POINT ( 'NONE',  ( 1.522309711286089939, -0.6046776061558809534, -0.2411417322834644161 ) ) ;
#80244 = CARTESIAN_POINT ( 'NONE',  ( 0.2867679344610365999, -0.2867679344610365444, -0.02559055118110245899 ) ) ;
#80245 = ADVANCED_FACE ( 'NONE', ( #23385 ), #37260, .T. ) ;
#80246 = CARTESIAN_POINT ( 'NONE',  ( 0.1246719160104994284, -0.6692913385826771977, 0.1292274648535927661 ) ) ;
#80247 = CARTESIAN_POINT ( 'NONE',  ( 0.1958661417322834775, 0.3392501089628018884, -2.183727034120734878 ) ) ;
#80248 = CARTESIAN_POINT ( 'NONE',  ( -1.115485564304461219, -0.004921259842519870586, -0.3153832671262229437 ) ) ;
#80249 = ORIENTED_EDGE ( 'NONE', *, *, #38804, .F. ) ;
#80250 = CARTESIAN_POINT ( 'NONE',  ( 0.3949938075777409963, 2.418639510665530435E-17, -2.322834645669291209 ) ) ;
#80251 = VERTEX_POINT ( 'NONE', #12006 ) ;
#80252 = CARTESIAN_POINT ( 'NONE',  ( -1.708538945418524024, 1.316053703249684625, 0.4200579243588399292 ) ) ;
#80253 = CARTESIAN_POINT ( 'NONE',  ( -1.463254593175852492, -0.6692913385826773087, -0.1292274648535924053 ) ) ;
#80254 = CARTESIAN_POINT ( 'NONE',  ( -0.3996062992125986035, -0.1070741851644056997, -0.9908136482939633449 ) ) ;
#80255 = CARTESIAN_POINT ( 'NONE',  ( -1.614173228346457378, 2.094556775020298023, 0.1372047244094476981 ) ) ;
#80256 = CARTESIAN_POINT ( 'NONE',  ( -1.548556430446193399, 0.2306618581243848609, 0.2411417322834645549 ) ) ;
#80257 = CARTESIAN_POINT ( 'NONE',  ( -0.4724409448818898682, 5.785732909357575061E-17, -2.755905511811024056 ) ) ;
#80258 = DIRECTION ( 'NONE',  ( 0.000000000000000000, 1.000000000000000000, 0.000000000000000000 ) ) ;
#80259 = CARTESIAN_POINT ( 'NONE',  ( 0.1049643490035303689, 0.3917322834645670104, 0.07939632545931750440 ) ) ;
#80260 = CARTESIAN_POINT ( 'NONE',  ( -0.4921259842519677963, 0.07958543189024071263, -0.2665933059059888421 ) ) ;
#80261 = CARTESIAN_POINT ( 'NONE',  ( -0.8005249343832013809, -0.3690944881889763329, 0.3153832671262228327 ) ) ;
#80262 = CARTESIAN_POINT ( 'NONE',  ( -1.364829396325458521, -0.6046776061558807314, 0.2411417322834647770 ) ) ;
#80263 = CARTESIAN_POINT ( 'NONE',  ( 0.5774278215223103139, -0.6046776061558809534, -0.2411417322834644161 ) ) ;
#80264 = CARTESIAN_POINT ( 'NONE',  ( -1.141732283464566011, 0.2952755905511811885, 0.000000000000000000 ) ) ;
#80265 = CARTESIAN_POINT ( 'NONE',  ( 0.5314960629921394730, 2.745602313593968891, -3.861135848600277143 ) ) ;
#80266 = VERTEX_POINT ( 'NONE', #61696 ) ;
#80267 = CARTESIAN_POINT ( 'NONE',  ( -1.318897637795274802, 0.1660481256975885056, 0.3530559997133364547 ) ) ;
#80268 = CARTESIAN_POINT ( 'NONE',  ( 0.4408028249046178626, 0.2072245076110159345, -0.1100941634872966285 ) ) ;
#80269 = AXIS2_PLACEMENT_3D ( 'NONE', #78648, #60512, #46211 ) ;
#80270 = CARTESIAN_POINT ( 'NONE',  ( -0.1265901696524993347, 0.4724409448818895907, -1.896325459317584894 ) ) ;
#80271 = CARTESIAN_POINT ( 'NONE',  ( -0.2017716535433071445, -0.2017716535433071445, -0.3937007874015748254 ) ) ;
#80272 = CARTESIAN_POINT ( 'NONE',  ( 0.1958661417322836440, -0.3392501089628017219, -0.8713910761154854967 ) ) ;
#80273 = CIRCLE ( 'NONE', #13075, 0.5118110236220472231 ) ;
#80274 = CARTESIAN_POINT ( 'NONE',  ( 0.4687364453271865017, 1.550612376216477184, -0.5180075785470105165 ) ) ;
#80275 = CARTESIAN_POINT ( 'NONE',  ( -0.8661417322834640276, -0.1870078740157479769, 0.4822834645669291653 ) ) ;
#80276 = CARTESIAN_POINT ( 'NONE',  ( 1.482939632545932307, -0.4281496062992124485, 0.4176697321401328655 ) ) ;
#80277 = VECTOR ( 'NONE', #59923, 39.37007874015748143 ) ;
#80279 = CARTESIAN_POINT ( 'NONE',  ( -0.4091458600556402980, -0.2362204724409451284, -1.942257217847769057 ) ) ;
#80278 = CARTESIAN_POINT ( 'NONE',  ( -1.581364829396324945, -0.3162353388693405765, 0.4822834645669290543 ) ) ;
#80280 = CARTESIAN_POINT ( 'NONE',  ( -1.482939632545930975, -0.4281496062992127816, -0.4176697321401328100 ) ) ;
#80281 = CARTESIAN_POINT ( 'NONE',  ( -0.9973753280839886548, -0.6046776061558809534, -0.2411417322834644161 ) ) ;
#80282 = CARTESIAN_POINT ( 'NONE',  ( 0.1049643490035304522, -0.3917322834645668994, 0.1496256149944375224 ) ) ;
#80283 = CARTESIAN_POINT ( 'NONE',  ( 0.2821522309711292364, -0.5511811023622046335, 0.09757992244046803654 ) ) ;
#80284 = CARTESIAN_POINT ( 'NONE',  ( 0.1958661417322834775, 0.3392501089628018884, -0.5439632545931759600 ) ) ;
#80285 = CARTESIAN_POINT ( 'NONE',  ( 0.04593175853018440641, -0.5511811023622046335, 0.09757992244046803654 ) ) ;
#80286 = CARTESIAN_POINT ( 'NONE',  ( 0.8989501312335963501, -0.5511811023622048555, -0.09757992244046775898 ) ) ;
#80287 = CARTESIAN_POINT ( 'NONE',  ( 0.8989501312335963501, -0.6692913385826773087, -0.1292274648535924053 ) ) ;
#80288 = CARTESIAN_POINT ( 'NONE',  ( -0.2559055118110227234, -0.4536011799217367080, 0.2665933059059888421 ) ) ;
#80289 = CARTESIAN_POINT ( 'NONE',  ( -0.1049643490035307020, 0.3917322834645669549, -2.203412073490814027 ) ) ;
#80290 = CARTESIAN_POINT ( 'NONE',  ( 1.555118110236221041, -0.5400638737290844871, 0.3530559997133364547 ) ) ;
#80291 = CARTESIAN_POINT ( 'NONE',  ( -1.338582677165353729, -0.1870078740157479769, 0.3641732283464567677 ) ) ;
#80292 = CARTESIAN_POINT ( 'NONE',  ( 0.4724409448818896462, 0.1265901696524990294, -0.2014435695538057958 ) ) ;
#80293 = CARTESIAN_POINT ( 'NONE',  ( -0.09186351706036689768, 0.05413385826771626580, -0.4176697321401330321 ) ) ;
#80294 = CARTESIAN_POINT ( 'NONE',  ( 0.06561679790026316017, -0.4281496062992124485, 0.4176697321401328655 ) ) ;
#80295 = CARTESIAN_POINT ( 'NONE',  ( 1.502624671916010790, -0.08942795157527998196, 0.3641732283464567121 ) ) ;
#80296 = CARTESIAN_POINT ( 'NONE',  ( 0.5971128608923890191, -0.5511811023622046335, 0.09757992244046803654 ) ) ;
#80297 = CARTESIAN_POINT ( 'NONE',  ( -0.1443569553805768291, -0.004921259842519576551, 0.3153832671262227771 ) ) ;
#80298 = CARTESIAN_POINT ( 'NONE',  ( -0.6233595800524928121, -0.3162353388693409650, -0.4822834645669289433 ) ) ;
#80299 = CARTESIAN_POINT ( 'NONE',  ( 0.000000000000000000, 0.000000000000000000, 0.000000000000000000 ) ) ;
#80300 = CARTESIAN_POINT ( 'NONE',  ( -0.1265901696524993347, 0.4724409448818896462, -1.973097112860892510 ) ) ;
#80301 = CARTESIAN_POINT ( 'NONE',  ( 0.03280839895013198948, -0.6692913385826773087, -0.1292274648535924053 ) ) ;
#80302 = CARTESIAN_POINT ( 'NONE',  ( 0.3996062992125985480, 2.446882876249141654E-17, -1.769685039370078927 ) ) ;
#80303 = CARTESIAN_POINT ( 'NONE',  ( 1.568241469816273437, -0.3162353388693405765, 0.4822834645669290543 ) ) ;
#80304 = CARTESIAN_POINT ( 'NONE',  ( -0.3937007874015740483, -0.1870078740157480601, -0.3641732283464567677 ) ) ;
#80305 = CARTESIAN_POINT ( 'NONE',  ( -0.09842519685039295696, 0.1660481256975883668, -0.3530559997133364547 ) ) ;
#80306 = CARTESIAN_POINT ( 'NONE',  ( -1.377952755905511140, -0.6692913385826771977, 8.415575281601705876E-17 ) ) ;
#80307 = CARTESIAN_POINT ( 'NONE',  ( 1.627296587926509996, -0.6046776061558807314, 0.2411417322834647770 ) ) ;
#80308 = CARTESIAN_POINT ( 'NONE',  ( 1.332020997375329197, -0.3162353388693405765, 0.4822834645669290543 ) ) ;
#80309 = DIRECTION ( 'NONE',  ( -3.491481338843132961E-15, -0.000000000000000000, 1.000000000000000000 ) ) ;
#80310 = CARTESIAN_POINT ( 'NONE',  ( -0.6167979002624665030, -0.004921259842519576551, 0.3153832671262227771 ) ) ;
#80311 = CARTESIAN_POINT ( 'NONE',  ( 0.1998031496062994128, -0.3460692066303957537, -0.3261154855643044748 ) ) ;
#80312 = CARTESIAN_POINT ( 'NONE',  ( -0.3996062992125986035, -7.340648628747425578E-17, -0.3543307086614173040 ) ) ;
#80313 = CARTESIAN_POINT ( 'NONE',  ( -0.3392501089628017219, -0.1958661417322836995, -2.883877583498374531 ) ) ;
#80314 = CARTESIAN_POINT ( 'NONE',  ( 1.430446194225722500, -0.3690944881889765550, -0.3153832671262227771 ) ) ;
#80315 = CARTESIAN_POINT ( 'NONE',  ( 1.272965879265092637, -0.004921259842519576551, 0.3153832671262227771 ) ) ;
#80316 = CARTESIAN_POINT ( 'NONE',  ( -1.686351706036744558, 0.2952755905511810774, -0.1292274648535930714 ) ) ;
#80317 = CARTESIAN_POINT ( 'NONE',  ( 0.6955380577427828781, 0.05413385826771626580, -0.4176697321401330321 ) ) ;
#80318 = CARTESIAN_POINT ( 'NONE',  ( -0.3420746716998660508, -0.1974969037888706924, -0.7591863517060368771 ) ) ;
#80319 = CARTESIAN_POINT ( 'NONE',  ( 1.049868766404200349, 0.1283753931104748280, 0.1820866141732283561 ) ) ;
#80320 = CARTESIAN_POINT ( 'NONE',  ( 0.1115485564304470323, 0.2952755905511811885, 0.1292274648535926551 ) ) ;
#80321 = CARTESIAN_POINT ( 'NONE',  ( -0.9711286089238838626, 0.2306618581243847221, -0.2411417322834647770 ) ) ;
#80322 = CARTESIAN_POINT ( 'NONE',  ( 1.660104986876641320, -0.05778040916215522460, 0.4822834645669289988 ) ) ;
#80323 = AXIS2_PLACEMENT_3D ( 'NONE', #49407, #40310, #48991 ) ;
#80324 = CARTESIAN_POINT ( 'NONE',  ( -0.3458507752293909498, 0.3458507752293907833, -1.122047244094488194 ) ) ;
#80325 = AXIS2_PLACEMENT_3D ( 'NONE', #62709, #74942, #62286 ) ;
#80326 = CARTESIAN_POINT ( 'NONE',  ( 0.2925321140481932369, -0.2925321140481931814, -2.145669291338582418 ) ) ;
#80327 = CARTESIAN_POINT ( 'NONE',  ( 0.4658792650918640033, -0.2845877964562159024, 0.3641732283464567677 ) ) ;
#80328 = ORIENTED_EDGE ( 'NONE', *, *, #55345, .F. ) ;
#80329 = CARTESIAN_POINT ( 'NONE',  ( 0.3392501089628018884, -0.1958661417322833942, -0.5741662974091357174 ) ) ;
#80330 = VERTEX_POINT ( 'NONE', #55364 ) ;
#80331 = CARTESIAN_POINT ( 'NONE',  ( -0.2493438320209966919, 0.05413385826771626580, -0.4176697321401330321 ) ) ;
#80332 = CARTESIAN_POINT ( 'NONE',  ( -0.3608923884514428360, 0.2952755905511811885, 0.1292274648535926551 ) ) ;
#80333 = CARTESIAN_POINT ( 'NONE',  ( -0.4921259842519677963, 0.07958543189024071263, -0.2665933059059888421 ) ) ;
#80334 = CARTESIAN_POINT ( 'NONE',  ( 0.8727034120734913358, -0.05778040916215522460, 0.4822834645669289988 ) ) ;
#80335 = CARTESIAN_POINT ( 'NONE',  ( -1.043307086614172041, -0.5400638737290844871, 0.3530559997133364547 ) ) ;
#80336 = CARTESIAN_POINT ( 'NONE',  ( -0.2755905511811018171, 0.2952755905511811885, 0.000000000000000000 ) ) ;
#80337 = CARTESIAN_POINT ( 'NONE',  ( 1.030183727034121421, -0.3162353388693409650, -0.4822834645669289433 ) ) ;
#80338 = B_SPLINE_CURVE_WITH_KNOTS ( 'NONE', 3,
 ( #2495, #27740, #79113, #40781, #47501, #47086, #2906, #55053, #72776, #53810, #28979, #28155, #66467, #60144, #74025, #60556, #48328, #41609, #8802, #28570, #34478, #34894, #41203, #79523, #21838, #73194, #60964, #79943, #15544, #15962, #9221, #54226, #16371, #35302, #54646, #10048, #35711, #61381, #3730, #63442 ),
 .UNSPECIFIED., .F., .F.,
 ( 4, 2, 2, 2, 2, 2, 2, 2, 2, 2, 2, 2, 2, 2, 2, 2, 2, 2, 2, 4 ),
 ( 0.01443715752414749184, 0.01533768712752721884, 0.01623821673090694584, 0.01713874633428667110, 0.01803927593766639637, 0.01893980554104612510, 0.01984033514442585036, 0.02029059994611567830, 0.02074086474780550277, 0.02119112954949533070, 0.02164139435118515517, 0.02254192395456481104, 0.02344245355794446345, 0.02434298316132411932, 0.02524351276470376826, 0.02614404236808342413, 0.02659430716977325554, 0.02704457197146308001, 0.02794510157484273241, 0.02884563117822238482 ),
 .UNSPECIFIED. ) ;
#80339 = CARTESIAN_POINT ( 'NONE',  ( 0.9514435695538062676, -0.05778040916215522460, 0.4822834645669289988 ) ) ;
#80340 = B_SPLINE_CURVE_WITH_KNOTS ( 'NONE', 3,
 ( #79360, #33894, #7391, #66305 ),
 .UNSPECIFIED., .F., .F.,
 ( 4, 4 ),
 ( 0.1090648859799403791, 0.1105484317322390914 ),
 .UNSPECIFIED. ) ;
#80341 = CARTESIAN_POINT ( 'NONE',  ( 0.8333333333333340365, -0.6692913385826771977, 0.1292274648535927661 ) ) ;
#80342 = CARTESIAN_POINT ( 'NONE',  ( -0.1958661417322836718, 0.3392501089628017219, -1.107611548556430403 ) ) ;
#80343 = CARTESIAN_POINT ( 'NONE',  ( -0.1706036745406816491, -0.004921259842519870586, -0.3153832671262229437 ) ) ;
#80344 = VERTEX_POINT ( 'NONE', #68431 ) ;
#80345 = CARTESIAN_POINT ( 'NONE',  ( -0.1974969037888706647, 0.3420746716998658843, -1.115485564304461885 ) ) ;
#80346 = ORIENTED_EDGE ( 'NONE', *, *, #28821, .T. ) ;
#80347 = CARTESIAN_POINT ( 'NONE',  ( -0.8136482939632537770, -0.5023911411419708095, 0.1820866141732285504 ) ) ;
#80348 = CARTESIAN_POINT ( 'NONE',  ( -0.4724409448818890911, -0.1870078740157480879, -0.4822834645669291653 ) ) ;
#80349 = LINE ( 'NONE', #42010, #40802 ) ;
#80350 = CARTESIAN_POINT ( 'NONE',  ( -0.4330708661417315697, 0.2952755905511811885, 0.000000000000000000 ) ) ;
#80351 = CARTESIAN_POINT ( 'NONE',  ( -0.3215223097112853146, -0.3162353388693405765, 0.4822834645669290543 ) ) ;
#80352 = CARTESIAN_POINT ( 'NONE',  ( -1.102362204724408601, -0.1870078740157480879, -0.4822834645669291653 ) ) ;
#80353 = CARTESIAN_POINT ( 'NONE',  ( -1.581364829396324945, -0.3162353388693405765, 0.4822834645669290543 ) ) ;
#80354 = CARTESIAN_POINT ( 'NONE',  ( 0.8398950131233602345, -0.5023911411419708095, 0.1820866141732285504 ) ) ;
#80355 = CARTESIAN_POINT ( 'NONE',  ( -0.1265901696524993347, 0.4724409448818896462, -0.3982939632545931530 ) ) ;
#80356 = CARTESIAN_POINT ( 'NONE',  ( -0.3458507752293906723, -0.3458507752293910609, -0.6082677165354329896 ) ) ;
#80357 = CARTESIAN_POINT ( 'NONE',  ( 0.5708661417322841158, -0.4536011799217368745, -0.2665933059059886201 ) ) ;
#80358 = CARTESIAN_POINT ( 'NONE',  ( -0.08530183727034056085, -0.3162353388693405765, 0.4822834645669290543 ) ) ;
#80359 = CARTESIAN_POINT ( 'NONE',  ( 0.3543307086614181922, -0.6692913385826771977, 8.415575281601705876E-17 ) ) ;
#80360 = ORIENTED_EDGE ( 'NONE', *, *, #5158, .T. ) ;
#80361 = CARTESIAN_POINT ( 'NONE',  ( -0.3996062992125986035, -0.1070741851644056997, -1.620734908136482799 ) ) ;
#80362 = CARTESIAN_POINT ( 'NONE',  ( -0.9285414500055713116, 2.165354330708661568, 0.6299212598425196763 ) ) ;
#80363 = VERTEX_POINT ( 'NONE', #75164 ) ;
#80364 = CARTESIAN_POINT ( 'NONE',  ( 0.2925321140481932369, -0.2925321140481931814, -1.120078740157480324 ) ) ;
#80365 = CARTESIAN_POINT ( 'NONE',  ( 1.574803149606299746, -0.1870078740157479769, 0.4822834645669291653 ) ) ;
#80366 = CARTESIAN_POINT ( 'NONE',  ( -0.6102362204724400829, 0.07958543189024085140, 0.2665933059059887866 ) ) ;
#80367 = CARTESIAN_POINT ( 'NONE',  ( -0.9448818897637790704, -0.1870078740157479769, 0.4822834645669291653 ) ) ;
#80368 = CARTESIAN_POINT ( 'NONE',  ( 0.3458507752293908943, 0.3458507752293908943, -0.4527559055118109965 ) ) ;
#80369 = CARTESIAN_POINT ( 'NONE',  ( -0.3917322834645670104, -7.196005306013484475E-17, -2.486220472440944906 ) ) ;
#80370 = CARTESIAN_POINT ( 'NONE',  ( 1.535433070866142558, 0.2952755905511811885, 0.000000000000000000 ) ) ;
#80371 = CARTESIAN_POINT ( 'NONE',  ( 0.6627296587926515548, 0.2952755905511811885, 0.1292274648535926551 ) ) ;
#80372 = CARTESIAN_POINT ( 'NONE',  ( 0.7217847769028878924, 0.05413385826771666132, 0.4176697321401328100 ) ) ;
#80373 = CARTESIAN_POINT ( 'NONE',  ( -0.4790026246719152336, -0.08942795157528024563, -0.3641732283464568787 ) ) ;
#80374 = CARTESIAN_POINT ( 'NONE',  ( 0.006561679790026889343, -0.05778040916215522460, 0.4822834645669289988 ) ) ;
#80375 = CARTESIAN_POINT ( 'NONE',  ( 0.4724409448818898682, 2.892866454678787531E-17, -2.399606299212598604 ) ) ;
#80376 = CARTESIAN_POINT ( 'NONE',  ( -0.4068241469816264999, -0.3690944881889763329, 0.3153832671262228327 ) ) ;
#80377 = CARTESIAN_POINT ( 'NONE',  ( -0.2887139107611542133, 0.2306618581243848609, 0.2411417322834645549 ) ) ;
#80378 = CARTESIAN_POINT ( 'NONE',  ( -0.1974969037888704149, -0.3420746716998661063, -1.874671916010499428 ) ) ;
#80379 = CARTESIAN_POINT ( 'NONE',  ( -1.430446194225721390, -0.4281496062992124485, 0.4176697321401328655 ) ) ;
#80380 = CARTESIAN_POINT ( 'NONE',  ( 0.2165354330708668673, 0.07958543189024071263, -0.2665933059059888421 ) ) ;
#80381 = CARTESIAN_POINT ( 'NONE',  ( 1.502624671916010790, -0.08942795157527998196, 0.3641732283464567121 ) ) ;
#80383 = EDGE_CURVE ( 'NONE', #74430, #74087, #62517, .T. ) ;
#80382 = CARTESIAN_POINT ( 'NONE',  ( -1.167979002624671470, -0.4281496062992127816, -0.4176697321401328100 ) ) ;
#80384 = CARTESIAN_POINT ( 'NONE',  ( -0.9186351706036736120, -0.5023911411419708095, -0.1820866141732282451 ) ) ;
#80385 = DIRECTION ( 'NONE',  ( 1.445602896647338917E-16, 1.000000000000000000, 0.000000000000000000 ) ) ;
#80386 = CARTESIAN_POINT ( 'NONE',  ( -1.227034120734907585, 0.2952755905511811885, 0.1292274648535926551 ) ) ;
#80387 = CARTESIAN_POINT ( 'NONE',  ( -0.5314960629921250401, 0.1660481256975885056, 0.3530559997133364547 ) ) ;
#80388 = CARTESIAN_POINT ( 'NONE',  ( 0.3215223097112867578, -0.3162353388693409650, -0.4822834645669289433 ) ) ;
#80390 = CARTESIAN_POINT ( 'NONE',  ( -0.1958661417322836440, 0.3392501089628016664, -2.455361261645982562 ) ) ;
#80389 = CIRCLE ( 'NONE', #30603, 3.444881889763779625 ) ;
#80391 = CARTESIAN_POINT ( 'NONE',  ( -1.877095671717788683, 1.091897865355345720, -0.1662078246829333805 ) ) ;
#80392 = CARTESIAN_POINT ( 'NONE',  ( 0.3937007874015754361, -0.1870078740157479769, 0.3641732283464567677 ) ) ;
#80393 = CARTESIAN_POINT ( 'NONE',  ( 1.181102362204724976, -0.1870078740157480879, -0.4822834645669291653 ) ) ;
#80394 = CARTESIAN_POINT ( 'NONE',  ( -1.049868766404198794, 0.1283753931104746893, -0.1820866141732285504 ) ) ;
#80395 = CARTESIAN_POINT ( 'NONE',  ( 0.9842519685039378130, -0.6692913385826771977, 8.415575281601705876E-17 ) ) ;
#80396 = CARTESIAN_POINT ( 'NONE',  ( -1.712598425196849572, 0.07958543189024085140, 0.2665933059059887866 ) ) ;
#80397 = CARTESIAN_POINT ( 'NONE',  ( -0.3805774278215216522, -0.4281496062992127816, -0.4176697321401328100 ) ) ;
#80398 = CARTESIAN_POINT ( 'NONE',  ( 0.3346456692913393205, -0.4536011799217368745, -0.2665933059059886201 ) ) ;
#80399 = CARTESIAN_POINT ( 'NONE',  ( -0.8478501267249328732, 2.401574803149606474, -0.8478501267249377582 ) ) ;
#80400 = CARTESIAN_POINT ( 'NONE',  ( 0.7414698162729663755, -0.5511811023622048555, -0.09757992244046775898 ) ) ;
#80401 = CARTESIAN_POINT ( 'NONE',  ( -0.01968503937007793844, 0.1660481256975883668, -0.3530559997133364547 ) ) ;
#80402 = EDGE_CURVE ( 'NONE', #5694, #38486, #6286, .T. ) ;
#80403 = CARTESIAN_POINT ( 'NONE',  ( -0.3996062992125986590, 0.1070741851644051723, -0.1095800524934383152 ) ) ;
#80404 = CARTESIAN_POINT ( 'NONE',  ( -1.279527559055116948, -0.5400638737290844871, 0.3530559997133364547 ) ) ;
#80405 = CARTESIAN_POINT ( 'NONE',  ( -0.1958661417322836718, 0.3392501089628017219, -1.987532808398950079 ) ) ;
#80406 = CARTESIAN_POINT ( 'NONE',  ( 1.135170603674541256, 0.1771653543307087630, 0.09757992244046791164 ) ) ;
#80407 = CARTESIAN_POINT ( 'NONE',  ( -0.08530183727034056085, -0.3162353388693405765, 0.4822834645669290543 ) ) ;
#80408 = CARTESIAN_POINT ( 'NONE',  ( -0.1837270341207340729, 0.2306618581243847221, -0.2411417322834647770 ) ) ;
#80409 = CARTESIAN_POINT ( 'NONE',  ( -0.4068241469816264999, -0.3690944881889763329, 0.3153832671262228327 ) ) ;
#80410 = CARTESIAN_POINT ( 'NONE',  ( 1.011202504342157527, 9.477779430591278127E-17, -0.3464511005275205946 ) ) ;
#80411 = CARTESIAN_POINT ( 'NONE',  ( -0.6561679790026240244, 0.1283753931104746893, -0.1820866141732285504 ) ) ;
#80412 = CARTESIAN_POINT ( 'NONE',  ( 0.1706036745406830368, -0.4281496062992127816, -0.4176697321401328100 ) ) ;
#80413 = CARTESIAN_POINT ( 'NONE',  ( -0.9908136482939626788, -0.5511811023622048555, -0.09757992244046775898 ) ) ;
#80414 = CARTESIAN_POINT ( 'NONE',  ( -0.3460692066303957537, -0.1998031496062994405, -0.7591863517060367661 ) ) ;
#80415 = CARTESIAN_POINT ( 'NONE',  ( -1.325459317585300889, 0.05413385826771666132, 0.4176697321401328100 ) ) ;
#80416 = CARTESIAN_POINT ( 'NONE',  ( 0.2362204724409449064, 0.4091458600556404646, -2.583333333333333481 ) ) ;
#80417 = ORIENTED_EDGE ( 'NONE', *, *, #5930, .F. ) ;
#80418 = CARTESIAN_POINT ( 'NONE',  ( -0.8537221893815262197, -2.294479370626195693E-15, 0.3464511005275217603 ) ) ;
#80419 = CARTESIAN_POINT ( 'NONE',  ( -0.4986876640419942164, -0.6046776061558807314, 0.2411417322834647770 ) ) ;
#80420 = EDGE_CURVE ( 'NONE', #43326, #78909, #81895, .T. ) ;
#80421 = CARTESIAN_POINT ( 'NONE',  ( 0.2628095437103130094, 1.142422500371641059, -1.473052246231814744 ) ) ;
#80422 = CARTESIAN_POINT ( 'NONE',  ( -1.108923884514435132, -0.05778040916215560624, -0.4822834645669293319 ) ) ;
#80423 = CARTESIAN_POINT ( 'NONE',  ( -0.3392501089628019995, 0.1958661417322832277, -1.370734908136483021 ) ) ;
#80424 = DIRECTION ( 'NONE',  ( 0.000000000000000000, 0.000000000000000000, -1.000000000000000000 ) ) ;
#80425 = CARTESIAN_POINT ( 'NONE',  ( 1.450131233595801428, -0.6692913385826773087, -0.1292274648535924053 ) ) ;
#80426 = CARTESIAN_POINT ( 'NONE',  ( 0.4790026246719168435, -0.3162353388693409650, -0.4822834645669289433 ) ) ;
#80427 = CARTESIAN_POINT ( 'NONE',  ( 0.3149606299212641680, 5.463695987328538763E-17, -1.076935383196056195 ) ) ;
#80428 = CARTESIAN_POINT ( 'NONE',  ( 0.1070741851644053527, 0.3996062992125985480, -2.274934383202099397 ) ) ;
#80429 = CARTESIAN_POINT ( 'NONE',  ( -1.574803149606298636, -0.1870078740157479769, 0.4822834645669291653 ) ) ;
#80430 = CARTESIAN_POINT ( 'NONE',  ( 0.2925321140481932369, -0.2925321140481932369, -0.5708661417322833387 ) ) ;
#80431 = ORIENTED_EDGE ( 'NONE', *, *, #21875, .F. ) ;
#80432 = CARTESIAN_POINT ( 'NONE',  ( -1.049868766404198794, -0.5023911411419708095, 0.1820866141732285504 ) ) ;
#80433 = CARTESIAN_POINT ( 'NONE',  ( 0.3392501089628018329, 0.1958661417322835607, -2.170603674540682260 ) ) ;
#80434 = EDGE_LOOP ( 'NONE', ( #49052, #61693, #81261, #82999 ) ) ;
#80435 = CARTESIAN_POINT ( 'NONE',  ( 0.6627296587926515548, 0.2952755905511811885, 0.1292274648535926551 ) ) ;
#80436 = CARTESIAN_POINT ( 'NONE',  ( -0.4724409448818890911, -0.1870078740157479769, 0.4822834645669291653 ) ) ;
#80437 = CARTESIAN_POINT ( 'NONE',  ( -1.062992125984250968, -0.6692913385826771977, 8.415575281601705876E-17 ) ) ;
#80438 = CARTESIAN_POINT ( 'NONE',  ( 1.240157480314961314, 0.1660481256975883668, -0.3530559997133364547 ) ) ;
#80439 = CARTESIAN_POINT ( 'NONE',  ( -1.286089238845143479, 0.1283753931104746893, -0.1820866141732285504 ) ) ;
#80440 = CARTESIAN_POINT ( 'NONE',  ( 0.000000000000000000, 0.000000000000000000, -2.362204724409448620 ) ) ;
#80441 = CARTESIAN_POINT ( 'NONE',  ( 0.2034120734908144990, -0.6692913385826771977, 0.1292274648535927661 ) ) ;
#80442 = CARTESIAN_POINT ( 'NONE',  ( -0.9383202099737524282, -0.3162353388693409650, -0.4822834645669289433 ) ) ;
#80443 = CARTESIAN_POINT ( 'NONE',  ( 0.1049643490035304522, -0.3917322834645668994, -1.582657849572491449 ) ) ;
#80444 = CARTESIAN_POINT ( 'NONE',  ( -1.122047244094487306, 0.1660481256975883668, -0.3530559997133364547 ) ) ;
#80445 = CARTESIAN_POINT ( 'NONE',  ( 0.3005662378122966882, 1.170051713876984811, -2.776705245712382641 ) ) ;
#80446 = CARTESIAN_POINT ( 'NONE',  ( 0.8398950131233602345, -0.6046776061558807314, 0.2411417322834647770 ) ) ;
#80447 = CARTESIAN_POINT ( 'NONE',  ( 1.292650918635171564, -0.5511811023622048555, -0.09757992244046775898 ) ) ;
#80448 = ORIENTED_EDGE ( 'NONE', *, *, #62891, .T. ) ;
#80449 = CARTESIAN_POINT ( 'NONE',  ( 0.2867679344610366554, -0.2867679344610365999, -2.772329027067928386 ) ) ;
#80450 = CARTESIAN_POINT ( 'NONE',  ( -0.5839895013123351797, -0.6692913385826771977, 0.1292274648535927661 ) ) ;
#80451 = ORIENTED_EDGE ( 'NONE', *, *, #51722, .T. ) ;
#80452 = VECTOR ( 'NONE', #45688, 39.37007874015748143 ) ;
#80453 = CARTESIAN_POINT ( 'NONE',  ( 0.3871391076115492380, -0.08942795157528024563, -0.3641732283464568787 ) ) ;
#80454 = CARTESIAN_POINT ( 'NONE',  ( -1.587926509186350810, -0.4281496062992124485, 0.4176697321401328655 ) ) ;
#80455 = CARTESIAN_POINT ( 'NONE',  ( 0.8464566929133865436, 0.1660481256975883668, -0.3530559997133364547 ) ) ;
#80456 = CARTESIAN_POINT ( 'NONE',  ( 0.6824146981627303710, 0.2306618581243847221, -0.2411417322834647770 ) ) ;
#80457 = CARTESIAN_POINT ( 'NONE',  ( -0.3543307086614165824, -0.6692913385826771977, 8.415575281601705876E-17 ) ) ;
#80458 = CARTESIAN_POINT ( 'NONE',  ( 0.1049643490035304799, -0.3917322834645670104, -1.341882832842206774 ) ) ;
#80459 = CARTESIAN_POINT ( 'NONE',  ( -0.7808398950131222316, -0.3162353388693409650, -0.4822834645669289433 ) ) ;
#80460 = CARTESIAN_POINT ( 'NONE',  ( -0.1958661417322836718, 0.3392501089628017219, -2.302493438320210029 ) ) ;
#80461 = CARTESIAN_POINT ( 'NONE',  ( -1.476377952755905110, -0.5400638737290845981, -0.3530559997133363437 ) ) ;
#80462 = CARTESIAN_POINT ( 'NONE',  ( -0.9514435695538050464, -0.05778040916215560624, -0.4822834645669293319 ) ) ;
#80463 = CARTESIAN_POINT ( 'NONE',  ( 1.141732283464567788, -0.6692913385826771977, 8.415575281601705876E-17 ) ) ;
#80464 = CARTESIAN_POINT ( 'NONE',  ( 1.679790026246720025, 0.2306618581243848609, 0.2411417322834645549 ) ) ;
#80465 = CARTESIAN_POINT ( 'NONE',  ( -0.7742782152230965886, 0.05413385826771666132, 0.4176697321401328100 ) ) ;
#80466 = CARTESIAN_POINT ( 'NONE',  ( -0.3460692066303960313, 0.1998031496062989965, -0.1030183727034120617 ) ) ;
#80467 = CARTESIAN_POINT ( 'NONE',  ( 0.4986876640419954376, 0.2306618581243848609, 0.2411417322834645549 ) ) ;
#80468 = CARTESIAN_POINT ( 'NONE',  ( 0.1998031496062992740, 0.3460692066303959757, -1.876640419947506411 ) ) ;
#80469 = CARTESIAN_POINT ( 'NONE',  ( -0.5183727034120726440, 0.2952755905511811885, 0.1292274648535926551 ) ) ;
#80470 = CARTESIAN_POINT ( 'NONE',  ( 1.574803149606299746, -0.1870078740157480879, -0.4822834645669291653 ) ) ;
#80471 = CARTESIAN_POINT ( 'NONE',  ( 0.4790026246719168435, -0.2845877964562161244, -0.3641732283464567121 ) ) ;
#80472 = CARTESIAN_POINT ( 'NONE',  ( 1.312335958005249825, 0.2306618581243847221, -0.2411417322834647770 ) ) ;
#80473 = CARTESIAN_POINT ( 'NONE',  ( 0.1265901696524989462, 0.4724409448818897572, -0.5426509186351704539 ) ) ;
#80474 = CARTESIAN_POINT ( 'NONE',  ( 0.9973753280839902091, -0.5023911411419708095, 0.1820866141732285504 ) ) ;
#80475 = CARTESIAN_POINT ( 'NONE',  ( 0.6364829396325465405, -0.05778040916215522460, 0.4822834645669289988 ) ) ;
#80476 = CARTESIAN_POINT ( 'NONE',  ( -0.2891555358219911054, 0.2891555358219909388, -0.4114173228346456046 ) ) ;
#80477 = CARTESIAN_POINT ( 'NONE',  ( -0.5511811023622041894, -0.1870078740157480879, -0.4822834645669291653 ) ) ;
#80478 = CARTESIAN_POINT ( 'NONE',  ( 1.207349081364829990, -0.5023911411419708095, -0.1820866141732282451 ) ) ;
#80479 = CARTESIAN_POINT ( 'NONE',  ( -0.6364829396325453192, -0.3162353388693405765, 0.4822834645669290543 ) ) ;
#80480 = CARTESIAN_POINT ( 'NONE',  ( 0.3949938075777409963, 2.418639510665530743E-17, -0.6673228346456693272 ) ) ;
#80481 = CARTESIAN_POINT ( 'NONE',  ( 1.364829396325460076, 0.2306618581243848609, 0.2411417322834645549 ) ) ;
#80482 = CARTESIAN_POINT ( 'NONE',  ( 0.2821522309711292364, -0.6692913385826771977, 0.1292274648535927661 ) ) ;
#80483 = CARTESIAN_POINT ( 'NONE',  ( 0.3740157480314966754, -0.4536011799217367080, 0.2665933059059888421 ) ) ;
#80484 = CARTESIAN_POINT ( 'NONE',  ( -0.4497599300473023587, 1.383355012730091538, -1.028042735862942259 ) ) ;
#80485 = CARTESIAN_POINT ( 'NONE',  ( -0.06561679790026180015, -0.004921259842519576551, 0.3153832671262227771 ) ) ;
#80486 = CARTESIAN_POINT ( 'NONE',  ( 0.8333333333333340365, 0.1771653543307087075, -0.09757992244046823083 ) ) ;
#80487 = CARTESIAN_POINT ( 'NONE',  ( -1.548556430446193399, -0.6046776061558809534, -0.2411417322834644161 ) ) ;
#80488 = CARTESIAN_POINT ( 'NONE',  ( -9.787531504996566615E-17, 0.3996062992125985480, -1.494094488188976610 ) ) ;
#80489 = CARTESIAN_POINT ( 'NONE',  ( 0.8005249343832028242, -0.4281496062992127816, -0.4176697321401328100 ) ) ;
#80490 = CARTESIAN_POINT ( 'NONE',  ( 0.1958661417322836440, -0.3392501089628017219, -1.186351706036745446 ) ) ;
#80491 = DIRECTION ( 'NONE',  ( 0.000000000000000000, 0.000000000000000000, 1.000000000000000000 ) ) ;
#80492 = DIRECTION ( 'NONE',  ( 0.000000000000000000, 0.000000000000000000, 1.000000000000000000 ) ) ;
#80493 = CARTESIAN_POINT ( 'NONE',  ( 0.1312335958005255154, -0.5023911411419708095, 0.1820866141732285504 ) ) ;
#80494 = CARTESIAN_POINT ( 'NONE',  ( 0.1837270341207357105, -0.6046776061558809534, -0.2411417322834644161 ) ) ;
#80495 = CARTESIAN_POINT ( 'NONE',  ( 1.522309711286089939, 0.1283753931104748280, 0.1820866141732283561 ) ) ;
#80496 = CARTESIAN_POINT ( 'NONE',  ( -1.430446194225721390, -0.3690944881889763329, 0.3153832671262228327 ) ) ;
#80497 = CARTESIAN_POINT ( 'NONE',  ( -1.423884514435694859, -0.3162353388693405765, 0.4822834645669290543 ) ) ;
#80498 = CARTESIAN_POINT ( 'NONE',  ( 0.5249343832021005074, -0.6046776061558807314, 0.2411417322834647770 ) ) ;
#80499 = CARTESIAN_POINT ( 'NONE',  ( 1.062992125984252745, 0.2952755905511811885, 0.000000000000000000 ) ) ;
#80500 = CARTESIAN_POINT ( 'NONE',  ( -0.2362204724409451284, 0.4091458600556402425, -0.2473753280839895152 ) ) ;
#80501 = CARTESIAN_POINT ( 'NONE',  ( 0.2887139107611556010, -0.6046776061558807314, 0.2411417322834647770 ) ) ;
#80502 = CARTESIAN_POINT ( 'NONE',  ( 1.128608923884515169, -0.6046776061558809534, -0.2411417322834644161 ) ) ;
#80503 = CARTESIAN_POINT ( 'NONE',  ( 1.030183727034121421, -0.05778040916215522460, 0.4822834645669289988 ) ) ;
#80504 = EDGE_CURVE ( 'NONE', #45375, #53039, #37660, .T. ) ;
#80505 = CARTESIAN_POINT ( 'NONE',  ( 0.4724409448818898682, 2.892866454678787531E-17, -0.3523622047244094335 ) ) ;
#80506 = CARTESIAN_POINT ( 'NONE',  ( 0.6496062992125991586, -0.4536011799217368745, -0.2665933059059886201 ) ) ;
#80507 = CARTESIAN_POINT ( 'NONE',  ( 1.522309711286089939, 0.2306618581243848609, 0.2411417322834645549 ) ) ;
#80508 = CARTESIAN_POINT ( 'NONE',  ( -0.09186351706036689768, -0.004921259842519870586, -0.3153832671262229437 ) ) ;
#80509 = CARTESIAN_POINT ( 'NONE',  ( -0.05249343832020911260, 0.2306618581243848609, 0.2411417322834645549 ) ) ;
#80510 = CARTESIAN_POINT ( 'NONE',  ( 0.5380577427821529035, 0.05413385826771626580, -0.4176697321401330321 ) ) ;
#80511 = CARTESIAN_POINT ( 'NONE',  ( -0.3871391076115476282, -0.05778040916215522460, 0.4822834645669289988 ) ) ;
#80512 = CARTESIAN_POINT ( 'NONE',  ( -0.2493438320209966919, -0.004921259842519870586, -0.3153832671262229437 ) ) ;
#80513 = CARTESIAN_POINT ( 'NONE',  ( 0.7808398950131240079, -0.3162353388693405765, 0.4822834645669290543 ) ) ;
#80514 = CARTESIAN_POINT ( 'NONE',  ( 1.115485564304462551, -0.3690944881889765550, -0.3153832671262227771 ) ) ;
#80515 = PLANE ( 'NONE',  #78315 ) ;
#80517 = CARTESIAN_POINT ( 'NONE',  ( -0.2925321140481932369, 0.2925321140481931814, -1.122047244094488194 ) ) ;
#80516 = DIRECTION ( 'NONE',  ( 0.000000000000000000, -8.326672684688674053E-16, 1.000000000000000000 ) ) ;
#80518 = DIRECTION ( 'NONE',  ( 0.000000000000000000, 0.000000000000000000, -1.000000000000000000 ) ) ;
#80519 = CARTESIAN_POINT ( 'NONE',  ( -1.095800524934382292, -0.3162353388693409650, -0.4822834645669289433 ) ) ;
#80520 = CARTESIAN_POINT ( 'NONE',  ( -0.6824146981627291497, -0.6046776061558809534, -0.2411417322834644161 ) ) ;
#80521 = B_SPLINE_CURVE_WITH_KNOTS ( 'NONE', 3,
 ( #30128, #15453, #41112, #34806, #60465, #56210, #12021, #38505, #75593, #24635 ),
 .UNSPECIFIED., .F., .F.,
 ( 4, 2, 2, 2, 4 ),
 ( 2.168404344971008868E-18, 0.003519800242347440305, 0.004399750302934300056, 0.005279700363521159373, 0.007039600484694878008 ),
 .UNSPECIFIED. ) ;
#80522 = EDGE_CURVE ( 'NONE', #820, #42318, #55481, .T. ) ;
#80523 =( BOUNDED_CURVE ( )  B_SPLINE_CURVE ( 2, ( #53359, #21385, #47040, #72733, #15079, #40737, #54602, #23860, #43198, #49109, #4090, #17565, #29758, #11243, #62579, #61332, #29351, #48699, #68080, #74815, #4921, #47869, #67255, #16329, #41973, #55421, #62162, #81128, #17160, #30170, #35257, #3686, #55010, #74397, #60921, #10424, #4503, #54181, #15918, #73573, #9588, #35668, #3272, #80718, #23445, #68893, #36903, #79894, #42793, #28933, #80311, #16741, #67666, #22626, #48286, #10003, #41566, #73983, #23033, #55833, #81541, #68488, #22212, #42381, #36082, #61753, #49527, #10827, #36487, #75220, #77278, #63809, #70966, #38963, #37723, #5732, #25083, #44428, #51162, #64647, #70537, #43610, #76042, #18387, #6148, #38552, #31822, #76858, #6566, #11662, #63397, #57482, #50757, #30589, #5332, #69312, #49937, #56255, #62993, #32238, #37321, #30990, #12893, #76457, #19190, #83176, #82359, #25496, #44839, #64232, #70122, #18784, #56658, #57896, #12065, #82762, #31403, #263, #57068, #25916, #24677, #50345, #19608, #12473, #81951, #24264, #51575, #38135, #45270, #44028, #13311, #75635, #17973, #69721, #40228, #59162, #79376, #26338, #53669, #47358, #2353, #21695, #53255, #73047, #15396, #8661, #59997, #71381, #1520, #46526, #51999, #77704, #20034, #33500, #66322, #14981, #27596, #45685, #26759, #33079, #34332, #33912, #41058, #6984, #32653, #78967, #13731, #39385, #52836, #52414, #58746, #7409, #46109, #65070, #1108, #682, #40640, #28009, #58319, #78123, #21287, #20456, #71802, #14155, #39811, #1932, #65910, #65501, #8247 ),
 .UNSPECIFIED., .F., .F. ) 
 B_SPLINE_CURVE_WITH_KNOTS ( ( 3, 2, 2, 2, 2, 2, 2, 2, 2, 2, 2, 2, 2, 2, 2, 2, 2, 2, 2, 2, 2, 2, 2, 2, 2, 2, 2, 2, 2, 2, 2, 2, 2, 2, 2, 2, 2, 2, 2, 2, 2, 2, 2, 2, 2, 2, 2, 2, 2, 2, 2, 2, 2, 2, 2, 2, 2, 2, 2, 2, 2, 2, 2, 2, 2, 2, 2, 2, 2, 2, 2, 2, 2, 2, 2, 2, 2, 2, 2, 2, 2, 2, 2, 2, 2, 2, 2, 2, 2, 2, 2, 2, 2, 2, 3 ),
 ( 0.07563788552403453991, 0.07916666666666666297, 0.08333333333333332871, 0.08749999999999999445, 0.09166666666666666019, 0.09583333333333333981, 0.1000000000000000056, 0.1041666666666666713, 0.1083333333333333370, 0.1125000000000000028, 0.1166666666666666685, 0.1208333333333333343, 0.1250000000000000000, 0.1291666666666666796, 0.1333333333333333315, 0.1375000000000000111, 0.1416666666666666630, 0.1458333333333333426, 0.1499999999999999944, 0.1541666666666666741, 0.1583333333333333259, 0.1625000000000000333, 0.1666666666666666574, 0.1708333333333333370, 0.1749999999999999889, 0.1791666666666666685, 0.1833333333333333204, 0.1875000000000000000, 0.1916666666666666796, 0.1958333333333333315, 0.2000000000000000111, 0.2041666666666666630, 0.2083333333333333703, 0.2125000000000000222, 0.2166666666666666741, 0.2208333333333333259, 0.2250000000000000333, 0.2291666666666666852, 0.2333333333333333370, 0.2374999999999999889, 0.2416666666666666408, 0.2458333333333333481, 0.2500000000000000000, 0.2541666666666666519, 0.2583333333333333037, 0.2625000000000000111, 0.2666666666666666630, 0.2708333333333333148, 0.2750000000000000222, 0.2791666666666666741, 0.2833333333333333259, 0.2874999999999999778, 0.2916666666666666852, 0.2958333333333333370, 0.2999999999999999889, 0.3041666666666666408, 0.3083333333333333481, 0.3125000000000000000, 0.3166666666666666519, 0.3208333333333333592, 0.3250000000000000111, 0.3291666666666666630, 0.3333333333333333148, 0.3375000000000000222, 0.3416666666666666741, 0.3458333333333333259, 0.3499999999999999778, 0.3541666666666666852, 0.3583333333333333370, 0.3624999999999999889, 0.3666666666666666408, 0.3708333333333333481, 0.3750000000000000000, 0.3791666666666666519, 0.3833333333333333592, 0.3875000000000000111, 0.3916666666666666630, 0.3958333333333333148, 0.4000000000000000222, 0.4041666666666666741, 0.4083333333333333259, 0.4124999999999999778, 0.4166666666666667407, 0.4208333333333333370, 0.4249999999999999889, 0.4291666666666666963, 0.4333333333333333481, 0.4375000000000000000, 0.4416666666666665964, 0.4458333333333333592, 0.4500000000000000666, 0.4541666666666666630, 0.4583333333333333148, 0.4625000000000000222, 0.4631378855240345094 ),
 .UNSPECIFIED. ) 
 CURVE ( )  GEOMETRIC_REPRESENTATION_ITEM ( )  RATIONAL_B_SPLINE_CURVE ( ( 0.9911642120907997455, 0.9711423276059423237, 1.000000000000000000, 0.9659258262890683122, 1.000000000000000000, 0.9659258262890683122, 1.000000000000000000, 0.9659258262890683122, 1.000000000000000000, 0.9659258262890683122, 1.000000000000000000, 0.9659258262890683122, 1.000000000000000000, 0.9659258262890683122, 1.000000000000000000, 0.9659258262890683122, 1.000000000000000000, 0.9659258262890683122, 1.000000000000000000, 0.9659258262890683122, 1.000000000000000000, 0.9659258262890683122, 1.000000000000000000, 0.9659258262890683122, 1.000000000000000000, 0.9659258262890683122, 1.000000000000000000, 0.9659258262890683122, 1.000000000000000000, 0.9659258262890683122, 1.000000000000000000, 0.9659258262890683122, 1.000000000000000000, 0.9659258262890683122, 1.000000000000000000, 0.9659258262890683122, 1.000000000000000000, 0.9659258262890683122, 1.000000000000000000, 0.9659258262890683122, 1.000000000000000000, 0.9659258262890683122, 1.000000000000000000, 0.9659258262890683122, 1.000000000000000000, 0.9659258262890683122, 1.000000000000000000, 0.9659258262890683122, 1.000000000000000000, 0.9659258262890683122, 1.000000000000000000, 0.9659258262890683122, 1.000000000000000000, 0.9659258262890683122, 1.000000000000000000, 0.9659258262890683122, 1.000000000000000000, 0.9659258262890683122, 1.000000000000000000, 0.9659258262890683122, 1.000000000000000000, 0.9659258262890683122, 1.000000000000000000, 0.9659258262890683122, 1.000000000000000000, 0.9659258262890683122, 1.000000000000000000, 0.9659258262890683122, 1.000000000000000000, 0.9659258262890683122, 1.000000000000000000, 0.9659258262890683122, 1.000000000000000000, 0.9659258262890683122, 1.000000000000000000, 0.9659258262890683122, 1.000000000000000000, 0.9659258262890683122, 1.000000000000000000, 0.9659258262890683122, 1.000000000000000000, 0.9659258262890683122, 1.000000000000000000, 0.9659258262890683122, 1.000000000000000000, 0.9659258262890683122, 1.000000000000000000, 0.9659258262890683122, 1.000000000000000000, 0.9659258262890683122, 1.000000000000000000, 0.9659258262890683122, 1.000000000000000000, 0.9659258262890683122, 1.000000000000000000, 0.9659258262890683122, 1.000000000000000000, 0.9659258262890683122, 1.000000000000000000, 0.9659258262890683122, 1.000000000000000000, 0.9659258262890683122, 1.000000000000000000, 0.9659258262890683122, 1.000000000000000000, 0.9659258262890683122, 1.000000000000000000, 0.9659258262890683122, 1.000000000000000000, 0.9659258262890683122, 1.000000000000000000, 0.9659258262890683122, 1.000000000000000000, 0.9659258262890683122, 1.000000000000000000, 0.9659258262890683122, 1.000000000000000000, 0.9659258262890683122, 1.000000000000000000, 0.9659258262890683122, 1.000000000000000000, 0.9659258262890683122, 1.000000000000000000, 0.9659258262890683122, 1.000000000000000000, 0.9659258262890683122, 1.000000000000000000, 0.9659258262890683122, 1.000000000000000000, 0.9659258262890683122, 1.000000000000000000, 0.9659258262890683122, 1.000000000000000000, 0.9659258262890683122, 1.000000000000000000, 0.9659258262890683122, 1.000000000000000000, 0.9659258262890683122, 1.000000000000000000, 0.9659258262890683122, 1.000000000000000000, 0.9659258262890683122, 1.000000000000000000, 0.9659258262890683122, 1.000000000000000000, 0.9659258262890683122, 1.000000000000000000, 0.9659258262890683122, 1.000000000000000000, 0.9659258262890683122, 1.000000000000000000, 0.9659258262890683122, 1.000000000000000000, 0.9659258262890683122, 1.000000000000000000, 0.9659258262890683122, 1.000000000000000000, 0.9659258262890683122, 1.000000000000000000, 0.9659258262890683122, 1.000000000000000000, 0.9659258262890683122, 1.000000000000000000, 0.9659258262890683122, 1.000000000000000000, 0.9659258262890683122, 1.000000000000000000, 0.9659258262890683122, 1.000000000000000000, 0.9659258262890683122, 1.000000000000000000, 0.9659258262890683122, 1.000000000000000000, 0.9659258262890683122, 1.000000000000000000, 0.9659258262890683122, 1.000000000000000000, 0.9659258262890683122, 1.000000000000000000, 0.9659258262890683122, 1.000000000000000000, 0.9659258262890683122, 1.000000000000000000, 0.9659258262890683122, 1.000000000000000000, 0.9659258262890683122, 1.000000000000000000, 0.9947834986831268766, 0.9911642120908008557 ) ) 
 REPRESENTATION_ITEM ( '' )  );
#80524 = CARTESIAN_POINT ( 'NONE',  ( -0.4724409448818895907, -0.1265901696524993070, -0.04593175853018372640 ) ) ;
#80525 = CARTESIAN_POINT ( 'NONE',  ( -0.1974969037888703871, -0.3420746716998661063, -2.270341207349081181 ) ) ;
#80526 = ORIENTED_EDGE ( 'NONE', *, *, #47459, .T. ) ;
#80527 = CARTESIAN_POINT ( 'NONE',  ( 0.7086614173228353852, -0.1870078740157479769, 0.3641732283464567677 ) ) ;
#80528 = CARTESIAN_POINT ( 'NONE',  ( -0.2867679344610365999, 0.2867679344610364889, -0.7992125984251968740 ) ) ;
#80529 = CARTESIAN_POINT ( 'NONE',  ( 1.030183727034121421, -0.3162353388693409650, -0.4822834645669289433 ) ) ;
#80530 = CARTESIAN_POINT ( 'NONE',  ( -0.3458507752293909498, 0.3458507752293907833, -2.381889763779527325 ) ) ;
#80531 = DIRECTION ( 'NONE',  ( 1.000000000000000000, -0.000000000000000000, -0.000000000000000000 ) ) ;
#80532 = EDGE_CURVE ( 'NONE', #43739, #82183, #31323, .T. ) ;
#80533 = CARTESIAN_POINT ( 'NONE',  ( -1.574803149606298636, -0.1870078740157479769, 0.3641732283464567677 ) ) ;
#80534 = CARTESIAN_POINT ( 'NONE',  ( 1.587926509186352586, -0.4281496062992127816, -0.4176697321401328100 ) ) ;
#80535 = CARTESIAN_POINT ( 'NONE',  ( 1.279527559055118724, 0.07958543189024085140, 0.2665933059059887866 ) ) ;
#80536 = CARTESIAN_POINT ( 'NONE',  ( 0.3018372703412079971, 0.05413385826771626580, -0.4176697321401330321 ) ) ;
#80537 = CARTESIAN_POINT ( 'NONE',  ( 0.1049643490035303689, 0.3917322834645668994, -0.3884321277877147427 ) ) ;
#80538 = CARTESIAN_POINT ( 'NONE',  ( -0.07217847769028787330, -0.05778040916215522460, 0.4822834645669289988 ) ) ;
#80539 = CARTESIAN_POINT ( 'NONE',  ( -0.7480314960629914633, 0.1771653543307087630, 0.000000000000000000 ) ) ;
#80540 = CARTESIAN_POINT ( 'NONE',  ( 0.3740157480314966754, 0.1660481256975883668, -0.3530559997133364547 ) ) ;
#80541 = CARTESIAN_POINT ( 'NONE',  ( -0.2296587926509179312, -0.3162353388693409650, -0.4822834645669289433 ) ) ;
#80542 = DIRECTION ( 'NONE',  ( 0.000000000000000000, 0.000000000000000000, -1.000000000000000000 ) ) ;
#80543 = DIRECTION ( 'NONE',  ( -3.096699300667737957E-16, 1.000000000000000000, -0.000000000000000000 ) ) ;
#80544 = CARTESIAN_POINT ( 'NONE',  ( -0.2867679344610367109, 0.2867679344610365444, -1.748706979823833718 ) ) ;
#80545 = CARTESIAN_POINT ( 'NONE',  ( 1.030183727034121421, -0.05778040916215522460, 0.4822834645669289988 ) ) ;
#80546 = CARTESIAN_POINT ( 'NONE',  ( -0.05905511811023545637, -0.5400638737290845981, -0.3530559997133363437 ) ) ;
#80547 = CARTESIAN_POINT ( 'NONE',  ( -0.9055118110236215490, -0.6692913385826771977, 8.415575281601705876E-17 ) ) ;
#80548 = CARTESIAN_POINT ( 'NONE',  ( 1.095800524934383846, -0.3162353388693405765, 0.4822834645669290543 ) ) ;
#80549 = CARTESIAN_POINT ( 'NONE',  ( 0.2624671916010504757, 0.2306618581243848609, 0.2411417322834645549 ) ) ;
#80550 = CARTESIAN_POINT ( 'NONE',  ( -0.3917322834645671215, 0.1049643490035301469, -0.9048556430446195176 ) ) ;
#80551 = CARTESIAN_POINT ( 'NONE',  ( -0.4724409448818890911, -0.1870078740157479769, 0.4822834645669291653 ) ) ;
#80552 = CARTESIAN_POINT ( 'NONE',  ( 0.8333333333333340365, -0.6692913385826771977, 0.1292274648535927661 ) ) ;
#80553 = CARTESIAN_POINT ( 'NONE',  ( -0.1706036745406816491, 0.05413385826771626580, -0.4176697321401330321 ) ) ;
#80554 = CARTESIAN_POINT ( 'NONE',  ( 0.8070866141732289112, -0.4536011799217368745, -0.2665933059059886201 ) ) ;
#80555 = CARTESIAN_POINT ( 'NONE',  ( -1.712598425196849572, 0.1660481256975885056, 0.3530559997133364547 ) ) ;
#80556 = CARTESIAN_POINT ( 'NONE',  ( -0.4744094488188880243, 1.528817788452848880, -2.554262525012306551 ) ) ;
#80557 = CARTESIAN_POINT ( 'NONE',  ( 0.3280839895013130669, 0.05413385826771666132, 0.4176697321401328100 ) ) ;
#80558 = CARTESIAN_POINT ( 'NONE',  ( 0.4724409448818898682, 2.892866454678787531E-17, -1.220472440944881942 ) ) ;
#80559 = EDGE_CURVE ( 'NONE', #74865, #27710, #23416, .T. ) ;
#80560 = CARTESIAN_POINT ( 'NONE',  ( -0.2867679344610365999, 0.2867679344610364889, -2.531496062992125484 ) ) ;
#80561 = EDGE_LOOP ( 'NONE', ( #2982, #8773 ) ) ;
#80562 = VERTEX_POINT ( 'NONE', #50286 ) ;
#80563 = CARTESIAN_POINT ( 'NONE',  ( 0.7939632545931766261, -0.3162353388693409650, -0.4822834645669289433 ) ) ;
#80564 = CARTESIAN_POINT ( 'NONE',  ( 0.4265091863517067039, -0.5511811023622048555, -0.09757992244046775898 ) ) ;
#80566 = PLANE ( 'NONE',  #4856 ) ;
#80565 = CARTESIAN_POINT ( 'NONE',  ( -1.586052503253845503, 2.125984251968505045, 0.1653254495020588799 ) ) ;
#80567 = CARTESIAN_POINT ( 'NONE',  ( -0.1958661417322834220, -0.3392501089628018884, -0.9376640419947508409 ) ) ;
#80568 = LINE ( 'NONE', #22879, #74639 ) ;
#80569 = FACE_OUTER_BOUND ( 'NONE', #70488, .T. ) ;
#80570 = CARTESIAN_POINT ( 'NONE',  ( -0.1958661417322834220, -0.3392501089628018884, -1.725065616797900381 ) ) ;
#80571 = ADVANCED_FACE ( 'NONE', ( #55774 ), #81481, .F. ) ;
#80572 = CARTESIAN_POINT ( 'NONE',  ( 0.2925321140481932369, -0.2925321140481931814, -2.379921259842520342 ) ) ;
#80573 = CARTESIAN_POINT ( 'NONE',  ( 0.8530183727034126306, 0.05413385826771626580, -0.4176697321401330321 ) ) ;
#80574 = CARTESIAN_POINT ( 'NONE',  ( -0.6036745406824141069, -0.6046776061558809534, -0.2411417322834644161 ) ) ;
#80575 = CARTESIAN_POINT ( 'NONE',  ( -0.9120734908136475250, 0.2952755905511811885, 0.1292274648535926551 ) ) ;
#80576 = CARTESIAN_POINT ( 'NONE',  ( 0.8005249343832027131, 0.05413385826771666132, 0.4176697321401328100 ) ) ;
#80577 = CARTESIAN_POINT ( 'NONE',  ( 1.561679790026247350, -0.4281496062992124485, 0.4176697321401328655 ) ) ;
#80578 = CARTESIAN_POINT ( 'NONE',  ( -1.063838992779605919, 1.224418437586606290, 0.3568528392778475000 ) ) ;
#80579 = ITEM_DEFINED_TRANSFORMATION ( 'NONE', 'NONE', #15446,  #22098 ) ;
#80580 = CARTESIAN_POINT ( 'NONE',  ( 1.371391076115485941, 0.1771653543307087630, 0.09757992244046791164 ) ) ;
#80581 = CARTESIAN_POINT ( 'NONE',  ( -0.2925321140481930149, -0.2925321140481933480, -2.183070866141731958 ) ) ;
#80582 = CARTESIAN_POINT ( 'NONE',  ( -1.174540682414697335, -0.08942795157527998196, 0.3641732283464567121 ) ) ;
#80583 = EDGE_CURVE ( 'NONE', #33327, #62412, #73118, .T. ) ;
#80584 = CARTESIAN_POINT ( 'NONE',  ( -0.1049643490035307020, 0.3917322834645669549, 0.001312335958005294862 ) ) ;
#80585 = CARTESIAN_POINT ( 'NONE',  ( 0.06561679790026316017, -0.4281496062992124485, 0.4176697321401328655 ) ) ;
#80586 = DIRECTION ( 'NONE',  ( 0.000000000000000000, 0.000000000000000000, -1.000000000000000000 ) ) ;
#80587 = CARTESIAN_POINT ( 'NONE',  ( -1.318897637795274802, -0.4536011799217368745, -0.2665933059059886201 ) ) ;
#80588 = CARTESIAN_POINT ( 'NONE',  ( 0.5577427821522316087, -0.05778040916215522460, 0.4822834645669289988 ) ) ;
#80589 = CARTESIAN_POINT ( 'NONE',  ( 1.318897637795276356, 0.07958543189024071263, -0.2665933059059888421 ) ) ;
#80590 = CARTESIAN_POINT ( 'NONE',  ( 0.1958661417322836162, -0.3392501089628018329, -1.274258899441258031 ) ) ;
#80591 = CARTESIAN_POINT ( 'NONE',  ( -1.017060367454067249, -0.2845877964562161244, -0.3641732283464567121 ) ) ;
#80592 = CARTESIAN_POINT ( 'NONE',  ( 1.410761154855643795, -0.05778040916215560624, -0.4822834645669293319 ) ) ;
#80593 = CARTESIAN_POINT ( 'NONE',  ( -0.5314960629921127166, 2.755905511811024056, -3.821484228344195433 ) ) ;
#80594 = CARTESIAN_POINT ( 'NONE',  ( -0.3149606299212590610, -0.1870078740157479769, 0.4822834645669291653 ) ) ;
#80595 = CARTESIAN_POINT ( 'NONE',  ( -1.535433070866141225, -0.5511811023622047445, 6.969142054262312111E-17 ) ) ;
#80596 = CARTESIAN_POINT ( 'NONE',  ( -0.6036745406824141069, 0.2306618581243848609, 0.2411417322834645549 ) ) ;
#80597 = CARTESIAN_POINT ( 'NONE',  ( 1.673228346456693494, 0.1660481256975885056, 0.3530559997133364547 ) ) ;
#80598 = CARTESIAN_POINT ( 'NONE',  ( -0.3392501089628019995, 0.1958661417322831999, -0.4954261399288207857 ) ) ;
#80599 = CARTESIAN_POINT ( 'NONE',  ( 0.3543307086614179147, 0.2952755905511811885, 0.000000000000000000 ) ) ;
#80600 = CARTESIAN_POINT ( 'NONE',  ( 1.568241469816273437, -0.3162353388693405765, 0.4822834645669290543 ) ) ;
#80601 = CARTESIAN_POINT ( 'NONE',  ( -1.157146581871515012E-16, 0.4724409448818898682, -1.966535433070865979 ) ) ;
#80602 = CARTESIAN_POINT ( 'NONE',  ( -1.391076115485563758, 0.2306618581243848609, 0.2411417322834645549 ) ) ;
#80603 = CARTESIAN_POINT ( 'NONE',  ( -0.7086614173228339419, -0.1870078740157480601, -0.3641732283464567677 ) ) ;
#80604 = CARTESIAN_POINT ( 'NONE',  ( -1.581364829396324945, -0.05778040916215560624, -0.4822834645669293319 ) ) ;
#80605 = CARTESIAN_POINT ( 'NONE',  ( -0.06561679790026180015, 0.05413385826771666132, 0.4176697321401328100 ) ) ;
#80606 = CARTESIAN_POINT ( 'NONE',  ( 0.3280839895013130669, -0.3690944881889765550, -0.3153832671262227771 ) ) ;
#80607 = CARTESIAN_POINT ( 'NONE',  ( -1.148293963254592542, -0.5511811023622048555, -0.09757992244046775898 ) ) ;
#80608 = CARTESIAN_POINT ( 'NONE',  ( -1.279527559055116948, -0.5400638737290844871, 0.3530559997133364547 ) ) ;
#80609 = CARTESIAN_POINT ( 'NONE',  ( -1.450131233595799651, -0.6692913385826771977, 0.1292274648535927661 ) ) ;
#80610 = CARTESIAN_POINT ( 'NONE',  ( 1.535433070866142558, 0.2952755905511811885, 0.000000000000000000 ) ) ;
#80611 = CARTESIAN_POINT ( 'NONE',  ( 0.08520949344211689591, 1.070405622666593226, 1.857259653016817280 ) ) ;
#80612 = CARTESIAN_POINT ( 'NONE',  ( 0.5118110236220480003, -0.5511811023622047445, 6.969142054262312111E-17 ) ) ;
#80613 = CARTESIAN_POINT ( 'NONE',  ( 1.076115485564305141, 0.2306618581243847221, -0.2411417322834647770 ) ) ;
#80614 = DIRECTION ( 'NONE',  ( 0.000000000000000000, 1.000000000000000000, 0.000000000000000000 ) ) ;
#80615 = CARTESIAN_POINT ( 'NONE',  ( 1.318897637795276356, 0.07958543189024071263, -0.2665933059059888421 ) ) ;
#80616 = EDGE_LOOP ( 'NONE', ( #13430, #24382, #47994, #27396 ) ) ;
#80617 = CARTESIAN_POINT ( 'NONE',  ( -1.207349081364828436, -0.6046776061558807314, 0.2411417322834647770 ) ) ;
#80618 = CARTESIAN_POINT ( 'NONE',  ( -0.7611548556430438595, -0.6046776061558809534, -0.2411417322834644161 ) ) ;
#80619 = CARTESIAN_POINT ( 'NONE',  ( 0.2821522309711292364, -0.6692913385826771977, 0.1292274648535927661 ) ) ;
#80620 = CARTESIAN_POINT ( 'NONE',  ( -2.165487897237678538, 1.580736828574222264, -0.4725026149319441759 ) ) ;
#80621 = CARTESIAN_POINT ( 'NONE',  ( -0.3996062992125985480, -7.340648628747423112E-17, -2.163385826771653697 ) ) ;
#80622 = CARTESIAN_POINT ( 'NONE',  ( 0.8792650918635177559, -0.4281496062992127816, -0.4176697321401328100 ) ) ;
#80623 = CARTESIAN_POINT ( 'NONE',  ( 1.522309711286089939, -0.5023911411419708095, -0.1820866141732282451 ) ) ;
#80624 = CARTESIAN_POINT ( 'NONE',  ( 0.08530183727034192087, -0.05778040916215522460, 0.4822834645669289988 ) ) ;
#80625 = CARTESIAN_POINT ( 'NONE',  ( 0.6036745406824153282, -0.6046776061558807314, 0.2411417322834647770 ) ) ;
#80626 = EDGE_CURVE ( 'NONE', #58460, #41616, #81231, .T. ) ;
#80627 = CARTESIAN_POINT ( 'NONE',  ( -0.2925321140481930704, -0.2925321140481933480, -1.633858267716534973 ) ) ;
#80628 = CARTESIAN_POINT ( 'NONE',  ( 0.3949938075777411073, -0.1058382717557499464, -1.056430446194225770 ) ) ;
#80629 = CARTESIAN_POINT ( 'NONE',  ( -0.1998031496062994683, 0.3460692066303958092, -2.375328083989501238 ) ) ;
#80630 = CARTESIAN_POINT ( 'NONE',  ( -0.1133856558944468518, -0.2726377952755905665, 0.1574803149606299191 ) ) ;
#80631 = CARTESIAN_POINT ( 'NONE',  ( -0.1208384647389192101, 0.3726288332213502641, 1.112018681666451222E-17 ) ) ;
#80632 = CARTESIAN_POINT ( 'NONE',  ( -0.08530183727034056085, -0.08942795157528024563, -0.3641732283464568787 ) ) ;
#80633 = CARTESIAN_POINT ( 'NONE',  ( -0.1312335958005241554, 0.2306618581243848609, 0.2411417322834645549 ) ) ;
#80634 = CARTESIAN_POINT ( 'NONE',  ( 0.7545931758530188826, -0.6692913385826771977, 0.1292274648535927661 ) ) ;
#80635 = CARTESIAN_POINT ( 'NONE',  ( 0.2891555358219910499, 0.2891555358219910499, -2.261811023622047667 ) ) ;
#80636 = CARTESIAN_POINT ( 'NONE',  ( -0.1837270341207340729, 0.1283753931104746893, -0.1820866141732285504 ) ) ;
#80637 = CARTESIAN_POINT ( 'NONE',  ( -1.161417322834644716, 0.1660481256975885056, 0.3530559997133364547 ) ) ;
#80638 = CARTESIAN_POINT ( 'NONE',  ( 1.397637795275591177, -0.5400638737290844871, 0.3530559997133364547 ) ) ;
#80639 = CARTESIAN_POINT ( 'NONE',  ( 0.1265901696524990294, -0.4724409448818896462, -2.447506561679789527 ) ) ;
#80640 = CARTESIAN_POINT ( 'NONE',  ( -0.3460692066303958092, -0.1998031496062994683, -1.942257217847769057 ) ) ;
#80641 = CARTESIAN_POINT ( 'NONE',  ( 0.4724409448818898682, 2.892866454678787531E-17, -2.714566929133858331 ) ) ;
#80642 = ORIENTED_EDGE ( 'NONE', *, *, #31497, .F. ) ;
#80643 = CARTESIAN_POINT ( 'NONE',  ( 0.8792650918635177559, -0.4281496062992127816, -0.4176697321401328100 ) ) ;
#80644 = CARTESIAN_POINT ( 'NONE',  ( 1.272965879265092637, -0.004921259842519576551, 0.3153832671262227771 ) ) ;
#80646 = CARTESIAN_POINT ( 'NONE',  ( 1.509186351706037543, -0.4281496062992127816, -0.4176697321401328100 ) ) ;
#80645 = CARTESIAN_POINT ( 'NONE',  ( -1.614173228346455824, 0.1771653543307087630, 0.000000000000000000 ) ) ;
#80647 = CARTESIAN_POINT ( 'NONE',  ( 0.3917322834645669549, 2.398668435337827645E-17, -2.717828453247031817 ) ) ;
#80648 = FACE_OUTER_BOUND ( 'NONE', #47762, .T. ) ;
#80649 = CARTESIAN_POINT ( 'NONE',  ( 1.187664041994751285, -0.05778040916215522460, 0.4822834645669289988 ) ) ;
#80650 = CARTESIAN_POINT ( 'NONE',  ( -1.463254593175852492, -0.6692913385826773087, -0.1292274648535924053 ) ) ;
#80651 = CARTESIAN_POINT ( 'NONE',  ( -0.09186351706036689768, 0.05413385826771626580, -0.4176697321401330321 ) ) ;
#80652 = CARTESIAN_POINT ( 'NONE',  ( -0.4658792650918627265, -0.05778040916215522460, 0.4822834645669289988 ) ) ;
#80653 = CARTESIAN_POINT ( 'NONE',  ( -1.574803149606298192, -0.1870078740157480879, -0.4822834645669291653 ) ) ;
#80654 = CARTESIAN_POINT ( 'NONE',  ( 4.797336870675656522E-17, -0.3917322834645670104, -0.1633858267716536417 ) ) ;
#80655 = CARTESIAN_POINT ( 'NONE',  ( 0.2034120734908142214, 0.2952755905511810774, -0.1292274648535930714 ) ) ;
#80656 =( BOUNDED_CURVE ( )  B_SPLINE_CURVE ( 2, ( #63152, #76208, #44189, #749, #75382, #39453, #65141, #7477, #62749, #36648, #56821, #56000, #32721 ),
 .UNSPECIFIED., .F., .F. ) 
 B_SPLINE_CURVE_WITH_KNOTS ( ( 3, 2, 2, 2, 2, 2, 3 ),
 ( 0.4125000000000000333, 0.4166666666666667407, 0.4208333333333333925, 0.4250000000000000444, 0.4291666666666666408, 0.4333333333333333481, 0.4375000000000000000 ),
 .UNSPECIFIED. ) 
 CURVE ( )  GEOMETRIC_REPRESENTATION_ITEM ( )  RATIONAL_B_SPLINE_CURVE ( ( 0.9999999999999995559, 0.9659258262890687563, 1.000000000000000000, 0.9659258262890683122, 1.000000000000000000, 0.9659258262890683122, 1.000000000000000000, 0.9659258262890683122, 1.000000000000000000, 0.9659258262890683122, 1.000000000000000000, 0.9659258262890683122, 1.000000000000000000 ) ) 
 REPRESENTATION_ITEM ( '' )  );
#80657 = CARTESIAN_POINT ( 'NONE',  ( 0.3392501089628018329, 0.1958661417322835607, -2.170603674540682260 ) ) ;
#80658 = CARTESIAN_POINT ( 'NONE',  ( 1.509186351706037543, 0.05413385826771666132, 0.4176697321401328100 ) ) ;
#80659 = EDGE_LOOP ( 'NONE', ( #13000, #59794, #59565, #75574 ) ) ;
#80660 = CARTESIAN_POINT ( 'NONE',  ( -0.1058382717557503211, 0.3949938075777409408, -2.526246719160105236 ) ) ;
#80661 = ORIENTED_EDGE ( 'NONE', *, *, #34718, .T. ) ;
#80662 = CARTESIAN_POINT ( 'NONE',  ( 0.4531182788721080934, 1.771653543307086354, -0.5309055118110237448 ) ) ;
#80663 = CARTESIAN_POINT ( 'NONE',  ( -1.489501312335957062, -0.3162353388693409650, -0.4822834645669289433 ) ) ;
#80664 = CARTESIAN_POINT ( 'NONE',  ( 0.3460692066303959202, 0.1998031496062993295, -0.9186351706036745002 ) ) ;
#80665 = CARTESIAN_POINT ( 'NONE',  ( 0.3812812444996376282, 2.409604939980833412E-17, -0.3464511005275205946 ) ) ;
#80666 = CARTESIAN_POINT ( 'NONE',  ( -0.1246719160104980684, 0.2066929133858267931, 0.1054918080437490802 ) ) ;
#80667 = CARTESIAN_POINT ( 'NONE',  ( -0.4744094488189058989, 1.537401574803149984, 2.554262525012261253 ) ) ;
#80668 = DIRECTION ( 'NONE',  ( -1.000000000000000000, -3.412570772413389987E-16, 0.000000000000000000 ) ) ;
#80669 = CARTESIAN_POINT ( 'NONE',  ( 0.1958661417322836440, -0.3392501089628017219, -0.01902887139107619849 ) ) ;
#80670 = CARTESIAN_POINT ( 'NONE',  ( -0.2624671916010490880, -0.5023911411419708095, 0.1820866141732285504 ) ) ;
#80671 = CARTESIAN_POINT ( 'NONE',  ( -1.148293963254592542, -0.5511811023622048555, -0.09757992244046775898 ) ) ;
#80672 = CARTESIAN_POINT ( 'NONE',  ( -1.062992125984250968, -0.6692913385826771977, 8.415575281601705876E-17 ) ) ;
#80673 = CARTESIAN_POINT ( 'NONE',  ( 0.3674540682414705883, 0.2306618581243847221, -0.2411417322834647770 ) ) ;
#80674 = CARTESIAN_POINT ( 'NONE',  ( -1.246719160104985846, -0.4281496062992127816, -0.4176697321401328100 ) ) ;
#80675 = PLANE ( 'NONE',  #9779 ) ;
#80676 = VERTEX_POINT ( 'NONE', #18325 ) ;
#80677 = CARTESIAN_POINT ( 'NONE',  ( -1.286089238845143479, 0.2306618581243847221, -0.2411417322834647770 ) ) ;
#80678 = DIRECTION ( 'NONE',  ( 0.000000000000000000, 0.000000000000000000, -1.000000000000000000 ) ) ;
#80679 = CARTESIAN_POINT ( 'NONE',  ( -0.2362204724409447953, -0.4091458600556404646, -1.640419947506561726 ) ) ;
#80680 = CARTESIAN_POINT ( 'NONE',  ( 2.170146923806635098, 1.528780496884629025, -0.4744094488188970171 ) ) ;
#80681 = CARTESIAN_POINT ( 'NONE',  ( 0.1049643490035303689, 0.3917322834645670104, -0.7729658792650916377 ) ) ;
#80682 = CARTESIAN_POINT ( 'NONE',  ( -1.646051170424378096, 0.000000000000000000, 0.3464511005275205946 ) ) ;
#80683 = CARTESIAN_POINT ( 'NONE',  ( -0.9317585301837263412, -0.4281496062992127816, -0.4176697321401328100 ) ) ;
#80684 = CARTESIAN_POINT ( 'NONE',  ( 1.456692913385827515, -0.6692913385826771977, 8.415575281601705876E-17 ) ) ;
#80686 = DIRECTION ( 'NONE',  ( 0.000000000000000000, -1.000000000000000000, 0.000000000000000000 ) ) ;
#80685 = CARTESIAN_POINT ( 'NONE',  ( -1.653543307086613234, -0.1870078740157480879, -0.4822834645669291653 ) ) ;
#80687 = B_SPLINE_CURVE_WITH_KNOTS ( 'NONE', 3,
 ( #46288, #59338, #53012, #78726, #46710, #37182, #30862, #47120, #15158, #40816, #21462, #34928, #66500, #14751 ),
 .UNSPECIFIED., .F., .F.,
 ( 4, 2, 2, 2, 2, 2, 4 ),
 ( 0.000000000000000000, 0.0003923887041693433029, 0.0007847774083386866058, 0.001177166112508029909, 0.001569554816677373212, 0.002354332225016059817, 0.003139109633354746423 ),
 .UNSPECIFIED. ) ;
#80688 = CARTESIAN_POINT ( 'NONE',  ( -1.679790026246718693, 0.2306618581243847221, -0.2411417322834647770 ) ) ;
#80689 = CARTESIAN_POINT ( 'NONE',  ( -0.8136482939632537770, -0.6046776061558807314, 0.2411417322834647770 ) ) ;
#80690 = CARTESIAN_POINT ( 'NONE',  ( 0.2867679344610365999, -0.2867679344610365999, -0.02097805954624490030 ) ) ;
#80691 = CARTESIAN_POINT ( 'NONE',  ( 0.2427821522309716595, -0.2845877964562161244, -0.3641732283464567121 ) ) ;
#80692 = CARTESIAN_POINT ( 'NONE',  ( -0.1958661417322834220, -0.3392501089628018884, -0.3077427821522311091 ) ) ;
#80693 = CARTESIAN_POINT ( 'NONE',  ( -0.1312335958005241554, -0.5023911411419708095, -0.1820866141732282451 ) ) ;
#80694 = CARTESIAN_POINT ( 'NONE',  ( 1.062992125984252745, -0.5511811023622047445, 6.969142054262312111E-17 ) ) ;
#80695 = CARTESIAN_POINT ( 'NONE',  ( 0.7020997375328090762, -0.05778040916215560624, -0.4822834645669293319 ) ) ;
#80696 = CARTESIAN_POINT ( 'NONE',  ( -0.4002624671916004129, -0.2845877964562159024, 0.3641732283464567677 ) ) ;
#80697 = CARTESIAN_POINT ( 'NONE',  ( -0.2867679344610365999, 0.2867679344610364889, -2.374015748031496287 ) ) ;
#80698 = CARTESIAN_POINT ( 'NONE',  ( -1.561679790026246017, -0.4281496062992127816, -0.4176697321401328100 ) ) ;
#80699 = CARTESIAN_POINT ( 'NONE',  ( -1.469816272965878357, 0.1283753931104748280, 0.1820866141732283561 ) ) ;
#80700 = CARTESIAN_POINT ( 'NONE',  ( 0.3458507752293908943, -0.3458507752293908943, -0.6476377952755905110 ) ) ;
#80701 = CARTESIAN_POINT ( 'NONE',  ( 0.08530183727034192087, -0.3162353388693409650, -0.4822834645669289433 ) ) ;
#80702 = CARTESIAN_POINT ( 'NONE',  ( -0.6102362204724400829, -0.5400638737290845981, -0.3530559997133363437 ) ) ;
#80703 = CARTESIAN_POINT ( 'NONE',  ( 1.548556430446194954, 0.1283753931104746893, -0.1820866141732285504 ) ) ;
#80704 = CARTESIAN_POINT ( 'NONE',  ( 0.2624671916010504757, -0.5023911411419708095, -0.1820866141732282451 ) ) ;
#80705 = CARTESIAN_POINT ( 'NONE',  ( -0.2559055118110230564, 0.1660481256975883668, -0.3530559997133364547 ) ) ;
#80706 = CARTESIAN_POINT ( 'NONE',  ( -0.7939632545931750718, -0.05778040916215560624, -0.4822834645669293319 ) ) ;
#80707 = CARTESIAN_POINT ( 'NONE',  ( -1.595398199321655275, 2.136509776695170615, 0.1559797534342493575 ) ) ;
#80708 = CARTESIAN_POINT ( 'NONE',  ( -1.012524390108115568, 5.991678263669262536E-15, 0.3954985857520036951 ) ) ;
#80709 = CARTESIAN_POINT ( 'NONE',  ( 0.3346456692913393205, -0.5400638737290845981, -0.3530559997133363437 ) ) ;
#80710 = CARTESIAN_POINT ( 'NONE',  ( -0.3996062992125986590, 0.1070741851644051723, -1.999343832020997525 ) ) ;
#80711 = CARTESIAN_POINT ( 'NONE',  ( 1.489501312335958172, -0.05778040916215560624, -0.4822834645669293319 ) ) ;
#80712 = CARTESIAN_POINT ( 'NONE',  ( -0.3215223097112853146, -0.2845877964562159024, 0.3641732283464567677 ) ) ;
#80713 = CARTESIAN_POINT ( 'NONE',  ( -0.4396325459317579898, 0.2952755905511811885, 0.1292274648535926551 ) ) ;
#80714 = CARTESIAN_POINT ( 'NONE',  ( 1.653543307086614789, -0.1870078740157479769, 0.4822834645669291653 ) ) ;
#80715 = CARTESIAN_POINT ( 'NONE',  ( 1.489501312335958172, -0.3162353388693405765, 0.4822834645669290543 ) ) ;
#80716 = CARTESIAN_POINT ( 'NONE',  ( -1.456692913385826182, 0.2952755905511811885, 0.000000000000000000 ) ) ;
#80717 = CARTESIAN_POINT ( 'NONE',  ( -0.8595800524934373854, -0.2845877964562161244, -0.3641732283464567121 ) ) ;
#80719 = ADVANCED_FACE ( 'NONE', ( #63748 ), #7772, .F. ) ;
#80718 = CARTESIAN_POINT ( 'NONE',  ( -0.3996062992125984925, -0.1070741851644056719, -0.2801837270341207553 ) ) ;
#80720 = CARTESIAN_POINT ( 'NONE',  ( 0.1070741851644053527, 0.3996062992125986590, -0.4658792650918635592 ) ) ;
#80721 = CARTESIAN_POINT ( 'NONE',  ( 0.2867679344610366554, -0.2867679344610365999, -2.772329027067928386 ) ) ;
#80722 = CARTESIAN_POINT ( 'NONE',  ( 1.620734908136483465, -0.5511811023622046335, 0.09757992244046803654 ) ) ;
#80723 = CARTESIAN_POINT ( 'NONE',  ( 1.266404199475066328, -0.08942795157527998196, 0.3641732283464567121 ) ) ;
#80724 = CARTESIAN_POINT ( 'NONE',  ( 0.8530183727034126306, 0.05413385826771626580, -0.4176697321401330321 ) ) ;
#80725 = CARTESIAN_POINT ( 'NONE',  ( -1.568241469816272105, -0.05778040916215522460, 0.4822834645669289988 ) ) ;
#80726 = CARTESIAN_POINT ( 'NONE',  ( 0.7152230971128614723, -0.3162353388693409650, -0.4822834645669289433 ) ) ;
#80727 = CARTESIAN_POINT ( 'NONE',  ( 0.1974969037888706092, -0.3420746716998660508, -0.7985564304461942875 ) ) ;
#80728 = CARTESIAN_POINT ( 'NONE',  ( 1.377952755905512472, 0.1771653543307087630, 0.000000000000000000 ) ) ;
#80729 = CARTESIAN_POINT ( 'NONE',  ( 0.2362204724409456558, -0.1870078740157479769, 0.4822834645669291653 ) ) ;
#80730 = CARTESIAN_POINT ( 'NONE',  ( -0.8005249343832011588, 0.05413385826771626580, -0.4176697321401330321 ) ) ;
#80731 = CARTESIAN_POINT ( 'NONE',  ( 1.259842519685040019, -0.1870078740157480879, -0.4822834645669291653 ) ) ;
#80732 = CARTESIAN_POINT ( 'NONE',  ( 0.1265901696524989462, 0.4724409448818897572, -1.253280839895013044 ) ) ;
#80733 = CARTESIAN_POINT ( 'NONE',  ( 0.1070741851644054915, -0.3996062992125985480, -2.447506561679789527 ) ) ;
#80734 = CARTESIAN_POINT ( 'NONE',  ( 0.3412073490813655186, 0.1283753931104748280, 0.1820866141732283561 ) ) ;
#80735 = VERTEX_POINT ( 'NONE', #77216 ) ;
#80736 = CARTESIAN_POINT ( 'NONE',  ( -0.3917322834645670659, -7.196005306013484475E-17, -0.6660298144695031564 ) ) ;
#80737 = ORIENTED_EDGE ( 'NONE', *, *, #13177, .T. ) ;
#80738 = CARTESIAN_POINT ( 'NONE',  ( -0.2559055118110230564, 0.1660481256975883668, -0.3530559997133364547 ) ) ;
#80739 = CARTESIAN_POINT ( 'NONE',  ( -0.3871391076115476282, -0.05778040916215522460, 0.4822834645669289988 ) ) ;
#80740 = CARTESIAN_POINT ( 'NONE',  ( -0.2165354330708654795, 0.1660481256975885056, 0.3530559997133364547 ) ) ;
#80741 = CARTESIAN_POINT ( 'NONE',  ( 0.8202099737532814183, -0.6692913385826773087, -0.1292274648535924053 ) ) ;
#80742 = CARTESIAN_POINT ( 'NONE',  ( -0.7874015748031489847, -0.1870078740157480879, -0.4822834645669291653 ) ) ;
#80743 = CARTESIAN_POINT ( 'NONE',  ( -0.5905511811023615998, 0.2952755905511811885, 0.000000000000000000 ) ) ;
#80744 = CARTESIAN_POINT ( 'NONE',  ( 1.253280839895013710, -0.3162353388693405765, 0.4822834645669290543 ) ) ;
#80745 = CARTESIAN_POINT ( 'NONE',  ( 0.6233595800524939223, -0.3162353388693405765, 0.4822834645669290543 ) ) ;
#80746 = CARTESIAN_POINT ( 'NONE',  ( 0.6430446194225729606, -0.4281496062992127816, -0.4176697321401328100 ) ) ;
#80747 = CARTESIAN_POINT ( 'NONE',  ( 0.3917322834645669549, 0.1049643490035304660, -1.219160104986876325 ) ) ;
#80748 = CARTESIAN_POINT ( 'NONE',  ( -0.5380577427821514602, -0.004921259842519576551, 0.3153832671262227771 ) ) ;
#80749 = ORIENTED_EDGE ( 'NONE', *, *, #6655, .F. ) ;
#80750 = CARTESIAN_POINT ( 'NONE',  ( 0.3949938075777409408, 0.1058382717557500574, -0.9120734908136481911 ) ) ;
#80751 = VERTEX_POINT ( 'NONE', #6087 ) ;
#80752 = CARTESIAN_POINT ( 'NONE',  ( -0.7939632545931754048, -0.2845877964562159024, 0.3641732283464567677 ) ) ;
#80753 = CARTESIAN_POINT ( 'NONE',  ( -0.6167979002624665030, -0.4281496062992127816, -0.4176697321401328100 ) ) ;
#80754 = DIRECTION ( 'NONE',  ( 0.000000000000000000, 0.000000000000000000, -1.000000000000000000 ) ) ;
#80755 = CARTESIAN_POINT ( 'NONE',  ( -0.6102362204724400829, 0.1660481256975885056, 0.3530559997133364547 ) ) ;
#80756 = CARTESIAN_POINT ( 'NONE',  ( -0.9186351706036736120, 0.2306618581243848609, 0.2411417322834645549 ) ) ;
#80757 = CARTESIAN_POINT ( 'NONE',  ( -1.332020997375327642, -0.05778040916215522460, 0.4822834645669289988 ) ) ;
#80758 = CARTESIAN_POINT ( 'NONE',  ( -1.482939632545930975, -0.4281496062992127816, -0.4176697321401328100 ) ) ;
#80759 = CARTESIAN_POINT ( 'NONE',  ( 1.036745406824147731, -0.004921259842519576551, 0.3153832671262227771 ) ) ;
#80760 = CARTESIAN_POINT ( 'NONE',  ( 0.4613966517175972504, 1.648900267337816139, 1.022797972794818655 ) ) ;
#80761 = CARTESIAN_POINT ( 'NONE',  ( -1.572991167713776672, 2.401574803149606474, 0.1227090857360981641 ) ) ;
#80762 = CARTESIAN_POINT ( 'NONE',  ( 0.2887139107611556010, -0.5023911411419708095, 0.1820866141732285504 ) ) ;
#80763 = CARTESIAN_POINT ( 'NONE',  ( 0.1706036745406830368, -0.4281496062992127816, -0.4176697321401328100 ) ) ;
#80764 = CARTESIAN_POINT ( 'NONE',  ( -0.01968503937007793844, 0.1660481256975883668, -0.3530559997133364547 ) ) ;
#80765 = ORIENTED_EDGE ( 'NONE', *, *, #77818, .F. ) ;
#80766 = CARTESIAN_POINT ( 'NONE',  ( -0.3460692066303958092, -0.1998031496062994683, -1.784776902887138972 ) ) ;
#80767 = CARTESIAN_POINT ( 'NONE',  ( -0.6167979002624665030, 0.05413385826771666132, 0.4176697321401328100 ) ) ;
#80768 = ORIENTED_EDGE ( 'NONE', *, *, #76404, .F. ) ;
#80769 = CARTESIAN_POINT ( 'NONE',  ( 0.1998031496062994128, -0.3460692066303957537, -1.270997375328083878 ) ) ;
#80770 = CARTESIAN_POINT ( 'NONE',  ( -0.1970133122064499087, 0.2199809220305531388, 0.1374248322900813168 ) ) ;
#80771 = CARTESIAN_POINT ( 'NONE',  ( -0.5905511811023615998, 0.1771653543307087630, 0.000000000000000000 ) ) ;
#80772 = CARTESIAN_POINT ( 'NONE',  ( -1.017060367454067249, -0.3162353388693409650, -0.4822834645669289433 ) ) ;
#80773 = CARTESIAN_POINT ( 'NONE',  ( 0.3458507752293908943, -0.3458507752293908943, -0.4133858267716534196 ) ) ;
#80774 = CARTESIAN_POINT ( 'NONE',  ( 4.797336870675656522E-17, -0.3917322834645670104, -2.525590551181102317 ) ) ;
#80775 = CARTESIAN_POINT ( 'NONE',  ( 1.574803149606299746, -0.1870078740157480879, -0.4822834645669291653 ) ) ;
#80776 = CARTESIAN_POINT ( 'NONE',  ( 0.5118110236220478892, 0.2952755905511811885, 0.000000000000000000 ) ) ;
#80777 = CARTESIAN_POINT ( 'NONE',  ( 0.7152230971128616943, -0.05778040916215522460, 0.4822834645669289988 ) ) ;
#80778 = CARTESIAN_POINT ( 'NONE',  ( -0.5643044619422565855, -0.3690944881889763329, 0.3153832671262228327 ) ) ;
#80779 = CARTESIAN_POINT ( 'NONE',  ( -0.07217847769028813698, -0.3162353388693409650, -0.4822834645669289433 ) ) ;
#80780 = CARTESIAN_POINT ( 'NONE',  ( -0.4724409448818899238, 0.1265901696524986686, -2.156824146981627166 ) ) ;
#80781 = CARTESIAN_POINT ( 'NONE',  ( -0.4133858267716528645, 0.1660481256975883668, -0.3530559997133364547 ) ) ;
#80782 = CARTESIAN_POINT ( 'NONE',  ( -0.2891555358219909388, -0.2891555358219912164, -1.868110236220472009 ) ) ;
#80783 = CARTESIAN_POINT ( 'NONE',  ( 1.325459317585302665, -0.004921259842519870586, -0.3153832671262229437 ) ) ;
#80784 = CARTESIAN_POINT ( 'NONE',  ( 0.1509186351706042484, -0.2845877964562159024, 0.3641732283464567677 ) ) ;
#80785 = CARTESIAN_POINT ( 'NONE',  ( 1.049868766404200349, 0.1283753931104748280, 0.1820866141732283561 ) ) ;
#80786 = CARTESIAN_POINT ( 'NONE',  ( -0.9514435695538050464, -0.3162353388693405765, 0.4822834645669290543 ) ) ;
#80787 = AXIS2_PLACEMENT_3D ( 'NONE', #13353, #32698, #52043 ) ;
#80788 = CARTESIAN_POINT ( 'NONE',  ( -1.325459317585300889, -0.004921259842519576551, 0.3153832671262227771 ) ) ;
#80789 = DIRECTION ( 'NONE',  ( 0.8660254037844361541, 0.000000000000000000, 0.5000000000000043299 ) ) ;
#80790 = CARTESIAN_POINT ( 'NONE',  ( -1.240157480314959759, 0.1660481256975885056, 0.3530559997133364547 ) ) ;
#80791 = CARTESIAN_POINT ( 'NONE',  ( -0.6299212598425188991, -0.1870078740157480879, -0.4822834645669291653 ) ) ;
#80792 = CARTESIAN_POINT ( 'NONE',  ( 0.4068241469816281097, 0.05413385826771666132, 0.4176697321401328100 ) ) ;
#80793 = CARTESIAN_POINT ( 'NONE',  ( -9.594673741351310580E-17, 0.3917322834645669549, -2.442237902065930388 ) ) ;
#80794 = CARTESIAN_POINT ( 'NONE',  ( -1.851299440327907941, 1.063968899401423140, -0.03484477857459079841 ) ) ;
#80795 = CARTESIAN_POINT ( 'NONE',  ( 0.4199475065616805614, 0.1283753931104748280, 0.1820866141732283561 ) ) ;
#80796 = CARTESIAN_POINT ( 'NONE',  ( 0.8858267716535438430, -0.5400638737290845981, -0.3530559997133363437 ) ) ;
#80797 = CARTESIAN_POINT ( 'NONE',  ( -0.3458507752293909498, 0.3458507752293908388, -1.041338582677165281 ) ) ;
#80798 = CARTESIAN_POINT ( 'NONE',  ( 0.7742782152230979209, 0.05413385826771626580, -0.4176697321401330321 ) ) ;
#80799 = CARTESIAN_POINT ( 'NONE',  ( -1.706036745406823485, 0.1283753931104748280, 0.1820866141732283561 ) ) ;
#80800 = CARTESIAN_POINT ( 'NONE',  ( -1.463254593175852492, -0.6692913385826773087, -0.1292274648535924053 ) ) ;
#80801 = CARTESIAN_POINT ( 'NONE',  ( -0.8923884514435688198, 0.2306618581243847221, -0.2411417322834647770 ) ) ;
#80802 = CARTESIAN_POINT ( 'NONE',  ( -0.1377952755905504645, -0.4536011799217368745, -0.2665933059059886201 ) ) ;
#80803 = CARTESIAN_POINT ( 'NONE',  ( -0.2726377952755906220, -0.1938976377952756625, 0.1574803149606299191 ) ) ;
#80804 = CARTESIAN_POINT ( 'NONE',  ( 0.7742782152230978099, -0.3690944881889763329, 0.3153832671262228327 ) ) ;
#80805 = VECTOR ( 'NONE', #40848, 39.37007874015748143 ) ;
#80806 = CARTESIAN_POINT ( 'NONE',  ( 0.06561679790026316017, -0.4281496062992124485, 0.4176697321401328655 ) ) ;
#80807 = CARTESIAN_POINT ( 'NONE',  ( -9.787531504996566615E-17, 0.3996062992125985480, -0.3917322834645669549 ) ) ;
#80808 = ADVANCED_FACE ( 'NONE', ( #18726 ), #62123, .F. ) ;
#80809 = CARTESIAN_POINT ( 'NONE',  ( -1.312335958005248715, -0.6046776061558809534, -0.2411417322834644161 ) ) ;
#80810 = CARTESIAN_POINT ( 'NONE',  ( 0.1049643490035304938, -0.3917322834645669549, -1.902230971128608727 ) ) ;
#80811 = CARTESIAN_POINT ( 'NONE',  ( 0.8858267716535438430, -0.4536011799217368745, -0.2665933059059886201 ) ) ;
#80812 = CARTESIAN_POINT ( 'NONE',  ( 0.1181102362204730916, 0.2952755905511811885, 0.000000000000000000 ) ) ;
#80813 = CARTESIAN_POINT ( 'NONE',  ( -0.07874015748031421014, -0.1870078740157479769, 0.4822834645669291653 ) ) ;
#80814 = CARTESIAN_POINT ( 'NONE',  ( -0.3871391076115476282, -0.08942795157527998196, 0.3641732283464567121 ) ) ;
#80815 = CARTESIAN_POINT ( 'NONE',  ( 0.9573014326657177664, 0.000000000000000000, 0.3464511005275205946 ) ) ;
#80816 = CARTESIAN_POINT ( 'NONE',  ( -0.5446194225721777693, -0.08942795157527998196, 0.3641732283464567121 ) ) ;
#80817 = CARTESIAN_POINT ( 'NONE',  ( 0.2296587926509192634, -0.3162353388693405765, 0.4822834645669290543 ) ) ;
#80818 = CARTESIAN_POINT ( 'NONE',  ( -1.358267716535432434, 0.07958543189024071263, -0.2665933059059888421 ) ) ;
#80819 = CARTESIAN_POINT ( 'NONE',  ( 0.3460692066303958092, 0.1998031496062993018, -1.467847769028871596 ) ) ;
#80820 = CARTESIAN_POINT ( 'NONE',  ( -1.653543307086613234, -0.1870078740157479769, 0.4822834645669291653 ) ) ;
#80821 = DIRECTION ( 'NONE',  ( -0.000000000000000000, -1.000000000000000000, -0.000000000000000000 ) ) ;
#80822 = ORIENTED_EDGE ( 'NONE', *, *, #38397, .F. ) ;
#80823 = CARTESIAN_POINT ( 'NONE',  ( -1.391076115485563758, 0.1283753931104748280, 0.1820866141732283561 ) ) ;
#80824 = CARTESIAN_POINT ( 'NONE',  ( -0.4593175853018366950, 0.05413385826771666132, 0.4176697321401328100 ) ) ;
#80825 = CARTESIAN_POINT ( 'NONE',  ( -1.351706036745406347, -0.4281496062992124485, 0.4176697321401328655 ) ) ;
#80826 = CARTESIAN_POINT ( 'NONE',  ( 0.1958661417322836440, -0.3392501089628017219, -1.593832020997375531 ) ) ;
#80827 = CARTESIAN_POINT ( 'NONE',  ( -0.3458507752293906723, -0.3458507752293910609, -2.106299212598425008 ) ) ;
#80828 = CARTESIAN_POINT ( 'NONE',  ( 1.253280839895013710, -0.05778040916215560624, -0.4822834645669293319 ) ) ;
#80829 = CARTESIAN_POINT ( 'NONE',  ( 0.5446194225721792126, -0.3162353388693405765, 0.4822834645669290543 ) ) ;
#80830 = CARTESIAN_POINT ( 'NONE',  ( 0.4724409448818898682, 2.892866454678787531E-17, -2.637795275590551380 ) ) ;
#80831 = CARTESIAN_POINT ( 'NONE',  ( 0.1998031496062994128, -0.3460692066303957537, -2.530839895013123453 ) ) ;
#80832 = CARTESIAN_POINT ( 'NONE',  ( 1.601049868766404982, 0.1283753931104748280, 0.1820866141732283561 ) ) ;
#80833 = B_SPLINE_CURVE_WITH_KNOTS ( 'NONE', 3,
 ( #54416, #48515, #60739, #36308, #17390, #48932, #29578, #61574 ),
 .UNSPECIFIED., .F., .F.,
 ( 4, 2, 2, 4 ),
 ( 0.07055950480717279594, 0.07177139162174094034, 0.07298327843630908474, 0.07540705206544540129 ),
 .UNSPECIFIED. ) ;
#80834 = CARTESIAN_POINT ( 'NONE',  ( 0.3996062992125986590, -0.1070741851644053111, -0.7414698162729659314 ) ) ;
#80835 = VERTEX_POINT ( 'NONE', #11071 ) ;
#80836 = CARTESIAN_POINT ( 'NONE',  ( -1.010498687664041384, -0.004921259842519576551, 0.3153832671262227771 ) ) ;
#80837 = CARTESIAN_POINT ( 'NONE',  ( 0.2867679344610365999, 0.2867679344610365999, -2.807086614173227357 ) ) ;
#80838 = ORIENTED_EDGE ( 'NONE', *, *, #48541, .T. ) ;
#80839 = CARTESIAN_POINT ( 'NONE',  ( 0.8464566929133865436, 0.1660481256975883668, -0.3530559997133364547 ) ) ;
#80840 = CARTESIAN_POINT ( 'NONE',  ( -0.5446194225721777693, -0.3162353388693409650, -0.4822834645669289433 ) ) ;
#80841 = CARTESIAN_POINT ( 'NONE',  ( -0.9383202099737524282, -0.3162353388693409650, -0.4822834645669289433 ) ) ;
#80842 = CARTESIAN_POINT ( 'NONE',  ( 1.089238845144357759, 0.05413385826771626580, -0.4176697321401330321 ) ) ;
#80843 = CARTESIAN_POINT ( 'NONE',  ( -1.364829396325458521, -0.5023911411419708095, 0.1820866141732285504 ) ) ;
#80844 = CARTESIAN_POINT ( 'NONE',  ( 0.2460629921259842590, 0.000000000000000000, 0.000000000000000000 ) ) ;
#80845 = CARTESIAN_POINT ( 'NONE',  ( 0.1706036745406830368, -0.4281496062992127816, -0.4176697321401328100 ) ) ;
#80846 = AXIS2_PLACEMENT_3D ( 'NONE', #11768, #31511, #58004 ) ;
#80847 = CARTESIAN_POINT ( 'NONE',  ( -0.7874015748031489847, -0.1870078740157480879, -0.4822834645669291653 ) ) ;
#80848 = CARTESIAN_POINT ( 'NONE',  ( -0.1049643490035301746, -0.3917322834645670659, -1.727014804953068916 ) ) ;
#80849 = CARTESIAN_POINT ( 'NONE',  ( -1.181102362204723644, -0.1870078740157479769, 0.4822834645669291653 ) ) ;
#80850 = PLANE ( 'NONE',  #51917 ) ;
#80851 = CARTESIAN_POINT ( 'NONE',  ( 0.9908136482939640111, -0.6692913385826771977, 0.1292274648535927661 ) ) ;
#80852 = CARTESIAN_POINT ( 'NONE',  ( 0.3392501089628018329, 0.1958661417322835607, -2.735564304461941987 ) ) ;
#80853 = CARTESIAN_POINT ( 'NONE',  ( 1.410761154855643795, -0.08942795157528024563, -0.3641732283464568787 ) ) ;
#80854 = ORIENTED_EDGE ( 'NONE', *, *, #80976, .T. ) ;
#80855 = CARTESIAN_POINT ( 'NONE',  ( -0.3917322834645671770, 0.1049643490035302024, -2.706712229167666184 ) ) ;
#80856 = CARTESIAN_POINT ( 'NONE',  ( -0.5905511811023613777, -0.6692913385826771977, 8.415575281601705876E-17 ) ) ;
#80857 = ORIENTED_EDGE ( 'NONE', *, *, #77077, .T. ) ;
#80858 = CARTESIAN_POINT ( 'NONE',  ( 0.2493438320209980519, -0.3690944881889765550, -0.3153832671262227771 ) ) ;
#80859 = CARTESIAN_POINT ( 'NONE',  ( -1.522309711286088607, 0.2306618581243847221, -0.2411417322834647770 ) ) ;
#80860 = CARTESIAN_POINT ( 'NONE',  ( 0.6102362204724416372, -0.5400638737290844871, 0.3530559997133364547 ) ) ;
#80861 = CARTESIAN_POINT ( 'NONE',  ( 0.9645669291338588858, 0.1660481256975885056, 0.3530559997133364547 ) ) ;
#80862 = CARTESIAN_POINT ( 'NONE',  ( -0.2296587926509179312, -0.3162353388693409650, -0.4822834645669289433 ) ) ;
#80863 = CARTESIAN_POINT ( 'NONE',  ( -0.3917322834645670659, -7.196005306013484475E-17, -1.453431389272652696 ) ) ;
#80864 = CARTESIAN_POINT ( 'NONE',  ( -0.8661417322834640276, -0.1870078740157479769, 0.4822834645669291653 ) ) ;
#80865 = CARTESIAN_POINT ( 'NONE',  ( 0.3917322834645670104, 2.398668435337828261E-17, -2.092519685039370358 ) ) ;
#80866 = CARTESIAN_POINT ( 'NONE',  ( -1.620734908136482577, -0.6692913385826773087, -0.1292274648535924053 ) ) ;
#80867 = CARTESIAN_POINT ( 'NONE',  ( -0.8792650918635160906, -0.4281496062992124485, 0.4176697321401328655 ) ) ;
#80868 = CARTESIAN_POINT ( 'NONE',  ( 1.351706036745407680, 0.05413385826771666132, 0.4176697321401328100 ) ) ;
#80869 = CARTESIAN_POINT ( 'NONE',  ( 1.181102362204725198, -0.1870078740157479769, 0.4822834645669291653 ) ) ;
#80870 = CARTESIAN_POINT ( 'NONE',  ( 0.2925321140481932369, -0.2925321140481932369, -0.5708661417322833387 ) ) ;
#80871 = CARTESIAN_POINT ( 'NONE',  ( -1.122047244094487306, -0.5400638737290844871, 0.3530559997133364547 ) ) ;
#80872 = CARTESIAN_POINT ( 'NONE',  ( 4.893765752498283308E-17, -0.3996062992125985480, 0.001968503937007862279 ) ) ;
#80873 = CARTESIAN_POINT ( 'NONE',  ( 0.2821522309711292364, -0.6692913385826771977, 0.1292274648535927661 ) ) ;
#80874 = CARTESIAN_POINT ( 'NONE',  ( 0.1070741851644054915, -0.3996062992125986035, -2.132545931758530244 ) ) ;
#80875 = CARTESIAN_POINT ( 'NONE',  ( -0.4199475065616791736, -0.6046776061558807314, 0.2411417322834647770 ) ) ;
#80876 = CARTESIAN_POINT ( 'NONE',  ( -1.640419947506561060, -0.004921259842519576551, 0.3153832671262227771 ) ) ;
#80877 = CARTESIAN_POINT ( 'NONE',  ( 0.5905511811023629321, 0.1771653543307087630, 0.000000000000000000 ) ) ;
#80878 = CARTESIAN_POINT ( 'NONE',  ( 1.292650918635171564, 0.2952755905511811885, 0.1292274648535926551 ) ) ;
#80879 = CARTESIAN_POINT ( 'NONE',  ( 0.4724409448818897572, -0.1265901696524988906, -0.9757217847769029673 ) ) ;
#80880 = CARTESIAN_POINT ( 'NONE',  ( 0.9711286089238851948, -0.5023911411419708095, -0.1820866141732282451 ) ) ;
#80881 = CARTESIAN_POINT ( 'NONE',  ( 0.9120734908136489683, -0.6692913385826771977, 0.1292274648535927661 ) ) ;
#80882 = CARTESIAN_POINT ( 'NONE',  ( 0.2891555358219910499, 0.2891555358219910499, -0.5295275590551180578 ) ) ;
#80883 = CARTESIAN_POINT ( 'NONE',  ( -0.7217847769028863381, 0.05413385826771626580, -0.4176697321401330321 ) ) ;
#80884 = CARTESIAN_POINT ( 'NONE',  ( 0.08874907683610111508, -2.191421614605370878E-15, 0.4445507791589071167 ) ) ;
#80885 = CARTESIAN_POINT ( 'NONE',  ( 1.548556430446194954, -0.5023911411419708095, 0.1820866141732285504 ) ) ;
#80886 = CARTESIAN_POINT ( 'NONE',  ( -0.6627296587926503335, -0.6692913385826771977, 0.1292274648535927661 ) ) ;
#80887 = CARTESIAN_POINT ( 'NONE',  ( 0.2099737532808405305, 0.2306618581243847221, -0.2411417322834647770 ) ) ;
#80888 = CARTESIAN_POINT ( 'NONE',  ( -1.148293963254592542, 0.2952755905511811885, 0.1292274648535926551 ) ) ;
#80889 = CARTESIAN_POINT ( 'NONE',  ( 0.2165354330708668673, 0.1660481256975883668, -0.3530559997133364547 ) ) ;
#80890 = CARTESIAN_POINT ( 'NONE',  ( 0.3346456692913393205, -0.4536011799217368745, -0.2665933059059886201 ) ) ;
#80891 = CARTESIAN_POINT ( 'NONE',  ( 0.8530183727034126306, 0.009842519685039144428, -0.3409548833797004797 ) ) ;
#80892 = CARTESIAN_POINT ( 'NONE',  ( -0.02624671916010428221, 0.1283753931104746893, -0.1820866141732285504 ) ) ;
#80893 = CARTESIAN_POINT ( 'NONE',  ( 0.8530183727034126306, -0.004921259842519870586, -0.3153832671262229437 ) ) ;
#80894 = PLANE ( 'NONE',  #49175 ) ;
#80895 = CARTESIAN_POINT ( 'NONE',  ( 0.3996062992125985480, 2.446882876249141654E-17, -1.927165354330708791 ) ) ;
#80896 = CARTESIAN_POINT ( 'NONE',  ( 0.4593175853018380828, 0.05413385826771626580, -0.4176697321401330321 ) ) ;
#80897 = CARTESIAN_POINT ( 'NONE',  ( 0.3917322834645669549, 0.1049643490035304660, -1.219160104986876325 ) ) ;
#80898 = CARTESIAN_POINT ( 'NONE',  ( 1.476377952755906442, -0.4536011799217367080, 0.2665933059059888421 ) ) ;
#80899 = CARTESIAN_POINT ( 'NONE',  ( 0.1377952755905518800, 0.1660481256975883391, -0.3530559997133364547 ) ) ;
#80900 = CARTESIAN_POINT ( 'NONE',  ( 0.1640419947506569498, -0.08942795157527998196, 0.3641732283464567121 ) ) ;
#80901 = CARTESIAN_POINT ( 'NONE',  ( 0.1115485564304470323, 0.2952755905511811885, 0.1292274648535926551 ) ) ;
#80902 = CARTESIAN_POINT ( 'NONE',  ( 1.292650918635171564, -0.5511811023622048555, -0.09757992244046775898 ) ) ;
#80903 = CARTESIAN_POINT ( 'NONE',  ( -1.279527559055116948, -0.4536011799217367080, 0.2665933059059888421 ) ) ;
#80904 = CARTESIAN_POINT ( 'NONE',  ( -1.555118110236219930, 0.1660481256975885056, 0.3530559997133364547 ) ) ;
#80905 = VECTOR ( 'NONE', #69155, 39.37007874015748143 ) ;
#80906 = CARTESIAN_POINT ( 'NONE',  ( 0.1902887139107617975, -0.6692913385826773087, -0.1292274648535924053 ) ) ;
#80907 = CARTESIAN_POINT ( 'NONE',  ( 1.279527559055118724, -0.5400638737290845981, -0.3530559997133363437 ) ) ;
#80908 = LINE ( 'NONE', #54797, #22227 ) ;
#80909 = CARTESIAN_POINT ( 'NONE',  ( -0.03280839895013062252, -0.6692913385826771977, 0.1292274648535927661 ) ) ;
#80910 = CARTESIAN_POINT ( 'NONE',  ( 1.233595800524935227, 0.2306618581243847221, -0.2411417322834647770 ) ) ;
#80911 = CARTESIAN_POINT ( 'NONE',  ( 1.154855643044620184, -0.6046776061558807314, 0.2411417322834647770 ) ) ;
#80912 = CARTESIAN_POINT ( 'NONE',  ( -1.586052503253845503, 2.125984251968505045, -0.1653254495020588799 ) ) ;
#80913 = CARTESIAN_POINT ( 'NONE',  ( 0.8070866141732289112, -0.4536011799217368745, -0.2665933059059886201 ) ) ;
#80914 = CARTESIAN_POINT ( 'NONE',  ( 1.496062992125985147, -0.1870078740157479769, 0.4822834645669291653 ) ) ;
#80915 = CARTESIAN_POINT ( 'NONE',  ( 0.2427821522309716595, -0.2845877964562161244, -0.3641732283464567121 ) ) ;
#80916 = CARTESIAN_POINT ( 'NONE',  ( -0.3871391076115476282, -0.05778040916215522460, 0.4822834645669289988 ) ) ;
#80917 = CARTESIAN_POINT ( 'NONE',  ( 0.5249343832021003964, 0.2306618581243847221, -0.2411417322834647770 ) ) ;
#80918 = CARTESIAN_POINT ( 'NONE',  ( -0.1902887139107604098, 0.2952755905511810774, -0.1292274648535930714 ) ) ;
#80919 = CARTESIAN_POINT ( 'NONE',  ( 0.3917322834645670659, 2.398668435337828261E-17, -2.162092806595487637 ) ) ;
#80920 = CARTESIAN_POINT ( 'NONE',  ( -0.1706036745406816491, -0.3690944881889763329, 0.3153832671262228327 ) ) ;
#80921 = CARTESIAN_POINT ( 'NONE',  ( 0.7283464566929140904, -0.5400638737290845981, -0.3530559997133363437 ) ) ;
#80922 = CARTESIAN_POINT ( 'NONE',  ( 1.049868766404200349, 0.1283753931104748280, 0.1820866141732283561 ) ) ;
#80923 = CARTESIAN_POINT ( 'NONE',  ( -1.720695750894368548, 1.210707077873740767, 0.3442465688542959978 ) ) ;
#80925 = DIRECTION ( 'NONE',  ( 0.000000000000000000, 0.000000000000000000, -1.000000000000000000 ) ) ;
#80924 = CARTESIAN_POINT ( 'NONE',  ( -0.9324623468618411515, 0.000000000000000000, 0.3464511005275205946 ) ) ;
#80926 = DIRECTION ( 'NONE',  ( 0.000000000000000000, 0.000000000000000000, 1.000000000000000000 ) ) ;
#80927 = CARTESIAN_POINT ( 'NONE',  ( -1.227034120734907141, -0.6692913385826773087, -0.1292274648535924053 ) ) ;
#80928 = CARTESIAN_POINT ( 'NONE',  ( -0.5249343832020990641, -0.6046776061558809534, -0.2411417322834644161 ) ) ;
#80929 = CARTESIAN_POINT ( 'NONE',  ( -0.1998031496062994683, 0.3460692066303958092, -2.847769028871391050 ) ) ;
#80930 = CARTESIAN_POINT ( 'NONE',  ( -0.3949938075777409963, -7.255918531996591613E-17, -2.401574803149606474 ) ) ;
#80931 = ORIENTED_EDGE ( 'NONE', *, *, #34562, .F. ) ;
#80932 = CARTESIAN_POINT ( 'NONE',  ( 0.1246719160104994284, 0.1771653543307087075, -0.09757992244046823083 ) ) ;
#80933 = CARTESIAN_POINT ( 'NONE',  ( 0.3917322834645670104, 2.398668435337828261E-17, -0.8976377952755905110 ) ) ;
#80934 = CARTESIAN_POINT ( 'NONE',  ( 1.200787401574803681, -0.5400638737290845981, -0.3530559997133363437 ) ) ;
#80935 = CARTESIAN_POINT ( 'NONE',  ( 0.4091458600556404646, -0.2362204724409448231, -2.309711286089239035 ) ) ;
#80936 = CARTESIAN_POINT ( 'NONE',  ( 1.012036180893693293, 0.02791078216816447743, -0.4328096321851892525 ) ) ;
#80937 = CARTESIAN_POINT ( 'NONE',  ( -0.2887139107611542133, 0.2306618581243848609, 0.2411417322834645549 ) ) ;
#80938 = CARTESIAN_POINT ( 'NONE',  ( 0.4359958488159758616, 1.724409448818897905, -1.033875059083675163 ) ) ;
#80939 = EDGE_CURVE ( 'NONE', #27190, #80251, #79867, .T. ) ;
#80940 = CARTESIAN_POINT ( 'NONE',  ( 1.430446194225722500, -0.004921259842519576551, 0.3153832671262227771 ) ) ;
#80941 = CARTESIAN_POINT ( 'NONE',  ( 0.6299212598425204535, -0.1870078740157480879, -0.4822834645669291653 ) ) ;
#80942 = CARTESIAN_POINT ( 'NONE',  ( 0.2867679344610365999, -0.2867679344610365999, -0.1784583745068747673 ) ) ;
#80943 = CARTESIAN_POINT ( 'NONE',  ( 0.1968503937007881344, -0.6692913385826771977, 8.415575281601705876E-17 ) ) ;
#80944 = CARTESIAN_POINT ( 'NONE',  ( -0.7414698162729651543, 0.1771653543307087075, -0.09757992244046823083 ) ) ;
#80945 = CARTESIAN_POINT ( 'NONE',  ( 0.6364829396325465405, -0.05778040916215522460, 0.4822834645669289988 ) ) ;
#80947 = EDGE_CURVE ( 'NONE', #46125, #46648, #54431, .T. ) ;
#80946 = CARTESIAN_POINT ( 'NONE',  ( -0.1377952755905504645, 0.1660481256975885056, 0.3530559997133364547 ) ) ;
#80948 = CARTESIAN_POINT ( 'NONE',  ( 0.2017716535433070613, -0.2017716535433070890, -0.3937007874015748254 ) ) ;
#80949 = CARTESIAN_POINT ( 'NONE',  ( 0.3996062992125986590, -0.1070741851644053111, -2.946194225721785465 ) ) ;
#80950 = CARTESIAN_POINT ( 'NONE',  ( -0.3917322834645670104, -0.1049643490035307020, -1.617473384023309091 ) ) ;
#80951 = CARTESIAN_POINT ( 'NONE',  ( 0.8005249343832028242, -0.4281496062992127816, -0.4176697321401328100 ) ) ;
#80952 = CARTESIAN_POINT ( 'NONE',  ( -0.2887139107611542133, 0.2306618581243848609, 0.2411417322834645549 ) ) ;
#80953 = CARTESIAN_POINT ( 'NONE',  ( -1.200787401574802349, -0.5400638737290844871, 0.3530559997133364547 ) ) ;
#80954 = CARTESIAN_POINT ( 'NONE',  ( 1.141732283464567566, 0.2952755905511811885, 0.000000000000000000 ) ) ;
#80955 = CARTESIAN_POINT ( 'NONE',  ( 0.4461942257217856311, 0.2306618581243847221, -0.2411417322834647770 ) ) ;
#80956 = CARTESIAN_POINT ( 'NONE',  ( -9.594673741351313045E-17, 0.3917322834645670104, -1.029527559055118280 ) ) ;
#80957 = CARTESIAN_POINT ( 'NONE',  ( -0.2559055118110230564, 0.1660481256975883668, -0.3530559997133364547 ) ) ;
#80958 = CARTESIAN_POINT ( 'NONE',  ( 0.2230971128608932319, -0.4281496062992124485, 0.4176697321401328655 ) ) ;
#80959 = CARTESIAN_POINT ( 'NONE',  ( -0.2690288713910754526, -0.6692913385826771977, 0.1292274648535927661 ) ) ;
#80960 = CARTESIAN_POINT ( 'NONE',  ( 0.3083989501312343062, -0.08942795157528024563, -0.3641732283464568787 ) ) ;
#80961 = FACE_OUTER_BOUND ( 'NONE', #40361, .T. ) ;
#80962 = CARTESIAN_POINT ( 'NONE',  ( -1.666666666666665853, 0.05413385826771626580, -0.4176697321401330321 ) ) ;
#80963 = CARTESIAN_POINT ( 'NONE',  ( 0.2099737532808405305, 0.2306618581243847221, -0.2411417322834647770 ) ) ;
#80964 = VECTOR ( 'NONE', #11034, 39.37007874015748143 ) ;
#80965 = LINE ( 'NONE', #22044, #11698 ) ;
#80966 = CARTESIAN_POINT ( 'NONE',  ( 1.351706036745407458, -0.4281496062992127816, -0.4176697321401328100 ) ) ;
#80967 = CARTESIAN_POINT ( 'NONE',  ( 0.3917322834645669549, 0.1049643490035304660, -2.479002624671915900 ) ) ;
#80968 = VERTEX_POINT ( 'NONE', #54013 ) ;
#80969 = EDGE_CURVE ( 'NONE', #29808, #41808, #54289, .T. ) ;
#80970 = VERTEX_POINT ( 'NONE', #30001 ) ;
#80971 = CARTESIAN_POINT ( 'NONE',  ( 0.6692913385826778638, -0.6692913385826771977, 8.415575281601705876E-17 ) ) ;
#80972 = CARTESIAN_POINT ( 'NONE',  ( 0.4068241469816279987, -0.3690944881889765550, -0.3153832671262227771 ) ) ;
#80974 = DIRECTION ( 'NONE',  ( 0.000000000000000000, 0.000000000000000000, 1.000000000000000000 ) ) ;
#80973 = CARTESIAN_POINT ( 'NONE',  ( 0.9548908091195654757, -4.927456884911482678E-16, 0.4445507791589062840 ) ) ;
#80975 = CARTESIAN_POINT ( 'NONE',  ( -0.1958661417322834220, -0.3392501089628018884, -0.7801837270341208663 ) ) ;
#80976 = EDGE_CURVE ( 'NONE', #36503, #41297, #61588, .T. ) ;
#80977 = FACE_OUTER_BOUND ( 'NONE', #60428, .T. ) ;
#80978 = LINE ( 'NONE', #4757, #80905 ) ;
#80979 = CARTESIAN_POINT ( 'NONE',  ( -0.1070741851644051862, -0.3996062992125986590, -2.353674540682414218 ) ) ;
#80980 = CARTESIAN_POINT ( 'NONE',  ( 0.8398950131233602345, 0.2306618581243847221, -0.2411417322834647770 ) ) ;
#80981 = CARTESIAN_POINT ( 'NONE',  ( -0.6299212598425188991, -0.1870078740157480879, -0.4822834645669291653 ) ) ;
#80982 = CARTESIAN_POINT ( 'NONE',  ( -0.7414698162729651543, 0.2952755905511810774, -0.1292274648535930714 ) ) ;
#80983 = CARTESIAN_POINT ( 'NONE',  ( 0.4790026246719167324, -0.05778040916215522460, 0.4822834645669289988 ) ) ;
#80984 = CARTESIAN_POINT ( 'NONE',  ( 1.332020997375328974, -0.05778040916215560624, -0.4822834645669293319 ) ) ;
#80985 = CARTESIAN_POINT ( 'NONE',  ( -1.024202178938476981, 1.413766264023041730, 0.4582849312594932667 ) ) ;
#80986 = APPLICATION_PROTOCOL_DEFINITION ( 'draft international standard', 'automotive_design', 1998, #56779 ) ;
#80987 = CARTESIAN_POINT ( 'NONE',  ( 1.397637795275591177, 0.07958543189024071263, -0.2665933059059888421 ) ) ;
#80988 = DIRECTION ( 'NONE',  ( 0.000000000000000000, 1.000000000000000000, 0.000000000000000000 ) ) ;
#80989 = CARTESIAN_POINT ( 'NONE',  ( -1.476377952755905110, 0.07958543189024085140, 0.2665933059059887866 ) ) ;
#80990 = DIRECTION ( 'NONE',  ( -0.8660254037844431485, 0.000000000000000000, 0.4999999999999918954 ) ) ;
#80991 = CARTESIAN_POINT ( 'NONE',  ( 0.2887139107611556010, 0.2306618581243847221, -0.2411417322834647770 ) ) ;
#80993 = CARTESIAN_POINT ( 'NONE',  ( -3.908806514029711021, 1.601083746178882938, -0.4703884258841616872 ) ) ;
#80992 = CARTESIAN_POINT ( 'NONE',  ( 1.108923884514436686, -0.3162353388693409650, -0.4822834645669289433 ) ) ;
#80994 = CARTESIAN_POINT ( 'NONE',  ( -1.332020997375327642, -0.2845877964562161244, -0.3641732283464567121 ) ) ;
#80995 = CARTESIAN_POINT ( 'NONE',  ( 0.5511811023622055217, -0.1870078740157479769, 0.4822834645669291653 ) ) ;
#80996 = CARTESIAN_POINT ( 'NONE',  ( 1.312335958005249825, 0.1283753931104746893, -0.1820866141732285504 ) ) ;
#80997 = CARTESIAN_POINT ( 'NONE',  ( 4.797336870675655290E-17, -0.3917322834645669549, -1.576096169782465140 ) ) ;
#80998 = CARTESIAN_POINT ( 'NONE',  ( -1.095800524934382292, -0.08942795157527998196, 0.3641732283464567121 ) ) ;
#80999 = CARTESIAN_POINT ( 'NONE',  ( 1.423884514435696413, -0.3162353388693409650, -0.4822834645669289433 ) ) ;
#81000 = CARTESIAN_POINT ( 'NONE',  ( 0.3127753386821575665, 1.605323575777892087, 0.01202575393854246610 ) ) ;
#81001 = CARTESIAN_POINT ( 'NONE',  ( -0.05249343832020938322, -0.5023911411419708095, -0.1820866141732282451 ) ) ;
#81002 = CARTESIAN_POINT ( 'NONE',  ( -0.03280839895013062252, -0.6692913385826771977, 0.1292274648535927661 ) ) ;
#81003 = CARTESIAN_POINT ( 'NONE',  ( -1.246719160104985846, -0.3690944881889765550, -0.3153832671262227771 ) ) ;
#81004 = CARTESIAN_POINT ( 'NONE',  ( -0.9120734908136475250, 0.2952755905511811885, 0.1292274648535926551 ) ) ;
#81005 = CARTESIAN_POINT ( 'NONE',  ( 1.377952755905512472, 0.2952755905511811885, 0.000000000000000000 ) ) ;
#81006 = CARTESIAN_POINT ( 'NONE',  ( -0.3392501089628017219, -0.1958661417322836995, -0.3641925441282957698 ) ) ;
#81007 = DIRECTION ( 'NONE',  ( 0.000000000000000000, 0.000000000000000000, -1.000000000000000000 ) ) ;
#81008 = CARTESIAN_POINT ( 'NONE',  ( 1.391076115485564868, -0.6046776061558807314, 0.2411417322834647770 ) ) ;
#81009 = CARTESIAN_POINT ( 'NONE',  ( -0.1265901696524986964, -0.4724409448818899238, -1.881233595800524849 ) ) ;
#81010 = CARTESIAN_POINT ( 'NONE',  ( -1.351706036745406347, 0.05413385826771626580, -0.4176697321401330321 ) ) ;
#81012 = EDGE_CURVE ( 'NONE', #53395, #46664, #43035, .T. ) ;
#81011 = CARTESIAN_POINT ( 'NONE',  ( -0.9908136482939626788, 0.1771653543307087630, 0.09757992244046791164 ) ) ;
#81013 = CARTESIAN_POINT ( 'NONE',  ( -0.7742782152230965886, -0.004921259842519576551, 0.3153832671262227771 ) ) ;
#81014 = LINE ( 'NONE', #75521, #46070 ) ;
#81015 = CARTESIAN_POINT ( 'NONE',  ( 0.07874015748031558404, -0.1870078740157479769, 0.4822834645669291653 ) ) ;
#81016 = CARTESIAN_POINT ( 'NONE',  ( 0.09186351706036827158, -0.004921259842519576551, 0.3153832671262227771 ) ) ;
#81017 = CARTESIAN_POINT ( 'NONE',  ( -1.253280839895012377, -0.08942795157527998196, 0.3641732283464567121 ) ) ;
#81018 = CARTESIAN_POINT ( 'NONE',  ( -1.417322834645668772, -0.1870078740157479769, 0.4822834645669291653 ) ) ;
#81019 = CARTESIAN_POINT ( 'NONE',  ( 1.515748031496063186, -0.4536011799217368745, -0.2665933059059886201 ) ) ;
#81020 = VECTOR ( 'NONE', #64814, 39.37007874015748143 ) ;
#81021 = CARTESIAN_POINT ( 'NONE',  ( 1.279527559055118724, -0.5400638737290845981, -0.3530559997133363437 ) ) ;
#81022 = CARTESIAN_POINT ( 'NONE',  ( 0.4744094488188898562, 1.528788477448867811, 2.170146923806596462 ) ) ;
#81023 = CARTESIAN_POINT ( 'NONE',  ( 0.6299212598425204535, -0.1870078740157480601, -0.3641732283464567677 ) ) ;
#81024 = CARTESIAN_POINT ( 'NONE',  ( 0.8267716535433078384, -0.6692913385826771977, 8.415575281601705876E-17 ) ) ;
#81025 = CARTESIAN_POINT ( 'NONE',  ( 0.9514435695538062676, -0.08942795157527998196, 0.3641732283464567121 ) ) ;
#81026 = VERTEX_POINT ( 'NONE', #42633 ) ;
#81027 = CARTESIAN_POINT ( 'NONE',  ( -1.102362204724408601, -0.1870078740157480879, -0.4822834645669291653 ) ) ;
#81028 = EDGE_CURVE ( 'NONE', #32917, #44550, #61454, .T. ) ;
#81029 = CARTESIAN_POINT ( 'NONE',  ( -1.043307086614172041, -0.5400638737290844871, 0.3530559997133364547 ) ) ;
#81030 = CARTESIAN_POINT ( 'NONE',  ( -0.1902887139107604098, -0.6692913385826771977, 0.1292274648535927661 ) ) ;
#81031 = CARTESIAN_POINT ( 'NONE',  ( -1.313877454013331780, 0.2755905511811023723, 0.7983292792091805090 ) ) ;
#81032 = CARTESIAN_POINT ( 'NONE',  ( 0.3996062992125984925, 0.1070741851644054637, -2.248687664041995049 ) ) ;
#81033 = CARTESIAN_POINT ( 'NONE',  ( 0.8464566929133865436, 0.1660481256975883668, -0.3530559997133364547 ) ) ;
#81034 = CARTESIAN_POINT ( 'NONE',  ( 1.332020997375328974, -0.08942795157528024563, -0.3641732283464568787 ) ) ;
#81035 = CARTESIAN_POINT ( 'NONE',  ( -0.1509186351706028884, -0.3162353388693409650, -0.4822834645669289433 ) ) ;
#81036 = CARTESIAN_POINT ( 'NONE',  ( 0.5971128608923890191, -0.6692913385826771977, 0.1292274648535927661 ) ) ;
#81037 = CARTESIAN_POINT ( 'NONE',  ( -0.1070741851644056997, 0.3996062992125986035, -1.581364829396325389 ) ) ;
#81038 = CARTESIAN_POINT ( 'NONE',  ( 0.3420746716998660508, -0.1974969037888703871, -0.8923884514435694859 ) ) ;
#81039 = CARTESIAN_POINT ( 'NONE',  ( -0.3460692066303958092, -0.1998031496062994683, -2.572178477690288734 ) ) ;
#81040 = DIRECTION ( 'NONE',  ( 0.000000000000000000, 0.000000000000000000, 1.000000000000000000 ) ) ;
#81041 = CARTESIAN_POINT ( 'NONE',  ( 0.3392501089628018329, 0.1958661417322835607, -0.7532808398950130435 ) ) ;
#81042 = CARTESIAN_POINT ( 'NONE',  ( -0.02624671916010428221, -0.5023911411419708095, 0.1820866141732285504 ) ) ;
#81043 = CARTESIAN_POINT ( 'NONE',  ( -0.8530183727034112984, -0.4281496062992127816, -0.4176697321401328100 ) ) ;
#81044 = CARTESIAN_POINT ( 'NONE',  ( 0.8530183727034126306, 0.05413385826771626580, -0.4176697321401330321 ) ) ;
#81045 = CARTESIAN_POINT ( 'NONE',  ( 0.1974969037888706092, -0.3420746716998660508, -2.058398950131233640 ) ) ;
#81046 = CARTESIAN_POINT ( 'NONE',  ( -0.3543307086614165824, 0.1771653543307087630, 0.000000000000000000 ) ) ;
#81047 = CARTESIAN_POINT ( 'NONE',  ( 1.555118110236221041, -0.5400638737290844871, 0.3530559997133364547 ) ) ;
#81048 = CARTESIAN_POINT ( 'NONE',  ( 1.003937007874016185, 0.1660481256975883668, -0.3530559997133364547 ) ) ;
#81049 = CARTESIAN_POINT ( 'NONE',  ( -0.1265901696524993347, 0.4724409448818895907, -2.368766404199475151 ) ) ;
#81050 = CARTESIAN_POINT ( 'NONE',  ( 4.893765752498283924E-17, -0.3996062992125986035, -1.811023622047244208 ) ) ;
#81051 = CARTESIAN_POINT ( 'NONE',  ( 0.8923884514435701520, -0.6046776061558809534, -0.2411417322834644161 ) ) ;
#81052 = CARTESIAN_POINT ( 'NONE',  ( 1.161417322834646271, 0.07958543189024071263, -0.2665933059059888421 ) ) ;
#81054 = CARTESIAN_POINT ( 'NONE',  ( -1.601049868766403650, 0.2306618581243847221, -0.2411417322834647770 ) ) ;
#81053 = CARTESIAN_POINT ( 'NONE',  ( 1.614173228346457378, -0.6692913385826771977, 8.415575281601705876E-17 ) ) ;
#81055 = CARTESIAN_POINT ( 'NONE',  ( -0.3917322834645668994, -0.1049643490035306742, -2.645649975556744415 ) ) ;
#81056 = CARTESIAN_POINT ( 'NONE',  ( 0.3149606299212736604, 2.559055118110236560, -3.937007874015761022 ) ) ;
#81057 = CARTESIAN_POINT ( 'NONE',  ( 0.7480314960629927956, 0.2952755905511811885, 0.000000000000000000 ) ) ;
#81058 = CARTESIAN_POINT ( 'NONE',  ( -1.541994750656167090, 0.2952755905511811885, 0.1292274648535926551 ) ) ;
#81059 = CARTESIAN_POINT ( 'NONE',  ( -0.4002624671916004129, -0.05778040916215560624, -0.4822834645669293319 ) ) ;
#81060 = CARTESIAN_POINT ( 'NONE',  ( -0.5314960629921254842, -0.5400638737290845981, -0.3530559997133363437 ) ) ;
#81061 = CARTESIAN_POINT ( 'NONE',  ( 1.607611548556431069, 0.2952755905511811885, 0.1292274648535926551 ) ) ;
#81062 = CARTESIAN_POINT ( 'NONE',  ( 0.3917322834645670104, 2.398668435337828261E-17, -0.04527559055118119541 ) ) ;
#81063 = CARTESIAN_POINT ( 'NONE',  ( 0.05905511811023681640, 0.1660481256975883668, -0.3530559997133364547 ) ) ;
#81064 = CARTESIAN_POINT ( 'NONE',  ( 0.3392501089628018329, 0.1958661417322835607, -2.328083989501312345 ) ) ;
#81065 = CARTESIAN_POINT ( 'NONE',  ( 1.679790026246720025, 0.2306618581243848609, 0.2411417322834645549 ) ) ;
#81066 = VERTEX_POINT ( 'NONE', #37968 ) ;
#81067 = CARTESIAN_POINT ( 'NONE',  ( -0.3420746716998661618, 0.1974969037888702206, -2.545931758530183497 ) ) ;
#81068 = ORIENTED_EDGE ( 'NONE', *, *, #29439, .F. ) ;
#81069 = CARTESIAN_POINT ( 'NONE',  ( -1.109025475590603493, 2.631261499653055225, -0.2618487365674062595 ) ) ;
#81070 = CARTESIAN_POINT ( 'NONE',  ( -1.509186351706035767, 0.05413385826771626580, -0.4176697321401330321 ) ) ;
#81071 = CARTESIAN_POINT ( 'NONE',  ( 0.3996062992125986035, 2.446882876249141962E-17, -1.062992125984252079 ) ) ;
#81072 = CARTESIAN_POINT ( 'NONE',  ( 1.587926509186352586, -0.3690944881889765550, -0.3153832671262227771 ) ) ;
#81073 = CARTESIAN_POINT ( 'NONE',  ( 0.1265901696524990572, -0.4724409448818897017, -0.7919947506561678674 ) ) ;
#81074 = DIRECTION ( 'NONE',  ( -3.491481338843132961E-15, -0.000000000000000000, 1.000000000000000000 ) ) ;
#81075 = DIRECTION ( 'NONE',  ( 0.000000000000000000, -1.000000000000000000, 0.000000000000000000 ) ) ;
#81076 = CARTESIAN_POINT ( 'NONE',  ( 0.1049643490035303689, 0.3917322834645670104, -0.2355643044619422921 ) ) ;
#81077 = VECTOR ( 'NONE', #27801, 39.37007874015748854 ) ;
#81078 = CARTESIAN_POINT ( 'NONE',  ( -0.3412073490813641308, 0.1283753931104746893, -0.1820866141732285504 ) ) ;
#81079 = CARTESIAN_POINT ( 'NONE',  ( -1.082677165354329896, 0.07958543189024085140, 0.2665933059059887866 ) ) ;
#81080 = CARTESIAN_POINT ( 'NONE',  ( 1.535433070866142335, -0.6692913385826771977, 8.415575281601705876E-17 ) ) ;
#81081 = CARTESIAN_POINT ( 'NONE',  ( 0.4790026246719167324, -0.05778040916215522460, 0.4822834645669289988 ) ) ;
#81082 = CARTESIAN_POINT ( 'NONE',  ( -1.528871391076114250, -0.6692913385826771977, 0.1292274648535927661 ) ) ;
#81083 = CARTESIAN_POINT ( 'NONE',  ( -0.1958661417322836718, 0.3392501089628017219, -0.1627296587926508609 ) ) ;
#81084 = EDGE_LOOP ( 'NONE', ( #51213, #25101, #30621, #30008, #48316 ) ) ;
#81085 = CARTESIAN_POINT ( 'NONE',  ( 1.561679790026247350, -0.4281496062992124485, 0.4176697321401328655 ) ) ;
#81086 = PLANE ( 'NONE',  #64893 ) ;
#81087 = CARTESIAN_POINT ( 'NONE',  ( 0.1265901696524990294, -0.4724409448818896462, -1.660104986876640210 ) ) ;
#81088 = CARTESIAN_POINT ( 'NONE',  ( 2.372150492836604986E-17, 0.5905511811023621549, 0.1937007874015747588 ) ) ;
#81089 = CARTESIAN_POINT ( 'NONE',  ( 0.3392501089628018884, -0.1958661417322834220, -2.709317585301837195 ) ) ;
#81090 = CARTESIAN_POINT ( 'NONE',  ( -0.9383202099737524282, -0.3162353388693409650, -0.4822834645669289433 ) ) ;
#81091 = CARTESIAN_POINT ( 'NONE',  ( 1.646981627296588035, -0.3162353388693405765, 0.4822834645669290543 ) ) ;
#81092 = CARTESIAN_POINT ( 'NONE',  ( 0.5314960629921061663, 2.755905511811024056, 1.895394334970797345 ) ) ;
#81093 = EDGE_CURVE ( 'NONE', #23282, #52953, #8244, .T. ) ;
#81094 = CARTESIAN_POINT ( 'NONE',  ( 1.653543307086614789, -0.1870078740157479769, 0.4822834645669291653 ) ) ;
#81095 = CARTESIAN_POINT ( 'NONE',  ( -0.6889763779527552368, -0.5400638737290845981, -0.3530559997133363437 ) ) ;
#81096 = CARTESIAN_POINT ( 'NONE',  ( 0.3917322834645668994, 0.1049643490035304522, -0.2047050936669798094 ) ) ;
#81097 = CARTESIAN_POINT ( 'NONE',  ( 0.08530183727034192087, -0.2845877964562161244, -0.3641732283464567121 ) ) ;
#81098 = CARTESIAN_POINT ( 'NONE',  ( 0.3917322834645670104, 2.398668435337828261E-17, -0.5177165354330709457 ) ) ;
#81099 = EDGE_CURVE ( 'NONE', #26979, #45807, #39579, .T. ) ;
#81100 = CARTESIAN_POINT ( 'NONE',  ( -0.04593175853018302557, 0.1771653543307087630, 0.09757992244046791164 ) ) ;
#81101 = CARTESIAN_POINT ( 'NONE',  ( 0.7217847769028878924, -0.3690944881889765550, -0.3153832671262227771 ) ) ;
#81102 = CARTESIAN_POINT ( 'NONE',  ( 0.6561679790026253567, 0.2306618581243848609, 0.2411417322834645549 ) ) ;
#81103 = CARTESIAN_POINT ( 'NONE',  ( -0.3608923884514428360, 0.1771653543307087630, 0.09757992244046791164 ) ) ;
#81104 = CARTESIAN_POINT ( 'NONE',  ( -0.3392501089628017219, -0.1958661417322836718, -2.406824146981627166 ) ) ;
#81105 = CARTESIAN_POINT ( 'NONE',  ( 1.568241469816273437, -0.3162353388693405765, 0.4822834645669290543 ) ) ;
#81106 = B_SPLINE_CURVE_WITH_KNOTS ( 'NONE', 3,
 ( #22820, #75008, #17355, #48895 ),
 .UNSPECIFIED., .F., .F.,
 ( 4, 4 ),
 ( 1.999999999927407068E-07, 0.006970199999999936863 ),
 .UNSPECIFIED. ) ;
#81107 = CARTESIAN_POINT ( 'NONE',  ( -1.187664041994749731, -0.3162353388693405765, 0.4822834645669290543 ) ) ;
#81108 = CARTESIAN_POINT ( 'NONE',  ( 0.2362204724409449064, 0.4091458600556404646, -0.6935695538057742304 ) ) ;
#81109 = CARTESIAN_POINT ( 'NONE',  ( 0.2362204724409456558, -0.1870078740157480879, -0.4822834645669291653 ) ) ;
#81110 = CARTESIAN_POINT ( 'NONE',  ( -0.5118110236220466680, 0.2952755905511811885, 0.000000000000000000 ) ) ;
#81111 = FACE_OUTER_BOUND ( 'NONE', #14207, .T. ) ;
#81112 = CARTESIAN_POINT ( 'NONE',  ( -0.05249343832020938322, -0.5023911411419708095, -0.1820866141732282451 ) ) ;
#81113 = CARTESIAN_POINT ( 'NONE',  ( -0.03937007874015669567, -0.6692913385826771977, 8.415575281601705876E-17 ) ) ;
#81114 = CARTESIAN_POINT ( 'NONE',  ( -0.7020997375328074108, -0.05778040916215522460, 0.4822834645669289988 ) ) ;
#81115 = DIRECTION ( 'NONE',  ( 0.000000000000000000, 0.000000000000000000, 1.000000000000000000 ) ) ;
#81116 = CARTESIAN_POINT ( 'NONE',  ( 1.640419947506562393, -0.3690944881889763329, 0.3153832671262228327 ) ) ;
#81117 = AXIS2_PLACEMENT_3D ( 'NONE', #22202, #16317, #65997 ) ;
#81118 = CARTESIAN_POINT ( 'NONE',  ( 0.1574803149606306130, -0.1870078740157480879, -0.4822834645669291653 ) ) ;
#81119 = ORIENTED_EDGE ( 'NONE', *, *, #20687, .F. ) ;
#81120 = CARTESIAN_POINT ( 'NONE',  ( 0.3460692066303959202, -0.1998031496062991630, -1.914041994750656395 ) ) ;
#81121 = CARTESIAN_POINT ( 'NONE',  ( 1.161417322834646271, 0.1660481256975883668, -0.3530559997133364547 ) ) ;
#81122 = CARTESIAN_POINT ( 'NONE',  ( -0.8267716535433065062, -0.5511811023622047445, 6.969142054262312111E-17 ) ) ;
#81123 = CARTESIAN_POINT ( 'NONE',  ( -0.5643044619422565855, 0.05413385826771626580, -0.4176697321401330321 ) ) ;
#81124 = CARTESIAN_POINT ( 'NONE',  ( 1.213910761154856299, 0.2952755905511811885, 0.1292274648535926551 ) ) ;
#81125 = CARTESIAN_POINT ( 'NONE',  ( 1.246719160104987623, 0.05413385826771626580, -0.4176697321401330321 ) ) ;
#81126 = CARTESIAN_POINT ( 'NONE',  ( -1.633858267716534529, 0.1660481256975885056, 0.3530559997133364547 ) ) ;
#81127 = CARTESIAN_POINT ( 'NONE',  ( -1.154855643044618851, -0.5023911411419708095, -0.1820866141732282451 ) ) ;
#81128 = CARTESIAN_POINT ( 'NONE',  ( 0.2925321140481931814, -0.2925321140481931259, -0.1751968503937008370 ) ) ;
#81129 = CARTESIAN_POINT ( 'NONE',  ( 0.3460692066303959757, -0.1998031496062991907, -0.5774278215223097588 ) ) ;
#81130 = AXIS2_PLACEMENT_3D ( 'NONE', #402, #39104, #44161 ) ;
#81131 = CARTESIAN_POINT ( 'NONE',  ( 0.3392501089628018329, 0.1958661417322835607, -2.805137426018059710 ) ) ;
#81132 = CARTESIAN_POINT ( 'NONE',  ( 1.633858267716535639, -0.4536011799217367080, 0.2665933059059888421 ) ) ;
#81133 = CARTESIAN_POINT ( 'NONE',  ( 1.049868766404200127, -0.5023911411419708095, -0.1820866141732282451 ) ) ;
#81134 = CARTESIAN_POINT ( 'NONE',  ( 0.3871391076115492380, -0.05778040916215560624, -0.4822834645669293319 ) ) ;
#81135 = CARTESIAN_POINT ( 'NONE',  ( -1.732283464566928277, -0.1870078740157479769, 0.4822834645669291653 ) ) ;
#81136 = CARTESIAN_POINT ( 'NONE',  ( 0.3949938075777409963, 2.418639510665530743E-17, -0.8248031496062994128 ) ) ;
#81137 = CARTESIAN_POINT ( 'NONE',  ( 0.6036745406824154392, 0.1283753931104746893, -0.1820866141732285504 ) ) ;
#81138 =( BOUNDED_CURVE ( )  B_SPLINE_CURVE ( 1, ( #71912, #27279 ),
 .UNSPECIFIED., .F., .F. ) 
 B_SPLINE_CURVE_WITH_KNOTS ( ( 2, 2 ),
 ( 3.469446951953614189E-18, 0.001999999999999994837 ),
 .UNSPECIFIED. ) 
 CURVE ( )  GEOMETRIC_REPRESENTATION_ITEM ( )  RATIONAL_B_SPLINE_CURVE ( ( 0.9875488213027523443, 0.9875488213027523443 ) ) 
 REPRESENTATION_ITEM ( '' )  );
#81139 = CARTESIAN_POINT ( 'NONE',  ( -0.3674540682414689785, 0.2306618581243848609, 0.2411417322834645549 ) ) ;
#81140 = CARTESIAN_POINT ( 'NONE',  ( -0.8136482939632537770, 0.2306618581243847221, -0.2411417322834647770 ) ) ;
#81141 = CARTESIAN_POINT ( 'NONE',  ( 1.456692913385827515, -0.6692913385826771977, 8.415575281601705876E-17 ) ) ;
#81142 = CARTESIAN_POINT ( 'NONE',  ( -0.1265901696524993347, 0.4724409448818895907, -1.266404199475065440 ) ) ;
#81143 = CARTESIAN_POINT ( 'NONE',  ( -0.1998031496062991907, -0.3460692066303959757, -2.270341207349081181 ) ) ;
#81144 = CARTESIAN_POINT ( 'NONE',  ( -0.03937007874015669567, -0.5511811023622047445, 6.969142054262312111E-17 ) ) ;
#81145 = ORIENTED_EDGE ( 'NONE', *, *, #49585, .F. ) ;
#81146 = CARTESIAN_POINT ( 'NONE',  ( 0.2867679344610366554, 0.2867679344610366554, -0.7644550113198971264 ) ) ;
#81147 = ORIENTED_EDGE ( 'NONE', *, *, #35131, .F. ) ;
#81148 = CARTESIAN_POINT ( 'NONE',  ( -0.9711286089238838626, -0.6046776061558807314, 0.2411417322834647770 ) ) ;
#81149 = CARTESIAN_POINT ( 'NONE',  ( -0.02624671916010428221, 0.2306618581243847221, -0.2411417322834647770 ) ) ;
#81150 = CARTESIAN_POINT ( 'NONE',  ( -0.5183727034120726440, 0.2952755905511811885, 0.1292274648535926551 ) ) ;
#81151 = CARTESIAN_POINT ( 'NONE',  ( 0.9645669291338591078, -0.5400638737290845981, -0.3530559997133363437 ) ) ;
#81152 = CARTESIAN_POINT ( 'NONE',  ( -0.2362204724409440182, -0.1870078740157479769, 0.4822834645669291653 ) ) ;
#81153 = CARTESIAN_POINT ( 'NONE',  ( -1.200787401574802349, -0.5400638737290844871, 0.3530559997133364547 ) ) ;
#81154 = CARTESIAN_POINT ( 'NONE',  ( -0.4330708661417315697, 0.2952755905511811885, 0.000000000000000000 ) ) ;
#81155 = CARTESIAN_POINT ( 'NONE',  ( 0.7086614173228352742, -0.1870078740157480879, -0.4822834645669291653 ) ) ;
#81156 = CARTESIAN_POINT ( 'NONE',  ( 0.3740157480314966754, 0.1660481256975883668, -0.3530559997133364547 ) ) ;
#81157 = CARTESIAN_POINT ( 'NONE',  ( 0.1049643490035304938, -0.3917322834645669549, -1.179790026246718915 ) ) ;
#81158 = CARTESIAN_POINT ( 'NONE',  ( -0.3805774278215216522, -0.004921259842519576551, 0.3153832671262227771 ) ) ;
#81159 = ORIENTED_EDGE ( 'NONE', *, *, #37239, .T. ) ;
#81160 = CARTESIAN_POINT ( 'NONE',  ( 0.3949938075777409408, 0.1058382717557500574, -1.541994750656168200 ) ) ;
#81161 = ORIENTED_EDGE ( 'NONE', *, *, #53636, .T. ) ;
#81162 = CARTESIAN_POINT ( 'NONE',  ( -1.358267716535432434, 0.07958543189024071263, -0.2665933059059888421 ) ) ;
#81163 = CARTESIAN_POINT ( 'NONE',  ( -0.4068241469816264999, -0.4281496062992124485, 0.4176697321401328655 ) ) ;
#81164 = CARTESIAN_POINT ( 'NONE',  ( 4.893765752498283924E-17, -0.3996062992125986035, 0.07874015748031494566 ) ) ;
#81165 = CARTESIAN_POINT ( 'NONE',  ( -0.5183727034120726440, -0.6692913385826773087, -0.1292274648535924053 ) ) ;
#81166 = CARTESIAN_POINT ( 'NONE',  ( -0.8858267716535425107, 0.1660481256975883668, -0.3530559997133364547 ) ) ;
#81167 = CARTESIAN_POINT ( 'NONE',  ( -1.417322834645668772, -0.1870078740157480879, -0.4822834645669291653 ) ) ;
#81168 = DIRECTION ( 'NONE',  ( -1.000000000000000000, -0.000000000000000000, -0.000000000000000000 ) ) ;
#81169 = CARTESIAN_POINT ( 'NONE',  ( 1.082677165354331228, 0.07958543189024071263, -0.2665933059059888421 ) ) ;
#81170 = CARTESIAN_POINT ( 'NONE',  ( 0.4724409448818897017, 0.1265901696524990294, -0.3589238845144357426 ) ) ;
#81171 = CARTESIAN_POINT ( 'NONE',  ( -0.3917322834645670104, -7.196005306013484475E-17, -0.1240157480314961758 ) ) ;
#81172 = CARTESIAN_POINT ( 'NONE',  ( 0.1509186351706042484, -0.2845877964562159024, 0.3641732283464567677 ) ) ;
#81173 = VECTOR ( 'NONE', #55506, 39.37007874015748143 ) ;
#81174 = CARTESIAN_POINT ( 'NONE',  ( -0.2690288713910754526, -0.6692913385826771977, 0.1292274648535927661 ) ) ;
#81175 = CARTESIAN_POINT ( 'NONE',  ( 0.05905511811023709395, -0.5400638737290844871, 0.3530559997133364547 ) ) ;
#81176 = ORIENTED_EDGE ( 'NONE', *, *, #59446, .T. ) ;
#81177 = CARTESIAN_POINT ( 'NONE',  ( 0.1998031496062992740, 0.3460692066303959757, -2.191601049868766360 ) ) ;
#81178 = CARTESIAN_POINT ( 'NONE',  ( -0.5314960629921170465, 2.729656594508716783, -2.556891439663424581 ) ) ;
#81179 = ORIENTED_EDGE ( 'NONE', *, *, #71143, .T. ) ;
#81180 = CARTESIAN_POINT ( 'NONE',  ( -0.3460692066303957537, -0.1998031496062994405, -1.546587926509186639 ) ) ;
#81181 = DIRECTION ( 'NONE',  ( -0.000000000000000000, -1.000000000000000000, -0.000000000000000000 ) ) ;
#81182 = CARTESIAN_POINT ( 'NONE',  ( -0.6955380577427815458, -0.3690944881889765550, -0.3153832671262227771 ) ) ;
#81183 = CARTESIAN_POINT ( 'NONE',  ( -0.8136482939632537770, -0.6046776061558807314, 0.2411417322834647770 ) ) ;
#81184 = CARTESIAN_POINT ( 'NONE',  ( 0.3458507752293908943, -0.3458507752293908943, -0.5708661417322833387 ) ) ;
#81185 = FACE_OUTER_BOUND ( 'NONE', #19206, .T. ) ;
#81186 = CARTESIAN_POINT ( 'NONE',  ( 0.3917322834645670104, 2.398668435337828261E-17, -2.407480314960630086 ) ) ;
#81187 = CARTESIAN_POINT ( 'NONE',  ( 1.305774278215223960, -0.6692913385826771977, 0.1292274648535927661 ) ) ;
#81188 = CARTESIAN_POINT ( 'NONE',  ( 0.4855643044619428750, 0.05413385826771666132, 0.4176697321401328100 ) ) ;
#81189 = CARTESIAN_POINT ( 'NONE',  ( 0.4133858267716541968, 0.1660481256975885056, 0.3530559997133364547 ) ) ;
#81190 = CARTESIAN_POINT ( 'NONE',  ( -0.8464566929133852113, 0.07958543189024085140, 0.2665933059059887866 ) ) ;
#81191 = CARTESIAN_POINT ( 'NONE',  ( -0.4593175853018366950, 0.05413385826771666132, 0.4176697321401328100 ) ) ;
#81192 = CARTESIAN_POINT ( 'NONE',  ( -0.2362204724409447953, -0.4091458600556404646, -2.504593175853018661 ) ) ;
#81193 = CARTESIAN_POINT ( 'NONE',  ( -0.3215223097112853146, -0.3162353388693405765, 0.4822834645669290543 ) ) ;
#81194 = EDGE_CURVE ( 'NONE', #24806, #34044, #37558, .T. ) ;
#81195 = AXIS2_PLACEMENT_3D ( 'NONE', #55887, #4145, #36132 ) ;
#81196 = CARTESIAN_POINT ( 'NONE',  ( 0.3420746716998660508, 0.1974969037888705814, -1.625328083989501460 ) ) ;
#81197 = CARTESIAN_POINT ( 'NONE',  ( 1.167979002624672580, -0.004921259842519870586, -0.3153832671262229437 ) ) ;
#81198 = CARTESIAN_POINT ( 'NONE',  ( -0.1837270341207343505, -0.5023911411419708095, 0.1820866141732285504 ) ) ;
#81199 = CARTESIAN_POINT ( 'NONE',  ( 1.272965879265092637, -0.3690944881889765550, -0.3153832671262227771 ) ) ;
#81200 = CARTESIAN_POINT ( 'NONE',  ( -1.351706036745406347, 0.05413385826771626580, -0.4176697321401330321 ) ) ;
#81201 = CARTESIAN_POINT ( 'NONE',  ( -1.030183727034119867, -0.2845877964562159024, 0.3641732283464567677 ) ) ;
#81202 = LINE ( 'NONE', #37394, #70864 ) ;
#81203 = CARTESIAN_POINT ( 'NONE',  ( -0.9973753280839886548, -0.6046776061558809534, -0.2411417322834644161 ) ) ;
#81204 = CARTESIAN_POINT ( 'NONE',  ( -0.3346456692913377662, 0.1660481256975883668, -0.3530559997133364547 ) ) ;
#81205 = CARTESIAN_POINT ( 'NONE',  ( 0.3018372703412079971, 0.05413385826771626580, -0.4176697321401330321 ) ) ;
#81206 = CARTESIAN_POINT ( 'NONE',  ( -2.104898677616466429, 1.365902157108392245, 0.4425616331406720394 ) ) ;
#81207 = CARTESIAN_POINT ( 'NONE',  ( 0.1509186351706045259, -0.08942795157528024563, -0.3641732283464568787 ) ) ;
#81208 = CARTESIAN_POINT ( 'NONE',  ( -1.653543307086613234, -0.1870078740157480601, -0.3641732283464567677 ) ) ;
#81209 = CARTESIAN_POINT ( 'NONE',  ( 0.8398950131233602345, -0.6046776061558807314, 0.2411417322834647770 ) ) ;
#81210 = CARTESIAN_POINT ( 'NONE',  ( -1.561679790026246017, -0.004921259842519576551, 0.3153832671262227771 ) ) ;
#81211 = CARTESIAN_POINT ( 'NONE',  ( 1.286089238845145033, 0.1283753931104748280, 0.1820866141732283561 ) ) ;
#81212 = CARTESIAN_POINT ( 'NONE',  ( -1.062992125984250968, 0.2952755905511811885, 0.000000000000000000 ) ) ;
#81213 = CARTESIAN_POINT ( 'NONE',  ( -0.2362204724409440182, -0.1870078740157479769, 0.3641732283464567677 ) ) ;
#81214 = CARTESIAN_POINT ( 'NONE',  ( 0.000000000000000000, 0.4374015748031496176, -1.178877988035069047 ) ) ;
#81215 = CARTESIAN_POINT ( 'NONE',  ( 0.05249343832021075018, 0.1283753931104746893, -0.1820866141732285504 ) ) ;
#81216 = CARTESIAN_POINT ( 'NONE',  ( -0.03280839895013062252, 0.2952755905511810774, -0.1292274648535930714 ) ) ;
#81217 = CARTESIAN_POINT ( 'NONE',  ( 0.1070741851644053388, 0.3996062992125986035, -0.5426509186351704539 ) ) ;
#81218 = CARTESIAN_POINT ( 'NONE',  ( 0.3917322834645670104, 2.398668435337828261E-17, -1.935039370078740273 ) ) ;
#81219 = CARTESIAN_POINT ( 'NONE',  ( 0.6627296587926515548, 0.1771653543307087630, 0.09757992244046791164 ) ) ;
#81220 = CARTESIAN_POINT ( 'NONE',  ( 0.1246719160104994284, 0.2952755905511810774, -0.1292274648535930714 ) ) ;
#81221 = CARTESIAN_POINT ( 'NONE',  ( -0.5643044619422565855, -0.4281496062992124485, 0.4176697321401328655 ) ) ;
#81222 = CARTESIAN_POINT ( 'NONE',  ( -0.6561679790026240244, 0.1283753931104746893, -0.1820866141732285504 ) ) ;
#81223 = CYLINDRICAL_SURFACE ( 'NONE', #22569, 0.3149606299212598381 ) ;
#81224 = CARTESIAN_POINT ( 'NONE',  ( -0.5183727034120726440, 0.1771653543307087630, 0.09757992244046791164 ) ) ;
#81225 = CARTESIAN_POINT ( 'NONE',  ( 0.07217847769028949700, -0.3162353388693405765, 0.4822834645669290543 ) ) ;
#81226 = CARTESIAN_POINT ( 'NONE',  ( -1.213910761154854745, 0.1771653543307087075, -0.09757992244046823083 ) ) ;
#81227 = CARTESIAN_POINT ( 'NONE',  ( -0.3996062992125984925, -0.1070741851644056858, -1.540026246719160108 ) ) ;
#81228 = CARTESIAN_POINT ( 'NONE',  ( 1.509186351706037543, -0.4281496062992127816, -0.4176697321401328100 ) ) ;
#81229 = CARTESIAN_POINT ( 'NONE',  ( 0.4605079024601035909, 2.141871057760741033E-18, -0.3627985898453511826 ) ) ;
#81230 = EDGE_LOOP ( 'NONE', ( #10128, #19877, #60839, #38389 ) ) ;
#81231 = CIRCLE ( 'NONE', #58303, 3.937007874015748143 ) ;
#81232 = CARTESIAN_POINT ( 'NONE',  ( -1.594488188976377563, -0.4536011799217367080, 0.2665933059059888421 ) ) ;
#81233 = CARTESIAN_POINT ( 'NONE',  ( -0.3018372703412066094, 0.05413385826771666132, 0.4176697321401328100 ) ) ;
#81234 = CARTESIAN_POINT ( 'NONE',  ( -0.9908136482939626788, 0.2952755905511811885, 0.1292274648535926551 ) ) ;
#81235 = CARTESIAN_POINT ( 'NONE',  ( 0.3917322834645670104, -0.1049643490035303411, -1.770997375328083656 ) ) ;
#81236 = CYLINDRICAL_SURFACE ( 'NONE', #22988, 2.362204724409449508 ) ;
#81237 = CARTESIAN_POINT ( 'NONE',  ( 1.391076115485564868, 0.2306618581243847221, -0.2411417322834647770 ) ) ;
#81238 = CARTESIAN_POINT ( 'NONE',  ( 0.2427821522309719648, -0.05778040916215522460, 0.4822834645669289988 ) ) ;
#81239 = DIRECTION ( 'NONE',  ( 9.381338752702732014E-17, -0.6427876096865392519, 0.7660444431189781245 ) ) ;
#81240 = CARTESIAN_POINT ( 'NONE',  ( -0.1998031496062991630, -0.3460692066303959202, -2.347112860892388575 ) ) ;
#81241 = CARTESIAN_POINT ( 'NONE',  ( 1.509186351706037543, -0.3690944881889765550, -0.3153832671262227771 ) ) ;
#81242 = CARTESIAN_POINT ( 'NONE',  ( -0.3996062992125986035, -7.340648628747425578E-17, -0.9842519685039369248 ) ) ;
#81243 = ORIENTED_EDGE ( 'NONE', *, *, #2315, .F. ) ;
#81244 = CARTESIAN_POINT ( 'NONE',  ( -1.036745406824146176, -0.3690944881889763329, 0.3153832671262228327 ) ) ;
#81246 = CARTESIAN_POINT ( 'NONE',  ( 0.3917322834645669549, 0.1049643490035304660, -2.636482939632545985 ) ) ;
#81245 = AXIS2_PLACEMENT_3D ( 'NONE', #73383, #34668, #60331 ) ;
#81247 = VERTEX_POINT ( 'NONE', #44674 ) ;
#81248 = CARTESIAN_POINT ( 'NONE',  ( 0.3083989501312343062, -0.3162353388693405765, 0.4822834645669290543 ) ) ;
#81249 = CARTESIAN_POINT ( 'NONE',  ( -0.5643044619422565855, 0.05413385826771626580, -0.4176697321401330321 ) ) ;
#81250 = CARTESIAN_POINT ( 'NONE',  ( -1.010498687664041384, 0.05413385826771666132, 0.4176697321401328100 ) ) ;
#81251 = CARTESIAN_POINT ( 'NONE',  ( 1.272965879265092637, -0.4281496062992127816, -0.4176697321401328100 ) ) ;
#81252 = CARTESIAN_POINT ( 'NONE',  ( -1.410761154855641575, -0.2845877964562161244, -0.3641732283464567121 ) ) ;
#81253 = CARTESIAN_POINT ( 'NONE',  ( -0.8761506516392493227, -2.567464376874931580E-15, -0.4445507791589072832 ) ) ;
#81254 = CARTESIAN_POINT ( 'NONE',  ( 0.05249343832021075018, -0.6046776061558807314, 0.2411417322834647770 ) ) ;
#81255 = CARTESIAN_POINT ( 'NONE',  ( -1.246719160104985846, -0.4281496062992127816, -0.4176697321401328100 ) ) ;
#81256 = CARTESIAN_POINT ( 'NONE',  ( -0.1958661417322834497, -0.3392501089628018884, -2.192894070044932420 ) ) ;
#81257 = CARTESIAN_POINT ( 'NONE',  ( 0.4177787735907000366, 0.000000000000000000, -1.559171609364239375 ) ) ;
#81258 = DIRECTION ( 'NONE',  ( -0.000000000000000000, 1.000000000000000000, -0.000000000000000000 ) ) ;
#81259 = CARTESIAN_POINT ( 'NONE',  ( -0.2867679344610364334, -0.2867679344610367109, -2.663385826771653253 ) ) ;
#81260 = CARTESIAN_POINT ( 'NONE',  ( 1.003937007874016407, -0.4536011799217367080, 0.2665933059059888421 ) ) ;
#81261 = ORIENTED_EDGE ( 'NONE', *, *, #22702, .T. ) ;
#81262 = CARTESIAN_POINT ( 'NONE',  ( 0.1058382717557500713, -0.3949938075777409408, -0.08530183727034125474 ) ) ;
#81263 = CARTESIAN_POINT ( 'NONE',  ( -0.9776902887139098386, 0.2952755905511810774, -0.1292274648535930714 ) ) ;
#81264 = ORIENTED_EDGE ( 'NONE', *, *, #67683, .F. ) ;
#81265 = CARTESIAN_POINT ( 'NONE',  ( 0.5905511811023629321, -0.5511811023622047445, 6.969142054262312111E-17 ) ) ;
#81266 = CARTESIAN_POINT ( 'NONE',  ( -1.719160104986876103, 0.05413385826771666132, 0.4176697321401328100 ) ) ;
#81267 = CARTESIAN_POINT ( 'NONE',  ( 0.7283464566929140904, -0.5400638737290845981, -0.3530559997133363437 ) ) ;
#81268 = CARTESIAN_POINT ( 'NONE',  ( 0.3871391076115492380, -0.05778040916215560624, -0.4822834645669293319 ) ) ;
#81269 = CARTESIAN_POINT ( 'NONE',  ( -0.2230971128608915943, -0.4281496062992127816, -0.4176697321401328100 ) ) ;
#81270 = CARTESIAN_POINT ( 'NONE',  ( -0.3392501089628017219, -0.1958661417322836995, -1.466554748852705092 ) ) ;
#81271 = CARTESIAN_POINT ( 'NONE',  ( -0.6167979002624665030, -0.4281496062992127816, -0.4176697321401328100 ) ) ;
#81272 = CARTESIAN_POINT ( 'NONE',  ( -0.2867679344610364334, -0.2867679344610367109, -2.033464566929133355 ) ) ;
#81273 = CARTESIAN_POINT ( 'NONE',  ( 1.410761154855643795, -0.2845877964562159024, 0.3641732283464567677 ) ) ;
#81274 = CARTESIAN_POINT ( 'NONE',  ( -1.187664041994749731, -0.3162353388693405765, 0.4822834645669290543 ) ) ;
#81275 = CARTESIAN_POINT ( 'NONE',  ( 1.181102362204725198, -0.1870078740157479769, 0.4822834645669291653 ) ) ;
#81276 = CARTESIAN_POINT ( 'NONE',  ( 1.266404199475066328, -0.3162353388693409650, -0.4822834645669289433 ) ) ;
#81277 = CARTESIAN_POINT ( 'NONE',  ( 0.2925321140481932369, -0.2925321140481932369, -0.4133858267716534196 ) ) ;
#81278 = CARTESIAN_POINT ( 'NONE',  ( -0.9317585301837263412, 0.05413385826771666132, 0.4176697321401328100 ) ) ;
#81279 = CARTESIAN_POINT ( 'NONE',  ( -0.1998031496062994405, 0.3460692066303957537, -0.2473753280839895152 ) ) ;
#81280 = CARTESIAN_POINT ( 'NONE',  ( 0.2230971128608929543, 0.05413385826771626580, -0.4176697321401330321 ) ) ;
#81281 = CARTESIAN_POINT ( 'NONE',  ( 0.1998031496062992740, 0.3460692066303959757, -2.349081364829396446 ) ) ;
#81282 = EDGE_CURVE ( 'NONE', #65725, #60134, #61548, .T. ) ;
#81283 = B_SPLINE_CURVE_WITH_KNOTS ( 'NONE', 3,
 ( #76802, #7343, #70479, #64177, #63342, #43970, #6924 ),
 .UNSPECIFIED., .F., .F.,
 ( 4, 3, 4 ),
 ( 1.734723475976807094E-18, 0.001246230184515552441, 0.002492489877932635087 ),
 .UNSPECIFIED. ) ;
#81284 = CARTESIAN_POINT ( 'NONE',  ( -0.5249343832020990641, 0.2306618581243848609, 0.2411417322834645549 ) ) ;
#81285 = CARTESIAN_POINT ( 'NONE',  ( -1.607611548556429737, 0.1771653543307087075, -0.09757992244046823083 ) ) ;
#81286 = CARTESIAN_POINT ( 'NONE',  ( 0.7283464566929143125, 0.07958543189024085140, 0.2665933059059887866 ) ) ;
#81287 = CARTESIAN_POINT ( 'NONE',  ( 1.174540682414699111, -0.05778040916215560624, -0.4822834645669293319 ) ) ;
#81288 = CARTESIAN_POINT ( 'NONE',  ( 0.4724409448818898682, 2.892866454678787531E-17, -1.139763779527559029 ) ) ;
#81289 = CARTESIAN_POINT ( 'NONE',  ( 0.9383202099737538715, -0.08942795157528024563, -0.3641732283464568787 ) ) ;
#81290 = CARTESIAN_POINT ( 'NONE',  ( 0.9448818897637802916, -0.1870078740157479769, 0.4822834645669291653 ) ) ;
#81291 = EDGE_CURVE ( 'NONE', #57445, #53885, #53010, .T. ) ;
#81292 = CARTESIAN_POINT ( 'NONE',  ( -0.3949938075777411073, 0.1058382717557497660, -0.7395013123359579499 ) ) ;
#81293 = CARTESIAN_POINT ( 'NONE',  ( -0.8136482939632537770, -0.6046776061558807314, 0.2411417322834647770 ) ) ;
#81294 = DIRECTION ( 'NONE',  ( 1.000000000000000000, 1.601283208593976204E-15, 0.000000000000000000 ) ) ;
#81295 = AXIS2_PLACEMENT_3D ( 'NONE', #57311, #69141, #50585 ) ;
#81296 = CARTESIAN_POINT ( 'NONE',  ( 0.8530183727034126306, -0.004921259842519870586, -0.3153832671262229437 ) ) ;
#81297 = CARTESIAN_POINT ( 'NONE',  ( -0.4986876640419942164, -0.6046776061558807314, 0.2411417322834647770 ) ) ;
#81298 = CARTESIAN_POINT ( 'NONE',  ( -0.01968503937007793844, -0.5400638737290844871, 0.3530559997133364547 ) ) ;
#81299 = DIRECTION ( 'NONE',  ( 0.000000000000000000, 0.000000000000000000, 1.000000000000000000 ) ) ;
#81300 = CARTESIAN_POINT ( 'NONE',  ( 0.2559055118110243332, -0.5400638737290845981, -0.3530559997133363437 ) ) ;
#81301 = CARTESIAN_POINT ( 'NONE',  ( -0.04593175853018302557, 0.1771653543307087630, 0.09757992244046791164 ) ) ;
#81302 = CARTESIAN_POINT ( 'NONE',  ( -2.800715669567006127, 1.143166703770576387, 0.2643333500026571192 ) ) ;
#81303 = CARTESIAN_POINT ( 'NONE',  ( -0.03280839895013062252, 0.1771653543307087075, -0.09757992244046823083 ) ) ;
#81304 = CARTESIAN_POINT ( 'NONE',  ( 0.5971128608923890191, -0.5511811023622046335, 0.09757992244046803654 ) ) ;
#81305 = CARTESIAN_POINT ( 'NONE',  ( 1.595398199321655275, 1.309738123151863665, 0.1559797534342494407 ) ) ;
#81306 = CARTESIAN_POINT ( 'NONE',  ( 0.3460692066303959202, -0.1998031496062991630, -1.599081364829396446 ) ) ;
#81307 = CARTESIAN_POINT ( 'NONE',  ( 0.4724409448818904789, -0.1870078740157480879, -0.4822834645669291653 ) ) ;
#81308 = CARTESIAN_POINT ( 'NONE',  ( 0.3392501089628018329, 0.1958661417322835607, -1.698162729658792891 ) ) ;
#81309 = DIRECTION ( 'NONE',  ( 0.000000000000000000, -1.000000000000000000, 0.000000000000000000 ) ) ;
#81310 = CARTESIAN_POINT ( 'NONE',  ( -0.3922539627124310702, 0.006303098004691234414, -4.648478490738284608E-18 ) ) ;
#81311 = CARTESIAN_POINT ( 'NONE',  ( -0.3149606299212590610, -0.1870078740157479769, 0.3641732283464567677 ) ) ;
#81312 = VECTOR ( 'NONE', #3530, 39.37007874015748143 ) ;
#81313 = CARTESIAN_POINT ( 'NONE',  ( -0.3805774278215216522, 0.05413385826771666132, 0.4176697321401328100 ) ) ;
#81314 = CARTESIAN_POINT ( 'NONE',  ( 0.9317585301837276734, -0.004921259842519870586, -0.3153832671262229437 ) ) ;
#81315 = CARTESIAN_POINT ( 'NONE',  ( -1.653543307086613234, -0.1870078740157480601, -0.3641732283464567677 ) ) ;
#81316 = CARTESIAN_POINT ( 'NONE',  ( -1.502624671916009680, -0.05778040916215560624, -0.4822834645669293319 ) ) ;
#81317 = CARTESIAN_POINT ( 'NONE',  ( -0.006561679790025524116, -0.05778040916215560624, -0.4822834645669293319 ) ) ;
#81318 = CARTESIAN_POINT ( 'NONE',  ( 1.227034120734908917, 0.2952755905511810774, -0.1292274648535930714 ) ) ;
#81319 = CARTESIAN_POINT ( 'NONE',  ( 0.3230994083235798064, 1.189706270649605768, -1.965018580821014993 ) ) ;
#81320 = CARTESIAN_POINT ( 'NONE',  ( 0.1509186351706042484, -0.3162353388693405765, 0.4822834645669290543 ) ) ;
#81321 = CARTESIAN_POINT ( 'NONE',  ( 1.476377952755906442, -0.5400638737290844871, 0.3530559997133364547 ) ) ;
#81322 = CARTESIAN_POINT ( 'NONE',  ( 1.095800524934383846, -0.05778040916215560624, -0.4822834645669293319 ) ) ;
#81323 = CARTESIAN_POINT ( 'NONE',  ( -1.719160104986876103, -0.004921259842519576551, 0.3153832671262227771 ) ) ;
#81324 = CARTESIAN_POINT ( 'NONE',  ( 0.8858267716535438430, 0.07958543189024085140, 0.2665933059059887866 ) ) ;
#81325 = CARTESIAN_POINT ( 'NONE',  ( 1.587926509186352586, -0.4281496062992127816, -0.4176697321401328100 ) ) ;
#81326 = CARTESIAN_POINT ( 'NONE',  ( 0.2821522309711292364, -0.5511811023622046335, 0.09757992244046803654 ) ) ;
#81327 = CARTESIAN_POINT ( 'NONE',  ( -0.2690288713910754526, -0.6692913385826771977, 0.1292274648535927661 ) ) ;
#81328 = CARTESIAN_POINT ( 'NONE',  ( 0.4986876640419954376, 0.2306618581243848609, 0.2411417322834645549 ) ) ;
#81329 = CARTESIAN_POINT ( 'NONE',  ( -0.2427821522309703550, -0.3162353388693405765, 0.4822834645669290543 ) ) ;
#81330 = CARTESIAN_POINT ( 'NONE',  ( -0.3917322834645670659, -7.196005306013484475E-17, -2.240832964075802458 ) ) ;
#81331 = CARTESIAN_POINT ( 'NONE',  ( -0.4199475065616791736, 0.1283753931104746893, -0.1820866141732285504 ) ) ;
#81332 = CARTESIAN_POINT ( 'NONE',  ( 0.7742782152230978099, -0.4281496062992124485, 0.4176697321401328655 ) ) ;
#81333 = CARTESIAN_POINT ( 'NONE',  ( 0.8989501312335964611, 0.1771653543307087630, 0.09757992244046791164 ) ) ;
#81334 = CARTESIAN_POINT ( 'NONE',  ( 0.2690288713910767848, 0.2952755905511811885, 0.1292274648535926551 ) ) ;
#81335 = PLANE ( 'NONE',  #9758 ) ;
#81337 = CARTESIAN_POINT ( 'NONE',  ( -0.3996062992125986590, 0.1070741851644051862, -1.135170603674540590 ) ) ;
#81336 = CARTESIAN_POINT ( 'NONE',  ( 1.572991167713778227, 1.535433070866141447, 0.1227090857360984416 ) ) ;
#81338 = CARTESIAN_POINT ( 'NONE',  ( 0.3392501089628018329, 0.1958661417322835607, -2.170603674540682260 ) ) ;
#81339 = CARTESIAN_POINT ( 'NONE',  ( -1.423884514435694859, -0.05778040916215560624, -0.4822834645669293319 ) ) ;
#81340 = CARTESIAN_POINT ( 'NONE',  ( -0.5577427821522301654, -0.05778040916215560624, -0.4822834645669293319 ) ) ;
#81341 = CARTESIAN_POINT ( 'NONE',  ( 0.2362204724409451007, -0.4091458600556402980, -0.09186351706036745279 ) ) ;
#81342 = CARTESIAN_POINT ( 'NONE',  ( -9.674558042662121740E-17, 0.3949938075777409963, -2.834645669291338432 ) ) ;
#81343 = ORIENTED_EDGE ( 'NONE', *, *, #59409, .T. ) ;
#81344 = CARTESIAN_POINT ( 'NONE',  ( 0.5314960629921267055, -0.4536011799217367080, 0.2665933059059888421 ) ) ;
#81345 = CARTESIAN_POINT ( 'NONE',  ( 0.3392501089628018329, 0.1958661417322835607, -1.225721784776902634 ) ) ;
#81346 = CARTESIAN_POINT ( 'NONE',  ( 0.6102362204724416372, -0.5400638737290844871, 0.3530559997133364547 ) ) ;
#81347 = EDGE_CURVE ( 'NONE', #72947, #16761, #72585, .T. ) ;
#81348 = CARTESIAN_POINT ( 'NONE',  ( 0.1265901696524989462, 0.4724409448818897572, -2.513123359580052174 ) ) ;
#81349 = CARTESIAN_POINT ( 'NONE',  ( 0.5971128608923891301, 0.1771653543307087075, -0.09757992244046823083 ) ) ;
#81350 = CARTESIAN_POINT ( 'NONE',  ( 1.603475055217291612, 0.7166759647713490944, 0.04573490813648272563 ) ) ;
#81351 = CARTESIAN_POINT ( 'NONE',  ( -1.614173228346456268, -0.5511811023622047445, 6.969142054262312111E-17 ) ) ;
#81352 = CARTESIAN_POINT ( 'NONE',  ( 1.653543307086614789, -0.1870078740157479769, 0.4822834645669291653 ) ) ;
#81353 = CARTESIAN_POINT ( 'NONE',  ( 1.181102362204724976, -0.1870078740157480601, -0.3641732283464567677 ) ) ;
#81354 = CARTESIAN_POINT ( 'NONE',  ( 0.4330708661417329575, 0.2952755905511811885, 0.000000000000000000 ) ) ;
#81355 = CARTESIAN_POINT ( 'NONE',  ( 0.1958661417322836162, -0.3392501089628018329, -0.1718966947168485970 ) ) ;
#81356 = CARTESIAN_POINT ( 'NONE',  ( -0.4593175853018364174, -0.4281496062992127816, -0.4176697321401328100 ) ) ;
#81357 = CARTESIAN_POINT ( 'NONE',  ( -0.7874015748031489847, -0.1870078740157479769, 0.3641732283464567677 ) ) ;
#81358 = CARTESIAN_POINT ( 'NONE',  ( 0.5314960629921264834, 0.1660481256975883668, -0.3530559997133364547 ) ) ;
#81359 = CARTESIAN_POINT ( 'NONE',  ( 0.03280839895013198948, 0.2952755905511811885, 0.1292274648535926551 ) ) ;
#81360 = DIRECTION ( 'NONE',  ( -0.000000000000000000, -1.000000000000000000, -0.000000000000000000 ) ) ;
#81361 = FACE_OUTER_BOUND ( 'NONE', #62276, .T. ) ;
#81362 = CARTESIAN_POINT ( 'NONE',  ( 0.3392501089628018329, 0.1958661417322835607, -1.545294906333020135 ) ) ;
#81363 = CARTESIAN_POINT ( 'NONE',  ( 0.7152230971128616943, -0.05778040916215522460, 0.4822834645669289988 ) ) ;
#81364 = CARTESIAN_POINT ( 'NONE',  ( -0.4265091863517051496, 0.2952755905511810774, -0.1292274648535930714 ) ) ;
#81365 = CARTESIAN_POINT ( 'NONE',  ( -1.332020997375327642, -0.05778040916215522460, 0.4822834645669289988 ) ) ;
#81366 = CARTESIAN_POINT ( 'NONE',  ( 1.181102362204724976, -0.1870078740157480879, -0.4822834645669291653 ) ) ;
#81367 = CARTESIAN_POINT ( 'NONE',  ( 0.4986876640419954376, -0.6046776061558809534, -0.2411417322834644161 ) ) ;
#81368 = CARTESIAN_POINT ( 'NONE',  ( 0.3392501089628018329, 0.1958661417322835607, -1.003280839895013266 ) ) ;
#81369 = CARTESIAN_POINT ( 'NONE',  ( -0.2821522309711278487, 0.2952755905511811885, 0.1292274648535926551 ) ) ;
#81370 = CARTESIAN_POINT ( 'NONE',  ( 0.1640419947506569498, -0.3162353388693409650, -0.4822834645669289433 ) ) ;
#81371 = CARTESIAN_POINT ( 'NONE',  ( -0.3149606299212590610, -0.1870078740157480879, -0.4822834645669291653 ) ) ;
#81372 = CARTESIAN_POINT ( 'NONE',  ( 0.3280839895013130669, -0.3690944881889765550, -0.3153832671262227771 ) ) ;
#81373 = CARTESIAN_POINT ( 'NONE',  ( -1.653543307086613234, -0.1870078740157480879, -0.4822834645669291653 ) ) ;
#81374 = CARTESIAN_POINT ( 'NONE',  ( 0.000000000000000000, 0.03937007874015747977, 0.000000000000000000 ) ) ;
#81375 = CARTESIAN_POINT ( 'NONE',  ( 0.4265091863517067039, -0.6692913385826773087, -0.1292274648535924053 ) ) ;
#81376 = CARTESIAN_POINT ( 'NONE',  ( -1.313877454013331780, 1.062992125984252079, 0.7983292792091805090 ) ) ;
#81377 = CARTESIAN_POINT ( 'NONE',  ( -1.528871391076114250, -0.6692913385826771977, 0.1292274648535927661 ) ) ;
#81378 = CARTESIAN_POINT ( 'NONE',  ( -0.1049643490035302024, -0.3917322834645671215, -2.583989501312335513 ) ) ;
#81379 = VERTEX_POINT ( 'NONE', #59411 ) ;
#81380 = EDGE_LOOP ( 'NONE', ( #60770, #52119, #82779, #8875 ) ) ;
#81381 = CARTESIAN_POINT ( 'NONE',  ( 0.5314960629921267055, -0.5400638737290844871, 0.3530559997133364547 ) ) ;
#81382 = CARTESIAN_POINT ( 'NONE',  ( 0.05249343832021075018, 0.1283753931104746893, -0.1820866141732285504 ) ) ;
#81384 = DIRECTION ( 'NONE',  ( -0.000000000000000000, -1.000000000000000000, -0.000000000000000000 ) ) ;
#81383 = CARTESIAN_POINT ( 'NONE',  ( 2.154527559055120278, 0.03937007874015747977, -0.4677827689124846589 ) ) ;
#81385 = CARTESIAN_POINT ( 'NONE',  ( 0.1958661417322834775, 0.3392501089628018884, -0.8589238845144357981 ) ) ;
#81386 = CARTESIAN_POINT ( 'NONE',  ( -0.9552210167251737882, -5.134928753749862370E-15, -0.4281989832122467532 ) ) ;
#81387 = CARTESIAN_POINT ( 'NONE',  ( 0.3042614371611548907, -3.790565315793794774E-16, -0.4118477457932737118 ) ) ;
#81388 = CARTESIAN_POINT ( 'NONE',  ( 0.3460692066303959202, -0.1998031496062991630, -2.543963254593176071 ) ) ;
#81389 = CARTESIAN_POINT ( 'NONE',  ( 0.5118110236220478892, 0.2952755905511811885, 0.000000000000000000 ) ) ;
#81390 = CARTESIAN_POINT ( 'NONE',  ( -0.6889763779527552368, 0.1660481256975885056, 0.3530559997133364547 ) ) ;
#81391 = CARTESIAN_POINT ( 'NONE',  ( -0.6036745406824141069, 0.2306618581243848609, 0.2411417322834645549 ) ) ;
#81392 = CARTESIAN_POINT ( 'NONE',  ( 0.5839895013123367340, -0.6692913385826773087, -0.1292274648535924053 ) ) ;
#81393 = CARTESIAN_POINT ( 'NONE',  ( 1.364829396325459854, -0.6046776061558809534, -0.2411417322834644161 ) ) ;
#81394 = CARTESIAN_POINT ( 'NONE',  ( 1.200787401574803681, 0.07958543189024085140, 0.2665933059059887866 ) ) ;
#81395 = CONTEXT_DEPENDENT_SHAPE_REPRESENTATION ( #26684, #27158 ) ;
#81396 = CARTESIAN_POINT ( 'NONE',  ( 1.108923884514436686, -0.2845877964562161244, -0.3641732283464567121 ) ) ;
#81397 = CARTESIAN_POINT ( 'NONE',  ( -0.8005249343832011588, 0.05413385826771626580, -0.4176697321401330321 ) ) ;
#81398 = CARTESIAN_POINT ( 'NONE',  ( -0.3996062992125984925, -0.1070741851644056858, -0.5951443569553805935 ) ) ;
#81399 = CARTESIAN_POINT ( 'NONE',  ( 1.660104986876641320, -0.05778040916215522460, 0.4822834645669289988 ) ) ;
#81400 = DIRECTION ( 'NONE',  ( -0.000000000000000000, 1.000000000000000000, -0.000000000000000000 ) ) ;
#81401 = CARTESIAN_POINT ( 'NONE',  ( -0.1443569553805765515, -0.4281496062992127816, -0.4176697321401328100 ) ) ;
#81403 = DIRECTION ( 'NONE',  ( 0.000000000000000000, 0.000000000000000000, 1.000000000000000000 ) ) ;
#81402 = CARTESIAN_POINT ( 'NONE',  ( 0.9908136482939640111, -0.6692913385826771977, 0.1292274648535927661 ) ) ;
#81404 = CARTESIAN_POINT ( 'NONE',  ( -1.181102362204723644, -0.1870078740157480601, -0.3641732283464567677 ) ) ;
#81405 = CARTESIAN_POINT ( 'NONE',  ( 0.3937007874015754361, -0.1870078740157479769, 0.4822834645669291653 ) ) ;
#81406 = CARTESIAN_POINT ( 'NONE',  ( 0.7086614173228352742, -0.1870078740157480601, -0.3641732283464567677 ) ) ;
#81407 = CARTESIAN_POINT ( 'NONE',  ( 0.3392501089628018329, -0.1958661417322834497, -1.444862573981940512 ) ) ;
#81408 = CARTESIAN_POINT ( 'NONE',  ( -1.299212598425196097, -0.5511811023622047445, 6.969142054262312111E-17 ) ) ;
#81409 = CARTESIAN_POINT ( 'NONE',  ( 1.345144356955381593, -0.05778040916215522460, 0.4822834645669289988 ) ) ;
#81410 = DIRECTION ( 'NONE',  ( -0.000000000000000000, 1.000000000000000000, -0.000000000000000000 ) ) ;
#81411 = CARTESIAN_POINT ( 'NONE',  ( -0.1771653543307080136, -0.4536011799217367080, 0.2665933059059888421 ) ) ;
#81412 = CARTESIAN_POINT ( 'NONE',  ( -0.1181102362204717315, 0.2952755905511811885, 0.000000000000000000 ) ) ;
#81413 = CARTESIAN_POINT ( 'NONE',  ( -1.213910761154854745, -0.5511811023622046335, 0.09757992244046803654 ) ) ;
#81414 = ADVANCED_FACE ( 'NONE', ( #19871 ), #40910, .T. ) ;
#81415 = CARTESIAN_POINT ( 'NONE',  ( -0.5839895013123351797, 0.2952755905511810774, -0.1292274648535930714 ) ) ;
#81416 = CARTESIAN_POINT ( 'NONE',  ( 1.318897637795276356, -0.5400638737290844871, 0.3530559997133364547 ) ) ;
#81417 = CARTESIAN_POINT ( 'NONE',  ( -0.2867679344610365444, -0.2867679344610367664, -0.3707542239183220789 ) ) ;
#81418 = CARTESIAN_POINT ( 'NONE',  ( -0.9776902887139098386, 0.1771653543307087075, -0.09757992244046823083 ) ) ;
#81419 = CARTESIAN_POINT ( 'NONE',  ( 0.4324858057354169505, 1.341834121656384715, -1.665041785426940368 ) ) ;
#81420 = CARTESIAN_POINT ( 'NONE',  ( 1.509186351706037543, -0.4281496062992127816, -0.4176697321401328100 ) ) ;
#81421 = CARTESIAN_POINT ( 'NONE',  ( 0.1265901696524990294, -0.4724409448818896462, -2.209317585301837195 ) ) ;
#81422 = AXIS2_PLACEMENT_3D ( 'NONE', #29130, #74175, #55200 ) ;
#81423 = CARTESIAN_POINT ( 'NONE',  ( -1.122047244094487306, -0.5400638737290844871, 0.3530559997133364547 ) ) ;
#81424 = CARTESIAN_POINT ( 'NONE',  ( -1.279527559055116948, 0.07958543189024071263, -0.2665933059059888421 ) ) ;
#81425 = CARTESIAN_POINT ( 'NONE',  ( -0.6955380577427815458, -0.3690944881889765550, -0.3153832671262227771 ) ) ;
#81426 = CARTESIAN_POINT ( 'NONE',  ( 0.3503937007874015630, -0.5120078740157480990, -0.4921259842519685179 ) ) ;
#81427 = CARTESIAN_POINT ( 'NONE',  ( 8.195543980992789655E-16, -0.1870078740157480879, -0.4822834645669291653 ) ) ;
#81428 = CARTESIAN_POINT ( 'NONE',  ( -0.1706036745406816491, -0.004921259842519870586, -0.3153832671262229437 ) ) ;
#81429 = CARTESIAN_POINT ( 'NONE',  ( -1.272965879265091305, -0.3690944881889763329, 0.3153832671262228327 ) ) ;
#81430 = CARTESIAN_POINT ( 'NONE',  ( -1.391076115485563758, 0.2306618581243848609, 0.2411417322834645549 ) ) ;
#81431 = CARTESIAN_POINT ( 'NONE',  ( 1.246719160104987623, -0.3690944881889763329, 0.3153832671262228327 ) ) ;
#81432 = CARTESIAN_POINT ( 'NONE',  ( 1.154855643044620184, -0.6046776061558807314, 0.2411417322834647770 ) ) ;
#81433 = CARTESIAN_POINT ( 'NONE',  ( -1.614173228346457378, 0.5038684218300933937, -0.1372047244094477536 ) ) ;
#81434 = CARTESIAN_POINT ( 'NONE',  ( 0.4330708661417329575, 0.1771653543307087630, 0.000000000000000000 ) ) ;
#81435 = CARTESIAN_POINT ( 'NONE',  ( 0.9908136482939640111, -0.6692913385826771977, 0.1292274648535927661 ) ) ;
#81436 = CARTESIAN_POINT ( 'NONE',  ( 0.8464566929133865436, 0.07958543189024071263, -0.2665933059059888421 ) ) ;
#81437 = ORIENTED_EDGE ( 'NONE', *, *, #80583, .F. ) ;
#81438 = CARTESIAN_POINT ( 'NONE',  ( -1.253280839895012377, -0.3162353388693409650, -0.4822834645669289433 ) ) ;
#81439 = EDGE_CURVE ( 'NONE', #35380, #76682, #13151, .T. ) ;
#81440 = CARTESIAN_POINT ( 'NONE',  ( -0.7020997375328074108, -0.05778040916215522460, 0.4822834645669289988 ) ) ;
#81441 = CARTESIAN_POINT ( 'NONE',  ( 0.1049868766404206816, -0.6046776061558809534, -0.2411417322834644161 ) ) ;
#81442 = CARTESIAN_POINT ( 'NONE',  ( -1.646051170424378096, 0.000000000000000000, -0.3464511005275205946 ) ) ;
#81443 = CARTESIAN_POINT ( 'NONE',  ( 0.1998031496062992463, 0.3460692066303959202, -2.425853018372703396 ) ) ;
#81444 = CARTESIAN_POINT ( 'NONE',  ( 1.043307086614173818, -0.5400638737290845981, -0.3530559997133363437 ) ) ;
#81445 = CARTESIAN_POINT ( 'NONE',  ( 1.482939632545932307, -0.004921259842519870586, -0.3153832671262229437 ) ) ;
#81446 = CARTESIAN_POINT ( 'NONE',  ( 0.1574803149606306130, -0.1870078740157480879, -0.4822834645669291653 ) ) ;
#81447 = CARTESIAN_POINT ( 'NONE',  ( 0.6627296587926515548, 0.2952755905511811885, 0.1292274648535926551 ) ) ;
#81448 = CARTESIAN_POINT ( 'NONE',  ( 4.893765752498283924E-17, -0.3996062992125986035, -1.811023622047244208 ) ) ;
#81449 = CARTESIAN_POINT ( 'NONE',  ( 0.3949938075777409963, 2.418639510665530435E-17, -1.692913385826771533 ) ) ;
#81450 = CARTESIAN_POINT ( 'NONE',  ( -0.4744094488189005143, 1.537401574803149984, 1.016821367227982220 ) ) ;
#81451 = CARTESIAN_POINT ( 'NONE',  ( -0.5636006452641416642, -2.613618158232546091E-15, -0.3464511005275220379 ) ) ;
#81452 = CARTESIAN_POINT ( 'NONE',  ( -0.2867679344610364334, -0.2867679344610367109, -0.5236220472440944462 ) ) ;
#81453 = CARTESIAN_POINT ( 'NONE',  ( -0.5577427821522301654, -0.08942795157528024563, -0.3641732283464568787 ) ) ;
#81454 = CARTESIAN_POINT ( 'NONE',  ( -0.6299212598425188991, -0.1870078740157479769, 0.4822834645669291653 ) ) ;
#81455 = CARTESIAN_POINT ( 'NONE',  ( 0.6627296587926515548, 0.2952755905511811885, 0.1292274648535926551 ) ) ;
#81456 = CARTESIAN_POINT ( 'NONE',  ( -0.3420746716998660508, -0.1974969037888706924, -2.019028871391076230 ) ) ;
#81457 = CARTESIAN_POINT ( 'NONE',  ( 0.8989501312335964611, 0.2952755905511811885, 0.1292274648535926551 ) ) ;
#81458 = CARTESIAN_POINT ( 'NONE',  ( -1.417322834645668772, -0.1870078740157480879, -0.4822834645669291653 ) ) ;
#81459 = CARTESIAN_POINT ( 'NONE',  ( 1.213910761154856299, -0.6692913385826773087, -0.1292274648535924053 ) ) ;
#81460 = CARTESIAN_POINT ( 'NONE',  ( -1.157146581871515012E-16, 0.4724409448818898682, -2.362204724409448620 ) ) ;
#81461 = CARTESIAN_POINT ( 'NONE',  ( 0.3460692066303959757, -0.1998031496062991907, -1.837270341207349000 ) ) ;
#81462 = CARTESIAN_POINT ( 'NONE',  ( 0.9186351706036751663, -0.6046776061558807314, 0.2411417322834647770 ) ) ;
#81463 = CARTESIAN_POINT ( 'NONE',  ( 0.6036745406824153282, -0.6046776061558807314, 0.2411417322834647770 ) ) ;
#81464 = CARTESIAN_POINT ( 'NONE',  ( 1.095800524934383846, -0.2845877964562159024, 0.3641732283464567677 ) ) ;
#81466 = CARTESIAN_POINT ( 'NONE',  ( -1.561679790026246017, -0.4281496062992127816, -0.4176697321401328100 ) ) ;
#81465 = CARTESIAN_POINT ( 'NONE',  ( -1.528871391076114250, -0.5511811023622046335, 0.09757992244046803654 ) ) ;
#81467 = CARTESIAN_POINT ( 'NONE',  ( 0.3917322834645668994, 0.1049643490035304522, -2.724390133037059236 ) ) ;
#81468 =( CONVERSION_BASED_UNIT ( 'INCH', #36831 ) LENGTH_UNIT ( ) NAMED_UNIT ( #24430 ) );
#81469 = CARTESIAN_POINT ( 'NONE',  ( 0.9645669291338591078, -0.5400638737290845981, -0.3530559997133363437 ) ) ;
#81470 = CARTESIAN_POINT ( 'NONE',  ( 1.568241469816273659, -0.08942795157528024563, -0.3641732283464568787 ) ) ;
#81471 = CARTESIAN_POINT ( 'NONE',  ( -0.5708661417322828946, 0.1660481256975883668, -0.3530559997133364547 ) ) ;
#81472 = CARTESIAN_POINT ( 'NONE',  ( -0.7545931758530177724, 0.2952755905511811885, 0.1292274648535926551 ) ) ;
#81473 = CARTESIAN_POINT ( 'NONE',  ( 1.397637795275591177, -0.5400638737290844871, 0.3530559997133364547 ) ) ;
#81474 = CARTESIAN_POINT ( 'NONE',  ( 0.3392501089628018329, 0.1958661417322835607, -0.2158792650918636147 ) ) ;
#81475 = CARTESIAN_POINT ( 'NONE',  ( 0.4068241469816279987, -0.4281496062992127816, -0.4176697321401328100 ) ) ;
#81476 = CARTESIAN_POINT ( 'NONE',  ( 0.1958661417322834775, 0.3392501089628018884, -2.498687664041994605 ) ) ;
#81477 = CARTESIAN_POINT ( 'NONE',  ( -1.561679790026246017, -0.3690944881889765550, -0.3153832671262227771 ) ) ;
#81478 = ORIENTED_EDGE ( 'NONE', *, *, #78936, .F. ) ;
#81479 = CARTESIAN_POINT ( 'NONE',  ( 0.1058382717557500713, -0.3949938075777409408, -2.762467191601050587 ) ) ;
#81480 = ORIENTED_EDGE ( 'NONE', *, *, #22453, .F. ) ;
#81481 = PLANE ( 'NONE',  #70444 ) ;
#81482 = CIRCLE ( 'NONE', #78787, 0.4822834645669291653 ) ;
#81483 = CARTESIAN_POINT ( 'NONE',  ( 1.181102362204724976, -0.1870078740157480601, -0.3641732283464567677 ) ) ;
#81484 = CARTESIAN_POINT ( 'NONE',  ( -0.3996062992125986035, -7.340648628747425578E-17, -0.8267716535433070613 ) ) ;
#81485 = CARTESIAN_POINT ( 'NONE',  ( 1.541994750656168645, 0.1771653543307087075, -0.09757992244046823083 ) ) ;
#81486 = LINE ( 'NONE', #11605, #53148 ) ;
#81487 = PLANE ( 'NONE',  #30211 ) ;
#81488 = CARTESIAN_POINT ( 'NONE',  ( -0.3126874984954384762, 1.620889671569059942, 0.01505614298776670329 ) ) ;
#81489 = CARTESIAN_POINT ( 'NONE',  ( -0.1958661417322836718, 0.3392501089628017219, -0.2552493438320210806 ) ) ;
#81490 = CARTESIAN_POINT ( 'NONE',  ( -0.5708661417322825615, -0.4536011799217367080, 0.2665933059059888421 ) ) ;
#81491 = CARTESIAN_POINT ( 'NONE',  ( -1.062992125984250968, 0.1771653543307087630, 0.000000000000000000 ) ) ;
#81492 = CARTESIAN_POINT ( 'NONE',  ( 1.443569553805774897, 0.2306618581243848609, 0.2411417322834645549 ) ) ;
#81493 = CARTESIAN_POINT ( 'NONE',  ( 0.6102362204724416372, -0.5400638737290844871, 0.3530559997133364547 ) ) ;
#81494 = CARTESIAN_POINT ( 'NONE',  ( -1.154855643044618851, 0.2306618581243848609, 0.2411417322834645549 ) ) ;
#81495 = CARTESIAN_POINT ( 'NONE',  ( -0.1049643490035307020, 0.3917322834645669549, -0.3136482939632545541 ) ) ;
#81496 = ORIENTED_EDGE ( 'NONE', *, *, #16301, .T. ) ;
#81497 = CARTESIAN_POINT ( 'NONE',  ( 1.377952755905512472, -0.6692913385826771977, 8.415575281601705876E-17 ) ) ;
#81498 = DIRECTION ( 'NONE',  ( -0.5653208194167064216, 0.6006868920394703437, 0.5653208194167143041 ) ) ;
#81499 = CARTESIAN_POINT ( 'NONE',  ( -0.1265901696524986964, -0.4724409448818899238, -1.646981627296587591 ) ) ;
#81500 = CARTESIAN_POINT ( 'NONE',  ( 2.103514684735005247, 1.710972922415816999, 0.4417590601942928408 ) ) ;
#81501 = CARTESIAN_POINT ( 'NONE',  ( 0.2867679344610366554, 0.2867679344610366554, -2.742125984251967630 ) ) ;
#81502 = CARTESIAN_POINT ( 'NONE',  ( -0.5380577427821514602, 0.05413385826771666132, 0.4176697321401328100 ) ) ;
#81503 = CARTESIAN_POINT ( 'NONE',  ( 0.8595800524934390507, -0.3162353388693405765, 0.4822834645669290543 ) ) ;
#81505 = DIRECTION ( 'NONE',  ( 0.000000000000000000, -0.8660254037844388186, 0.4999999999999997224 ) ) ;
#81504 = CARTESIAN_POINT ( 'NONE',  ( 0.000000000000000000, 0.000000000000000000, 0.1574803149606299191 ) ) ;
#81506 = CARTESIAN_POINT ( 'NONE',  ( -1.633858267716534529, -0.5400638737290845981, -0.3530559997133363437 ) ) ;
#81507 = CARTESIAN_POINT ( 'NONE',  ( -0.9251968503937002541, 0.1660481256975885056, 0.3530559997133364547 ) ) ;
#81508 = CARTESIAN_POINT ( 'NONE',  ( -0.1958661417322836440, 0.3392501089628016664, -0.2506368521971635843 ) ) ;
#81509 = CARTESIAN_POINT ( 'NONE',  ( 0.1443569553805781891, -0.3690944881889763329, 0.3153832671262228327 ) ) ;
#81510 = CARTESIAN_POINT ( 'NONE',  ( -0.3917322834645671215, 0.1049643490035301469, -0.5898950131233596794 ) ) ;
#81511 = CARTESIAN_POINT ( 'NONE',  ( 0.006561679790026889343, -0.2845877964562161244, -0.3641732283464567121 ) ) ;
#81513 = EDGE_CURVE ( 'NONE', #49988, #34953, #14412, .T. ) ;
#81512 = CARTESIAN_POINT ( 'NONE',  ( 0.6692913385826777528, 0.1771653543307087630, 0.000000000000000000 ) ) ;
#81514 = CARTESIAN_POINT ( 'NONE',  ( 0.4330708661417329575, -0.6692913385826771977, 8.415575281601705876E-17 ) ) ;
#81515 = CARTESIAN_POINT ( 'NONE',  ( -0.8661417322834640276, -0.1870078740157479769, 0.3641732283464567677 ) ) ;
#81516 = CARTESIAN_POINT ( 'NONE',  ( -0.2867679344610365999, 0.2867679344610364889, -2.216535433070866201 ) ) ;
#81517 = CARTESIAN_POINT ( 'NONE',  ( -1.627296587926508442, 0.2306618581243848609, 0.2411417322834645549 ) ) ;
#81518 = CIRCLE ( 'NONE', #39801, 3.937007874015748143 ) ;
#81519 = CARTESIAN_POINT ( 'NONE',  ( -1.128608923884513837, 0.2306618581243847221, -0.2411417322834647770 ) ) ;
#81520 = CONICAL_SURFACE ( 'NONE', #62694, 1.181102362204724310, 0.7853981633974621568 ) ;
#81521 = CARTESIAN_POINT ( 'NONE',  ( 0.4091458600556404646, -0.2362204724409448231, -0.9691601049868766582 ) ) ;
#81522 = CARTESIAN_POINT ( 'NONE',  ( 0.1377952755905518800, -0.5400638737290844871, 0.3530559997133364547 ) ) ;
#81523 = CARTESIAN_POINT ( 'NONE',  ( -0.5577427821522301654, -0.3162353388693405765, 0.4822834645669290543 ) ) ;
#81524 = CARTESIAN_POINT ( 'NONE',  ( 1.043307086614173818, 0.07958543189024085140, 0.2665933059059887866 ) ) ;
#81525 = CARTESIAN_POINT ( 'NONE',  ( -0.06561679790026180015, -0.3690944881889765550, -0.3153832671262227771 ) ) ;
#81526 = CARTESIAN_POINT ( 'NONE',  ( -0.1181102362204717315, 0.2952755905511811885, 0.000000000000000000 ) ) ;
#81527 = CARTESIAN_POINT ( 'NONE',  ( -1.213910761154854745, -0.6692913385826771977, 0.1292274648535927661 ) ) ;
#81528 = CARTESIAN_POINT ( 'NONE',  ( -3.896872718254346779, 2.702643891907236640, 0.5314960629921260393 ) ) ;
#81529 = LINE ( 'NONE', #23849, #35498 ) ;
#81530 = CARTESIAN_POINT ( 'NONE',  ( 0.1640419947506569498, -0.3162353388693409650, -0.4822834645669289433 ) ) ;
#81531 = ORIENTED_EDGE ( 'NONE', *, *, #76698, .F. ) ;
#81532 = CARTESIAN_POINT ( 'NONE',  ( -0.2925321140481932369, 0.2925321140481931259, -1.828740157480315265 ) ) ;
#81533 = CARTESIAN_POINT ( 'NONE',  ( 1.345144356955381593, -0.3162353388693409650, -0.4822834645669289433 ) ) ;
#81534 = CARTESIAN_POINT ( 'NONE',  ( -0.7480314960629914633, 0.1771653543307087630, 0.000000000000000000 ) ) ;
#81535 = VECTOR ( 'NONE', #81603, 39.37007874015748143 ) ;
#81536 = CARTESIAN_POINT ( 'NONE',  ( -0.3740157480314953431, -0.5400638737290845981, -0.3530559997133363437 ) ) ;
#81537 = CARTESIAN_POINT ( 'NONE',  ( 1.102362204724410155, -0.1870078740157480879, -0.4822834645669291653 ) ) ;
#81538 = CARTESIAN_POINT ( 'NONE',  ( 1.089238845144357759, 0.05413385826771626580, -0.4176697321401330321 ) ) ;
#81539 = CARTESIAN_POINT ( 'NONE',  ( -1.548556430446193399, -0.6046776061558809534, -0.2411417322834644161 ) ) ;
#81540 = CARTESIAN_POINT ( 'NONE',  ( -1.220472440944881054, 0.1771653543307087630, 0.000000000000000000 ) ) ;
#81541 = CARTESIAN_POINT ( 'NONE',  ( -9.787531504996566615E-17, 0.3996062992125985480, -0.3917322834645669549 ) ) ;
#81542 = CARTESIAN_POINT ( 'NONE',  ( 0.1998031496062994405, -0.3460692066303958092, -0.4068241469816273326 ) ) ;
#81543 = CARTESIAN_POINT ( 'NONE',  ( 0.3917322834645670659, 2.398668435337828261E-17, -2.949494381398636733 ) ) ;
#81544 = B_SPLINE_CURVE_WITH_KNOTS ( 'NONE', 3,
 ( #41170, #33612, #8771, #59688, #72746, #60114, #66861, #20574, #2043, #2874, #39932, #72338, #60525, #8360, #34027, #21399 ),
 .UNSPECIFIED., .F., .F.,
 ( 4, 2, 2, 2, 2, 2, 2, 4 ),
 ( 0.000000000000000000, 0.0003923911760484627724, 0.0007847823520969255447, 0.001177173528145388209, 0.001569564704193851089, 0.001961955880242313970, 0.002354347056290776417, 0.003139129408387686133 ),
 .UNSPECIFIED. ) ;
#81545 = CARTESIAN_POINT ( 'NONE',  ( 1.437007874015748810, -0.4536011799217368745, -0.2665933059059886201 ) ) ;
#81546 = CARTESIAN_POINT ( 'NONE',  ( 0.7742782152230978099, -0.3690944881889763329, 0.3153832671262228327 ) ) ;
#81547 = CARTESIAN_POINT ( 'NONE',  ( 0.5249343832021003964, 0.2306618581243847221, -0.2411417322834647770 ) ) ;
#81548 = CARTESIAN_POINT ( 'NONE',  ( 0.4724409448818898127, -0.1265901696524988629, -2.393044619422572072 ) ) ;
#81549 = CARTESIAN_POINT ( 'NONE',  ( 0.1974969037888706092, -0.3420746716998660508, -0.9560367454068241511 ) ) ;
#81550 = CARTESIAN_POINT ( 'NONE',  ( 0.9776902887139113929, -0.5511811023622048555, -0.09757992244046775898 ) ) ;
#81551 = CARTESIAN_POINT ( 'NONE',  ( -0.4396325459317577122, -0.6692913385826773087, -0.1292274648535924053 ) ) ;
#81552 = CARTESIAN_POINT ( 'NONE',  ( -0.6561679790026240244, 0.2306618581243847221, -0.2411417322834647770 ) ) ;
#81553 = CARTESIAN_POINT ( 'NONE',  ( 1.279527559055118724, -0.5400638737290845981, -0.3530559997133363437 ) ) ;
#81554 = CARTESIAN_POINT ( 'NONE',  ( 0.1265901696524990294, -0.4724409448818896462, -1.345144356955380704 ) ) ;
#81555 = CARTESIAN_POINT ( 'NONE',  ( -0.3996062992125986590, 0.1070741851644051862, -2.395013123359579943 ) ) ;
#81556 = CARTESIAN_POINT ( 'NONE',  ( -0.2427821522309703550, -0.08942795157528024563, -0.3641732283464568787 ) ) ;
#81557 = EDGE_CURVE ( 'NONE', #41461, #42318, #24776, .T. ) ;
#81558 = VERTEX_POINT ( 'NONE', #59003 ) ;
#81559 = CARTESIAN_POINT ( 'NONE',  ( 0.1049643490035304799, -0.3917322834645670104, -0.7119615729996870979 ) ) ;
#81560 = EDGE_LOOP ( 'NONE', ( #76876, #79102, #44256, #5786 ) ) ;
#81561 = CARTESIAN_POINT ( 'NONE',  ( -0.8661417322834640276, -0.1870078740157480879, -0.4822834645669291653 ) ) ;
#81562 = CARTESIAN_POINT ( 'NONE',  ( -0.08530183727034056085, -0.3162353388693405765, 0.4822834645669290543 ) ) ;
#81563 = CARTESIAN_POINT ( 'NONE',  ( -0.1443569553805765515, -0.4281496062992127816, -0.4176697321401328100 ) ) ;
#81564 = CARTESIAN_POINT ( 'NONE',  ( 0.4002624671916016896, -0.05778040916215522460, 0.4822834645669289988 ) ) ;
#81565 = ADVANCED_FACE ( 'NONE', ( #2181 ), #1767, .T. ) ;
#81566 = CARTESIAN_POINT ( 'NONE',  ( -0.4265091863517051496, -0.6692913385826771977, 0.1292274648535927661 ) ) ;
#81567 = CARTESIAN_POINT ( 'NONE',  ( -1.305774278215222184, 0.2952755905511811885, 0.1292274648535926551 ) ) ;
#81568 = CARTESIAN_POINT ( 'NONE',  ( -0.9055118110236215490, 0.2952755905511811885, 0.000000000000000000 ) ) ;
#81569 = CARTESIAN_POINT ( 'NONE',  ( 0.6955380577427828781, 0.05413385826771626580, -0.4176697321401330321 ) ) ;
#81570 = CARTESIAN_POINT ( 'NONE',  ( 0.6824146981627303710, 0.2306618581243847221, -0.2411417322834647770 ) ) ;
#81571 = CARTESIAN_POINT ( 'NONE',  ( -0.2867679344610364334, -0.2867679344610367109, -0.8385826771653541734 ) ) ;
#81572 = CARTESIAN_POINT ( 'NONE',  ( -0.2821522309711278487, -0.5511811023622048555, -0.09757992244046775898 ) ) ;
#81573 = ORIENTED_EDGE ( 'NONE', *, *, #49711, .F. ) ;
#81574 = CARTESIAN_POINT ( 'NONE',  ( -0.3420746716998661618, 0.1974969037888702206, -1.601049868766404094 ) ) ;
#81575 = VECTOR ( 'NONE', #70401, 39.37007874015748143 ) ;
#81576 = ORIENTED_EDGE ( 'NONE', *, *, #3360, .T. ) ;
#81577 = CARTESIAN_POINT ( 'NONE',  ( -1.351706036745406347, -0.004921259842519870586, -0.3153832671262229437 ) ) ;
#81578 = AXIS2_PLACEMENT_3D ( 'NONE', #41404, #15750, #67086 ) ;
#81579 = CIRCLE ( 'NONE', #13012, 0.01968503937007875723 ) ;
#81580 = CARTESIAN_POINT ( 'NONE',  ( -0.4396325459317577122, -0.6692913385826773087, -0.1292274648535924053 ) ) ;
#81581 = CARTESIAN_POINT ( 'NONE',  ( -0.3996062992125986035, -7.340648628747425578E-17, 0.1181102362204724254 ) ) ;
#81582 = CARTESIAN_POINT ( 'NONE',  ( -0.4921259842519677963, -0.5400638737290844871, 0.3530559997133364547 ) ) ;
#81583 = CARTESIAN_POINT ( 'NONE',  ( -0.9645669291338575535, -0.5400638737290844871, 0.3530559997133364547 ) ) ;
#81584 = CARTESIAN_POINT ( 'NONE',  ( -1.587926509186350810, 0.05413385826771626580, -0.4176697321401330321 ) ) ;
#81585 = DIRECTION ( 'NONE',  ( -0.000000000000000000, -1.000000000000000000, -0.000000000000000000 ) ) ;
#81586 = CARTESIAN_POINT ( 'NONE',  ( 0.8727034120734913358, -0.08942795157527998196, 0.3641732283464567121 ) ) ;
#81587 = CARTESIAN_POINT ( 'NONE',  ( 3.224202737261815166, 2.716535433070866645, 0.5314960629921260393 ) ) ;
#81588 = CARTESIAN_POINT ( 'NONE',  ( -0.1958661417322836718, 0.3392501089628017219, 0.2171916010498686767 ) ) ;
#81589 = CARTESIAN_POINT ( 'NONE',  ( 0.1443569553805781891, -0.3690944881889763329, 0.3153832671262228327 ) ) ;
#81590 = CARTESIAN_POINT ( 'NONE',  ( -0.2755905511811015396, -0.6692913385826771977, 8.415575281601705876E-17 ) ) ;
#81591 = CARTESIAN_POINT ( 'NONE',  ( 3.920840774341704638, 1.223555610140524941, 0.3571001360657545254 ) ) ;
#81592 = CARTESIAN_POINT ( 'NONE',  ( -0.03937007874015669567, 0.2952755905511811885, 0.000000000000000000 ) ) ;
#81593 = ORIENTED_EDGE ( 'NONE', *, *, #81194, .T. ) ;
#81594 = CARTESIAN_POINT ( 'NONE',  ( -0.3460692066303958092, -0.1998031496062994683, -1.942257217847769057 ) ) ;
#81595 = DIRECTION ( 'NONE',  ( 0.000000000000000000, 1.000000000000000000, 0.000000000000000000 ) ) ;
#81596 = ORIENTED_EDGE ( 'NONE', *, *, #66936, .F. ) ;
#81597 = CARTESIAN_POINT ( 'NONE',  ( 0.3996062992125986035, -0.1070741851644052972, -1.605643044619422977 ) ) ;
#81598 = CARTESIAN_POINT ( 'NONE',  ( 5.333846858410640380E-15, 1.062992125984252079, -1.444810848096780953 ) ) ;
#81599 = CARTESIAN_POINT ( 'NONE',  ( -0.5118110236220466680, -0.5511811023622047445, 6.969142054262312111E-17 ) ) ;
#81600 = CARTESIAN_POINT ( 'NONE',  ( -0.8267716535433065062, -0.6692913385826771977, 8.415575281601705876E-17 ) ) ;
#81601 = CARTESIAN_POINT ( 'NONE',  ( -0.4724409448818898682, -8.678599364036362592E-17, -0.5118110236220472231 ) ) ;
#81602 = EDGE_CURVE ( 'NONE', #46245, #11181, #48415, .T. ) ;
#81603 = DIRECTION ( 'NONE',  ( -0.000000000000000000, -0.000000000000000000, 1.000000000000000000 ) ) ;
#81604 = CARTESIAN_POINT ( 'NONE',  ( -0.1049643490035307020, 0.3917322834645669549, 0.1587926509186352031 ) ) ;
#81605 = CARTESIAN_POINT ( 'NONE',  ( 1.207349081364829990, 0.2306618581243848609, 0.2411417322834645549 ) ) ;
#81606 = CARTESIAN_POINT ( 'NONE',  ( 0.4330708661417329575, -0.6692913385826771977, 8.415575281601705876E-17 ) ) ;
#81607 = CARTESIAN_POINT ( 'NONE',  ( 0.5446194225721792126, -0.3162353388693405765, 0.4822834645669290543 ) ) ;
#81608 = CARTESIAN_POINT ( 'NONE',  ( -0.6496062992125976043, 0.07958543189024071263, -0.2665933059059888421 ) ) ;
#81609 = B_SPLINE_CURVE_WITH_KNOTS ( 'NONE', 3,
 ( #53755, #24664, #48689, #80708, #30578, #55821, #42781 ),
 .UNSPECIFIED., .F., .F.,
 ( 4, 3, 4 ),
 ( 7.459310946700270506E-17, 0.001246232571205254649, 0.002492492258783168303 ),
 .UNSPECIFIED. ) ;
#81610 = CARTESIAN_POINT ( 'NONE',  ( -0.3280839895013117347, -0.4281496062992124485, 0.4176697321401328655 ) ) ;
#81611 = CARTESIAN_POINT ( 'NONE',  ( -0.3458507752293909498, 0.3458507752293907833, -2.301181102362204633 ) ) ;
#81612 = CARTESIAN_POINT ( 'NONE',  ( -1.049868766404198794, 0.2306618581243847221, -0.2411417322834647770 ) ) ;
#81613 = ADVANCED_FACE ( 'NONE', ( #38801 ), #4101, .F. ) ;
#81614 = CARTESIAN_POINT ( 'NONE',  ( 0.2891555358219910499, -0.2891555358219909944, -2.222440944881889813 ) ) ;
#81615 = CARTESIAN_POINT ( 'NONE',  ( 1.266404199475066328, -0.08942795157527998196, 0.3641732283464567121 ) ) ;
#81616 = CARTESIAN_POINT ( 'NONE',  ( -0.1443569553805768291, -0.004921259842519576551, 0.3153832671262227771 ) ) ;
#81617 = CARTESIAN_POINT ( 'NONE',  ( 1.056430446194226658, 0.1771653543307087630, 0.09757992244046791164 ) ) ;
#81618 = CARTESIAN_POINT ( 'NONE',  ( -1.574803149606298636, -0.1870078740157479769, 0.4822834645669291653 ) ) ;
#81619 = CARTESIAN_POINT ( 'NONE',  ( -1.049868766404198794, -0.5023911411419708095, 0.1820866141732285504 ) ) ;
#81620 = DIRECTION ( 'NONE',  ( -0.000000000000000000, -1.000000000000000000, -0.000000000000000000 ) ) ;
#81621 = CARTESIAN_POINT ( 'NONE',  ( 0.6430446194225729606, -0.3690944881889765550, -0.3153832671262227771 ) ) ;
#81622 = CARTESIAN_POINT ( 'NONE',  ( -0.2952755905511803003, -0.5400638737290845981, -0.3530559997133363437 ) ) ;
#81623 = EDGE_CURVE ( 'NONE', #36505, #41893, #15044, .T. ) ;
#81624 = CARTESIAN_POINT ( 'NONE',  ( 0.2493438320209980519, 0.05413385826771666132, 0.4176697321401328100 ) ) ;
#81625 = CARTESIAN_POINT ( 'NONE',  ( -0.2690288713910754526, -0.5511811023622046335, 0.09757992244046803654 ) ) ;
#81626 = B_SPLINE_CURVE_WITH_KNOTS ( 'NONE', 3,
 ( #6849, #51441, #77144, #45129 ),
 .UNSPECIFIED., .F., .F.,
 ( 4, 4 ),
 ( 1.999999999927407068E-07, 0.006970199999999936863 ),
 .UNSPECIFIED. ) ;
#81627 = CYLINDRICAL_SURFACE ( 'NONE', #72194, 0.4724409448818898682 ) ;
#81628 = CARTESIAN_POINT ( 'NONE',  ( 0.8595800524934390507, -0.3162353388693405765, 0.4822834645669290543 ) ) ;
#81629 = FACE_OUTER_BOUND ( 'NONE', #57535, .T. ) ;
#81630 = CARTESIAN_POINT ( 'NONE',  ( 1.181102362204724976, -0.1870078740157480601, -0.3641732283464567677 ) ) ;
#81631 = CARTESIAN_POINT ( 'NONE',  ( -0.9383202099737524282, -0.05778040916215522460, 0.4822834645669289988 ) ) ;
#81632 = CARTESIAN_POINT ( 'NONE',  ( -0.2690288713910754526, -0.5511811023622046335, 0.09757992244046803654 ) ) ;
#81633 = CARTESIAN_POINT ( 'NONE',  ( -0.7426113562971994320, 1.972848275015058439, 0.5309055118110236338 ) ) ;
#81634 = CARTESIAN_POINT ( 'NONE',  ( 0.3805774278215230400, -0.004921259842519870586, -0.3153832671262229437 ) ) ;
#81635 = CONICAL_SURFACE ( 'NONE', #77597, 0.1190944881889763746, 0.8726646259971653219 ) ;
#81636 = CARTESIAN_POINT ( 'NONE',  ( -0.3280839895013117347, 0.05413385826771626580, -0.4176697321401330321 ) ) ;
#81637 = CARTESIAN_POINT ( 'NONE',  ( -0.3996062992125984925, -0.1070741851644056858, -0.5951443569553805935 ) ) ;
#81638 = AXIS2_PLACEMENT_3D ( 'NONE', #18049, #29829, #80789 ) ;
#81639 = CARTESIAN_POINT ( 'NONE',  ( 0.1049643490035304938, -0.3917322834645669549, -2.217191601049868677 ) ) ;
#81640 = CARTESIAN_POINT ( 'NONE',  ( 0.7020997375328090762, -0.08942795157528024563, -0.3641732283464568787 ) ) ;
#81642 = AXIS2_PLACEMENT_3D ( 'NONE', #49863, #4023, #61682 ) ;
#81641 = CARTESIAN_POINT ( 'NONE',  ( -0.2690288713910754526, -0.6692913385826771977, 0.1292274648535927661 ) ) ;
#81643 = CARTESIAN_POINT ( 'NONE',  ( -0.8727034120734901146, -0.3162353388693405765, 0.4822834645669290543 ) ) ;
#81644 = CARTESIAN_POINT ( 'NONE',  ( -0.8727034120734901146, -0.2845877964562159024, 0.3641732283464567677 ) ) ;
#81645 = DIRECTION ( 'NONE',  ( -1.000000000000000000, -3.083952846180990774E-16, 0.000000000000000000 ) ) ;
#81646 = CARTESIAN_POINT ( 'NONE',  ( -0.1902887139107604098, 0.2952755905511810774, -0.1292274648535930714 ) ) ;
#81647 = CARTESIAN_POINT ( 'NONE',  ( -1.181102362204723644, -0.1870078740157480601, -0.3641732283464567677 ) ) ;
#81648 = CARTESIAN_POINT ( 'NONE',  ( -1.581364829396324945, -0.05778040916215560624, -0.4822834645669293319 ) ) ;
#81649 = CARTESIAN_POINT ( 'NONE',  ( -0.2362204724409451284, 0.4091458600556402425, -2.609580052493438274 ) ) ;
#81650 = ORIENTED_EDGE ( 'NONE', *, *, #32101, .F. ) ;
#81651 = CARTESIAN_POINT ( 'NONE',  ( -1.377952755905511140, 0.1771653543307087630, 0.000000000000000000 ) ) ;
#81652 = CARTESIAN_POINT ( 'NONE',  ( -1.338582677165353729, -0.1870078740157480879, -0.4822834645669291653 ) ) ;
#81653 = CARTESIAN_POINT ( 'NONE',  ( -0.5446194225721777693, -0.3162353388693409650, -0.4822834645669289433 ) ) ;
#81654 = CARTESIAN_POINT ( 'NONE',  ( -1.102362204724408601, -0.1870078740157480879, -0.4822834645669291653 ) ) ;
#81655 = CARTESIAN_POINT ( 'NONE',  ( -0.2867679344610365999, 0.2867679344610364889, -1.364173228346456268 ) ) ;
#81656 = CARTESIAN_POINT ( 'NONE',  ( 0.08989863709126331981, 0.3814249188612193198, -1.220472440944881942 ) ) ;
#81657 = CARTESIAN_POINT ( 'NONE',  ( 0.9776902887139113929, -0.6692913385826773087, -0.1292274648535924053 ) ) ;
#81658 = CARTESIAN_POINT ( 'NONE',  ( 0.4396325459317593221, 0.2952755905511810774, -0.1292274648535930714 ) ) ;
#81659 = CARTESIAN_POINT ( 'NONE',  ( 0.5314960629920989499, 2.755905511811024056, 2.583694225513486042 ) ) ;
#81660 = CARTESIAN_POINT ( 'NONE',  ( -0.3996062992125985480, -7.340648628747423112E-17, -2.478346456692913868 ) ) ;
#81661 = CARTESIAN_POINT ( 'NONE',  ( 1.220472440944882386, -0.5511811023622047445, 6.969142054262312111E-17 ) ) ;
#81662 = EDGE_CURVE ( 'NONE', #2979, #51375, #19442, .T. ) ;
#81663 = CARTESIAN_POINT ( 'NONE',  ( -0.1070741851644056997, 0.3996062992125986035, -0.9514435695538056015 ) ) ;
#81664 = ORIENTED_EDGE ( 'NONE', *, *, #49134, .F. ) ;
#81665 = CARTESIAN_POINT ( 'NONE',  ( -0.9514435695538050464, -0.08942795157528024563, -0.3641732283464568787 ) ) ;
#81666 = CARTESIAN_POINT ( 'NONE',  ( -0.3392501089628019995, 0.1958661417322832277, -2.695538057742782101 ) ) ;
#81667 = ORIENTED_EDGE ( 'NONE', *, *, #30238, .F. ) ;
#81668 = CARTESIAN_POINT ( 'NONE',  ( 0.2165354330708668673, 0.1660481256975883668, -0.3530559997133364547 ) ) ;
#81669 = CARTESIAN_POINT ( 'NONE',  ( -0.3740157480314953431, -0.5400638737290845981, -0.3530559997133363437 ) ) ;
#81670 = CARTESIAN_POINT ( 'NONE',  ( -1.115485564304461219, 0.05413385826771626580, -0.4176697321401330321 ) ) ;
#81671 = CARTESIAN_POINT ( 'NONE',  ( 1.253280839895013710, -0.05778040916215560624, -0.4822834645669293319 ) ) ;
#81672 = CARTESIAN_POINT ( 'NONE',  ( 1.561679790026247350, 0.05413385826771626580, -0.4176697321401330321 ) ) ;
#81673 = CARTESIAN_POINT ( 'NONE',  ( 0.09023630363248136277, 7.699586553780600482E-16, 0.3791483426435171555 ) ) ;
#81674 = CARTESIAN_POINT ( 'NONE',  ( -0.1246719160104980823, -0.6692913385826773087, -0.1292274648535924053 ) ) ;
#81675 = CARTESIAN_POINT ( 'NONE',  ( -1.358267716535432434, -0.5400638737290844871, 0.3530559997133364547 ) ) ;
#81676 = CARTESIAN_POINT ( 'NONE',  ( -0.2867679344610366554, 0.2867679344610365444, -1.989481996554119059 ) ) ;
#81677 = CARTESIAN_POINT ( 'NONE',  ( -1.456692913385826182, 0.2952755905511811885, 0.000000000000000000 ) ) ;
#81678 = DIRECTION ( 'NONE',  ( -3.114085624724525612E-16, 1.000000000000000000, 5.270319453084425600E-32 ) ) ;
#81679 = CARTESIAN_POINT ( 'NONE',  ( 0.1958661417322834775, 0.3392501089628018884, 0.02099737532808403431 ) ) ;
#81680 = CARTESIAN_POINT ( 'NONE',  ( 0.7545931758530189937, 0.1771653543307087075, -0.09757992244046823083 ) ) ;
#81681 = ORIENTED_EDGE ( 'NONE', *, *, #302, .T. ) ;
#81682 = CARTESIAN_POINT ( 'NONE',  ( 0.3949938075777409408, 0.1058382717557500574, -0.1246719160104987345 ) ) ;
#81683 = CARTESIAN_POINT ( 'NONE',  ( -1.043307086614172041, -0.5400638737290844871, 0.3530559997133364547 ) ) ;
#81684 = ORIENTED_EDGE ( 'NONE', *, *, #47141, .F. ) ;
#81685 = CARTESIAN_POINT ( 'NONE',  ( -0.07874015748031421014, -0.1870078740157480601, -0.3641732283464567677 ) ) ;
#81686 = CARTESIAN_POINT ( 'NONE',  ( -1.607611548556429737, -0.6692913385826771977, 0.1292274648535927661 ) ) ;
#81687 = CARTESIAN_POINT ( 'NONE',  ( 0.5511811023622054106, -0.1870078740157480879, -0.4822834645669291653 ) ) ;
#81688 = CARTESIAN_POINT ( 'NONE',  ( 0.4790026246719167324, -0.05778040916215522460, 0.4822834645669289988 ) ) ;
#81689 = CARTESIAN_POINT ( 'NONE',  ( -0.4790026246719154557, -0.3162353388693405765, 0.4822834645669290543 ) ) ;
#81690 = CARTESIAN_POINT ( 'NONE',  ( -0.2867679344610365444, -0.2867679344610367664, -1.158155798721471896 ) ) ;
#81691 = CARTESIAN_POINT ( 'NONE',  ( -0.7874015748031489847, -0.1870078740157480879, -0.4822834645669291653 ) ) ;
#81692 = CARTESIAN_POINT ( 'NONE',  ( -0.2867679344610365999, 0.2867679344610364889, -2.466535433070865757 ) ) ;
#81693 = CARTESIAN_POINT ( 'NONE',  ( 1.509186351706037543, -0.3690944881889765550, -0.3153832671262227771 ) ) ;
#81694 = CARTESIAN_POINT ( 'NONE',  ( -1.036745406824146176, -0.4281496062992124485, 0.4176697321401328655 ) ) ;
#81695 = CARTESIAN_POINT ( 'NONE',  ( 0.7480314960629927956, 0.2952755905511811885, 0.000000000000000000 ) ) ;
#81696 = CARTESIAN_POINT ( 'NONE',  ( 1.010498687664042716, -0.4281496062992124485, 0.4176697321401328655 ) ) ;
#81697 = CARTESIAN_POINT ( 'NONE',  ( -0.1998031496062994683, 0.3460692066303958092, -0.8005249343832020470 ) ) ;
#81698 = CARTESIAN_POINT ( 'NONE',  ( -1.522309711286088607, 0.2306618581243847221, -0.2411417322834647770 ) ) ;
#81699 = CARTESIAN_POINT ( 'NONE',  ( 0.3460692066303958092, 0.1998031496062993018, -0.3654855643044619407 ) ) ;
#81700 = CARTESIAN_POINT ( 'NONE',  ( 0.4527559055118117182, -0.5400638737290844871, 0.3530559997133364547 ) ) ;
#81701 = CARTESIAN_POINT ( 'NONE',  ( -0.1070741851644051862, -0.3996062992125987146, -2.434383202099737353 ) ) ;
#81702 = CIRCLE ( 'NONE', #9118, 0.5118110236220471121 ) ;
#81703 = CARTESIAN_POINT ( 'NONE',  ( -1.548556430446193399, -0.5023911411419708095, -0.1820866141732282451 ) ) ;
#81704 = CARTESIAN_POINT ( 'NONE',  ( 0.7808398950131241190, -0.08942795157528024563, -0.3641732283464568787 ) ) ;
#81705 = CARTESIAN_POINT ( 'NONE',  ( 0.9711286089238851948, 0.2306618581243848609, 0.2411417322834645549 ) ) ;
#81706 = CARTESIAN_POINT ( 'NONE',  ( -0.3458507752293906723, -0.3458507752293910609, -1.080708661417322691 ) ) ;
#81707 = CARTESIAN_POINT ( 'NONE',  ( 0.7020997375328090762, -0.2845877964562159024, 0.3641732283464567677 ) ) ;
#81708 = CARTESIAN_POINT ( 'NONE',  ( 0.5052493438320215802, 0.2952755905511811885, 0.1292274648535926551 ) ) ;
#81709 = CARTESIAN_POINT ( 'NONE',  ( -0.1974969037888704149, -0.3420746716998661063, -0.9297900262467193588 ) ) ;
#81710 = CARTESIAN_POINT ( 'NONE',  ( -0.7020997375328076329, -0.3162353388693409650, -0.4822834645669289433 ) ) ;
#81711 = CARTESIAN_POINT ( 'NONE',  ( -3.224202737261815166, 2.716535433070866645, -0.5314960629921260393 ) ) ;
#81712 = CARTESIAN_POINT ( 'NONE',  ( 1.135170603674541256, 0.1771653543307087630, 0.09757992244046791164 ) ) ;
#81713 = CARTESIAN_POINT ( 'NONE',  ( -0.05905511811023545637, -0.5400638737290845981, -0.3530559997133363437 ) ) ;
#81714 = CARTESIAN_POINT ( 'NONE',  ( -3.937007874015748143, 2.755905511811024056, 0.5314960629921260393 ) ) ;
#81715 = CARTESIAN_POINT ( 'NONE',  ( -0.4986876640419942164, -0.6046776061558807314, 0.2411417322834647770 ) ) ;
#81716 = CARTESIAN_POINT ( 'NONE',  ( 0.3083989501312343062, -0.08942795157528024563, -0.3641732283464568787 ) ) ;
#81717 = CARTESIAN_POINT ( 'NONE',  ( -2.571327113428939715, 1.453547212638086172, 0.4672029448317639444 ) ) ;
#81718 = CARTESIAN_POINT ( 'NONE',  ( 0.04593175853018440641, -0.5511811023622046335, 0.09757992244046803654 ) ) ;
#81719 = CARTESIAN_POINT ( 'NONE',  ( 0.7545931758530188826, -0.5511811023622046335, 0.09757992244046803654 ) ) ;
#81720 = CARTESIAN_POINT ( 'NONE',  ( -0.08327261094992825796, 1.070339138594046835, -1.465778323607621392 ) ) ;
#81721 = CARTESIAN_POINT ( 'NONE',  ( 0.3460692066303959202, -0.1998031496062991630, -1.756561679790026309 ) ) ;
#81722 = CARTESIAN_POINT ( 'NONE',  ( 0.2362204724409456558, -0.1870078740157479769, 0.4822834645669291653 ) ) ;
#81723 = CARTESIAN_POINT ( 'NONE',  ( 0.3917322834645669549, 0.1049643490035304660, -1.376640419947506189 ) ) ;
#81724 = CARTESIAN_POINT ( 'NONE',  ( 1.377952755905512472, 0.1771653543307087630, 0.000000000000000000 ) ) ;
#81725 = CARTESIAN_POINT ( 'NONE',  ( -1.313877454013331780, 1.062992125984252079, 0.6999040823587869831 ) ) ;
#81726 = CARTESIAN_POINT ( 'NONE',  ( -0.4133858267716528645, 0.07958543189024071263, -0.2665933059059888421 ) ) ;
#81727 = CARTESIAN_POINT ( 'NONE',  ( -0.3871391076115479057, -0.2845877964562161244, -0.3641732283464567121 ) ) ;
#81728 = CARTESIAN_POINT ( 'NONE',  ( -0.4133858267716528645, -0.5400638737290844871, 0.3530559997133364547 ) ) ;
#81729 = CARTESIAN_POINT ( 'NONE',  ( 0.7939632545931766261, -0.2845877964562161244, -0.3641732283464567121 ) ) ;
#81730 = CARTESIAN_POINT ( 'NONE',  ( 0.2895113455958823745, 1.161258846611464834, -1.084123980916873231 ) ) ;
#81731 = CARTESIAN_POINT ( 'NONE',  ( -1.712598425196849572, 0.1660481256975885056, 0.3530559997133364547 ) ) ;
#81732 = CARTESIAN_POINT ( 'NONE',  ( 0.03280839895013198948, -0.6692913385826773087, -0.1292274648535924053 ) ) ;
#81733 = CARTESIAN_POINT ( 'NONE',  ( 1.371391076115485941, 0.2952755905511811885, 0.1292274648535926551 ) ) ;
#81734 = CARTESIAN_POINT ( 'NONE',  ( 0.4744094488189052328, 1.537401574803149984, -2.170146923806634653 ) ) ;
#81735 = CARTESIAN_POINT ( 'NONE',  ( 0.2034120734908142214, 0.2952755905511810774, -0.1292274648535930714 ) ) ;
#81736 = CARTESIAN_POINT ( 'NONE',  ( 0.3917322834645670104, 2.398668435337828261E-17, -1.147637795275590733 ) ) ;
#81737 = CARTESIAN_POINT ( 'NONE',  ( 0.7283464566929143125, 0.1660481256975885056, 0.3530559997133364547 ) ) ;
#81738 = CARTESIAN_POINT ( 'NONE',  ( 0.7611548556430454138, 0.2306618581243847221, -0.2411417322834647770 ) ) ;
#81739 = CARTESIAN_POINT ( 'NONE',  ( -1.572991167713776672, 2.401574803149606474, -0.1227090857360982196 ) ) ;
#81740 = CARTESIAN_POINT ( 'NONE',  ( 0.6889763779527566800, -0.4536011799217367080, 0.2665933059059888421 ) ) ;
#81741 = CARTESIAN_POINT ( 'NONE',  ( 1.167979002624672580, -0.4281496062992124485, 0.4176697321401328655 ) ) ;
#81742 = CARTESIAN_POINT ( 'NONE',  ( -0.08530183727034056085, -0.08942795157528024563, -0.3641732283464568787 ) ) ;
#81743 = CARTESIAN_POINT ( 'NONE',  ( -0.3543307086614165824, 0.2952755905511811885, 0.000000000000000000 ) ) ;
#81744 = CARTESIAN_POINT ( 'NONE',  ( 0.1771653543307093182, 0.1660481256975885056, 0.3530559997133364547 ) ) ;
#81745 = CARTESIAN_POINT ( 'NONE',  ( -0.7414698162729651543, -0.6692913385826771977, 0.1292274648535927661 ) ) ;
#81746 = CARTESIAN_POINT ( 'NONE',  ( -0.3674540682414692561, -0.5023911411419708095, -0.1820866141732282451 ) ) ;
#81747 = CARTESIAN_POINT ( 'NONE',  ( 0.9580052493438326877, 0.05413385826771666132, 0.4176697321401328100 ) ) ;
#81748 = CARTESIAN_POINT ( 'NONE',  ( 0.9251968503937015864, 0.07958543189024071263, -0.2665933059059888421 ) ) ;
#81749 = CARTESIAN_POINT ( 'NONE',  ( 0.2559055118110243332, 0.1660481256975885056, 0.3530559997133364547 ) ) ;
#81750 = CARTESIAN_POINT ( 'NONE',  ( 1.148293963254593653, 0.2066929133858267098, -0.1054918080437494132 ) ) ;
#81752 = CARTESIAN_POINT ( 'NONE',  ( -0.1998031496062994683, 0.3460692066303958092, -1.115485564304461885 ) ) ;
#81751 = PLANE ( 'NONE',  #31176 ) ;
#81753 = CARTESIAN_POINT ( 'NONE',  ( 1.594488188976378673, -0.5400638737290845981, -0.3530559997133363437 ) ) ;
#81754 = CARTESIAN_POINT ( 'NONE',  ( -9.594673741351313045E-17, 0.3917322834645670104, -2.039370078740157410 ) ) ;
#81755 = VECTOR ( 'NONE', #64746, 39.37007874015748143 ) ;
#81756 = CARTESIAN_POINT ( 'NONE',  ( -1.299212598425196097, 0.2952755905511811885, 0.000000000000000000 ) ) ;
#81757 = CARTESIAN_POINT ( 'NONE',  ( -0.9711286089238838626, -0.6046776061558807314, 0.2411417322834647770 ) ) ;
#81758 = CARTESIAN_POINT ( 'NONE',  ( -0.1265901696524986964, -0.4724409448818899238, -0.2296587926509186250 ) ) ;
#81759 = CARTESIAN_POINT ( 'NONE',  ( 0.3949938075777411073, -0.1058382717557499464, -2.946194225721785909 ) ) ;
#81760 = ORIENTED_EDGE ( 'NONE', *, *, #6471, .F. ) ;
#81761 = CARTESIAN_POINT ( 'NONE',  ( 0.4855643044619430415, -0.3690944881889765550, -0.3153832671262227771 ) ) ;
#81762 = CARTESIAN_POINT ( 'NONE',  ( 0.3392501089628018884, -0.1958661417322834220, -1.356955380577427928 ) ) ;
#81763 = CARTESIAN_POINT ( 'NONE',  ( 0.5183727034120741983, 0.2952755905511810774, -0.1292274648535930714 ) ) ;
#81764 = CARTESIAN_POINT ( 'NONE',  ( 0.1265901696524989462, 0.4724409448818897572, -2.670603674540682260 ) ) ;
#81765 = CARTESIAN_POINT ( 'NONE',  ( 0.1265901696524989184, 0.4724409448818898127, -0.8576115485564304031 ) ) ;
#81766 = CARTESIAN_POINT ( 'NONE',  ( -1.581364829396324945, -0.2845877964562159024, 0.3641732283464567677 ) ) ;
#81767 = CARTESIAN_POINT ( 'NONE',  ( 1.312335958005250269, -0.6046776061558807314, 0.2411417322834647770 ) ) ;
#81768 = CARTESIAN_POINT ( 'NONE',  ( 1.417322834645670104, -0.1870078740157479769, 0.3641732283464567677 ) ) ;
#81769 = CARTESIAN_POINT ( 'NONE',  ( -0.03280839895013062252, 0.2952755905511810774, -0.1292274648535930714 ) ) ;
#81770 = CARTESIAN_POINT ( 'NONE',  ( -0.1958661417322834497, -0.3392501089628018884, -0.7755712353992633146 ) ) ;
#81771 = CARTESIAN_POINT ( 'NONE',  ( -0.4921259842519677963, 0.1660481256975883668, -0.3530559997133364547 ) ) ;
#81772 = CARTESIAN_POINT ( 'NONE',  ( -0.9251968503937002541, 0.07958543189024085140, 0.2665933059059887866 ) ) ;
#81773 = CARTESIAN_POINT ( 'NONE',  ( 0.4527559055118117182, -0.5400638737290844871, 0.3530559997133364547 ) ) ;
#81774 = CARTESIAN_POINT ( 'NONE',  ( -0.6824146981627291497, -0.6046776061558809534, -0.2411417322834644161 ) ) ;
#81775 = DIRECTION ( 'NONE',  ( -0.000000000000000000, 1.000000000000000000, -0.000000000000000000 ) ) ;
#81776 = CARTESIAN_POINT ( 'NONE',  ( 0.6889763779527560139, 0.000000000000000000, 0.000000000000000000 ) ) ;
#81777 = ORIENTED_EDGE ( 'NONE', *, *, #43470, .F. ) ;
#81778 = CARTESIAN_POINT ( 'NONE',  ( -0.3917322834645670104, -0.1049643490035307020, -2.247394643865828545 ) ) ;
#81779 = CARTESIAN_POINT ( 'NONE',  ( 0.2493438320209980519, 0.05413385826771666132, 0.4176697321401328100 ) ) ;
#81780 = CARTESIAN_POINT ( 'NONE',  ( -0.3412073490813641308, -0.6046776061558807314, 0.2411417322834647770 ) ) ;
#81781 = CARTESIAN_POINT ( 'NONE',  ( -1.515748031496062076, -0.5400638737290844871, 0.3530559997133364547 ) ) ;
#81782 = CARTESIAN_POINT ( 'NONE',  ( 0.7545931758530188826, -0.6692913385826771977, 0.1292274648535927661 ) ) ;
#81783 = CARTESIAN_POINT ( 'NONE',  ( 0.4724409448818904789, -0.1870078740157480879, -0.4822834645669291653 ) ) ;
#81784 = CARTESIAN_POINT ( 'NONE',  ( -0.3917322834645670104, -7.196005306013484475E-17, -1.541338582677165503 ) ) ;
#81785 = CARTESIAN_POINT ( 'NONE',  ( -0.7611548556430438595, 0.2306618581243848609, 0.2411417322834645549 ) ) ;
#81786 = CARTESIAN_POINT ( 'NONE',  ( 0.2427821522309719648, -0.05778040916215522460, 0.4822834645669289988 ) ) ;
#81787 = CARTESIAN_POINT ( 'NONE',  ( -0.3018372703412066094, -0.4281496062992127816, -0.4176697321401328100 ) ) ;
#81788 = CARTESIAN_POINT ( 'NONE',  ( 0.1049868766404206816, 0.1283753931104748280, 0.1820866141732283561 ) ) ;
#81789 = CARTESIAN_POINT ( 'NONE',  ( 1.653543307086614789, -0.1870078740157479769, 0.3641732283464567677 ) ) ;
#81790 = CARTESIAN_POINT ( 'NONE',  ( -0.2845468109762787079, -0.07963338598832103710, 5.543284456214096600 ) ) ;
#81791 = CARTESIAN_POINT ( 'NONE',  ( -0.1049868766404193215, 0.2306618581243847221, -0.2411417322834647770 ) ) ;
#81792 = CARTESIAN_POINT ( 'NONE',  ( 3.908418136489574923, 1.569398530225769139, -0.4736046740121441778 ) ) ;
#81793 = CARTESIAN_POINT ( 'NONE',  ( -1.601049868766403650, 0.2306618581243847221, -0.2411417322834647770 ) ) ;
#81794 = CARTESIAN_POINT ( 'NONE',  ( 0.1958661417322834775, 0.3392501089628018884, -2.656167979002624691 ) ) ;
#81795 = ORIENTED_EDGE ( 'NONE', *, *, #13007, .F. ) ;
#81796 = VERTEX_POINT ( 'NONE', #67219 ) ;
#81797 = CARTESIAN_POINT ( 'NONE',  ( 0.6889763779527566800, -0.5400638737290844871, 0.3530559997133364547 ) ) ;
#81798 = CARTESIAN_POINT ( 'NONE',  ( 0.2099737532808405305, 0.1283753931104746893, -0.1820866141732285504 ) ) ;
#81800 = DIRECTION ( 'NONE',  ( 1.047444401652940007E-14, -0.000000000000000000, -1.000000000000000000 ) ) ;
#81799 = CARTESIAN_POINT ( 'NONE',  ( 0.6175017169405826456, 2.784432375088962958E-17, -0.3464511005275205946 ) ) ;
#81801 = CARTESIAN_POINT ( 'NONE',  ( -0.3917322834645670104, -7.196005306013484475E-17, -0.5964566929133858775 ) ) ;
#81802 = CARTESIAN_POINT ( 'NONE',  ( 0.4091458600556404646, -0.2362204724409448231, 0.1332020997375328031 ) ) ;
#81803 = CARTESIAN_POINT ( 'NONE',  ( -0.2925321140481930149, -0.2925321140481933480, -2.340551181102362488 ) ) ;
#81804 = CARTESIAN_POINT ( 'NONE',  ( 0.3937007874015754361, -0.1870078740157480879, -0.4822834645669291653 ) ) ;
#81805 = CARTESIAN_POINT ( 'NONE',  ( -1.397637795275589623, -0.5400638737290845981, -0.3530559997133363437 ) ) ;
#81806 = CARTESIAN_POINT ( 'NONE',  ( -1.240157480314959759, 0.1660481256975885056, 0.3530559997133364547 ) ) ;
#81807 = CARTESIAN_POINT ( 'NONE',  ( 0.7480314960629927956, -0.6692913385826771977, 8.415575281601705876E-17 ) ) ;
#81808 = CARTESIAN_POINT ( 'NONE',  ( 1.318897637795276356, 0.1660481256975883668, -0.3530559997133364547 ) ) ;
#81809 = CARTESIAN_POINT ( 'NONE',  ( 1.299212598425197429, -0.5511811023622047445, 6.969142054262312111E-17 ) ) ;
#81810 = ITEM_DEFINED_TRANSFORMATION ( 'NONE', 'NONE', #32909,  #22098 ) ;
#81811 = CARTESIAN_POINT ( 'NONE',  ( 1.062992125984252745, 0.1771653543307087630, 0.000000000000000000 ) ) ;
#81812 = CARTESIAN_POINT ( 'NONE',  ( -0.9973753280839886548, 0.2306618581243848609, 0.2411417322834645549 ) ) ;
#81813 = CARTESIAN_POINT ( 'NONE',  ( -0.3460692066303957537, -0.1998031496062994405, -0.2867454068241469534 ) ) ;
#81814 = CARTESIAN_POINT ( 'NONE',  ( 1.391076115485564868, 0.2306618581243847221, -0.2411417322834647770 ) ) ;
#81815 = B_SPLINE_CURVE_WITH_KNOTS ( 'NONE', 3,
 ( #10697, #24129, #67112, #80993, #54881, #11104, #49798, #49391 ),
 .UNSPECIFIED., .F., .F.,
 ( 4, 2, 2, 4 ),
 ( 0.04257512569008879699, 0.04378708032589691268, 0.04499903496170502837, 0.04742294423332127362 ),
 .UNSPECIFIED. ) ;
#81816 = CARTESIAN_POINT ( 'NONE',  ( -0.1049643490035307020, 0.3917322834645669549, -0.1561679790026246351 ) ) ;
#81817 = CARTESIAN_POINT ( 'NONE',  ( -0.3018372703412066094, -0.4281496062992127816, -0.4176697321401328100 ) ) ;
#81819 = FACE_OUTER_BOUND ( 'NONE', #13937, .T. ) ;
#81818 = CARTESIAN_POINT ( 'NONE',  ( 1.292650918635171564, -0.6692913385826773087, -0.1292274648535924053 ) ) ;
#81820 = CARTESIAN_POINT ( 'NONE',  ( -1.187664041994750175, -0.08942795157528024563, -0.3641732283464568787 ) ) ;
#81821 = CARTESIAN_POINT ( 'NONE',  ( 0.5643044619422579178, 0.05413385826771666132, 0.4176697321401328100 ) ) ;
#81822 = CARTESIAN_POINT ( 'NONE',  ( 0.8792650918635177559, -0.3690944881889765550, -0.3153832671262227771 ) ) ;
#81823 = CARTESIAN_POINT ( 'NONE',  ( 0.1958661417322834497, 0.3392501089628018329, -1.799193282643357428 ) ) ;
#81824 = CARTESIAN_POINT ( 'NONE',  ( -1.200787401574802349, 0.07958543189024071263, -0.2665933059059888421 ) ) ;
#81825 = CARTESIAN_POINT ( 'NONE',  ( 1.135170603674541256, -0.6692913385826773087, -0.1292274648535924053 ) ) ;
#81826 = CYLINDRICAL_SURFACE ( 'NONE', #30362, 0.1771653543307088186 ) ;
#81827 = CARTESIAN_POINT ( 'NONE',  ( -0.5643044619422565855, -0.004921259842519870586, -0.3153832671262229437 ) ) ;
#81828 = CARTESIAN_POINT ( 'NONE',  ( -0.6627296587926503335, -0.6692913385826771977, 0.1292274648535927661 ) ) ;
#81829 = CARTESIAN_POINT ( 'NONE',  ( -1.522309711286088607, -0.5023911411419708095, 0.1820866141732285504 ) ) ;
#81830 = CARTESIAN_POINT ( 'NONE',  ( -0.5446194225721777693, -0.3162353388693409650, -0.4822834645669289433 ) ) ;
#81831 = CARTESIAN_POINT ( 'NONE',  ( 1.404199475065617708, 0.05413385826771626580, -0.4176697321401330321 ) ) ;
#81832 = CARTESIAN_POINT ( 'NONE',  ( 0.2867679344610366554, 0.2867679344610366554, -0.7644550113198971264 ) ) ;
#81833 = CARTESIAN_POINT ( 'NONE',  ( -1.043307086614172041, -0.4536011799217367080, 0.2665933059059888421 ) ) ;
#81834 = CARTESIAN_POINT ( 'NONE',  ( -0.7330049731599687091, 2.221336660396680429, 0.5178675056769429519 ) ) ;
#81835 = CARTESIAN_POINT ( 'NONE',  ( 1.587926509186352142, 0.05413385826771666132, 0.4176697321401328100 ) ) ;
#81836 = CARTESIAN_POINT ( 'NONE',  ( -0.2362204724409451284, 0.4091458600556402425, -1.979658792650918597 ) ) ;
#81837 = CARTESIAN_POINT ( 'NONE',  ( -1.305774278215222184, -0.6692913385826773087, -0.1292274648535924053 ) ) ;
#81838 = CARTESIAN_POINT ( 'NONE',  ( -1.502624671916009680, -0.2845877964562159024, 0.3641732283464567677 ) ) ;
#81839 = CARTESIAN_POINT ( 'NONE',  ( -0.4461942257217840213, 0.1283753931104748280, 0.1820866141732283561 ) ) ;
#81840 = CARTESIAN_POINT ( 'NONE',  ( -0.5380577427821514602, 0.009842519685039467087, 0.3409548833797002021 ) ) ;
#81841 = CARTESIAN_POINT ( 'NONE',  ( -0.2887139107611542133, -0.6046776061558809534, -0.2411417322834644161 ) ) ;
#81842 = CARTESIAN_POINT ( 'NONE',  ( 0.02624671916010564918, -0.5023911411419708095, -0.1820866141732282451 ) ) ;
#81843 = CARTESIAN_POINT ( 'NONE',  ( -0.9580052493438311334, -0.3690944881889763329, 0.3153832671262228327 ) ) ;
#81844 = CARTESIAN_POINT ( 'NONE',  ( -1.371391076115484831, 0.2952755905511810774, -0.1292274648535930714 ) ) ;
#81845 = CARTESIAN_POINT ( 'NONE',  ( 1.463254593175853824, 0.1771653543307087075, -0.09757992244046823083 ) ) ;
#81846 = CARTESIAN_POINT ( 'NONE',  ( 0.9973753280839902091, -0.6046776061558807314, 0.2411417322834647770 ) ) ;
#81847 = CARTESIAN_POINT ( 'NONE',  ( 0.06850640440391080055, 1.067651707476381606, 1.854710246793788819 ) ) ;
#81848 = CARTESIAN_POINT ( 'NONE',  ( 0.2690288713910767848, 0.1771653543307087630, 0.09757992244046791164 ) ) ;
#81849 = CARTESIAN_POINT ( 'NONE',  ( 0.3674540682414705883, -0.6046776061558807314, 0.2411417322834647770 ) ) ;
#81850 = CARTESIAN_POINT ( 'NONE',  ( 0.9317585301837276734, -0.3690944881889763329, 0.3153832671262228327 ) ) ;
#81851 = ORIENTED_EDGE ( 'NONE', *, *, #59902, .T. ) ;
#81852 = CARTESIAN_POINT ( 'NONE',  ( -1.082677165354329896, -0.5400638737290845981, -0.3530559997133363437 ) ) ;
#81853 = EDGE_CURVE ( 'NONE', #57471, #71398, #75570, .T. ) ;
#81854 = CARTESIAN_POINT ( 'NONE',  ( -0.9055118110236215490, -0.6692913385826771977, 8.415575281601705876E-17 ) ) ;
#81855 = CARTESIAN_POINT ( 'NONE',  ( -0.1377952755905504645, 0.1660481256975885056, 0.3530559997133364547 ) ) ;
#81856 = CARTESIAN_POINT ( 'NONE',  ( -0.2925321140481932369, 0.2925321140481931259, -2.458661417322834719 ) ) ;
#81857 = CARTESIAN_POINT ( 'NONE',  ( 0.5183727034120741983, 0.2952755905511810774, -0.1292274648535930714 ) ) ;
#81858 = CARTESIAN_POINT ( 'NONE',  ( -1.719160104986876103, 0.05413385826771666132, 0.4176697321401328100 ) ) ;
#81859 = CARTESIAN_POINT ( 'NONE',  ( 0.1902887139107617975, -0.6692913385826773087, -0.1292274648535924053 ) ) ;
#81860 = CARTESIAN_POINT ( 'NONE',  ( 0.5708661417322841158, -0.5400638737290845981, -0.3530559997133363437 ) ) ;
#81861 = CARTESIAN_POINT ( 'NONE',  ( -0.3996062992125987146, 0.1070741851644051862, -2.395013123359580387 ) ) ;
#81862 = CARTESIAN_POINT ( 'NONE',  ( -9.674558042662121740E-17, 0.3949938075777409963, -1.574803149606299302 ) ) ;
#81863 = CARTESIAN_POINT ( 'NONE',  ( -0.3460692066303960868, 0.1998031496062990242, -2.703412073490813583 ) ) ;
#81864 = CARTESIAN_POINT ( 'NONE',  ( -1.840815010931731832, 2.729664643556220849, -0.5314960629921260393 ) ) ;
#81865 = CARTESIAN_POINT ( 'NONE',  ( 0.3392501089628018329, 0.1958661417322835607, -0.5958005249343831800 ) ) ;
#81866 = CARTESIAN_POINT ( 'NONE',  ( -0.3871391076115479057, -0.2845877964562161244, -0.3641732283464567121 ) ) ;
#81867 = CARTESIAN_POINT ( 'NONE',  ( -0.7217847769028863381, 0.05413385826771626580, -0.4176697321401330321 ) ) ;
#81868 = CARTESIAN_POINT ( 'NONE',  ( 0.4461942257217855201, -0.6046776061558807314, 0.2411417322834647770 ) ) ;
#81869 = CARTESIAN_POINT ( 'NONE',  ( -0.1974969037888706924, 0.3420746716998658843, -2.452099737532808632 ) ) ;
#81870 = CARTESIAN_POINT ( 'NONE',  ( 0.8070866141732289112, -0.5400638737290845981, -0.3530559997133363437 ) ) ;
#81871 = CARTESIAN_POINT ( 'NONE',  ( -1.496062992125983815, -0.1870078740157479769, 0.4822834645669291653 ) ) ;
#81872 = CARTESIAN_POINT ( 'NONE',  ( 0.7480314960629927956, -0.6692913385826771977, 8.415575281601705876E-17 ) ) ;
#81873 = CARTESIAN_POINT ( 'NONE',  ( 5.785732909357575061E-17, -0.4724409448818898682, -2.283464566929133799 ) ) ;
#81874 = CARTESIAN_POINT ( 'NONE',  ( -0.3996062992125986035, -7.340648628747425578E-17, -2.086614173228346303 ) ) ;
#81875 = CARTESIAN_POINT ( 'NONE',  ( 1.496062992125985147, -0.1870078740157479769, 0.4822834645669291653 ) ) ;
#81876 = CARTESIAN_POINT ( 'NONE',  ( 0.7545931758530188826, -0.6692913385826771977, 0.1292274648535927661 ) ) ;
#81877 = CARTESIAN_POINT ( 'NONE',  ( 0.4527559055118117182, -0.5400638737290844871, 0.3530559997133364547 ) ) ;
#81878 = CARTESIAN_POINT ( 'NONE',  ( 1.364829396325459854, -0.5023911411419708095, -0.1820866141732282451 ) ) ;
#81880 = CARTESIAN_POINT ( 'NONE',  ( -1.587926509186350810, 0.05413385826771626580, -0.4176697321401330321 ) ) ;
#81879 = CARTESIAN_POINT ( 'NONE',  ( 1.666666666666667185, 0.05413385826771666132, 0.4176697321401328100 ) ) ;
#81881 = CARTESIAN_POINT ( 'NONE',  ( -0.3392501089628017219, -0.1958661417322836718, 0.1778215223097112108 ) ) ;
#81882 = CARTESIAN_POINT ( 'NONE',  ( -3.924389226575468737, 2.165354330708661568, -0.3149606299212600047 ) ) ;
#81883 = CARTESIAN_POINT ( 'NONE',  ( 0.8989501312335964611, 0.2952755905511811885, 0.1292274648535926551 ) ) ;
#81884 = CARTESIAN_POINT ( 'NONE',  ( 1.489501312335958172, -0.2845877964562159024, 0.3641732283464567677 ) ) ;
#81885 = CARTESIAN_POINT ( 'NONE',  ( -0.3805774278215216522, -0.4281496062992127816, -0.4176697321401328100 ) ) ;
#81886 = CARTESIAN_POINT ( 'NONE',  ( -0.4724409448818890911, -0.1870078740157479769, 0.4822834645669291653 ) ) ;
#81887 = CARTESIAN_POINT ( 'NONE',  ( -1.561679790026246017, -0.4281496062992127816, -0.4176697321401328100 ) ) ;
#81888 = CARTESIAN_POINT ( 'NONE',  ( 0.2867679344610365999, 0.2867679344610365999, -0.3799212598425197318 ) ) ;
#81889 = CARTESIAN_POINT ( 'NONE',  ( -0.3392501089628017219, -0.1958661417322836718, -1.619422572178477848 ) ) ;
#81890 = CARTESIAN_POINT ( 'NONE',  ( -0.3392501089628017219, -0.1958661417322836718, -2.091863517060367439 ) ) ;
#81891 = CARTESIAN_POINT ( 'NONE',  ( 1.502624671916010790, -0.05778040916215522460, 0.4822834645669289988 ) ) ;
#81892 = ORIENTED_EDGE ( 'NONE', *, *, #79905, .F. ) ;
#81893 = CARTESIAN_POINT ( 'NONE',  ( 4.837279021331060870E-17, -0.3949938075777409963, -2.755905511811023167 ) ) ;
#81894 = ORIENTED_EDGE ( 'NONE', *, *, #18320, .F. ) ;
#81895 = LINE ( 'NONE', #81069, #1917 ) ;
#81896 = CARTESIAN_POINT ( 'NONE',  ( 1.574803149606299746, -0.1870078740157479769, 0.3641732283464567677 ) ) ;
#81897 = CARTESIAN_POINT ( 'NONE',  ( 0.2925321140481932369, -0.2925321140481932369, -1.358267716535433101 ) ) ;
#81898 = CARTESIAN_POINT ( 'NONE',  ( 0.5622787594981834003, 7.570362723507360306E-16, 0.3954985857520059711 ) ) ;
#81899 = CARTESIAN_POINT ( 'NONE',  ( 0.2362204724409449064, 0.000000000000000000, 0.000000000000000000 ) ) ;
#81900 = CARTESIAN_POINT ( 'NONE',  ( 0.4724409448818898682, 2.892866454678787531E-17, -0.1948818897637795422 ) ) ;
#81901 = CARTESIAN_POINT ( 'NONE',  ( -0.3122834589929986970, 1.651567687059297240, 0.02415997947403120821 ) ) ;
#81902 = CARTESIAN_POINT ( 'NONE',  ( 0.3917322834645669549, 0.1049643490035304660, -0.3667979002624672802 ) ) ;
#81903 = CARTESIAN_POINT ( 'NONE',  ( -0.8727034120734901146, -0.2845877964562159024, 0.3641732283464567677 ) ) ;
#81904 = CARTESIAN_POINT ( 'NONE',  ( -1.167979002624671470, -0.3690944881889765550, -0.3153832671262227771 ) ) ;
#81905 = CARTESIAN_POINT ( 'NONE',  ( 0.05249343832021075018, 0.2306618581243847221, -0.2411417322834647770 ) ) ;
#81906 = CARTESIAN_POINT ( 'NONE',  ( -1.318897637795274802, 0.1660481256975885056, 0.3530559997133364547 ) ) ;
#81907 = CARTESIAN_POINT ( 'NONE',  ( 0.2867679344610365999, 0.2867679344610365999, -0.1299212598425196485 ) ) ;
#81908 = EDGE_LOOP ( 'NONE', ( #63337, #26976, #77735, #44983 ) ) ;
#81909 = CARTESIAN_POINT ( 'NONE',  ( 1.463254593175853824, 0.2952755905511810774, -0.1292274648535930714 ) ) ;
#81910 = CARTESIAN_POINT ( 'NONE',  ( -1.115134929062664426, 0.004960608223778509643, -0.3437734562760191848 ) ) ;
#81911 =( NAMED_UNIT ( * ) PLANE_ANGLE_UNIT ( ) SI_UNIT ( $, .RADIAN. ) );
#81912 = CARTESIAN_POINT ( 'NONE',  ( 0.4091458600556404646, -0.2362204724409448231, -1.837270341207349000 ) ) ;
#81913 = LINE ( 'NONE', #49896, #39827 ) ;
#81914 = CARTESIAN_POINT ( 'NONE',  ( -0.4790026246719152336, -0.08942795157528024563, -0.3641732283464568787 ) ) ;
#81915 = CARTESIAN_POINT ( 'NONE',  ( 0.4724409448818897017, 0.1265901696524990294, -0.9120734908136483021 ) ) ;
#81916 = CARTESIAN_POINT ( 'NONE',  ( -1.332020997375327642, -0.05778040916215522460, 0.4822834645669289988 ) ) ;
#81917 = CARTESIAN_POINT ( 'NONE',  ( 0.9908136482939640111, -0.6692913385826771977, 0.1292274648535927661 ) ) ;
#81918 = ORIENTED_EDGE ( 'NONE', *, *, #33182, .F. ) ;
#81920 = CARTESIAN_POINT ( 'NONE',  ( -1.646051170424378096, 0.4405861044731112508, 0.5309055118110234117 ) ) ;
#81919 = LINE ( 'NONE', #24230, #23466 ) ;
#81921 = CARTESIAN_POINT ( 'NONE',  ( 1.607611548556431069, -0.6692913385826773087, -0.1292274648535924053 ) ) ;
#81922 = CARTESIAN_POINT ( 'NONE',  ( -1.371391076115484831, 0.2952755905511810774, -0.1292274648535930714 ) ) ;
#81923 = CARTESIAN_POINT ( 'NONE',  ( -0.2867679344610366554, 0.2867679344610365444, -0.5721591619084497315 ) ) ;
#81924 = CARTESIAN_POINT ( 'NONE',  ( 0.05905511811023681640, 0.07958543189024071263, -0.2665933059059888421 ) ) ;
#81925 = CARTESIAN_POINT ( 'NONE',  ( -0.1049643490035307020, 0.3917322834645669549, -1.036089238845144367 ) ) ;
#81926 = CARTESIAN_POINT ( 'NONE',  ( -0.1509186351706028884, -0.2845877964562161244, -0.3641732283464567121 ) ) ;
#81927 = CARTESIAN_POINT ( 'NONE',  ( 0.6233595800524939223, -0.2845877964562159024, 0.3641732283464567677 ) ) ;
#81928 = CARTESIAN_POINT ( 'NONE',  ( 0.6167979002624678353, -0.4281496062992124485, 0.4176697321401328655 ) ) ;
#81929 = CARTESIAN_POINT ( 'NONE',  ( -0.6430446194225712953, -0.004921259842519870586, -0.3153832671262229437 ) ) ;
#81930 = CARTESIAN_POINT ( 'NONE',  ( -0.1049643490035307020, 0.3917322834645669549, -2.360892388451444113 ) ) ;
#81931 = CARTESIAN_POINT ( 'NONE',  ( 1.292650918635171564, 0.2952755905511811885, 0.1292274648535926551 ) ) ;
#81932 = CARTESIAN_POINT ( 'NONE',  ( -0.9448818897637790704, -0.1870078740157480879, -0.4822834645669291653 ) ) ;
#81933 = CARTESIAN_POINT ( 'NONE',  ( -0.4091458600556405756, 0.2362204724409446288, -0.7329396325459317518 ) ) ;
#81934 = CARTESIAN_POINT ( 'NONE',  ( 0.03280839895013198948, 0.2952755905511811885, 0.1292274648535926551 ) ) ;
#81935 = CARTESIAN_POINT ( 'NONE',  ( -0.4461942257217840213, -0.6046776061558809534, -0.2411417322834644161 ) ) ;
#81936 = CARTESIAN_POINT ( 'NONE',  ( 1.135170603674541256, -0.5511811023622048555, -0.09757992244046775898 ) ) ;
#81937 = CARTESIAN_POINT ( 'NONE',  ( -0.04593175853018302557, -0.5511811023622048555, -0.09757992244046775898 ) ) ;
#81938 = CARTESIAN_POINT ( 'NONE',  ( -0.2165354330708654795, -0.5400638737290845981, -0.3530559997133363437 ) ) ;
#81939 = CARTESIAN_POINT ( 'NONE',  ( -0.9645669291338575535, 0.1660481256975883668, -0.3530559997133364547 ) ) ;
#81940 = CARTESIAN_POINT ( 'NONE',  ( -0.7186703366786194591, -2.567464376874931580E-15, -0.4445507791589072832 ) ) ;
#81941 = CARTESIAN_POINT ( 'NONE',  ( -0.1771653543307080136, 0.1660481256975883668, -0.3530559997133364547 ) ) ;
#81942 = VERTEX_POINT ( 'NONE', #42346 ) ;
#81943 = CARTESIAN_POINT ( 'NONE',  ( 4.893765752498283308E-17, -0.3996062992125985480, -2.045275590551181022 ) ) ;
#81944 = CARTESIAN_POINT ( 'NONE',  ( 1.167979002624672580, 0.05413385826771626580, -0.4176697321401330321 ) ) ;
#81945 = CARTESIAN_POINT ( 'NONE',  ( -0.8530183727034112984, -0.3690944881889765550, -0.3153832671262227771 ) ) ;
#81946 = CARTESIAN_POINT ( 'NONE',  ( -0.6233595800524928121, -0.05778040916215522460, 0.4822834645669289988 ) ) ;
#81947 = CARTESIAN_POINT ( 'NONE',  ( 1.437007874015748810, -0.5400638737290845981, -0.3530559997133363437 ) ) ;
#81948 = CARTESIAN_POINT ( 'NONE',  ( 0.9317585301837276734, 0.05413385826771626580, -0.4176697321401330321 ) ) ;
#81949 = DIRECTION ( 'NONE',  ( 0.000000000000000000, 0.000000000000000000, -1.000000000000000000 ) ) ;
#81950 = CARTESIAN_POINT ( 'NONE',  ( -1.108923884514435132, -0.2845877964562159024, 0.3641732283464567677 ) ) ;
#81951 = CARTESIAN_POINT ( 'NONE',  ( 0.3460692066303959202, -0.1998031496062991630, -0.8116797900262466836 ) ) ;
#81952 = CARTESIAN_POINT ( 'NONE',  ( -0.2925321140481930704, -0.2925321140481933480, -0.5314960629921260393 ) ) ;
#81953 = CARTESIAN_POINT ( 'NONE',  ( -0.2891555358219911054, 0.2891555358219909388, -0.1771653543307087630 ) ) ;
#81954 = CARTESIAN_POINT ( 'NONE',  ( 0.2472359589189098705, 1.132503624486270066, -1.510687062895181398 ) ) ;
#81955 = CARTESIAN_POINT ( 'NONE',  ( 0.9711286089238851948, -0.5023911411419708095, -0.1820866141732282451 ) ) ;
#81956 = CARTESIAN_POINT ( 'NONE',  ( 0.5314960629921264834, 0.07958543189024071263, -0.2665933059059888421 ) ) ;
#81957 = CARTESIAN_POINT ( 'NONE',  ( 0.3149606299212603933, -0.1870078740157479769, 0.4822834645669291653 ) ) ;
#81958 = FACE_OUTER_BOUND ( 'NONE', #36518, .T. ) ;
#81959 = CARTESIAN_POINT ( 'NONE',  ( -0.3420746716998662729, 0.1974969037888702206, -1.205380577427821454 ) ) ;
#81960 = CARTESIAN_POINT ( 'NONE',  ( 0.7086614173228353852, -0.1870078740157479769, 0.3641732283464567677 ) ) ;
#81961 = CARTESIAN_POINT ( 'NONE',  ( -0.1706036745406816491, 0.05413385826771626580, -0.4176697321401330321 ) ) ;
#81962 = CARTESIAN_POINT ( 'NONE',  ( -0.7217847769028863381, -0.4281496062992124485, 0.4176697321401328655 ) ) ;
#81963 = CARTESIAN_POINT ( 'NONE',  ( 1.443569553805774897, -0.6046776061558809534, -0.2411417322834644161 ) ) ;
#81964 = CARTESIAN_POINT ( 'NONE',  ( 0.4091458600556404646, -0.2362204724409448231, -1.049868766404199460 ) ) ;
#81965 = CARTESIAN_POINT ( 'NONE',  ( 0.1998031496062992740, 0.3460692066303959757, -2.191601049868766360 ) ) ;
#81966 = CARTESIAN_POINT ( 'NONE',  ( -0.1246719160104980823, 0.1771653543307087630, 0.09757992244046791164 ) ) ;
#81967 = VERTEX_POINT ( 'NONE', #3654 ) ;
#81968 = CARTESIAN_POINT ( 'NONE',  ( 0.3917322834645670659, -0.1049643490035303273, -0.7382082921597920011 ) ) ;
#81969 = ORIENTED_EDGE ( 'NONE', *, *, #16168, .F. ) ;
#81970 = CARTESIAN_POINT ( 'NONE',  ( -0.6955380577427815458, -0.4281496062992127816, -0.4176697321401328100 ) ) ;
#81971 = CARTESIAN_POINT ( 'NONE',  ( -0.2952755905511803003, -0.5400638737290845981, -0.3530559997133363437 ) ) ;
#81972 = CARTESIAN_POINT ( 'NONE',  ( -0.3412073490813641308, 0.2306618581243847221, -0.2411417322834647770 ) ) ;
#81973 = DIMENSIONAL_EXPONENTS ( 1.000000000000000000, 0.000000000000000000, 0.000000000000000000, 0.000000000000000000, 0.000000000000000000, 0.000000000000000000, 0.000000000000000000 ) ;
#81974 = CARTESIAN_POINT ( 'NONE',  ( 0.5839895013123367340, 0.2952755905511811885, 0.1292274648535926551 ) ) ;
#81975 = CARTESIAN_POINT ( 'NONE',  ( -0.4593175853018364174, -0.4281496062992127816, -0.4176697321401328100 ) ) ;
#81976 = CARTESIAN_POINT ( 'NONE',  ( -1.299212598425196097, 0.2952755905511811885, 0.000000000000000000 ) ) ;
#81977 = CARTESIAN_POINT ( 'NONE',  ( -0.6627296587926503335, -0.6692913385826771977, 0.1292274648535927661 ) ) ;
#81978 = CARTESIAN_POINT ( 'NONE',  ( 0.6233595800524939223, -0.3162353388693405765, 0.4822834645669290543 ) ) ;
#81979 = EDGE_CURVE ( 'NONE', #47474, #46955, #53730, .T. ) ;
#81980 = ADVANCED_FACE ( 'NONE', ( #73111 ), #41120, .F. ) ;
#81981 = CARTESIAN_POINT ( 'NONE',  ( -0.1049643490035302024, -0.3917322834645671215, -0.8517060367454066805 ) ) ;
#81982 = CARTESIAN_POINT ( 'NONE',  ( -0.3280839895013117347, -0.004921259842519870586, -0.3153832671262229437 ) ) ;
#81983 = EDGE_LOOP ( 'NONE', ( #37018, #36935, #73183, #79599 ) ) ;
#81984 = CARTESIAN_POINT ( 'NONE',  ( -0.2891555358219908833, -0.2891555358219912164, -1.318897637795275912 ) ) ;
#81985 = ORIENTED_EDGE ( 'NONE', *, *, #16394, .F. ) ;
#81986 = CARTESIAN_POINT ( 'NONE',  ( -1.456692913385826182, -0.5511811023622047445, 6.969142054262312111E-17 ) ) ;
#81987 = CARTESIAN_POINT ( 'NONE',  ( -0.9776902887139098386, 0.2952755905511810774, -0.1292274648535930714 ) ) ;
#81988 = CARTESIAN_POINT ( 'NONE',  ( -0.9776902887139098386, 0.2952755905511810774, -0.1292274648535930714 ) ) ;
#81989 = DIRECTION ( 'NONE',  ( 0.000000000000000000, 1.000000000000000000, 0.000000000000000000 ) ) ;
#81990 = CARTESIAN_POINT ( 'NONE',  ( -0.6955380577427815458, -0.4281496062992127816, -0.4176697321401328100 ) ) ;
#81991 = CARTESIAN_POINT ( 'NONE',  ( -0.8464566929133852113, -0.5400638737290845981, -0.3530559997133363437 ) ) ;
#81992 = LINE ( 'NONE', #70161, #55273 ) ;
#81993 = CARTESIAN_POINT ( 'NONE',  ( -0.4712111919743346422, 1.601159491416950242, -3.908712531853713479 ) ) ;
#81994 = CARTESIAN_POINT ( 'NONE',  ( 0.5839895013123367340, 0.1771653543307087630, 0.09757992244046791164 ) ) ;
#81995 = CARTESIAN_POINT ( 'NONE',  ( 0.4606732211681152100, 1.541615089183626441, 0.5309055118110234117 ) ) ;
#81996 = CARTESIAN_POINT ( 'NONE',  ( 0.1049643490035304938, -0.3917322834645669549, 0.1450131233595799429 ) ) ;
#81997 = CARTESIAN_POINT ( 'NONE',  ( 5.463695987328526437E-16, -0.1870078740157479769, 0.3641732283464567677 ) ) ;
#81998 = CARTESIAN_POINT ( 'NONE',  ( -0.4396325459317577122, -0.6692913385826773087, -0.1292274648535924053 ) ) ;
#81999 = CARTESIAN_POINT ( 'NONE',  ( 3.937010599584712001, 1.062969507148802562, 0.03102431951651077324 ) ) ;
#82000 = CARTESIAN_POINT ( 'NONE',  ( 0.09842519685039434474, 0.1660481256975885056, 0.3530559997133364547 ) ) ;
#82001 = ORIENTED_EDGE ( 'NONE', *, *, #35805, .T. ) ;
#82002 = CARTESIAN_POINT ( 'NONE',  ( -0.2925321140481932924, 0.2925321140481931814, -1.909448818897637512 ) ) ;
#82003 = CARTESIAN_POINT ( 'NONE',  ( 1.080276388343102000E-18, 0.000000000000000000, 0.000000000000000000 ) ) ;
#82004 = ORIENTED_EDGE ( 'NONE', *, *, #29595, .T. ) ;
#82005 = CARTESIAN_POINT ( 'NONE',  ( 0.1998031496062994128, -0.3460692066303957537, -1.428477690288713964 ) ) ;
#82006 = CARTESIAN_POINT ( 'NONE',  ( -0.1751536117528151582, 0.2379288306351265425, 0.1496817530000226215 ) ) ;
#82007 = CARTESIAN_POINT ( 'NONE',  ( -1.154855643044618851, -0.5023911411419708095, -0.1820866141732282451 ) ) ;
#82008 = CARTESIAN_POINT ( 'NONE',  ( -0.8530183727034112984, -0.4281496062992127816, -0.4176697321401328100 ) ) ;
#82009 = CARTESIAN_POINT ( 'NONE',  ( -0.3458507752293909498, 0.3458507752293907833, -0.4921259842519684624 ) ) ;
#82010 = CARTESIAN_POINT ( 'NONE',  ( -0.07763727620476214286, 1.069130918477190662, 3.936271712427351854 ) ) ;
#82011 = EDGE_CURVE ( 'NONE', #62516, #35589, #2825, .T. ) ;
#82012 = CARTESIAN_POINT ( 'NONE',  ( -0.2867679344610365999, 0.2867679344610364889, -0.01181102362204719709 ) ) ;
#82013 = CARTESIAN_POINT ( 'NONE',  ( 1.371391076115485941, 0.2952755905511811885, 0.1292274648535926551 ) ) ;
#82014 = CARTESIAN_POINT ( 'NONE',  ( 0.5249343832021003964, 0.2306618581243847221, -0.2411417322834647770 ) ) ;
#82015 = CARTESIAN_POINT ( 'NONE',  ( -0.08530183727034056085, -0.3162353388693405765, 0.4822834645669290543 ) ) ;
#82016 = CARTESIAN_POINT ( 'NONE',  ( -1.259842519685038686, -0.1870078740157480601, -0.3641732283464567677 ) ) ;
#82017 = CARTESIAN_POINT ( 'NONE',  ( -0.5511811023622041894, -0.1870078740157480879, -0.4822834645669291653 ) ) ;
#82018 = CARTESIAN_POINT ( 'NONE',  ( 0.4724409448818897572, -0.1265901696524988906, -2.550524934383202158 ) ) ;
#82019 = EDGE_CURVE ( 'NONE', #2910, #6386, #71852, .T. ) ;
#82020 = CARTESIAN_POINT ( 'NONE',  ( -0.8464566929133852113, -0.5400638737290845981, -0.3530559997133363437 ) ) ;
#82021 = CARTESIAN_POINT ( 'NONE',  ( -0.1058382717557497660, -0.3949938075777411073, -2.353674540682414218 ) ) ;
#82022 = CARTESIAN_POINT ( 'NONE',  ( 1.371391076115485719, -0.5511811023622048555, -0.09757992244046775898 ) ) ;
#82023 = CARTESIAN_POINT ( 'NONE',  ( -0.4724409448818890911, -0.1870078740157479769, 0.3641732283464567677 ) ) ;
#82024 = CARTESIAN_POINT ( 'NONE',  ( 1.332020997375329197, -0.2845877964562159024, 0.3641732283464567677 ) ) ;
#82025 = CARTESIAN_POINT ( 'NONE',  ( -1.469816272965878357, -0.6046776061558809534, -0.2411417322834644161 ) ) ;
#82026 = CARTESIAN_POINT ( 'NONE',  ( -1.062992125984250968, -0.5511811023622047445, 6.969142054262312111E-17 ) ) ;
#82027 = DIRECTION ( 'NONE',  ( 0.000000000000000000, 1.000000000000000000, 0.000000000000000000 ) ) ;
#82028 = CARTESIAN_POINT ( 'NONE',  ( 0.4002624671916016896, -0.08942795157527998196, 0.3641732283464567121 ) ) ;
#82029 = CARTESIAN_POINT ( 'NONE',  ( -0.2821522309711278487, -0.6692913385826773087, -0.1292274648535924053 ) ) ;
#82030 = CARTESIAN_POINT ( 'NONE',  ( 0.5314960629920990609, 2.742780008954323279, 2.570293882282747688 ) ) ;
#82031 = CARTESIAN_POINT ( 'NONE',  ( 0.05249343832021075018, -0.5023911411419708095, 0.1820866141732285504 ) ) ;
#82032 = CARTESIAN_POINT ( 'NONE',  ( 0.1265901696524989184, 0.4724409448818898127, -1.015091863517060267 ) ) ;
#82033 = CARTESIAN_POINT ( 'NONE',  ( 0.7545931758530189937, 0.2952755905511810774, -0.1292274648535930714 ) ) ;
#82034 = DIRECTION ( 'NONE',  ( -1.000000000000000000, -0.000000000000000000, -0.000000000000000000 ) ) ;
#82035 = CARTESIAN_POINT ( 'NONE',  ( 1.456692913385827515, 0.1771653543307087630, 0.000000000000000000 ) ) ;
#82036 = CARTESIAN_POINT ( 'NONE',  ( -0.7545931758530177724, 0.2952755905511811885, 0.1292274648535926551 ) ) ;
#82037 = CARTESIAN_POINT ( 'NONE',  ( -0.1509186351706028884, -0.2845877964562161244, -0.3641732283464567121 ) ) ;
#82038 = CARTESIAN_POINT ( 'NONE',  ( 0.000000000000000000, 2.559055118110236560, 0.000000000000000000 ) ) ;
#82039 = CARTESIAN_POINT ( 'NONE',  ( 0.2165354330708668673, 0.07958543189024071263, -0.2665933059059888421 ) ) ;
#82040 = EDGE_CURVE ( 'NONE', #75665, #73526, #78855, .T. ) ;
#82041 = CARTESIAN_POINT ( 'NONE',  ( -1.122047244094487306, -0.5400638737290844871, 0.3530559997133364547 ) ) ;
#82042 = CARTESIAN_POINT ( 'NONE',  ( -0.5052493438320203589, 0.2952755905511810774, -0.1292274648535930714 ) ) ;
#82043 = SHAPE_REPRESENTATION ( 'Screw Bronze Bushing Sleeve Inserts', ( #22098 ), #65120 ) ;
#82044 = CARTESIAN_POINT ( 'NONE',  ( 0.1070741851644054776, -0.3996062992125984925, -0.7919947506561679784 ) ) ;
#82045 = CARTESIAN_POINT ( 'NONE',  ( 0.3392501089628018884, -0.1958661417322834220, -2.394356955380577467 ) ) ;
#82046 = CARTESIAN_POINT ( 'NONE',  ( 0.4133858267716541968, -0.4536011799217368745, -0.2665933059059886201 ) ) ;
#82047 = CARTESIAN_POINT ( 'NONE',  ( -0.2427821522309703550, -0.3162353388693405765, 0.4822834645669290543 ) ) ;
#82048 = CARTESIAN_POINT ( 'NONE',  ( -0.7349081364829387342, -0.6046776061558807314, 0.2411417322834647770 ) ) ;
#82049 = CARTESIAN_POINT ( 'NONE',  ( -0.9055118110236215490, -0.5511811023622047445, 6.969142054262312111E-17 ) ) ;
#82050 = CARTESIAN_POINT ( 'NONE',  ( -3.927314176868121898, 1.151522056532830796, -0.2764061900857891496 ) ) ;
#82051 = CARTESIAN_POINT ( 'NONE',  ( 0.1246719160104994284, 0.2952755905511810774, -0.1292274648535930714 ) ) ;
#82052 = CARTESIAN_POINT ( 'NONE',  ( -1.148293963254592542, -0.5511811023622048555, -0.09757992244046775898 ) ) ;
#82053 = CARTESIAN_POINT ( 'NONE',  ( -1.633858267716534529, 0.1660481256975885056, 0.3530559997133364547 ) ) ;
#82054 = CARTESIAN_POINT ( 'NONE',  ( 0.2362204724409449064, 0.4091458600556404646, -2.191601049868766360 ) ) ;
#82055 = ORIENTED_EDGE ( 'NONE', *, *, #77836, .T. ) ;
#82056 = CARTESIAN_POINT ( 'NONE',  ( -1.351706036745406347, -0.004921259842519870586, -0.3153832671262229437 ) ) ;
#82057 = CARTESIAN_POINT ( 'NONE',  ( -1.194225721784776262, 0.05413385826771626580, -0.4176697321401330321 ) ) ;
#82058 = CARTESIAN_POINT ( 'NONE',  ( -0.7020997375328076329, -0.3162353388693409650, -0.4822834645669289433 ) ) ;
#82059 = EDGE_CURVE ( 'NONE', #5054, #6583, #70722, .T. ) ;
#82060 = CARTESIAN_POINT ( 'NONE',  ( -1.482939632545930975, 0.05413385826771666132, 0.4176697321401328100 ) ) ;
#82061 = CARTESIAN_POINT ( 'NONE',  ( -0.1958661417322834220, -0.3392501089628018884, -1.410104986876640654 ) ) ;
#82062 = CARTESIAN_POINT ( 'NONE',  ( 0.2065800153021795649, 0.3330030935778863221, -1.220472440944882164 ) ) ;
#82063 = CARTESIAN_POINT ( 'NONE',  ( 0.9645669291338591078, -0.5400638737290845981, -0.3530559997133363437 ) ) ;
#82064 = CARTESIAN_POINT ( 'NONE',  ( 0.3346456692913393205, -0.5400638737290845981, -0.3530559997133363437 ) ) ;
#82065 = CARTESIAN_POINT ( 'NONE',  ( -1.614173228346456712, 1.267785121476993737, -0.1372047244094478091 ) ) ;
#82066 = CARTESIAN_POINT ( 'NONE',  ( -0.3996062992125986035, 0.1070741851644051584, -2.314304461942256808 ) ) ;
#82067 = CARTESIAN_POINT ( 'NONE',  ( 1.332020997375328974, -0.08942795157528024563, -0.3641732283464568787 ) ) ;
#82068 = CARTESIAN_POINT ( 'NONE',  ( -0.3460692066303960868, 0.1998031496062990242, -0.8136482939632546652 ) ) ;
#82069 = VERTEX_POINT ( 'NONE', #12436 ) ;
#82070 = CARTESIAN_POINT ( 'NONE',  ( -1.023622047244093558, -0.1870078740157479769, 0.3641732283464567677 ) ) ;
#82071 = CARTESIAN_POINT ( 'NONE',  ( 0.3917322834645670104, 2.398668435337828261E-17, -2.472440944881889813 ) ) ;
#82072 = ORIENTED_EDGE ( 'NONE', *, *, #2754, .F. ) ;
#82073 = CARTESIAN_POINT ( 'NONE',  ( 0.4921259842519691285, 0.1660481256975885056, 0.3530559997133364547 ) ) ;
#82074 = CARTESIAN_POINT ( 'NONE',  ( -0.6233595800524928121, -0.05778040916215522460, 0.4822834645669289988 ) ) ;
#82075 = CARTESIAN_POINT ( 'NONE',  ( -0.9317585301837263412, -0.4281496062992127816, -0.4176697321401328100 ) ) ;
#82076 = CARTESIAN_POINT ( 'NONE',  ( 1.049868766404200349, 0.2306618581243848609, 0.2411417322834645549 ) ) ;
#82077 = CARTESIAN_POINT ( 'NONE',  ( -1.528871391076114250, -0.5511811023622046335, 0.09757992244046803654 ) ) ;
#82078 = DIRECTION ( 'NONE',  ( -1.000000000000000000, -0.000000000000000000, -0.000000000000000000 ) ) ;
#82079 = CARTESIAN_POINT ( 'NONE',  ( 0.1115485564304470323, 0.2952755905511811885, 0.1292274648535926551 ) ) ;
#82080 = CARTESIAN_POINT ( 'NONE',  ( -1.194225721784776262, -0.4281496062992124485, 0.4176697321401328655 ) ) ;
#82081 = CARTESIAN_POINT ( 'NONE',  ( 1.620734908136483465, -0.6692913385826771977, 0.1292274648535927661 ) ) ;
#82082 = EDGE_CURVE ( 'NONE', #11714, #34573, #82597, .T. ) ;
#82083 = CARTESIAN_POINT ( 'NONE',  ( -0.1958661417322834220, -0.3392501089628018884, -2.669947506561679784 ) ) ;
#82084 = CARTESIAN_POINT ( 'NONE',  ( 1.010498687664042716, -0.3690944881889763329, 0.3153832671262228327 ) ) ;
#82085 = ORIENTED_EDGE ( 'NONE', *, *, #32628, .T. ) ;
#82086 = CARTESIAN_POINT ( 'NONE',  ( 0.1058382717557499880, 0.3949938075777411073, -0.1509186351706037210 ) ) ;
#82087 = ORIENTED_EDGE ( 'NONE', *, *, #79479, .F. ) ;
#82088 = CARTESIAN_POINT ( 'NONE',  ( -0.1246719160104980823, 0.1771653543307087630, 0.09757992244046791164 ) ) ;
#82089 = CARTESIAN_POINT ( 'NONE',  ( -1.423884514435694859, -0.3162353388693405765, 0.4822834645669290543 ) ) ;
#82090 = CARTESIAN_POINT ( 'NONE',  ( 0.3805774278215230400, 0.05413385826771626580, -0.4176697321401330321 ) ) ;
#82091 = CARTESIAN_POINT ( 'NONE',  ( 0.2952755905511816326, -0.5400638737290844871, 0.3530559997133364547 ) ) ;
#82092 = CARTESIAN_POINT ( 'NONE',  ( -0.6233595800524928121, -0.05778040916215522460, 0.4822834645669289988 ) ) ;
#82093 = CARTESIAN_POINT ( 'NONE',  ( 0.2867679344610366554, 0.2867679344610366554, -1.551856586123046888 ) ) ;
#82094 = CARTESIAN_POINT ( 'NONE',  ( -1.043307086614172041, -0.5400638737290844871, 0.3530559997133364547 ) ) ;
#82095 = CARTESIAN_POINT ( 'NONE',  ( 0.3392501089628018329, 0.1958661417322835607, -2.578083989501311901 ) ) ;
#82096 = CARTESIAN_POINT ( 'NONE',  ( 1.318897637795276356, 0.07958543189024071263, -0.2665933059059888421 ) ) ;
#82097 = CARTESIAN_POINT ( 'NONE',  ( -0.9842519685039360366, 0.2952755905511811885, 0.000000000000000000 ) ) ;
#82098 = CARTESIAN_POINT ( 'NONE',  ( 0.8595800524934390507, -0.3162353388693405765, 0.4822834645669290543 ) ) ;
#82099 = CARTESIAN_POINT ( 'NONE',  ( 1.003937007874016407, -0.5400638737290844871, 0.3530559997133364547 ) ) ;
#82100 = AXIS2_PLACEMENT_3D ( 'NONE', #28777, #22470, #73827 ) ;
#82101 = CARTESIAN_POINT ( 'NONE',  ( -0.3996062992125986035, -0.1070741851644056997, -0.9908136482939633449 ) ) ;
#82102 = CARTESIAN_POINT ( 'NONE',  ( -1.496062992125983815, -0.1870078740157480879, -0.4822834645669291653 ) ) ;
#82103 = CARTESIAN_POINT ( 'NONE',  ( -0.3460692066303960313, 0.1998031496062989965, -0.2604986876640419946 ) ) ;
#82104 = CARTESIAN_POINT ( 'NONE',  ( 0.3937007874015754361, -0.1870078740157480879, -0.4822834645669291653 ) ) ;
#82105 = CARTESIAN_POINT ( 'NONE',  ( 0.2925321140481932369, -0.2925321140481932369, -2.303149606299212060 ) ) ;
#82106 = CARTESIAN_POINT ( 'NONE',  ( 0.2867679344610365999, 0.2867679344610365999, -1.482283464566929387 ) ) ;
#82107 = CARTESIAN_POINT ( 'NONE',  ( -1.541994750656167090, -0.5511811023622048555, -0.09757992244046775898 ) ) ;
#82108 = CARTESIAN_POINT ( 'NONE',  ( 0.3805774278215230400, -0.3690944881889763329, 0.3153832671262228327 ) ) ;
#82109 = CARTESIAN_POINT ( 'NONE',  ( 1.082677165354331228, -0.5400638737290844871, 0.3530559997133364547 ) ) ;
#82110 = CARTESIAN_POINT ( 'NONE',  ( -0.4091458600556405756, 0.2362204724409446288, -1.047900262467191590 ) ) ;
#82111 = CARTESIAN_POINT ( 'NONE',  ( 0.8727034120734913358, -0.08942795157527998196, 0.3641732283464567121 ) ) ;
#82112 = CARTESIAN_POINT ( 'NONE',  ( 0.5839895013123367340, -0.6692913385826773087, -0.1292274648535924053 ) ) ;
#82113 = CARTESIAN_POINT ( 'NONE',  ( 0.2891555358219910499, -0.2891555358219909944, -0.9625984251968502381 ) ) ;
#82114 = CARTESIAN_POINT ( 'NONE',  ( -0.8923884514435688198, 0.2306618581243847221, -0.2411417322834647770 ) ) ;
#82115 = CARTESIAN_POINT ( 'NONE',  ( -0.1771653543307080136, 0.1660481256975883391, -0.3530559997133364547 ) ) ;
#82116 = CARTESIAN_POINT ( 'NONE',  ( 1.128608923884514947, 0.1283753931104748280, 0.1820866141732283561 ) ) ;
#82117 = VECTOR ( 'NONE', #59785, 39.37007874015748143 ) ;
#82118 = CARTESIAN_POINT ( 'NONE',  ( 0.1049868766404206677, 0.1539470093639523085, 0.1968503937007873850 ) ) ;
#82119 = CARTESIAN_POINT ( 'NONE',  ( -0.3280839895013117347, -0.4281496062992124485, 0.4176697321401328655 ) ) ;
#82120 = CARTESIAN_POINT ( 'NONE',  ( 0.2230971128608932319, -0.3690944881889763329, 0.3153832671262228327 ) ) ;
#82121 = CARTESIAN_POINT ( 'NONE',  ( 0.06632061457837788720, 2.409604939980833412E-17, -0.3464511005275205946 ) ) ;
#82122 = CARTESIAN_POINT ( 'NONE',  ( -0.4330708661417315697, 0.2952755905511811885, 0.000000000000000000 ) ) ;
#82123 = CARTESIAN_POINT ( 'NONE',  ( 0.7742782152230978099, -0.3690944881889763329, 0.3153832671262228327 ) ) ;
#82124 = CARTESIAN_POINT ( 'NONE',  ( -0.5314960629921324786, 2.716535433070866645, 1.854472803289050509 ) ) ;
#82125 = CARTESIAN_POINT ( 'NONE',  ( 0.3996062992125985480, 2.446882876249141654E-17, -1.769685039370078927 ) ) ;
#82126 = CARTESIAN_POINT ( 'NONE',  ( 0.2034120734908144990, -0.6692913385826771977, 0.1292274648535927661 ) ) ;
#82127 = CARTESIAN_POINT ( 'NONE',  ( 1.108923884514436686, -0.2845877964562161244, -0.3641732283464567121 ) ) ;
#82128 = CARTESIAN_POINT ( 'NONE',  ( 0.2034120734908141659, 0.2952755905511810219, -0.1292274648535930437 ) ) ;
#82129 = CARTESIAN_POINT ( 'NONE',  ( -0.2493438320209966919, -0.004921259842519870586, -0.3153832671262229437 ) ) ;
#82130 = EDGE_CURVE ( 'NONE', #11499, #30580, #59417, .T. ) ;
#82131 = CARTESIAN_POINT ( 'NONE',  ( -0.5971128608923877978, 0.1771653543307087630, 0.09757992244046791164 ) ) ;
#82132 = CARTESIAN_POINT ( 'NONE',  ( -0.1968503937007867743, 0.2952755905511811885, 0.000000000000000000 ) ) ;
#82133 = CARTESIAN_POINT ( 'NONE',  ( 0.2559055118110243332, -0.5400638737290845981, -0.3530559997133363437 ) ) ;
#82134 = CARTESIAN_POINT ( 'NONE',  ( 1.003937007874016407, -0.4536011799217367080, 0.2665933059059888421 ) ) ;
#82135 = CARTESIAN_POINT ( 'NONE',  ( -1.601049868766403650, -0.5023911411419708095, 0.1820866141732285504 ) ) ;
#82136 = CARTESIAN_POINT ( 'NONE',  ( 1.502624671916010790, -0.2845877964562161244, -0.3641732283464567121 ) ) ;
#82137 = EDGE_CURVE ( 'NONE', #53393, #72873, #23826, .T. ) ;
#82138 = CARTESIAN_POINT ( 'NONE',  ( 0.9186351706036752773, 0.2306618581243847221, -0.2411417322834647770 ) ) ;
#82139 = CARTESIAN_POINT ( 'NONE',  ( 0.4744094488189051773, 1.528817788452848880, -2.170146923806634209 ) ) ;
#82140 = CARTESIAN_POINT ( 'NONE',  ( -0.01312335958005186876, -0.4281496062992124485, 0.4176697321401328655 ) ) ;
#82141 = CARTESIAN_POINT ( 'NONE',  ( -9.594673741351313045E-17, 0.3917322834645670104, -1.029527559055118280 ) ) ;
#82142 = CARTESIAN_POINT ( 'NONE',  ( 0.9973753280839902091, -0.6046776061558807314, 0.2411417322834647770 ) ) ;
#82143 = CARTESIAN_POINT ( 'NONE',  ( 0.7545931758530189937, 0.2952755905511810774, -0.1292274648535930714 ) ) ;
#82144 = DIRECTION ( 'NONE',  ( 0.000000000000000000, -1.000000000000000000, 0.000000000000000000 ) ) ;
#82145 = CARTESIAN_POINT ( 'NONE',  ( 0.4658792650918641698, -0.08942795157528024563, -0.3641732283464568787 ) ) ;
#82146 = CARTESIAN_POINT ( 'NONE',  ( 1.030183727034121421, -0.05778040916215522460, 0.4822834645669289988 ) ) ;
#82147 = CARTESIAN_POINT ( 'NONE',  ( 0.07874015748031558404, -0.1870078740157480601, -0.3641732283464567677 ) ) ;
#82148 = CARTESIAN_POINT ( 'NONE',  ( -0.1049868766404193215, -0.6046776061558807314, 0.2411417322834647770 ) ) ;
#82149 = DIRECTION ( 'NONE',  ( 0.000000000000000000, 1.000000000000000000, 0.000000000000000000 ) ) ;
#82150 = CARTESIAN_POINT ( 'NONE',  ( 0.3280839895013130669, 0.05413385826771666132, 0.4176697321401328100 ) ) ;
#82151 = CARTESIAN_POINT ( 'NONE',  ( -0.8595800524934373854, -0.05778040916215522460, 0.4822834645669289988 ) ) ;
#82152 = CARTESIAN_POINT ( 'NONE',  ( -0.1246719160104980823, 0.1771653543307087630, 0.09757992244046791164 ) ) ;
#82153 = CIRCLE ( 'NONE', #79467, 0.4822834645669291653 ) ;
#82154 = CARTESIAN_POINT ( 'NONE',  ( 0.4133858267716541968, -0.5400638737290845981, -0.3530559997133363437 ) ) ;
#82155 = CARTESIAN_POINT ( 'NONE',  ( 1.128608923884515169, -0.5023911411419708095, -0.1820866141732282451 ) ) ;
#82156 = CARTESIAN_POINT ( 'NONE',  ( -0.4002624671916004129, -0.3162353388693405765, 0.4822834645669290543 ) ) ;
#82157 = CARTESIAN_POINT ( 'NONE',  ( -0.4724409448818898682, -8.678599364036362592E-17, -0.5118110236220472231 ) ) ;
#82159 = DIRECTION ( 'NONE',  ( -0.7071067811865429098, 0.7071067811865521247, 0.000000000000000000 ) ) ;
#82158 = CARTESIAN_POINT ( 'NONE',  ( 0.000000000000000000, 0.2726377952755905665, 0.07874015748031495954 ) ) ;
#82160 = CARTESIAN_POINT ( 'NONE',  ( 1.601049868766404982, -0.6046776061558809534, -0.2411417322834644161 ) ) ;
#82161 = CARTESIAN_POINT ( 'NONE',  ( 0.000000000000000000, 0.000000000000000000, -1.220472440944881942 ) ) ;
#82162 = CARTESIAN_POINT ( 'NONE',  ( -1.266404199475064773, -0.05778040916215560624, -0.4822834645669293319 ) ) ;
#82163 = CARTESIAN_POINT ( 'NONE',  ( -0.7086614173228339419, -0.1870078740157480879, -0.4822834645669291653 ) ) ;
#82164 = CARTESIAN_POINT ( 'NONE',  ( -0.1265901696524993347, 0.4724409448818895907, -0.4790026246719158998 ) ) ;
#82165 = CARTESIAN_POINT ( 'NONE',  ( -0.1070741851644056997, 0.3996062992125986035, 0.1509186351706036100 ) ) ;
#82166 = ORIENTED_EDGE ( 'NONE', *, *, #46764, .F. ) ;
#82167 = CARTESIAN_POINT ( 'NONE',  ( 0.1312335958005257930, 0.1283753931104746893, -0.1820866141732285504 ) ) ;
#82168 = CARTESIAN_POINT ( 'NONE',  ( 0.3917322834645670104, 2.398668435337828261E-17, -1.527559055118110409 ) ) ;
#82169 = CARTESIAN_POINT ( 'NONE',  ( 0.5839895013123367340, -0.6692913385826773087, -0.1292274648535924053 ) ) ;
#82170 = CARTESIAN_POINT ( 'NONE',  ( 5.785732909357575061E-17, -0.4724409448818898682, -2.283464566929133799 ) ) ;
#82171 = CARTESIAN_POINT ( 'NONE',  ( -0.5611900217179893735, -2.567464376874931580E-15, -0.4445507791589072832 ) ) ;
#82173 = AXIS2_PLACEMENT_3D ( 'NONE', #8926, #9752, #34603 ) ;
#82172 = CARTESIAN_POINT ( 'NONE',  ( -1.587926509186350810, -0.3690944881889763329, 0.3153832671262228327 ) ) ;
#82174 = CARTESIAN_POINT ( 'NONE',  ( 1.043307086614173818, 0.1660481256975885056, 0.3530559997133364547 ) ) ;
#82175 = CARTESIAN_POINT ( 'NONE',  ( 1.437007874015748810, 0.07958543189024085140, 0.2665933059059887866 ) ) ;
#82176 = CARTESIAN_POINT ( 'NONE',  ( 0.1312335958005257930, 0.2306618581243847221, -0.2411417322834647770 ) ) ;
#82177 = CARTESIAN_POINT ( 'NONE',  ( 0.3392501089628018329, -0.1958661417322834497, -0.6574609991787909724 ) ) ;
#82178 = CARTESIAN_POINT ( 'NONE',  ( -0.2624671916010490880, -0.6046776061558807314, 0.2411417322834647770 ) ) ;
#82179 = CARTESIAN_POINT ( 'NONE',  ( -1.259842519685038686, -0.1870078740157479769, 0.3641732283464567677 ) ) ;
#82180 = CARTESIAN_POINT ( 'NONE',  ( -0.6167979002624665030, 0.05413385826771666132, 0.4176697321401328100 ) ) ;
#82181 = DIRECTION ( 'NONE',  ( -1.000000000000000000, -3.469446951953613696E-16, 0.000000000000000000 ) ) ;
#82182 = CARTESIAN_POINT ( 'NONE',  ( -0.2248141966262267588, 1.118402650174327384, -1.901317244778563342 ) ) ;
#82183 = VERTEX_POINT ( 'NONE', #18349 ) ;
#82184 = CARTESIAN_POINT ( 'NONE',  ( 0.3917322834645670659, 2.398668435337828261E-17, -2.004612491634857552 ) ) ;
#82185 = CARTESIAN_POINT ( 'NONE',  ( 0.5839895013123367340, 0.2952755905511811885, 0.1292274648535926551 ) ) ;
#82186 = ORIENTED_EDGE ( 'NONE', *, *, #45702, .T. ) ;
#82187 = CARTESIAN_POINT ( 'NONE',  ( -0.4986876640419942164, -0.6046776061558807314, 0.2411417322834647770 ) ) ;
#82188 = CARTESIAN_POINT ( 'NONE',  ( -1.377952755905511140, -0.6692913385826771977, 8.415575281601705876E-17 ) ) ;
#82189 = CARTESIAN_POINT ( 'NONE',  ( 0.5905511811023629321, -0.6692913385826771977, 8.415575281601705876E-17 ) ) ;
#82190 = CARTESIAN_POINT ( 'NONE',  ( -0.08530183727034056085, -0.3162353388693405765, 0.4822834645669290543 ) ) ;
#82191 = CARTESIAN_POINT ( 'NONE',  ( 0.3392501089628018884, -0.1958661417322834220, -1.291994750656167978 ) ) ;
#82192 = CARTESIAN_POINT ( 'NONE',  ( -0.6233595800524928121, -0.05778040916215522460, 0.4822834645669289988 ) ) ;
#82193 = CARTESIAN_POINT ( 'NONE',  ( 0.4330708661417329575, 0.2952755905511811885, 0.000000000000000000 ) ) ;
#82194 = CARTESIAN_POINT ( 'NONE',  ( -0.5905511811023613777, -0.6692913385826771977, 8.415575281601705876E-17 ) ) ;
#82195 = CARTESIAN_POINT ( 'NONE',  ( 0.2427821522309719648, -0.08942795157527998196, 0.3641732283464567121 ) ) ;
#82196 = CARTESIAN_POINT ( 'NONE',  ( -0.2524556255358376688, -0.1533185143264484962, 5.612478741320920506 ) ) ;
#82197 = CARTESIAN_POINT ( 'NONE',  ( -0.07217847769028813698, -0.3162353388693409650, -0.4822834645669289433 ) ) ;
#82198 = CARTESIAN_POINT ( 'NONE',  ( 0.000000000000000000, 1.724409448818897461, 0.000000000000000000 ) ) ;
#82199 = CARTESIAN_POINT ( 'NONE',  ( -1.555118110236219930, -0.5400638737290845981, -0.3530559997133363437 ) ) ;
#82200 = CARTESIAN_POINT ( 'NONE',  ( -0.3917322834645671215, 0.1049643490035301469, -2.702099737532808632 ) ) ;
#82201 = ORIENTED_EDGE ( 'NONE', *, *, #40849, .F. ) ;
#82202 = ORIENTED_EDGE ( 'NONE', *, *, #73105, .F. ) ;
#82203 = CARTESIAN_POINT ( 'NONE',  ( 0.7086614173228353852, -0.1870078740157479769, 0.4822834645669291653 ) ) ;
#82204 = CARTESIAN_POINT ( 'NONE',  ( 0.2165354330708668673, 0.07958543189024071263, -0.2665933059059888421 ) ) ;
#82206 = CARTESIAN_POINT ( 'NONE',  ( -0.4744094488189045666, 1.537401574803149984, 2.170146923806632877 ) ) ;
#82205 = LINE ( 'NONE', #10677, #14876 ) ;
#82207 = CARTESIAN_POINT ( 'NONE',  ( 0.2867679344610365999, 0.2867679344610365999, -1.324803149606299302 ) ) ;
#82208 = CARTESIAN_POINT ( 'NONE',  ( 0.3458507752293908943, 0.3458507752293908943, 0.1003937007874015769 ) ) ;
#82209 = CARTESIAN_POINT ( 'NONE',  ( 0.2952755905511810774, 3.616083068348483797E-17, 0.1574803149606299191 ) ) ;
#82210 = CARTESIAN_POINT ( 'NONE',  ( 0.2925321140481932369, 0.2925321140481932369, -2.734251968503936148 ) ) ;
#82211 = CARTESIAN_POINT ( 'NONE',  ( 0.4921259842519691285, 0.1660481256975885056, 0.3530559997133364547 ) ) ;
#82212 = CARTESIAN_POINT ( 'NONE',  ( -1.181102362204723644, -0.1870078740157479769, 0.4822834645669291653 ) ) ;
#82213 = CARTESIAN_POINT ( 'NONE',  ( -1.023622047244094002, -0.1870078740157480879, -0.4822834645669291653 ) ) ;
#82214 = CARTESIAN_POINT ( 'NONE',  ( 0.3346456692913390985, 0.1660481256975885056, 0.3530559997133364547 ) ) ;
#82215 = CIRCLE ( 'NONE', #78014, 2.598425196850393970 ) ;
#82216 = CARTESIAN_POINT ( 'NONE',  ( 0.9448818897637802916, -0.1870078740157479769, 0.4822834645669291653 ) ) ;
#82217 = CARTESIAN_POINT ( 'NONE',  ( 1.174540682414699111, -0.2845877964562159024, 0.3641732283464567677 ) ) ;
#82218 = CARTESIAN_POINT ( 'NONE',  ( 1.377952755905512472, 0.1771653543307087630, 0.000000000000000000 ) ) ;
#82219 = CARTESIAN_POINT ( 'NONE',  ( -0.6824146981627288167, 0.2306618581243848609, 0.2411417322834645549 ) ) ;
#82220 = CARTESIAN_POINT ( 'NONE',  ( 0.3460692066303958092, 0.1998031496062993018, -0.5229658792650918597 ) ) ;
#82221 = CARTESIAN_POINT ( 'NONE',  ( 1.673228346456693494, 0.1660481256975885056, 0.3530559997133364547 ) ) ;
#82222 = CARTESIAN_POINT ( 'NONE',  ( -0.1958661417322836718, 0.3392501089628017219, -0.3202099737532808077 ) ) ;
#82223 = CARTESIAN_POINT ( 'NONE',  ( -0.1312335958005241554, -0.6046776061558809534, -0.2411417322834644161 ) ) ;
#82225 = CARTESIAN_POINT ( 'NONE',  ( -0.4698424923132972220, 1.469648236684816256, 2.159177592673387824 ) ) ;
#82224 = CARTESIAN_POINT ( 'NONE',  ( 1.167979002624672580, -0.4281496062992124485, 0.4176697321401328655 ) ) ;
#82226 = CARTESIAN_POINT ( 'NONE',  ( -1.509186351706035767, -0.004921259842519870586, -0.3153832671262229437 ) ) ;
#82227 = CARTESIAN_POINT ( 'NONE',  ( -0.07874015748031421014, -0.1870078740157479769, 0.4822834645669291653 ) ) ;
#82228 = CARTESIAN_POINT ( 'NONE',  ( 0.7545931758530188826, -0.5511811023622046335, 0.09757992244046803654 ) ) ;
#82229 = EDGE_CURVE ( 'NONE', #38768, #312, #16765, .T. ) ;
#82230 = CARTESIAN_POINT ( 'NONE',  ( -1.450131233595799651, -0.5511811023622046335, 0.09757992244046803654 ) ) ;
#82231 = CARTESIAN_POINT ( 'NONE',  ( 1.062992125984252745, 0.2952755905511811885, 0.000000000000000000 ) ) ;
#82232 = CARTESIAN_POINT ( 'NONE',  ( -0.7426113562971994320, 1.972848275015058439, 0.5309055118110236338 ) ) ;
#82233 = CARTESIAN_POINT ( 'NONE',  ( -0.4133858267716528645, 0.07958543189024071263, -0.2665933059059888421 ) ) ;
#82234 = CARTESIAN_POINT ( 'NONE',  ( -0.5052493438320203589, -0.6692913385826771977, 0.1292274648535927661 ) ) ;
#82235 = CARTESIAN_POINT ( 'NONE',  ( 1.443569553805774897, -0.6046776061558809534, -0.2411417322834644161 ) ) ;
#82236 = CARTESIAN_POINT ( 'NONE',  ( -1.069553805774277722, 0.2952755905511811885, 0.1292274648535926551 ) ) ;
#82237 = CARTESIAN_POINT ( 'NONE',  ( 1.299212598425197429, -0.6692913385826771977, 8.415575281601705876E-17 ) ) ;
#82238 = CARTESIAN_POINT ( 'NONE',  ( -9.594673741351313045E-17, 0.3917322834645670659, -0.9416203656506056952 ) ) ;
#82239 = CARTESIAN_POINT ( 'NONE',  ( -1.207349081364828436, -0.5023911411419708095, 0.1820866141732285504 ) ) ;
#82240 = CARTESIAN_POINT ( 'NONE',  ( 1.115278074387389351, 1.079212911816122888, -0.1239772976664039461 ) ) ;
#82241 = CARTESIAN_POINT ( 'NONE',  ( 1.450131233595801428, 0.2952755905511811885, 0.1292274648535926551 ) ) ;
#82242 = CARTESIAN_POINT ( 'NONE',  ( 0.1265901696524990294, -0.4724409448818896462, -2.051837270341206665 ) ) ;
#82243 = CARTESIAN_POINT ( 'NONE',  ( -1.640419947506561060, -0.4281496062992127816, -0.4176697321401328100 ) ) ;
#82244 = CARTESIAN_POINT ( 'NONE',  ( -1.364829396325458521, -0.5023911411419708095, 0.1820866141732285504 ) ) ;
#82245 = CARTESIAN_POINT ( 'NONE',  ( -1.030183727034119867, -0.08942795157528024563, -0.3641732283464568787 ) ) ;
#82246 = CARTESIAN_POINT ( 'NONE',  ( 1.555118110236221041, 0.07958543189024071263, -0.2665933059059888421 ) ) ;
#82247 = CARTESIAN_POINT ( 'NONE',  ( -0.3412073490813641308, 0.2306618581243847221, -0.2411417322834647770 ) ) ;
#82248 = CARTESIAN_POINT ( 'NONE',  ( -0.02624671916010428221, 0.1283753931104746893, -0.1820866141732285504 ) ) ;
#82249 = CARTESIAN_POINT ( 'NONE',  ( -0.9908136482939626788, -0.5511811023622048555, -0.09757992244046775898 ) ) ;
#82250 = CARTESIAN_POINT ( 'NONE',  ( 1.430446194225722500, -0.004921259842519576551, 0.3153832671262227771 ) ) ;
#82251 = CARTESIAN_POINT ( 'NONE',  ( 0.9055118110236227702, 0.2952755905511811885, 0.000000000000000000 ) ) ;
#82252 = CARTESIAN_POINT ( 'NONE',  ( 1.509186351706037543, -0.4281496062992127816, -0.4176697321401328100 ) ) ;
#82253 = CARTESIAN_POINT ( 'NONE',  ( 0.2887139107611556010, 0.1283753931104746893, -0.1820866141732285504 ) ) ;
#82254 = CARTESIAN_POINT ( 'NONE',  ( 0.4265091863517067594, 0.2952755905511811885, 0.1292274648535926551 ) ) ;
#82255 = CARTESIAN_POINT ( 'NONE',  ( 1.194225721784777594, -0.3690944881889765550, -0.3153832671262227771 ) ) ;
#82256 = EDGE_LOOP ( 'NONE', ( #28514, #42079, #70257, #75591 ) ) ;
#82257 = CARTESIAN_POINT ( 'NONE',  ( -1.450131233595799651, 0.2952755905511810774, -0.1292274648535930714 ) ) ;
#82258 = B_SPLINE_CURVE_WITH_KNOTS ( 'NONE', 3,
 ( #69805, #30678, #69398, #81633 ),
 .UNSPECIFIED., .F., .F.,
 ( 4, 4 ),
 ( 0.000000000000000000, 0.001434885020664813287 ),
 .UNSPECIFIED. ) ;
#82259 = CARTESIAN_POINT ( 'NONE',  ( -1.469816272965878357, 0.2306618581243848609, 0.2411417322834645549 ) ) ;
#82260 = CARTESIAN_POINT ( 'NONE',  ( -0.2165354330708654795, -0.5400638737290845981, -0.3530559997133363437 ) ) ;
#82261 = CARTESIAN_POINT ( 'NONE',  ( 0.5408419829024507797, -1.283732188437465593E-15, -0.4281993546915538462 ) ) ;
#82262 = CARTESIAN_POINT ( 'NONE',  ( -9.787531504996566615E-17, 0.3996062992125985480, -2.596456692913385655 ) ) ;
#82263 = CARTESIAN_POINT ( 'NONE',  ( 0.4199475065616803948, -0.6046776061558809534, -0.2411417322834644161 ) ) ;
#82264 = CARTESIAN_POINT ( 'NONE',  ( 1.141732283464567566, 0.1771653543307087630, 0.000000000000000000 ) ) ;
#82265 = CARTESIAN_POINT ( 'NONE',  ( 0.1246719160104994284, 0.2952755905511810774, -0.1292274648535930714 ) ) ;
#82266 = CARTESIAN_POINT ( 'NONE',  ( 0.5183727034120741983, 0.2952755905511810774, -0.1292274648535930714 ) ) ;
#82267 = CARTESIAN_POINT ( 'NONE',  ( -0.3460692066303960868, 0.1998031496062990242, -2.230971128608923770 ) ) ;
#82268 = CARTESIAN_POINT ( 'NONE',  ( 0.3949938075777411073, -0.1058382717557499464, -1.686351706036745668 ) ) ;
#82269 = CARTESIAN_POINT ( 'NONE',  ( -0.2925321140481932924, 0.2925321140481931814, -2.854330708661417138 ) ) ;
#82270 = CARTESIAN_POINT ( 'NONE',  ( 0.4724409448818897017, 0.1265901696524990294, -2.486876640419947382 ) ) ;
#82271 = CARTESIAN_POINT ( 'NONE',  ( 0.1958661417322836440, -0.3392501089628017219, -0.3989501312335957950 ) ) ;
#82272 = CARTESIAN_POINT ( 'NONE',  ( -0.7020997375328076329, -0.2845877964562161244, -0.3641732283464567121 ) ) ;
#82273 = CARTESIAN_POINT ( 'NONE',  ( -0.8727034120734901146, -0.05778040916215560624, -0.4822834645669293319 ) ) ;
#82274 = CARTESIAN_POINT ( 'NONE',  ( 0.3608923884514443348, 0.2952755905511810774, -0.1292274648535930714 ) ) ;
#82275 = CARTESIAN_POINT ( 'NONE',  ( -0.1974969037888706924, 0.3420746716998658843, -2.609580052493438718 ) ) ;
#82276 = CARTESIAN_POINT ( 'NONE',  ( 0.8136482939632553313, -0.6046776061558809534, -0.2411417322834644161 ) ) ;
#82277 = CARTESIAN_POINT ( 'NONE',  ( -1.548556430446193399, -0.6046776061558809534, -0.2411417322834644161 ) ) ;
#82278 = CARTESIAN_POINT ( 'NONE',  ( 0.8661417322834652488, -0.1870078740157480879, -0.4822834645669291653 ) ) ;
#82279 = CARTESIAN_POINT ( 'NONE',  ( -0.1265901696524986964, -0.4724409448818899238, -2.749343832020996636 ) ) ;
#82280 = CARTESIAN_POINT ( 'NONE',  ( 0.3996062992125986590, -0.1070741851644053111, -2.316272965879265122 ) ) ;
#82281 = DIRECTION ( 'NONE',  ( 0.000000000000000000, 0.000000000000000000, 1.000000000000000000 ) ) ;
#82282 = CARTESIAN_POINT ( 'NONE',  ( 0.8792650918635177559, -0.4281496062992127816, -0.4176697321401328100 ) ) ;
#82283 = CARTESIAN_POINT ( 'NONE',  ( 0.6692913385826777528, 0.2952755905511811885, 0.000000000000000000 ) ) ;
#82284 = CARTESIAN_POINT ( 'NONE',  ( 1.384514435695538337, -0.5511811023622046335, 0.09757992244046803654 ) ) ;
#82285 = CARTESIAN_POINT ( 'NONE',  ( 1.555118110236221041, 0.1660481256975883668, -0.3530559997133364547 ) ) ;
#82286 = CARTESIAN_POINT ( 'NONE',  ( -0.3392501089628017219, -0.1958661417322836718, -0.2946194225721785465 ) ) ;
#82287 = LINE ( 'NONE', #81056, #41037 ) ;
#82288 = CARTESIAN_POINT ( 'NONE',  ( 0.6430446194225729606, -0.4281496062992127816, -0.4176697321401328100 ) ) ;
#82289 = CARTESIAN_POINT ( 'NONE',  ( 1.417322834645670104, -0.1870078740157480601, -0.3641732283464567677 ) ) ;
#82290 = CARTESIAN_POINT ( 'NONE',  ( -0.4986876640419942164, -0.6046776061558807314, 0.2411417322834647770 ) ) ;
#82291 = CARTESIAN_POINT ( 'NONE',  ( -0.9383202099737524282, -0.05778040916215522460, 0.4822834645669289988 ) ) ;
#82292 = CARTESIAN_POINT ( 'NONE',  ( 0.9908136482939640111, 0.2952755905511810774, -0.1292274648535930714 ) ) ;
#82293 = CARTESIAN_POINT ( 'NONE',  ( -0.2867679344610365999, 0.2867679344610364889, -0.4192913385826772532 ) ) ;
#82294 = CARTESIAN_POINT ( 'NONE',  ( -0.1958661417322836718, 0.3392501089628017219, -1.580052493438320216 ) ) ;
#82295 = CARTESIAN_POINT ( 'NONE',  ( 0.1958661417322836440, -0.3392501089628017219, -2.603674540682414218 ) ) ;
#82296 = CARTESIAN_POINT ( 'NONE',  ( -1.587926509186350810, -0.004921259842519870586, -0.3153832671262229437 ) ) ;
#82297 = ORIENTED_EDGE ( 'NONE', *, *, #58451, .F. ) ;
#82298 = CARTESIAN_POINT ( 'NONE',  ( -0.1974969037888706647, 0.3420746716998658843, -2.690288713910760965 ) ) ;
#82299 = ORIENTED_EDGE ( 'NONE', *, *, #80402, .T. ) ;
#82300 = DIRECTION ( 'NONE',  ( 0.000000000000000000, -1.000000000000000000, 1.408710688920637755E-15 ) ) ;
#82301 = CARTESIAN_POINT ( 'NONE',  ( 1.555118110236221041, -0.4536011799217367080, 0.2665933059059888421 ) ) ;
#82302 = CARTESIAN_POINT ( 'NONE',  ( -0.3996062992125987146, 0.1070741851644051862, -1.292650918635170454 ) ) ;
#82303 = CARTESIAN_POINT ( 'NONE',  ( 1.463254593175853824, -0.5511811023622046335, 0.09757992244046803654 ) ) ;
#82304 = DIRECTION ( 'NONE',  ( -0.000000000000000000, -1.000000000000000000, -0.000000000000000000 ) ) ;
#82305 = CARTESIAN_POINT ( 'NONE',  ( 0.000000000000000000, 2.559055118110236560, 0.000000000000000000 ) ) ;
#82306 = CARTESIAN_POINT ( 'NONE',  ( 1.076935383196057749, 2.165354330708661568, -0.3149606299212595606 ) ) ;
#82307 = CARTESIAN_POINT ( 'NONE',  ( -0.3917322834645671215, 0.1049643490035301469, -0.2749343832020998413 ) ) ;
#82308 = CARTESIAN_POINT ( 'NONE',  ( -0.7217847769028863381, -0.3690944881889763329, 0.3153832671262228327 ) ) ;
#82309 = CARTESIAN_POINT ( 'NONE',  ( -1.351706036745406347, -0.004921259842519870586, -0.3153832671262229437 ) ) ;
#82310 = CARTESIAN_POINT ( 'NONE',  ( -1.351706036745406347, -0.4281496062992124485, 0.4176697321401328655 ) ) ;
#82311 = CARTESIAN_POINT ( 'NONE',  ( 0.2427821522309716595, -0.3162353388693409650, -0.4822834645669289433 ) ) ;
#82312 = CARTESIAN_POINT ( 'NONE',  ( 1.548556430446194954, -0.6046776061558807314, 0.2411417322834647770 ) ) ;
#82313 = EDGE_LOOP ( 'NONE', ( #3164, #23797, #82085, #63860 ) ) ;
#82314 = CARTESIAN_POINT ( 'NONE',  ( 1.325459317585302665, 0.05413385826771626580, -0.4176697321401330321 ) ) ;
#82315 = DIRECTION ( 'NONE',  ( -0.000000000000000000, 1.000000000000000000, -0.000000000000000000 ) ) ;
#82316 = CARTESIAN_POINT ( 'NONE',  ( -0.1265901696524993347, 0.4724409448818895907, -2.053805774278214979 ) ) ;
#82317 = CARTESIAN_POINT ( 'NONE',  ( 3.924389226575468737, 2.165354330708661568, 0.3149606299212600047 ) ) ;
#82318 = CARTESIAN_POINT ( 'NONE',  ( -0.3937007874015740483, -0.1870078740157479769, 0.3641732283464567677 ) ) ;
#82319 = ADVANCED_FACE ( 'NONE', ( #68859 ), #44390, .F. ) ;
#82320 = CARTESIAN_POINT ( 'NONE',  ( -1.292650918635170010, 0.2952755905511810774, -0.1292274648535930714 ) ) ;
#82321 = CARTESIAN_POINT ( 'NONE',  ( 1.200787401574803681, 0.1660481256975885056, 0.3530559997133364547 ) ) ;
#82322 = VERTEX_POINT ( 'NONE', #57031 ) ;
#82324 = CARTESIAN_POINT ( 'NONE',  ( 0.4091458600556404646, -0.2362204724409448231, -2.701443569553806157 ) ) ;
#82323 = DIRECTION ( 'NONE',  ( 1.000000000000000000, 1.460819769243627131E-15, 0.000000000000000000 ) ) ;
#82325 = CARTESIAN_POINT ( 'NONE',  ( -1.666666666666665853, 0.05413385826771626580, -0.4176697321401330321 ) ) ;
#82326 = CARTESIAN_POINT ( 'NONE',  ( -1.213910761154854745, 0.2952755905511810774, -0.1292274648535930714 ) ) ;
#82327 = CARTESIAN_POINT ( 'NONE',  ( -0.3917322834645669549, -7.196005306013483243E-17, -0.5918442012785283257 ) ) ;
#82328 = EDGE_CURVE ( 'NONE', #70570, #16375, #35558, .T. ) ;
#82329 = CARTESIAN_POINT ( 'NONE',  ( -0.1902887139107604098, -0.5511811023622046335, 0.09757992244046803654 ) ) ;
#82330 = CARTESIAN_POINT ( 'NONE',  ( 0.1958661417322834775, 0.3392501089628018884, -0.8589238845144357981 ) ) ;
#82331 = CARTESIAN_POINT ( 'NONE',  ( -0.5249343832020990641, 0.1283753931104748280, 0.1820866141732283561 ) ) ;
#82332 = CARTESIAN_POINT ( 'NONE',  ( 0.5118110236220478892, 0.1771653543307087630, 0.000000000000000000 ) ) ;
#82333 = CARTESIAN_POINT ( 'NONE',  ( 0.7414698162729663755, -0.6692913385826773087, -0.1292274648535924053 ) ) ;
#82334 = CARTESIAN_POINT ( 'NONE',  ( -0.5314960629921250401, 0.07958543189024085140, 0.2665933059059887866 ) ) ;
#82335 = CARTESIAN_POINT ( 'NONE',  ( 0.1049643490035304938, -0.3917322834645669549, -2.754593175853017328 ) ) ;
#82336 = CARTESIAN_POINT ( 'NONE',  ( 0.9842519685039375910, 0.2952755905511811885, 0.000000000000000000 ) ) ;
#82337 = CARTESIAN_POINT ( 'NONE',  ( -0.9842519685039360366, 0.2952755905511811885, 0.000000000000000000 ) ) ;
#82338 = CARTESIAN_POINT ( 'NONE',  ( -0.2362204724409447953, -0.4091458600556404646, -0.9297900262467192478 ) ) ;
#82339 = CARTESIAN_POINT ( 'NONE',  ( -0.5446194225721777693, -0.3162353388693409650, -0.4822834645669289433 ) ) ;
#82340 = CARTESIAN_POINT ( 'NONE',  ( -0.3740157480314953431, 0.1660481256975885056, 0.3530559997133364547 ) ) ;
#82341 = CARTESIAN_POINT ( 'NONE',  ( 1.351706036745407680, -0.004921259842519576551, 0.3153832671262227771 ) ) ;
#82342 = CARTESIAN_POINT ( 'NONE',  ( -0.09186351706036689768, -0.004921259842519870586, -0.3153832671262229437 ) ) ;
#82343 = CARTESIAN_POINT ( 'NONE',  ( -0.1574803149606292529, -0.1870078740157479769, 0.4822834645669291653 ) ) ;
#82344 = CARTESIAN_POINT ( 'NONE',  ( -1.108923884514435132, -0.05778040916215560624, -0.4822834645669293319 ) ) ;
#82345 = CARTESIAN_POINT ( 'NONE',  ( 0.000000000000000000, 0.000000000000000000, -1.220472440944881942 ) ) ;
#82346 = LINE ( 'NONE', #76030, #77129 ) ;
#82347 = CARTESIAN_POINT ( 'NONE',  ( -0.3083989501312330295, -0.3162353388693409650, -0.4822834645669289433 ) ) ;
#82348 = CARTESIAN_POINT ( 'NONE',  ( -1.148293963254592542, -0.6692913385826773087, -0.1292274648535924053 ) ) ;
#82349 = EDGE_LOOP ( 'NONE', ( #41822, #33514, #45405, #27205 ) ) ;
#82350 = CARTESIAN_POINT ( 'NONE',  ( 0.3460692066303959202, -0.1998031496062991630, -2.071522309711285814 ) ) ;
#82351 =( BOUNDED_SURFACE ( )  B_SPLINE_SURFACE ( 1, 2, ( 
 ( #32759, #6667, #58426, #32339, #58001, #365, #26021, #19714, #7517, #2031, #58854, #20972, #71487, #14674, #40331, #46631, #28112, #59676, #54182, #39493, #65180, #22213, #72327, #33185, #27697, #14259, #66846, #52520, #53361, #8759, #53766, #79071, #78650, #21387, #34434, #47456, #78228, #8348, #34850, #71908, #66010, #47042, #34014, #52937, #72735, #20561, #33598, #79477, #21793, #39917, #1211, #79895, #26861, #9179, #46213, #65606, #7937, #59263, #60513, #2454, #15081, #73150, #41157, #1620, #40739, #27276, #66423, #60100, #15499, #13834, #2861, #28524, #30590, #17566, #28934, #4922, #73984, #68081, #80312, #55834, #36904, #68489, #73574, #36488, #43199, #55011, #81542, #4091, #48700, #55422, #16330, #15920, #67256, #61754, #35258, #80720, #47870, #74398, #16742, #23034, #4504, #36083, #56256, #41567, #9589, #81952, #42382, #60922, #29760, #41974, #68894, #54603, #81129, #10828, #30171, #23446, #10425, #49110, #62164, #23861, #22627, #74816, #11245, #48288, #17161, #42794, #49528, #29352, #75221, #67667, #62580, #3273, #10004, #35669, #61333, #3687, #19191, #19609, #64233, #57484, #6149, #13312, #12894, #70123, #77279, #51576, #32239, #24678, #6568, #83177, #63810, #31823, #82360, #57897, #45271, #25497, #62994, #58320, #264, #38136, #31404, #69722, #51163, #12066, #25917, #12474, #37724, #50346, #70967, #43612, #38965, #64648, #6985, #30991, #76859, #44840, #76044, #32654, #24265, #70538, #5333, #49938, #75636, #38553, #57069, #63398, #17974, #5733, #69313, #11663, #82763, #18388, #37322, #56659, #44029, #25085, #50758, #76458, #18785, #44429, #8662, #52415, #71383, #66748, #52000, #79377, #33080, #77705, #20458, #20035, #47359, #14982, #20874, #59998, #53670, #45686, #72227, #13732, #14577, #78124, #34334, #9083, #7410, #7834, #34754, #21696, #65071, #41059, #26760, #46527, #58747, #2354, #73048, #21288, #26339, #72634, #15397, #33501, #28010, #40229, #1521, #8248, #46110, #39386, #1109, #65911, #71803, #59163, #683, #27175, #52838, #78549, #40641, #33913, #14156, #39812, #65502, #59577, #1934, #27597, #53256, #78968, #46942, #66323, #74300, #81037, #42703, #48605, #67570, #10329, #23349, #36396, #41474, #80627, #23765, #60823, #9902, #35991, #35573, #41876, #61661, #9488, #62071, #73476, #22531, #68400, #80215, #67159, #55328, #55740, #17066, #4002, #42286, #49436, #49020, #22938, #30077, #4409, #10739, #3174, #81448, #29667, #61236, #3591, #75130, #28424, #74717, #48193, #47775, #73889, #17475, #16646, #29256, #15826, #43106, #35162, #16229, #28838, #67984, #54501, #22115, #54920, #68802, #11148, #60414, #2765, #54084, #79799, #36806, #30495, #82671, #24173, #31726, #17881, #18695, #5235, #51478, #83081, #12797, #51066, #44337, #57798, #11564, #11973, #25818, #43516, #43934, #44745, #19096, #63714, #24987, #30899, #62482, #19512, #38039, #25403, #69215, #37223, #70440, #50662, #76766, #6054, #62900, #56566, #82267, #38453, #76362, #70028, #24585, #64139, #18289, #5642, #37628, #57390, #69628, #6472, #75541, #50252, #12381, #75949, #32142, #165, #63304, #31309, #77181, #45166, #56973, #70872, #4817, #81861, #56158, #49842, #1833, #33404, #77607, #8149, #8562, #27493, #59893, #2245, #53570, #26664, #21188, #20354, #66224, #72118, #46427, #78862, #19940, #584, #46842, #39283, #65816, #40130, #71701, #52319, #52737, #27911, #72536, #47256, #58218, #32555, #1421, #78025, #33814, #21594, #71283, #58643, #32976, #14477, #14884, #59479, #78447, #20773, #13631, #53150, #40544, #34231, #51900, #13221, #79279, #27077, #46005, #1011, #38869, #14055, #64548, #6885, #39710, #64970, #26239, #45590, #7306, #65401, #7738, #59066, #35056, #55222, #80929, #41372, #60314, #55632, #40958, #68300, #22012, #66640, #9386, #8977, #36291, #3900, #9797, #48914, #42598, #34650, #61133 ),
 ( #73788, #10636, #2663, #16542, #60722, #28322, #3072, #22836, #35469, #48088, #53983, #74615, #47672, #28738, #15716, #54820, #67053, #79695, #73367, #61965, #29560, #35887, #16124, #54399, #4304, #72945, #80111, #3485, #22429, #67882, #41770, #80524, #67463, #29967, #61557, #16959, #23244, #48495, #81341, #29151, #74196, #23656, #42187, #10220, #15297, #31618, #76256, #11872, #43409, #75028, #32038, #50553, #37935, #56049, #49737, #57280, #37524, #12278, #18591, #81758, #75437, #11456, #63612, #5539, #63198, #17776, #25296, #30796, #18185, #50146, #12692, #5949, #69522, #50962, #18992, #43003, #31204, #68697, #56871, #69108, #82977, #57697, #24068, #56462, #59, #44640, #30383, #6366, #37114, #82565, #62798, #76659, #38351, #69923, #17373, #70337, #64026, #82164, #49326, #24884, #75843, #44234, #5132, #11038, #36696, #62371, #4709, #24480, #43818, #52219, #77922, #909, #66859, #13951, #9601, #77076, #19410, #60934, #58542, #45061, #39609, #51796, #22225, #6779, #65298, #47469, #9190, #7636, #32874, #58968, #73161, #2873, #32451, #45902, #73587, #26134, #26565, #1325, #20253, #7203, #26974, #58113, #28536, #38766, #71182, #34862, #45485, #479, #21805, #47881, #60524, #52639, #33307, #15931, #15510, #71599, #79909, #54193, #41578, #77501, #67268, #79490, #41169, #35269, #19836, #25713, #51373, #70764, #64443, #13114, #13524, #39180, #64864, #48713, #42806, #74411, #36916, #74828, #16755, #29364, #62592, #22639, #49950, #43624, #81964, #10016, #42394, #68906, #11258, #55024, #73996, #69326, #54614, #24279, #35681, #80324, #23046, #48299, #68093, #36500, #36095, #4106, #75648, #16343, #30183, #10438, #41986, #61766, #62176, #49122, #29772, #67680, #4935, #61347, #55433, #80732, #68500, #81142, #3700, #23457, #17988, #17577, #49539, #17172, #10840, #56268, #3284, #4514, #55845, #81554, #23872, #75234, #43210, #30602, #11676, #37333, #28949, #77291, #70551, #695, #37737, #38150, #52012, #44042, #70135, #70979, #45284, #6580, #25511, #57081, #5345, #45699, #64245, #51590, #69735, #63411, #13324, #51176, #25931, #32251, #12079, #5746, #25098, #19622, #19204, #76872, #31417, #38977, #44442, #31836, #63822, #57912, #12486, #276, #18400, #82776, #44853, #50770, #12906, #38565, #6161, #57497, #64660, #26351, #76471, #18798, #6999, #24691, #83188, #32666, #58333, #77717, #20047, #71395, #13744, #63006, #31004, #56672, #82372, #50359, #76056, #46538, #9094, #14994, #72644, #21707, #20470, #26772, #73061, #65513, #8673, #66335, #14587, #78561, #78978, #28437, #15411, #73488, #1121, #58759, #27607, #52850, #34344, #47786, #14168, #1532, #59174, #7422, #2777, #53680, #59588, #41071, #34767, #33092, #53268, #52427, #21299, #7845, #47371, #22128, #46123, #72238, #39401, #60426, #71818, #79811, #33512, #1945, #39825, #66760, #54096, #60009, #65084, #28021, #78137, #40240, #27186, #46952, #65923, #40651, #20887, #8260, #33925, #2365, #79388, #48618, #15838, #42299, #67996, #74312, #55752, #4014, #81873, #67172, #9501, #49854, #16659, #35174, #29678, #41889, #11161, #80227, #55341, #36407, #81460, #81049, #22951, #49032, #62082, #75142, #22543, #36003, #62495, #16242, #10342, #74728, #61673, #80639, #17077, #48206, #17487, #28851, #61249, #23777, #35586, #73901, #10750, #36820, #49448, #42714, #23361, #4830, #4422, #68410, #68815, #43118, #30508, #67582, #56170, #30089, #24185, #41486, #9914, #60835, #3187, #54513, #3603, #29268, #54932, #6066, #82682, #37639, #31737, #63316, #25830, #63726, #5654, #18301, #51489, #11576, #38882, #32569, #70883, #82279, #31320, #57810, #177, #43945, #62914, #58231, #43530, #13232, #24597, #69229, #12393, #56578, #70452, #64561, #64150, #6898, #598, #26254, #56985, #77192, #24999, #45177, #51078, #25414, #19524, #50265, #5247, #75554, #69640, #44756, #19108 ) ),
 .UNSPECIFIED., .F., .F., .F. ) 
 B_SPLINE_SURFACE_WITH_KNOTS ( ( 2, 2 ),
 ( 3, 2, 2, 2, 2, 2, 2, 2, 2, 2, 2, 2, 2, 2, 2, 2, 2, 2, 2, 2, 2, 2, 2, 2, 2, 2, 2, 2, 2, 2, 2, 2, 2, 2, 2, 2, 2, 2, 2, 2, 2, 2, 2, 2, 2, 2, 2, 2, 2, 2, 2, 2, 2, 2, 2, 2, 2, 2, 2, 2, 2, 2, 2, 2, 2, 2, 2, 2, 2, 2, 2, 2, 2, 2, 2, 2, 2, 2, 2, 2, 2, 2, 2, 2, 2, 2, 2, 2, 2, 2, 2, 2, 2, 2, 2, 2, 2, 2, 2, 2, 2, 2, 2, 2, 2, 2, 2, 2, 2, 2, 2, 2, 2, 2, 2, 2, 2, 2, 2, 2, 2, 2, 2, 2, 2, 2, 2, 2, 2, 2, 2, 2, 2, 2, 2, 2, 2, 2, 2, 2, 2, 2, 2, 2, 2, 2, 2, 2, 2, 2, 2, 2, 2, 2, 2, 2, 2, 2, 2, 2, 2, 2, 2, 2, 2, 2, 2, 2, 2, 2, 2, 2, 2, 2, 2, 2, 2, 2, 2, 2, 2, 2, 2, 2, 2, 2, 2, 2, 2, 2, 2, 2, 2, 2, 2, 2, 2, 2, 2, 2, 2, 2, 2, 2, 2, 2, 2, 2, 2, 2, 2, 2, 2, 2, 2, 2, 2, 2, 2, 2, 2, 2, 2, 2, 2, 2, 2, 2, 2, 2, 2, 2, 2, 2, 2, 2, 2, 3 ),
 ( 0.000000000000000000, 1.000000000000000000 ),
 ( 0.000000000000000000, 0.004166666666666666609, 0.008333333333333333218, 0.01250000000000000069, 0.01666666666666666644, 0.02083333333333333218, 0.02500000000000000139, 0.02916666666666666713, 0.03333333333333333287, 0.03749999999999999861, 0.04166666666666666435, 0.04583333333333333010, 0.05000000000000000278, 0.05416666666666666852, 0.05833333333333333426, 0.06250000000000000000, 0.06666666666666666574, 0.07083333333333333148, 0.07499999999999999722, 0.07916666666666666297, 0.08333333333333332871, 0.08749999999999999445, 0.09166666666666666019, 0.09583333333333333981, 0.1000000000000000056, 0.1041666666666666713, 0.1083333333333333370, 0.1125000000000000028, 0.1166666666666666685, 0.1208333333333333343, 0.1250000000000000000, 0.1291666666666666796, 0.1333333333333333315, 0.1375000000000000111, 0.1416666666666666630, 0.1458333333333333426, 0.1499999999999999944, 0.1541666666666666741, 0.1583333333333333259, 0.1625000000000000056, 0.1666666666666666574, 0.1708333333333333370, 0.1749999999999999889, 0.1791666666666666685, 0.1833333333333333204, 0.1875000000000000000, 0.1916666666666666796, 0.1958333333333333315, 0.2000000000000000111, 0.2041666666666666630, 0.2083333333333333426, 0.2124999999999999944, 0.2166666666666666741, 0.2208333333333333259, 0.2250000000000000056, 0.2291666666666666574, 0.2333333333333333370, 0.2374999999999999889, 0.2416666666666666685, 0.2458333333333333204, 0.2500000000000000000, 0.2541666666666666519, 0.2583333333333333592, 0.2625000000000000111, 0.2666666666666666630, 0.2708333333333333148, 0.2750000000000000222, 0.2791666666666666741, 0.2833333333333333259, 0.2874999999999999778, 0.2916666666666666852, 0.2958333333333333370, 0.2999999999999999889, 0.3041666666666666408, 0.3083333333333333481, 0.3125000000000000000, 0.3166666666666666519, 0.3208333333333333592, 0.3250000000000000111, 0.3291666666666666630, 0.3333333333333333148, 0.3375000000000000222, 0.3416666666666666741, 0.3458333333333333259, 0.3499999999999999778, 0.3541666666666666852, 0.3583333333333333370, 0.3624999999999999889, 0.3666666666666666408, 0.3708333333333333481, 0.3750000000000000000, 0.3791666666666666519, 0.3833333333333333592, 0.3875000000000000111, 0.3916666666666666630, 0.3958333333333333148, 0.4000000000000000222, 0.4041666666666666741, 0.4083333333333333259, 0.4124999999999999778, 0.4166666666666666852, 0.4208333333333333370, 0.4249999999999999889, 0.4291666666666666408, 0.4333333333333333481, 0.4375000000000000000, 0.4416666666666666519, 0.4458333333333333592, 0.4500000000000000111, 0.4541666666666666630, 0.4583333333333333148, 0.4625000000000000222, 0.4666666666666666741, 0.4708333333333333259, 0.4749999999999999778, 0.4791666666666666852, 0.4833333333333333370, 0.4874999999999999889, 0.4916666666666666408, 0.4958333333333333481, 0.5000000000000000000, 0.5041666666666666519, 0.5083333333333333037, 0.5124999999999999556, 0.5166666666666667185, 0.5208333333333333703, 0.5250000000000000222, 0.5291666666666666741, 0.5333333333333333259, 0.5374999999999999778, 0.5416666666666666297, 0.5458333333333332815, 0.5500000000000000444, 0.5541666666666666963, 0.5583333333333333481, 0.5625000000000000000, 0.5666666666666666519, 0.5708333333333333037, 0.5749999999999999556, 0.5791666666666667185, 0.5833333333333333703, 0.5875000000000000222, 0.5916666666666666741, 0.5958333333333333259, 0.5999999999999999778, 0.6041666666666666297, 0.6083333333333332815, 0.6125000000000000444, 0.6166666666666666963, 0.6208333333333333481, 0.6250000000000000000, 0.6291666666666666519, 0.6333333333333333037, 0.6374999999999999556, 0.6416666666666667185, 0.6458333333333333703, 0.6500000000000000222, 0.6541666666666666741, 0.6583333333333333259, 0.6624999999999999778, 0.6666666666666666297, 0.6708333333333332815, 0.6750000000000000444, 0.6791666666666666963, 0.6833333333333333481, 0.6875000000000000000, 0.6916666666666666519, 0.6958333333333333037, 0.6999999999999999556, 0.7041666666666667185, 0.7083333333333333703, 0.7125000000000000222, 0.7166666666666666741, 0.7208333333333333259, 0.7249999999999999778, 0.7291666666666666297, 0.7333333333333332815, 0.7375000000000000444, 0.7416666666666666963, 0.7458333333333333481, 0.7500000000000000000, 0.7541666666666666519, 0.7583333333333333037, 0.7624999999999999556, 0.7666666666666667185, 0.7708333333333333703, 0.7750000000000000222, 0.7791666666666666741, 0.7833333333333333259, 0.7874999999999999778, 0.7916666666666666297, 0.7958333333333332815, 0.8000000000000000444, 0.8041666666666666963, 0.8083333333333333481, 0.8125000000000000000, 0.8166666666666666519, 0.8208333333333333037, 0.8249999999999999556, 0.8291666666666667185, 0.8333333333333333703, 0.8375000000000000222, 0.8416666666666666741, 0.8458333333333333259, 0.8499999999999999778, 0.8541666666666666297, 0.8583333333333332815, 0.8625000000000000444, 0.8666666666666666963, 0.8708333333333333481, 0.8750000000000000000, 0.8791666666666666519, 0.8833333333333333037, 0.8874999999999999556, 0.8916666666666667185, 0.8958333333333333703, 0.9000000000000000222, 0.9041666666666666741, 0.9083333333333333259, 0.9124999999999999778, 0.9166666666666666297, 0.9208333333333332815, 0.9250000000000000444, 0.9291666666666666963, 0.9333333333333333481, 0.9375000000000000000, 0.9416666666666666519, 0.9458333333333333037, 0.9499999999999999556, 0.9541666666666667185, 0.9583333333333333703, 0.9625000000000000222, 0.9666666666666666741, 0.9708333333333333259, 0.9749999999999999778, 0.9791666666666666297, 0.9833333333333332815, 0.9875000000000000444 ),
 .UNSPECIFIED. ) 
 GEOMETRIC_REPRESENTATION_ITEM ( )  RATIONAL_B_SPLINE_SURFACE ( (
 ( 1.000000000000000000, 0.9659258262890683122, 1.000000000000000000, 0.9659258262890683122, 1.000000000000000000, 0.9659258262890683122, 1.000000000000000000, 0.9659258262890683122, 1.000000000000000000, 0.9659258262890683122, 1.000000000000000000, 0.9659258262890683122, 1.000000000000000000, 0.9659258262890683122, 1.000000000000000000, 0.9659258262890683122, 1.000000000000000000, 0.9659258262890683122, 1.000000000000000000, 0.9659258262890683122, 1.000000000000000000, 0.9659258262890683122, 1.000000000000000000, 0.9659258262890683122, 1.000000000000000000, 0.9659258262890683122, 1.000000000000000000, 0.9659258262890683122, 1.000000000000000000, 0.9659258262890683122, 1.000000000000000000, 0.9659258262890683122, 1.000000000000000000, 0.9659258262890683122, 1.000000000000000000, 0.9659258262890683122, 1.000000000000000000, 0.9659258262890683122, 1.000000000000000000, 0.9659258262890683122, 1.000000000000000000, 0.9659258262890683122, 1.000000000000000000, 0.9659258262890683122, 1.000000000000000000, 0.9659258262890683122, 1.000000000000000000, 0.9659258262890683122, 1.000000000000000000, 0.9659258262890683122, 1.000000000000000000, 0.9659258262890683122, 1.000000000000000000, 0.9659258262890683122, 1.000000000000000000, 0.9659258262890683122, 1.000000000000000000, 0.9659258262890683122, 1.000000000000000000, 0.9659258262890683122, 1.000000000000000000, 0.9659258262890683122, 1.000000000000000000, 0.9659258262890683122, 1.000000000000000000, 0.9659258262890683122, 1.000000000000000000, 0.9659258262890683122, 1.000000000000000000, 0.9659258262890683122, 1.000000000000000000, 0.9659258262890683122, 1.000000000000000000, 0.9659258262890683122, 1.000000000000000000, 0.9659258262890683122, 1.000000000000000000, 0.9659258262890683122, 1.000000000000000000, 0.9659258262890683122, 1.000000000000000000, 0.9659258262890683122, 1.000000000000000000, 0.9659258262890683122, 1.000000000000000000, 0.9659258262890683122, 1.000000000000000000, 0.9659258262890683122, 1.000000000000000000, 0.9659258262890683122, 1.000000000000000000, 0.9659258262890683122, 1.000000000000000000, 0.9659258262890683122, 1.000000000000000000, 0.9659258262890683122, 1.000000000000000000, 0.9659258262890683122, 1.000000000000000000, 0.9659258262890683122, 1.000000000000000000, 0.9659258262890683122, 1.000000000000000000, 0.9659258262890683122, 1.000000000000000000, 0.9659258262890683122, 1.000000000000000000, 0.9659258262890683122, 1.000000000000000000, 0.9659258262890683122, 1.000000000000000000, 0.9659258262890683122, 1.000000000000000000, 0.9659258262890683122, 1.000000000000000000, 0.9659258262890683122, 1.000000000000000000, 0.9659258262890683122, 1.000000000000000000, 0.9659258262890683122, 1.000000000000000000, 0.9659258262890683122, 1.000000000000000000, 0.9659258262890683122, 1.000000000000000000, 0.9659258262890683122, 1.000000000000000000, 0.9659258262890683122, 1.000000000000000000, 0.9659258262890683122, 1.000000000000000000, 0.9659258262890683122, 1.000000000000000000, 0.9659258262890683122, 1.000000000000000000, 0.9659258262890683122, 1.000000000000000000, 0.9659258262890683122, 1.000000000000000000, 0.9659258262890683122, 1.000000000000000000, 0.9659258262890683122, 1.000000000000000000, 0.9659258262890683122, 1.000000000000000000, 0.9659258262890683122, 1.000000000000000000, 0.9659258262890683122, 1.000000000000000000, 0.9659258262890683122, 1.000000000000000000, 0.9659258262890683122, 1.000000000000000000, 0.9659258262890683122, 1.000000000000000000, 0.9659258262890683122, 1.000000000000000000, 0.9659258262890683122, 1.000000000000000000, 0.9659258262890683122, 1.000000000000000000, 0.9659258262890683122, 1.000000000000000000, 0.9659258262890683122, 1.000000000000000000, 0.9659258262890683122, 1.000000000000000000, 0.9659258262890683122, 1.000000000000000000, 0.9659258262890683122, 1.000000000000000000, 0.9659258262890683122, 1.000000000000000000, 0.9659258262890683122, 1.000000000000000000, 0.9659258262890683122, 1.000000000000000000, 0.9659258262890683122, 1.000000000000000000, 0.9659258262890683122, 1.000000000000000000, 0.9659258262890683122, 1.000000000000000000, 0.9659258262890683122, 1.000000000000000000, 0.9659258262890683122, 1.000000000000000000, 0.9659258262890683122, 1.000000000000000000, 0.9659258262890683122, 1.000000000000000000, 0.9659258262890683122, 1.000000000000000000, 0.9659258262890683122, 1.000000000000000000, 0.9659258262890683122, 1.000000000000000000, 0.9659258262890683122, 1.000000000000000000, 0.9659258262890683122, 1.000000000000000000, 0.9659258262890683122, 1.000000000000000000, 0.9659258262890683122, 1.000000000000000000, 0.9659258262890683122, 1.000000000000000000, 0.9659258262890683122, 1.000000000000000000, 0.9659258262890683122, 1.000000000000000000, 0.9659258262890683122, 1.000000000000000000, 0.9659258262890683122, 1.000000000000000000, 0.9659258262890683122, 1.000000000000000000, 0.9659258262890683122, 1.000000000000000000, 0.9659258262890683122, 1.000000000000000000, 0.9659258262890683122, 1.000000000000000000, 0.9659258262890683122, 1.000000000000000000, 0.9659258262890683122, 1.000000000000000000, 0.9659258262890683122, 1.000000000000000000, 0.9659258262890683122, 1.000000000000000000, 0.9659258262890683122, 1.000000000000000000, 0.9659258262890683122, 1.000000000000000000, 0.9659258262890683122, 1.000000000000000000, 0.9659258262890683122, 1.000000000000000000, 0.9659258262890683122, 1.000000000000000000, 0.9659258262890683122, 1.000000000000000000, 0.9659258262890683122, 1.000000000000000000, 0.9659258262890683122, 1.000000000000000000, 0.9659258262890683122, 1.000000000000000000, 0.9659258262890683122, 1.000000000000000000, 0.9659258262890683122, 1.000000000000000000, 0.9659258262890683122, 1.000000000000000000, 0.9659258262890683122, 1.000000000000000000, 0.9659258262890683122, 1.000000000000000000, 0.9659258262890683122, 1.000000000000000000, 0.9659258262890683122, 1.000000000000000000, 0.9659258262890683122, 1.000000000000000000, 0.9659258262890683122, 1.000000000000000000, 0.9659258262890683122, 1.000000000000000000, 0.9659258262890683122, 1.000000000000000000, 0.9659258262890683122, 1.000000000000000000, 0.9659258262890683122, 1.000000000000000000, 0.9659258262890683122, 1.000000000000000000, 0.9659258262890683122, 1.000000000000000000, 0.9659258262890683122, 1.000000000000000000, 0.9659258262890683122, 1.000000000000000000, 0.9659258262890683122, 1.000000000000000000, 0.9659258262890683122, 1.000000000000000000, 0.9659258262890683122, 1.000000000000000000, 0.9659258262890683122, 1.000000000000000000, 0.9659258262890683122, 1.000000000000000000, 0.9659258262890683122, 1.000000000000000000, 0.9659258262890683122, 1.000000000000000000, 0.9659258262890683122, 1.000000000000000000, 0.9659258262890683122, 1.000000000000000000, 0.9659258262890683122, 1.000000000000000000, 0.9659258262890683122, 1.000000000000000000, 0.9659258262890683122, 1.000000000000000000, 0.9659258262890683122, 1.000000000000000000, 0.9659258262890683122, 1.000000000000000000, 0.9659258262890683122, 1.000000000000000000, 0.9659258262890683122, 1.000000000000000000, 0.9659258262890683122, 1.000000000000000000, 0.9659258262890683122, 1.000000000000000000, 0.9659258262890683122, 1.000000000000000000, 0.9659258262890683122, 1.000000000000000000, 0.9659258262890683122, 1.000000000000000000, 0.9659258262890683122, 1.000000000000000000, 0.9659258262890683122, 1.000000000000000000, 0.9659258262890683122, 1.000000000000000000, 0.9659258262890683122, 1.000000000000000000, 0.9659258262890683122, 1.000000000000000000, 0.9659258262890683122, 1.000000000000000000, 0.9659258262890683122, 1.000000000000000000, 0.9659258262890683122, 1.000000000000000000, 0.9659258262890683122, 1.000000000000000000, 0.9659258262890683122, 1.000000000000000000, 0.9659258262890683122, 1.000000000000000000, 0.9659258262890683122, 1.000000000000000000, 0.9659258262890683122, 1.000000000000000000, 0.9659258262890683122, 1.000000000000000000, 0.9659258262890683122, 1.000000000000000000, 0.9659258262890683122, 1.000000000000000000, 0.9659258262890683122, 1.000000000000000000, 0.9659258262890683122, 1.000000000000000000, 0.9659258262890683122, 1.000000000000000000, 0.9659258262890683122, 1.000000000000000000, 0.9659258262890683122, 1.000000000000000000, 0.9659258262890683122, 1.000000000000000000, 0.9659258262890683122, 1.000000000000000000, 0.9659258262890683122, 1.000000000000000000, 0.9659258262890683122, 1.000000000000000000, 0.9659258262890683122, 1.000000000000000000, 0.9659258262890683122, 1.000000000000000000, 0.9659258262890683122, 1.000000000000000000, 0.9659258262890683122, 1.000000000000000000, 0.9659258262890683122, 1.000000000000000000, 0.9659258262890683122, 1.000000000000000000, 0.9659258262890683122, 1.000000000000000000, 0.9659258262890683122, 1.000000000000000000, 0.9659258262890683122, 1.000000000000000000, 0.9659258262890683122, 1.000000000000000000, 0.9659258262890683122, 1.000000000000000000, 0.9659258262890683122, 1.000000000000000000, 0.9659258262890683122, 1.000000000000000000, 0.9659258262890683122, 1.000000000000000000, 0.9659258262890683122, 1.000000000000000000, 0.9659258262890683122, 1.000000000000000000, 0.9659258262890683122, 1.000000000000000000, 0.9659258262890683122, 1.000000000000000000, 0.9659258262890683122, 1.000000000000000000, 0.9659258262890683122, 1.000000000000000000, 0.9659258262890683122, 1.000000000000000000, 0.9659258262890683122, 1.000000000000000000, 0.9659258262890683122, 1.000000000000000000, 0.9659258262890683122, 1.000000000000000000, 0.9659258262890683122, 1.000000000000000000, 0.9659258262890683122, 1.000000000000000000, 0.9659258262890683122, 1.000000000000000000, 0.9659258262890683122, 1.000000000000000000, 0.9659258262890683122, 1.000000000000000000, 0.9659258262890683122, 1.000000000000000000, 0.9659258262890683122, 1.000000000000000000, 0.9659258262890683122, 1.000000000000000000, 0.9659258262890683122, 1.000000000000000000, 0.9659258262890683122, 1.000000000000000000, 0.9659258262890683122, 1.000000000000000000, 0.9659258262890683122, 1.000000000000000000, 0.9659258262890683122, 1.000000000000000000, 0.9659258262890683122, 1.000000000000000000, 0.9659258262890683122, 1.000000000000000000, 0.9659258262890683122, 1.000000000000000000, 0.9659258262890683122, 1.000000000000000000, 0.9659258262890683122, 1.000000000000000000, 0.9659258262890683122, 1.000000000000000000, 0.9659258262890683122, 1.000000000000000000, 0.9659258262890683122, 1.000000000000000000, 0.9659258262890683122, 1.000000000000000000, 0.9659258262890683122, 1.000000000000000000, 0.9659258262890683122, 1.000000000000000000, 0.9659258262890683122, 1.000000000000000000, 0.9659258262890683122, 1.000000000000000000),
 ( 1.000000000000000000, 0.9659258262890683122, 1.000000000000000000, 0.9659258262890683122, 1.000000000000000000, 0.9659258262890683122, 1.000000000000000000, 0.9659258262890683122, 1.000000000000000000, 0.9659258262890683122, 1.000000000000000000, 0.9659258262890683122, 1.000000000000000000, 0.9659258262890683122, 1.000000000000000000, 0.9659258262890683122, 1.000000000000000000, 0.9659258262890683122, 1.000000000000000000, 0.9659258262890683122, 1.000000000000000000, 0.9659258262890683122, 1.000000000000000000, 0.9659258262890683122, 1.000000000000000000, 0.9659258262890683122, 1.000000000000000000, 0.9659258262890683122, 1.000000000000000000, 0.9659258262890683122, 1.000000000000000000, 0.9659258262890683122, 1.000000000000000000, 0.9659258262890683122, 1.000000000000000000, 0.9659258262890683122, 1.000000000000000000, 0.9659258262890683122, 1.000000000000000000, 0.9659258262890683122, 1.000000000000000000, 0.9659258262890683122, 1.000000000000000000, 0.9659258262890683122, 1.000000000000000000, 0.9659258262890683122, 1.000000000000000000, 0.9659258262890683122, 1.000000000000000000, 0.9659258262890683122, 1.000000000000000000, 0.9659258262890683122, 1.000000000000000000, 0.9659258262890683122, 1.000000000000000000, 0.9659258262890683122, 1.000000000000000000, 0.9659258262890683122, 1.000000000000000000, 0.9659258262890683122, 1.000000000000000000, 0.9659258262890683122, 1.000000000000000000, 0.9659258262890683122, 1.000000000000000000, 0.9659258262890683122, 1.000000000000000000, 0.9659258262890683122, 1.000000000000000000, 0.9659258262890683122, 1.000000000000000000, 0.9659258262890683122, 1.000000000000000000, 0.9659258262890683122, 1.000000000000000000, 0.9659258262890683122, 1.000000000000000000, 0.9659258262890683122, 1.000000000000000000, 0.9659258262890683122, 1.000000000000000000, 0.9659258262890683122, 1.000000000000000000, 0.9659258262890683122, 1.000000000000000000, 0.9659258262890683122, 1.000000000000000000, 0.9659258262890683122, 1.000000000000000000, 0.9659258262890683122, 1.000000000000000000, 0.9659258262890683122, 1.000000000000000000, 0.9659258262890683122, 1.000000000000000000, 0.9659258262890683122, 1.000000000000000000, 0.9659258262890683122, 1.000000000000000000, 0.9659258262890683122, 1.000000000000000000, 0.9659258262890683122, 1.000000000000000000, 0.9659258262890683122, 1.000000000000000000, 0.9659258262890683122, 1.000000000000000000, 0.9659258262890683122, 1.000000000000000000, 0.9659258262890683122, 1.000000000000000000, 0.9659258262890683122, 1.000000000000000000, 0.9659258262890683122, 1.000000000000000000, 0.9659258262890683122, 1.000000000000000000, 0.9659258262890683122, 1.000000000000000000, 0.9659258262890683122, 1.000000000000000000, 0.9659258262890683122, 1.000000000000000000, 0.9659258262890683122, 1.000000000000000000, 0.9659258262890683122, 1.000000000000000000, 0.9659258262890683122, 1.000000000000000000, 0.9659258262890683122, 1.000000000000000000, 0.9659258262890683122, 1.000000000000000000, 0.9659258262890683122, 1.000000000000000000, 0.9659258262890683122, 1.000000000000000000, 0.9659258262890683122, 1.000000000000000000, 0.9659258262890683122, 1.000000000000000000, 0.9659258262890683122, 1.000000000000000000, 0.9659258262890683122, 1.000000000000000000, 0.9659258262890683122, 1.000000000000000000, 0.9659258262890683122, 1.000000000000000000, 0.9659258262890683122, 1.000000000000000000, 0.9659258262890683122, 1.000000000000000000, 0.9659258262890683122, 1.000000000000000000, 0.9659258262890683122, 1.000000000000000000, 0.9659258262890683122, 1.000000000000000000, 0.9659258262890683122, 1.000000000000000000, 0.9659258262890683122, 1.000000000000000000, 0.9659258262890683122, 1.000000000000000000, 0.9659258262890683122, 1.000000000000000000, 0.9659258262890683122, 1.000000000000000000, 0.9659258262890683122, 1.000000000000000000, 0.9659258262890683122, 1.000000000000000000, 0.9659258262890683122, 1.000000000000000000, 0.9659258262890683122, 1.000000000000000000, 0.9659258262890683122, 1.000000000000000000, 0.9659258262890683122, 1.000000000000000000, 0.9659258262890683122, 1.000000000000000000, 0.9659258262890683122, 1.000000000000000000, 0.9659258262890683122, 1.000000000000000000, 0.9659258262890683122, 1.000000000000000000, 0.9659258262890683122, 1.000000000000000000, 0.9659258262890683122, 1.000000000000000000, 0.9659258262890683122, 1.000000000000000000, 0.9659258262890683122, 1.000000000000000000, 0.9659258262890683122, 1.000000000000000000, 0.9659258262890683122, 1.000000000000000000, 0.9659258262890683122, 1.000000000000000000, 0.9659258262890683122, 1.000000000000000000, 0.9659258262890683122, 1.000000000000000000, 0.9659258262890683122, 1.000000000000000000, 0.9659258262890683122, 1.000000000000000000, 0.9659258262890683122, 1.000000000000000000, 0.9659258262890683122, 1.000000000000000000, 0.9659258262890683122, 1.000000000000000000, 0.9659258262890683122, 1.000000000000000000, 0.9659258262890683122, 1.000000000000000000, 0.9659258262890683122, 1.000000000000000000, 0.9659258262890683122, 1.000000000000000000, 0.9659258262890683122, 1.000000000000000000, 0.9659258262890683122, 1.000000000000000000, 0.9659258262890683122, 1.000000000000000000, 0.9659258262890683122, 1.000000000000000000, 0.9659258262890683122, 1.000000000000000000, 0.9659258262890683122, 1.000000000000000000, 0.9659258262890683122, 1.000000000000000000, 0.9659258262890683122, 1.000000000000000000, 0.9659258262890683122, 1.000000000000000000, 0.9659258262890683122, 1.000000000000000000, 0.9659258262890683122, 1.000000000000000000, 0.9659258262890683122, 1.000000000000000000, 0.9659258262890683122, 1.000000000000000000, 0.9659258262890683122, 1.000000000000000000, 0.9659258262890683122, 1.000000000000000000, 0.9659258262890683122, 1.000000000000000000, 0.9659258262890683122, 1.000000000000000000, 0.9659258262890683122, 1.000000000000000000, 0.9659258262890683122, 1.000000000000000000, 0.9659258262890683122, 1.000000000000000000, 0.9659258262890683122, 1.000000000000000000, 0.9659258262890683122, 1.000000000000000000, 0.9659258262890683122, 1.000000000000000000, 0.9659258262890683122, 1.000000000000000000, 0.9659258262890683122, 1.000000000000000000, 0.9659258262890683122, 1.000000000000000000, 0.9659258262890683122, 1.000000000000000000, 0.9659258262890683122, 1.000000000000000000, 0.9659258262890683122, 1.000000000000000000, 0.9659258262890683122, 1.000000000000000000, 0.9659258262890683122, 1.000000000000000000, 0.9659258262890683122, 1.000000000000000000, 0.9659258262890683122, 1.000000000000000000, 0.9659258262890683122, 1.000000000000000000, 0.9659258262890683122, 1.000000000000000000, 0.9659258262890683122, 1.000000000000000000, 0.9659258262890683122, 1.000000000000000000, 0.9659258262890683122, 1.000000000000000000, 0.9659258262890683122, 1.000000000000000000, 0.9659258262890683122, 1.000000000000000000, 0.9659258262890683122, 1.000000000000000000, 0.9659258262890683122, 1.000000000000000000, 0.9659258262890683122, 1.000000000000000000, 0.9659258262890683122, 1.000000000000000000, 0.9659258262890683122, 1.000000000000000000, 0.9659258262890683122, 1.000000000000000000, 0.9659258262890683122, 1.000000000000000000, 0.9659258262890683122, 1.000000000000000000, 0.9659258262890683122, 1.000000000000000000, 0.9659258262890683122, 1.000000000000000000, 0.9659258262890683122, 1.000000000000000000, 0.9659258262890683122, 1.000000000000000000, 0.9659258262890683122, 1.000000000000000000, 0.9659258262890683122, 1.000000000000000000, 0.9659258262890683122, 1.000000000000000000, 0.9659258262890683122, 1.000000000000000000, 0.9659258262890683122, 1.000000000000000000, 0.9659258262890683122, 1.000000000000000000, 0.9659258262890683122, 1.000000000000000000, 0.9659258262890683122, 1.000000000000000000, 0.9659258262890683122, 1.000000000000000000, 0.9659258262890683122, 1.000000000000000000, 0.9659258262890683122, 1.000000000000000000, 0.9659258262890683122, 1.000000000000000000, 0.9659258262890683122, 1.000000000000000000, 0.9659258262890683122, 1.000000000000000000, 0.9659258262890683122, 1.000000000000000000, 0.9659258262890683122, 1.000000000000000000, 0.9659258262890683122, 1.000000000000000000, 0.9659258262890683122, 1.000000000000000000, 0.9659258262890683122, 1.000000000000000000, 0.9659258262890683122, 1.000000000000000000, 0.9659258262890683122, 1.000000000000000000, 0.9659258262890683122, 1.000000000000000000, 0.9659258262890683122, 1.000000000000000000, 0.9659258262890683122, 1.000000000000000000, 0.9659258262890683122, 1.000000000000000000, 0.9659258262890683122, 1.000000000000000000, 0.9659258262890683122, 1.000000000000000000, 0.9659258262890683122, 1.000000000000000000, 0.9659258262890683122, 1.000000000000000000, 0.9659258262890683122, 1.000000000000000000, 0.9659258262890683122, 1.000000000000000000, 0.9659258262890683122, 1.000000000000000000, 0.9659258262890683122, 1.000000000000000000, 0.9659258262890683122, 1.000000000000000000, 0.9659258262890683122, 1.000000000000000000, 0.9659258262890683122, 1.000000000000000000, 0.9659258262890683122, 1.000000000000000000, 0.9659258262890683122, 1.000000000000000000, 0.9659258262890683122, 1.000000000000000000, 0.9659258262890683122, 1.000000000000000000, 0.9659258262890683122, 1.000000000000000000, 0.9659258262890683122, 1.000000000000000000, 0.9659258262890683122, 1.000000000000000000, 0.9659258262890683122, 1.000000000000000000, 0.9659258262890683122, 1.000000000000000000, 0.9659258262890683122, 1.000000000000000000, 0.9659258262890683122, 1.000000000000000000, 0.9659258262890683122, 1.000000000000000000, 0.9659258262890683122, 1.000000000000000000, 0.9659258262890683122, 1.000000000000000000, 0.9659258262890683122, 1.000000000000000000, 0.9659258262890683122, 1.000000000000000000, 0.9659258262890683122, 1.000000000000000000, 0.9659258262890683122, 1.000000000000000000, 0.9659258262890683122, 1.000000000000000000, 0.9659258262890683122, 1.000000000000000000, 0.9659258262890683122, 1.000000000000000000, 0.9659258262890683122, 1.000000000000000000, 0.9659258262890683122, 1.000000000000000000, 0.9659258262890683122, 1.000000000000000000, 0.9659258262890683122, 1.000000000000000000, 0.9659258262890683122, 1.000000000000000000, 0.9659258262890683122, 1.000000000000000000, 0.9659258262890683122, 1.000000000000000000, 0.9659258262890683122, 1.000000000000000000, 0.9659258262890683122, 1.000000000000000000, 0.9659258262890683122, 1.000000000000000000, 0.9659258262890683122, 1.000000000000000000, 0.9659258262890683122, 1.000000000000000000, 0.9659258262890683122, 1.000000000000000000, 0.9659258262890683122, 1.000000000000000000, 0.9659258262890683122, 1.000000000000000000, 0.9659258262890683122, 1.000000000000000000) ) ) 
 REPRESENTATION_ITEM ( '' )  SURFACE ( )  );
#82352 = CARTESIAN_POINT ( 'NONE',  ( 1.108923884514436242, -0.05778040916215522460, 0.4822834645669289988 ) ) ;
#82353 = CARTESIAN_POINT ( 'NONE',  ( -0.4986876640419942164, -0.5023911411419708095, 0.1820866141732285504 ) ) ;
#82354 = CARTESIAN_POINT ( 'NONE',  ( -0.5380577427821514602, -0.4281496062992127816, -0.4176697321401328100 ) ) ;
#82355 = CARTESIAN_POINT ( 'NONE',  ( 1.135170603674541256, -0.6692913385826773087, -0.1292274648535924053 ) ) ;
#82356 = CARTESIAN_POINT ( 'NONE',  ( 1.108923884514436686, -0.3162353388693409650, -0.4822834645669289433 ) ) ;
#82357 = CIRCLE ( 'NONE', #46045, 0.3149606299212597826 ) ;
#82358 = CARTESIAN_POINT ( 'NONE',  ( -0.9776902887139098386, -0.5511811023622046335, 0.09757992244046803654 ) ) ;
#82359 = CARTESIAN_POINT ( 'NONE',  ( 0.1998031496062992463, 0.3460692066303959202, -0.6935695538057742304 ) ) ;
#82360 = CARTESIAN_POINT ( 'NONE',  ( -0.3460692066303958092, -0.1998031496062994683, -0.8398950131233595684 ) ) ;
#82361 = CARTESIAN_POINT ( 'NONE',  ( 4.837279021331060870E-17, -0.3949938075777409963, -0.07874015748031501505 ) ) ;
#82362 = CARTESIAN_POINT ( 'NONE',  ( 0.2492877267040487788, 1.133758322672524743, -1.503986617498455303 ) ) ;
#82363 = CARTESIAN_POINT ( 'NONE',  ( 1.030183727034121421, -0.08942795157527998196, 0.3641732283464567121 ) ) ;
#82364 = CARTESIAN_POINT ( 'NONE',  ( 0.8595800524934390507, -0.08942795157528024563, -0.3641732283464568787 ) ) ;
#82365 = CARTESIAN_POINT ( 'NONE',  ( 0.4527559055118117182, -0.5400638737290844871, 0.3530559997133364547 ) ) ;
#82366 = CARTESIAN_POINT ( 'NONE',  ( 1.568241469816273437, -0.3162353388693405765, 0.4822834645669290543 ) ) ;
#82367 = CARTESIAN_POINT ( 'NONE',  ( 0.3420746716998660508, -0.1974969037888704149, -1.284120734908136718 ) ) ;
#82368 = CARTESIAN_POINT ( 'NONE',  ( 0.6299212598425204535, -0.1870078740157480601, -0.3641732283464567677 ) ) ;
#82369 = CARTESIAN_POINT ( 'NONE',  ( -0.3543307086614165824, 0.2952755905511811885, 0.000000000000000000 ) ) ;
#82370 = CARTESIAN_POINT ( 'NONE',  ( -1.325459317585300889, 0.05413385826771666132, 0.4176697321401328100 ) ) ;
#82371 = CARTESIAN_POINT ( 'NONE',  ( 1.056430446194226658, 0.2952755905511811885, 0.1292274648535926551 ) ) ;
#82372 = CARTESIAN_POINT ( 'NONE',  ( -0.2362204724409447953, -0.4091458600556404646, -1.797900262467191590 ) ) ;
#82373 = CARTESIAN_POINT ( 'NONE',  ( -0.7349081364829390672, 0.2306618581243847221, -0.2411417322834647770 ) ) ;
#82374 = CARTESIAN_POINT ( 'NONE',  ( -0.01968503937007793844, -0.4536011799217367080, 0.2665933059059888421 ) ) ;
#82375 = VERTEX_POINT ( 'NONE', #81092 ) ;
#82376 = ORIENTED_EDGE ( 'NONE', *, *, #42359, .F. ) ;
#82377 = AXIS2_PLACEMENT_3D ( 'NONE', #28476, #22992, #29718 ) ;
#82378 = CARTESIAN_POINT ( 'NONE',  ( -0.6496062992125976043, -0.5400638737290844871, 0.3530559997133364547 ) ) ;
#82379 = ADVANCED_FACE ( 'NONE', ( #36453 ), #49494, .F. ) ;
#82380 = CARTESIAN_POINT ( 'NONE',  ( -0.4658792650918627265, -0.3162353388693409650, -0.4822834645669289433 ) ) ;
#82381 = CARTESIAN_POINT ( 'NONE',  ( -0.1377952755905504645, -0.5400638737290845981, -0.3530559997133363437 ) ) ;
#82382 = CARTESIAN_POINT ( 'NONE',  ( 0.2821522309711292364, 0.2952755905511810774, -0.1292274648535930714 ) ) ;
#82383 = CARTESIAN_POINT ( 'NONE',  ( -0.3412073490813641308, 0.2306618581243847221, -0.2411417322834647770 ) ) ;
#82384 = CARTESIAN_POINT ( 'NONE',  ( -1.167979002624671470, 0.05413385826771666132, 0.4176697321401328100 ) ) ;
#82385 = CARTESIAN_POINT ( 'NONE',  ( -0.7349081364829390672, 0.2306618581243847221, -0.2411417322834647770 ) ) ;
#82386 = CARTESIAN_POINT ( 'NONE',  ( 0.8005249343832027131, 0.05413385826771666132, 0.4176697321401328100 ) ) ;
#82387 = CARTESIAN_POINT ( 'NONE',  ( 0.3392501089628018329, 0.1958661417322835607, -1.383202099737532942 ) ) ;
#82388 = CARTESIAN_POINT ( 'NONE',  ( -0.3608923884514428360, 0.1771653543307087630, 0.09757992244046791164 ) ) ;
#82389 = ORIENTED_EDGE ( 'NONE', *, *, #73735, .T. ) ;
#82390 = CARTESIAN_POINT ( 'NONE',  ( -0.3949938075777411628, 0.1058382717557497937, -1.450131233595800762 ) ) ;
#82391 = ORIENTED_EDGE ( 'NONE', *, *, #55872, .T. ) ;
#82392 = CARTESIAN_POINT ( 'NONE',  ( -1.332020997375327642, -0.2845877964562161244, -0.3641732283464567121 ) ) ;
#82393 = CARTESIAN_POINT ( 'NONE',  ( -0.9580052493438311334, 0.05413385826771626580, -0.4176697321401330321 ) ) ;
#82394 = CARTESIAN_POINT ( 'NONE',  ( -1.049868766404198794, -0.6046776061558807314, 0.2411417322834647770 ) ) ;
#82395 = CARTESIAN_POINT ( 'NONE',  ( 0.2925321140481932369, 0.2925321140481932369, -0.1377952755905512139 ) ) ;
#82396 = CARTESIAN_POINT ( 'NONE',  ( -0.5643044619422565855, 0.05413385826771626580, -0.4176697321401330321 ) ) ;
#82397 = CARTESIAN_POINT ( 'NONE',  ( -0.8005249343832013809, -0.4281496062992124485, 0.4176697321401328655 ) ) ;
#82398 = CARTESIAN_POINT ( 'NONE',  ( -1.528871391076114250, -0.6692913385826771977, 0.1292274648535927661 ) ) ;
#82399 = CARTESIAN_POINT ( 'NONE',  ( -1.725721784776902190, -0.05778040916215522460, 0.4822834645669289988 ) ) ;
#82400 = CARTESIAN_POINT ( 'NONE',  ( 0.6758530183727039509, -0.5511811023622046335, 0.09757992244046803654 ) ) ;
#82401 = DIRECTION ( 'NONE',  ( 0.000000000000000000, 0.000000000000000000, -1.000000000000000000 ) ) ;
#82402 = CARTESIAN_POINT ( 'NONE',  ( -9.594673741351313045E-17, 0.3917322834645670104, 0.2303149606299211838 ) ) ;
#82403 = CARTESIAN_POINT ( 'NONE',  ( 0.1640419947506569498, -0.08942795157527998196, 0.3641732283464567121 ) ) ;
#82404 = CARTESIAN_POINT ( 'NONE',  ( -0.5052493438320203589, 0.2952755905511810774, -0.1292274648535930714 ) ) ;
#82405 = CARTESIAN_POINT ( 'NONE',  ( 1.522309711286089939, -0.6046776061558809534, -0.2411417322834644161 ) ) ;
#82406 = CARTESIAN_POINT ( 'NONE',  ( -0.1181102362204717315, -0.6692913385826771977, 8.415575281601705876E-17 ) ) ;
#82407 = ORIENTED_EDGE ( 'NONE', *, *, #82040, .T. ) ;
#82408 = CARTESIAN_POINT ( 'NONE',  ( 0.1070741851644054915, -0.3996062992125986035, -2.132545931758530244 ) ) ;
#82409 = DIRECTION ( 'NONE',  ( -1.000000000000000000, -0.000000000000000000, -0.000000000000000000 ) ) ;
#82410 = ORIENTED_EDGE ( 'NONE', *, *, #2607, .T. ) ;
#82411 = CARTESIAN_POINT ( 'NONE',  ( -0.2925321140481932369, 0.2925321140481931259, -1.671259842519685179 ) ) ;
#82412 = CARTESIAN_POINT ( 'NONE',  ( 1.167979002624672580, 0.05413385826771626580, -0.4176697321401330321 ) ) ;
#82413 = CARTESIAN_POINT ( 'NONE',  ( -1.207349081364828880, 0.1283753931104746893, -0.1820866141732285504 ) ) ;
#82414 = CARTESIAN_POINT ( 'NONE',  ( -1.522309711286088607, 0.2306618581243847221, -0.2411417322834647770 ) ) ;
#82415 = CARTESIAN_POINT ( 'NONE',  ( -0.4724409448818898682, -8.678599364036362592E-17, -0.9842519685039369248 ) ) ;
#82416 = CARTESIAN_POINT ( 'NONE',  ( -0.4501900775161314372, 1.384563962073082966, 3.911202265604141193 ) ) ;
#82417 = CARTESIAN_POINT ( 'NONE',  ( 0.3917322834645669549, 0.1049643490035304660, 0.04068241469816277767 ) ) ;
#82418 = CARTESIAN_POINT ( 'NONE',  ( 1.423884514435696413, -0.3162353388693409650, -0.4822834645669289433 ) ) ;
#82419 = CARTESIAN_POINT ( 'NONE',  ( 0.4199475065616803948, -0.6046776061558809534, -0.2411417322834644161 ) ) ;
#82420 = CARTESIAN_POINT ( 'NONE',  ( 0.1640419947506569498, -0.3162353388693409650, -0.4822834645669289433 ) ) ;
#82421 = CARTESIAN_POINT ( 'NONE',  ( -1.141732283464566011, 0.1771653543307087630, 0.000000000000000000 ) ) ;
#82422 = CARTESIAN_POINT ( 'NONE',  ( -0.4921259842519677963, -0.5400638737290844871, 0.3530559997133364547 ) ) ;
#82423 = CARTESIAN_POINT ( 'NONE',  ( -0.1070741851644051862, -0.3996062992125986590, 0.1660104986876640154 ) ) ;
#82424 = CARTESIAN_POINT ( 'NONE',  ( -0.9776902887139098386, -0.6692913385826771977, 0.1292274648535927661 ) ) ;
#82425 = CARTESIAN_POINT ( 'NONE',  ( 0.3949938075777408852, 0.1058382717557500435, -2.406167979002624691 ) ) ;
#82426 = CARTESIAN_POINT ( 'NONE',  ( 1.318897637795276356, 0.07958543189024071263, -0.2665933059059888421 ) ) ;
#82427 = CARTESIAN_POINT ( 'NONE',  ( -0.3871391076115479057, -0.2845877964562161244, -0.3641732283464567121 ) ) ;
#82428 = VECTOR ( 'NONE', #44823, 39.37007874015748143 ) ;
#82429 = CARTESIAN_POINT ( 'NONE',  ( 1.161417322834646493, -0.4536011799217367080, 0.2665933059059888421 ) ) ;
#82430 = CARTESIAN_POINT ( 'NONE',  ( -1.666666666666665853, 0.05413385826771626580, -0.4176697321401330321 ) ) ;
#82431 = CARTESIAN_POINT ( 'NONE',  ( 0.1474713956048451791, 8.471767977567108961E-16, -0.4445507791589058955 ) ) ;
#82432 = CARTESIAN_POINT ( 'NONE',  ( 0.6692913385826778638, -0.5511811023622047445, 6.969142054262312111E-17 ) ) ;
#82433 = CARTESIAN_POINT ( 'NONE',  ( -0.7808398950131222316, -0.3162353388693409650, -0.4822834645669289433 ) ) ;
#82434 = CARTESIAN_POINT ( 'NONE',  ( 0.2624671916010504757, 0.2306618581243848609, 0.2411417322834645549 ) ) ;
#82435 = CARTESIAN_POINT ( 'NONE',  ( 8.195543980992789655E-16, -0.1870078740157480601, -0.3641732283464567677 ) ) ;
#82436 = CARTESIAN_POINT ( 'NONE',  ( -1.712598425196849572, 0.07958543189024085140, 0.2665933059059887866 ) ) ;
#82437 = CARTESIAN_POINT ( 'NONE',  ( 0.9383202099737538715, -0.05778040916215560624, -0.4822834645669293319 ) ) ;
#82438 = CARTESIAN_POINT ( 'NONE',  ( -1.220472440944882830, 0.2066929133858268208, 2.389277853677468338E-14 ) ) ;
#82439 = AXIS2_PLACEMENT_3D ( 'NONE', #71168, #5934, #82963 ) ;
#82440 = CARTESIAN_POINT ( 'NONE',  ( 1.364829396325459854, -0.5023911411419708095, -0.1820866141732282451 ) ) ;
#82441 = CARTESIAN_POINT ( 'NONE',  ( -0.7611548556430438595, 0.2306618581243848609, 0.2411417322834645549 ) ) ;
#82442 = CARTESIAN_POINT ( 'NONE',  ( -0.3608923884514428360, 0.1771653543307087630, 0.09757992244046791164 ) ) ;
#82443 = FACE_OUTER_BOUND ( 'NONE', #36293, .T. ) ;
#82444 = CARTESIAN_POINT ( 'NONE',  ( 0.07217847769028949700, -0.08942795157528024563, -0.3641732283464568787 ) ) ;
#82445 = CARTESIAN_POINT ( 'NONE',  ( -1.227034120734907585, 0.2952755905511811885, 0.1292274648535926551 ) ) ;
#82446 = EDGE_CURVE ( 'NONE', #23151, #3487, #81919, .T. ) ;
#82447 = CARTESIAN_POINT ( 'NONE',  ( -0.6430446194225712953, 0.05413385826771626580, -0.4176697321401330321 ) ) ;
#82448 = CARTESIAN_POINT ( 'NONE',  ( 0.2925321140481932369, -0.2925321140481931814, -0.6476377952755905110 ) ) ;
#82449 = EDGE_CURVE ( 'NONE', #13017, #82375, #59453, .T. ) ;
#82450 = CARTESIAN_POINT ( 'NONE',  ( 0.2867679344610365999, -0.2867679344610365444, -2.072834645669291209 ) ) ;
#82451 = CARTESIAN_POINT ( 'NONE',  ( 0.4330708661417329575, -0.5511811023622047445, 6.969142054262312111E-17 ) ) ;
#82452 = CARTESIAN_POINT ( 'NONE',  ( -0.2755905511811015396, -0.6692913385826771977, 8.415575281601705876E-17 ) ) ;
#82453 = CARTESIAN_POINT ( 'NONE',  ( -0.8595800524934373854, -0.05778040916215522460, 0.4822834645669289988 ) ) ;
#82454 = CARTESIAN_POINT ( 'NONE',  ( -0.7020997375328074108, -0.08942795157527998196, 0.3641732283464567121 ) ) ;
#82455 = CARTESIAN_POINT ( 'NONE',  ( -3.909771271330827691, 1.429805566235350378, 0.4623082157241558687 ) ) ;
#82456 = CARTESIAN_POINT ( 'NONE',  ( -0.2362204724409440182, -0.1870078740157479769, 0.4822834645669291653 ) ) ;
#82457 = CARTESIAN_POINT ( 'NONE',  ( -1.719160104986876103, -0.004921259842519576551, 0.3153832671262227771 ) ) ;
#82458 = CARTESIAN_POINT ( 'NONE',  ( -1.502624671916009680, -0.3162353388693405765, 0.4822834645669290543 ) ) ;
#82459 = CARTESIAN_POINT ( 'NONE',  ( -0.2462293917967295909, -2.567464376874931580E-15, -0.4445507791589072832 ) ) ;
#82460 = ORIENTED_EDGE ( 'NONE', *, *, #41491, .T. ) ;
#82461 = DIRECTION ( 'NONE',  ( -0.000000000000000000, 1.000000000000000000, -0.000000000000000000 ) ) ;
#82462 = CARTESIAN_POINT ( 'NONE',  ( -1.397637795275589623, 0.1660481256975885056, 0.3530559997133364547 ) ) ;
#82463 = CARTESIAN_POINT ( 'NONE',  ( -0.8595800524934373854, -0.3162353388693409650, -0.4822834645669289433 ) ) ;
#82464 = CARTESIAN_POINT ( 'NONE',  ( -1.456692913385826182, 0.2952755905511811885, 0.000000000000000000 ) ) ;
#82465 = CARTESIAN_POINT ( 'NONE',  ( 0.3917322834645669549, 0.1049643490035304660, -2.099081364829396446 ) ) ;
#82466 = DIRECTION ( 'NONE',  ( 0.000000000000000000, 0.000000000000000000, -1.000000000000000000 ) ) ;
#82467 = EDGE_CURVE ( 'NONE', #24385, #53683, #64824, .T. ) ;
#82468 = CARTESIAN_POINT ( 'NONE',  ( 0.7742782152230979209, 0.05413385826771626580, -0.4176697321401330321 ) ) ;
#82469 = CARTESIAN_POINT ( 'NONE',  ( -0.1837270341207340729, 0.2306618581243847221, -0.2411417322834647770 ) ) ;
#82470 = CARTESIAN_POINT ( 'NONE',  ( -0.4724409448818898682, 5.785732909357575061E-17, -2.755905511811024056 ) ) ;
#82471 = CARTESIAN_POINT ( 'NONE',  ( -0.6561679790026240244, 0.2306618581243847221, -0.2411417322834647770 ) ) ;
#82472 = CARTESIAN_POINT ( 'NONE',  ( 1.062992125984252745, -0.5511811023622047445, 6.969142054262312111E-17 ) ) ;
#82473 = CARTESIAN_POINT ( 'NONE',  ( -0.1070741851644056997, 0.3996062992125986035, -1.108923884514435798 ) ) ;
#82474 = VERTEX_POINT ( 'NONE', #52795 ) ;
#82475 = CARTESIAN_POINT ( 'NONE',  ( 0.3917322834645670104, -0.1049643490035303411, -2.780839895013122565 ) ) ;
#82476 = VERTEX_POINT ( 'NONE', #25874 ) ;
#82477 = CARTESIAN_POINT ( 'NONE',  ( 0.4986876640419954376, 0.2306618581243848609, 0.2411417322834645549 ) ) ;
#82478 = CARTESIAN_POINT ( 'NONE',  ( -0.6758530183727028406, -0.6692913385826773087, -0.1292274648535924053 ) ) ;
#82479 = CARTESIAN_POINT ( 'NONE',  ( -1.548556430446193399, -0.6046776061558809534, -0.2411417322834644161 ) ) ;
#82480 = CARTESIAN_POINT ( 'NONE',  ( 0.7874015748031503170, -0.1870078740157480879, -0.4822834645669291653 ) ) ;
#82481 = CIRCLE ( 'NONE', #47503, 3.937007874015748143 ) ;
#82482 = CARTESIAN_POINT ( 'NONE',  ( -1.535433070866141225, -0.5511811023622047445, 6.969142054262312111E-17 ) ) ;
#82483 = DIRECTION ( 'NONE',  ( 1.000000000000000000, 0.000000000000000000, 0.000000000000000000 ) ) ;
#82484 = CARTESIAN_POINT ( 'NONE',  ( -0.1312335958005241554, -0.6046776061558809534, -0.2411417322834644161 ) ) ;
#82485 = CARTESIAN_POINT ( 'NONE',  ( -1.450131233595799651, 0.2952755905511810774, -0.1292274648535930714 ) ) ;
#82486 = CARTESIAN_POINT ( 'NONE',  ( -1.627296587926508442, 0.2306618581243848609, 0.2411417322834645549 ) ) ;
#82487 = CARTESIAN_POINT ( 'NONE',  ( 1.614173228346457378, -0.6692913385826771977, 8.415575281601705876E-17 ) ) ;
#82488 = CARTESIAN_POINT ( 'NONE',  ( -0.3917322834645669549, -0.1049643490035306603, 0.1194225721784776956 ) ) ;
#82489 = CARTESIAN_POINT ( 'NONE',  ( 0.7086614173228353852, -0.1870078740157479769, 0.3641732283464567677 ) ) ;
#82490 = ORIENTED_EDGE ( 'NONE', *, *, #21410, .F. ) ;
#82491 = CARTESIAN_POINT ( 'NONE',  ( -0.3949938075777411628, 0.1058382717557497937, -0.1902887139107612702 ) ) ;
#82492 = ORIENTED_EDGE ( 'NONE', *, *, #75384, .T. ) ;
#82493 = CARTESIAN_POINT ( 'NONE',  ( -0.1640419947506555343, -0.2845877964562159024, 0.3641732283464567677 ) ) ;
#82494 = CYLINDRICAL_SURFACE ( 'NONE', #46193, 0.4724409448818898682 ) ;
#82495 = CARTESIAN_POINT ( 'NONE',  ( 0.4133858267716541968, -0.5400638737290845981, -0.3530559997133363437 ) ) ;
#82496 = CARTESIAN_POINT ( 'NONE',  ( 0.4265091863517067039, -0.6692913385826773087, -0.1292274648535924053 ) ) ;
#82497 = CARTESIAN_POINT ( 'NONE',  ( -0.4921259842519677963, -0.5400638737290844871, 0.3530559997133364547 ) ) ;
#82498 = CARTESIAN_POINT ( 'NONE',  ( -0.1049643490035307158, 0.3917322834645670104, -1.735583620243781322 ) ) ;
#82499 = CARTESIAN_POINT ( 'NONE',  ( -1.122047244094487306, 0.1660481256975883668, -0.3530559997133364547 ) ) ;
#82500 = CARTESIAN_POINT ( 'NONE',  ( 0.1958661417322836440, -0.3392501089628017219, -2.538713910761154491 ) ) ;
#82501 = CARTESIAN_POINT ( 'NONE',  ( 1.371391076115485719, -0.5511811023622048555, -0.09757992244046775898 ) ) ;
#82502 = CARTESIAN_POINT ( 'NONE',  ( -1.469816272965878357, 0.2306618581243848609, 0.2411417322834645549 ) ) ;
#82503 = CARTESIAN_POINT ( 'NONE',  ( 1.076115485564305141, 0.2306618581243847221, -0.2411417322834647770 ) ) ;
#82504 = CARTESIAN_POINT ( 'NONE',  ( 1.312335958005250269, -0.6046776061558807314, 0.2411417322834647770 ) ) ;
#82505 = CARTESIAN_POINT ( 'NONE',  ( 0.2925321140481932369, 0.2925321140481932369, -0.9251968503937008093 ) ) ;
#82506 = CARTESIAN_POINT ( 'NONE',  ( -1.141732283464566011, -0.6692913385826771977, 8.415575281601705876E-17 ) ) ;
#82507 = CARTESIAN_POINT ( 'NONE',  ( 0.1070741851644053388, 0.3996062992125986035, -0.3851706036745406458 ) ) ;
#82508 = CARTESIAN_POINT ( 'NONE',  ( -0.2559055118110230564, 0.1660481256975883668, -0.3530559997133364547 ) ) ;
#82509 = CARTESIAN_POINT ( 'NONE',  ( 0.3460692066303959202, 0.1998031496062993295, -2.335958005249343827 ) ) ;
#82510 = CARTESIAN_POINT ( 'NONE',  ( 0.1958661417322836440, -0.3392501089628017219, -1.751312335958005395 ) ) ;
#82511 = CARTESIAN_POINT ( 'NONE',  ( 1.332020997375329197, -0.3162353388693405765, 0.4822834645669290543 ) ) ;
#82512 = CARTESIAN_POINT ( 'NONE',  ( 0.06561679790026316017, -0.3690944881889763329, 0.3153832671262228327 ) ) ;
#82513 = CARTESIAN_POINT ( 'NONE',  ( 0.8464566929133865436, 0.1660481256975883668, -0.3530559997133364547 ) ) ;
#82514 = CARTESIAN_POINT ( 'NONE',  ( -0.4724409448818898682, -8.678599364036362592E-17, -1.218503937007874072 ) ) ;
#82515 = CARTESIAN_POINT ( 'NONE',  ( 0.9251968503937015864, 0.07958543189024071263, -0.2665933059059888421 ) ) ;
#82516 = CARTESIAN_POINT ( 'NONE',  ( 0.5183727034120741983, 0.2952755905511810774, -0.1292274648535930714 ) ) ;
#82517 = CARTESIAN_POINT ( 'NONE',  ( -0.1974969037888706924, 0.3420746716998658843, -1.034776902887139194 ) ) ;
#82518 = CARTESIAN_POINT ( 'NONE',  ( -0.6299212598425188991, -0.1870078740157479769, 0.4822834645669291653 ) ) ;
#82519 = CARTESIAN_POINT ( 'NONE',  ( 0.4849061582275022153, 1.805669738366188382, 0.4921425059946344938 ) ) ;
#82520 = CARTESIAN_POINT ( 'NONE',  ( 0.7874015748031503170, -0.1870078740157479769, 0.3641732283464567677 ) ) ;
#82521 = CARTESIAN_POINT ( 'NONE',  ( 0.1674892343164159914, -2.191421614605370878E-15, 0.4445507791589071167 ) ) ;
#82522 = CARTESIAN_POINT ( 'NONE',  ( -0.4002624671916004129, -0.05778040916215560624, -0.4822834645669293319 ) ) ;
#82523 = CARTESIAN_POINT ( 'NONE',  ( 0.2690288713910767848, 0.1771653543307087630, 0.09757992244046791164 ) ) ;
#82524 = CARTESIAN_POINT ( 'NONE',  ( -2.860656214895221261, 1.077434660671925393, -0.1173752429317476975 ) ) ;
#82525 = CARTESIAN_POINT ( 'NONE',  ( -0.1115485564304456306, 0.2952755905511810774, -0.1292274648535930714 ) ) ;
#82526 = CARTESIAN_POINT ( 'NONE',  ( 0.5052493438320215802, 0.1771653543307087630, 0.09757992244046791164 ) ) ;
#82527 = EDGE_CURVE ( 'NONE', #55143, #33617, #47367, .T. ) ;
#82528 = CARTESIAN_POINT ( 'NONE',  ( 0.1070741851644053388, 0.3996062992125986035, -1.802493438320210029 ) ) ;
#82529 = CARTESIAN_POINT ( 'NONE',  ( 0.5052493438320218022, -0.6692913385826773087, -0.1292274648535924053 ) ) ;
#82530 = CARTESIAN_POINT ( 'NONE',  ( 1.023622047244095334, -0.1870078740157479769, 0.3641732283464567677 ) ) ;
#82531 = CARTESIAN_POINT ( 'NONE',  ( 0.1706036745406830368, 0.05413385826771666132, 0.4176697321401328100 ) ) ;
#82532 = CARTESIAN_POINT ( 'NONE',  ( -0.3543307086614165824, -0.5511811023622047445, 6.969142054262312111E-17 ) ) ;
#82533 = CARTESIAN_POINT ( 'NONE',  ( -0.7349081364829390672, 0.1283753931104746893, -0.1820866141732285504 ) ) ;
#82534 = CARTESIAN_POINT ( 'NONE',  ( -0.3608923884514428360, 0.2952755905511811885, 0.1292274648535926551 ) ) ;
#82535 = CARTESIAN_POINT ( 'NONE',  ( 0.1181102362204730916, -0.6692913385826771977, 8.415575281601705876E-17 ) ) ;
#82536 = CARTESIAN_POINT ( 'NONE',  ( 0.8005249343832028242, -0.3690944881889765550, -0.3153832671262227771 ) ) ;
#82537 = CARTESIAN_POINT ( 'NONE',  ( 1.403614904275686858E-14, 1.537401574803149984, -3.937007874015761910 ) ) ;
#82538 = CARTESIAN_POINT ( 'NONE',  ( 1.482939632545932307, -0.004921259842519870586, -0.3153832671262229437 ) ) ;
#82539 = CIRCLE ( 'NONE', #48944, 1.122047244094488194 ) ;
#82540 = CARTESIAN_POINT ( 'NONE',  ( 0.8727034120734913358, -0.05778040916215522460, 0.4822834645669289988 ) ) ;
#82541 = CARTESIAN_POINT ( 'NONE',  ( 0.000000000000000000, 2.755905511811024056, 0.000000000000000000 ) ) ;
#82542 = CARTESIAN_POINT ( 'NONE',  ( -0.2034120734908131112, -0.6692913385826773087, -0.1292274648535924053 ) ) ;
#82543 = CARTESIAN_POINT ( 'NONE',  ( -0.1049643490035302024, -0.3917322834645671215, -1.101706036745407014 ) ) ;
#82544 = CARTESIAN_POINT ( 'NONE',  ( 0.7480314960629927956, 0.2952755905511811885, 0.000000000000000000 ) ) ;
#82545 = CARTESIAN_POINT ( 'NONE',  ( 0.5708661417322842269, 0.1660481256975885056, 0.3530559997133364547 ) ) ;
#82546 = DIRECTION ( 'NONE',  ( 0.000000000000000000, 0.000000000000000000, -1.000000000000000000 ) ) ;
#82547 = CARTESIAN_POINT ( 'NONE',  ( 0.5774278215223104249, 0.1283753931104748280, 0.1820866141732283561 ) ) ;
#82548 = CARTESIAN_POINT ( 'NONE',  ( 1.332020997375329197, -0.3162353388693405765, 0.4822834645669290543 ) ) ;
#82549 = CARTESIAN_POINT ( 'NONE',  ( -0.4330708661417315697, 0.1771653543307087630, 0.000000000000000000 ) ) ;
#82550 = AXIS2_PLACEMENT_3D ( 'NONE', #21871, #74060, #10082 ) ;
#82551 = CARTESIAN_POINT ( 'NONE',  ( -0.3149606299212590610, -0.1870078740157480879, -0.4822834645669291653 ) ) ;
#82552 = CARTESIAN_POINT ( 'NONE',  ( -0.2362204724409447953, -0.4091458600556404646, -2.585301837270341352 ) ) ;
#82553 = CARTESIAN_POINT ( 'NONE',  ( 0.1115485564304467270, -0.6692913385826773087, -0.1292274648535924053 ) ) ;
#82554 = CARTESIAN_POINT ( 'NONE',  ( -0.9383202099737524282, -0.3162353388693409650, -0.4822834645669289433 ) ) ;
#82555 = CARTESIAN_POINT ( 'NONE',  ( -0.7742782152230965886, -0.004921259842519576551, 0.3153832671262227771 ) ) ;
#82556 = CARTESIAN_POINT ( 'NONE',  ( 0.2493438320209980519, -0.4281496062992127816, -0.4176697321401328100 ) ) ;
#82557 = CARTESIAN_POINT ( 'NONE',  ( -1.207349081364828880, 0.2306618581243847221, -0.2411417322834647770 ) ) ;
#82558 = CARTESIAN_POINT ( 'NONE',  ( -0.3083989501312330295, -0.3162353388693409650, -0.4822834645669289433 ) ) ;
#82560 = CARTESIAN_POINT ( 'NONE',  ( 1.430446194225722500, 0.05413385826771666132, 0.4176697321401328100 ) ) ;
#82559 = CARTESIAN_POINT ( 'NONE',  ( -0.9333857237505057691, -2.609244250047836720E-15, 0.3791475997938242304 ) ) ;
#82561 = CARTESIAN_POINT ( 'NONE',  ( 1.607611548556431069, -0.6692913385826773087, -0.1292274648535924053 ) ) ;
#82562 = CARTESIAN_POINT ( 'NONE',  ( -0.1958661417322834220, -0.3392501089628018884, -1.947506561679789971 ) ) ;
#82563 = DIRECTION ( 'NONE',  ( -0.000000000000000000, -1.000000000000000000, -0.000000000000000000 ) ) ;
#82564 = CARTESIAN_POINT ( 'NONE',  ( -0.7939632545931754048, -0.3162353388693405765, 0.4822834645669290543 ) ) ;
#82565 = CARTESIAN_POINT ( 'NONE',  ( 0.4724409448818897572, -0.1265901696524988906, -0.4265091863517060933 ) ) ;
#82566 = CARTESIAN_POINT ( 'NONE',  ( -0.1998031496062994683, 0.3460692066303958092, 0.1443569553805774119 ) ) ;
#82567 = ORIENTED_EDGE ( 'NONE', *, *, #27771, .T. ) ;
#82568 = CARTESIAN_POINT ( 'NONE',  ( 0.5380577427821529035, -0.3690944881889763329, 0.3153832671262228327 ) ) ;
#82569 = CARTESIAN_POINT ( 'NONE',  ( -0.3917322834645669549, -0.1049643490035306603, -1.455380577427821676 ) ) ;
#82570 = CARTESIAN_POINT ( 'NONE',  ( 0.6167979002624678353, -0.4281496062992124485, 0.4176697321401328655 ) ) ;
#82571 = PLANE ( 'NONE',  #74464 ) ;
#82572 = CARTESIAN_POINT ( 'NONE',  ( -0.5636006452641416642, -2.613618158232546091E-15, -0.3464511005275220379 ) ) ;
#82573 = CARTESIAN_POINT ( 'NONE',  ( -0.2887139107611542133, -0.5023911411419708095, -0.1820866141732282451 ) ) ;
#82574 = CARTESIAN_POINT ( 'NONE',  ( -0.2478063387913458926, 0.02791078216816347476, -0.4328096321851898631 ) ) ;
#82575 = CARTESIAN_POINT ( 'NONE',  ( 1.305774278215223960, -0.6692913385826771977, 0.1292274648535927661 ) ) ;
#82576 = CARTESIAN_POINT ( 'NONE',  ( 0.7808398950131240079, -0.2845877964562159024, 0.3641732283464567677 ) ) ;
#82577 = CARTESIAN_POINT ( 'NONE',  ( -0.1443569553805765515, -0.4281496062992127816, -0.4176697321401328100 ) ) ;
#82578 = CARTESIAN_POINT ( 'NONE',  ( 0.1049643490035304522, -0.3917322834645668994, -0.7952562747693419087 ) ) ;
#82579 = CARTESIAN_POINT ( 'NONE',  ( -0.3871391076115476282, -0.05778040916215522460, 0.4822834645669289988 ) ) ;
#82580 = CARTESIAN_POINT ( 'NONE',  ( -1.377952755905511140, 0.1771653543307087630, 0.000000000000000000 ) ) ;
#82581 = CARTESIAN_POINT ( 'NONE',  ( -0.3608923884514428360, -0.6692913385826773087, -0.1292274648535924053 ) ) ;
#82582 = CARTESIAN_POINT ( 'NONE',  ( -1.016821367227983997, 1.537401574803149984, 0.4744094488188970171 ) ) ;
#82583 = CARTESIAN_POINT ( 'NONE',  ( -0.06818963398611965765, 1.067605756753705393, -1.854667707163995871 ) ) ;
#82584 = ORIENTED_EDGE ( 'NONE', *, *, #56851, .F. ) ;
#82585 = CARTESIAN_POINT ( 'NONE',  ( 0.1958661417322836718, -0.3392501089628017219, -1.978365772474752537 ) ) ;
#82586 = CARTESIAN_POINT ( 'NONE',  ( 0.5314960629921267055, -0.5400638737290844871, 0.3530559997133364547 ) ) ;
#82587 = ORIENTED_EDGE ( 'NONE', *, *, #65801, .F. ) ;
#82588 = CARTESIAN_POINT ( 'NONE',  ( -0.4658792650918627265, -0.05778040916215522460, 0.4822834645669289988 ) ) ;
#82589 = CARTESIAN_POINT ( 'NONE',  ( -1.653543307086613234, -0.1870078740157479769, 0.4822834645669291653 ) ) ;
#82590 = ADVANCED_FACE ( 'NONE', ( #52373 ), #63778, .F. ) ;
#82591 = CARTESIAN_POINT ( 'NONE',  ( 0.8070866141732288002, 0.1660481256975885056, 0.3530559997133364547 ) ) ;
#82592 = CARTESIAN_POINT ( 'NONE',  ( -0.07874015748031421014, -0.1870078740157479769, 0.4822834645669291653 ) ) ;
#82593 = CARTESIAN_POINT ( 'NONE',  ( -0.2867679344610364334, -0.2867679344610367109, -1.561023622047243986 ) ) ;
#82594 = CARTESIAN_POINT ( 'NONE',  ( -0.5774278215223089816, 0.2306618581243847221, -0.2411417322834647770 ) ) ;
#82595 = CARTESIAN_POINT ( 'NONE',  ( -0.2624671916010490880, -0.6046776061558807314, 0.2411417322834647770 ) ) ;
#82596 = CARTESIAN_POINT ( 'NONE',  ( -0.8661417322834640276, -0.1870078740157479769, 0.4822834645669291653 ) ) ;
#82597 = CIRCLE ( 'NONE', #57038, 1.929133858267716661 ) ;
#82598 = EDGE_CURVE ( 'NONE', #40878, #71072, #78505, .T. ) ;
#82599 = CARTESIAN_POINT ( 'NONE',  ( 0.4921259842519691285, -0.4536011799217368745, -0.2665933059059886201 ) ) ;
#82600 = CARTESIAN_POINT ( 'NONE',  ( -0.2596871853482274894, -0.1407230452551245514, 5.593746434152945035 ) ) ;
#82601 = CARTESIAN_POINT ( 'NONE',  ( -0.2559055118110230564, 0.1660481256975883668, -0.3530559997133364547 ) ) ;
#82602 = CARTESIAN_POINT ( 'NONE',  ( 0.000000000000000000, 2.716535433070866645, 0.000000000000000000 ) ) ;
#82603 = CARTESIAN_POINT ( 'NONE',  ( 1.128608923884514947, 0.2306618581243848609, 0.2411417322834645549 ) ) ;
#82604 = CARTESIAN_POINT ( 'NONE',  ( -9.594673741351313045E-17, 0.3917322834645670104, -2.826771653543306506 ) ) ;
#82605 = ORIENTED_EDGE ( 'NONE', *, *, #40252, .F. ) ;
#82606 = ORIENTED_EDGE ( 'NONE', *, *, #32173, .T. ) ;
#82607 = CARTESIAN_POINT ( 'NONE',  ( 0.3083989501312343062, -0.05778040916215560624, -0.4822834645669293319 ) ) ;
#82608 = CARTESIAN_POINT ( 'NONE',  ( 0.2887139107611556010, -0.5023911411419708095, 0.1820866141732285504 ) ) ;
#82610 = DIRECTION ( 'NONE',  ( -0.000000000000000000, -1.000000000000000000, -0.000000000000000000 ) ) ;
#82609 = CARTESIAN_POINT ( 'NONE',  ( 1.246719160104987623, -0.004921259842519870586, -0.3153832671262229437 ) ) ;
#82611 = CARTESIAN_POINT ( 'NONE',  ( 0.3917322834645670104, -0.1049643490035303411, -1.141076115485564202 ) ) ;
#82612 = CARTESIAN_POINT ( 'NONE',  ( -0.4724409448818898682, -8.678599364036362592E-17, 0.04133858267716534335 ) ) ;
#82613 = AXIS2_PLACEMENT_3D ( 'NONE', #10536, #30281, #36192 ) ;
#82614 = CARTESIAN_POINT ( 'NONE',  ( 0.1998031496062992463, 0.3460692066303959202, -2.740813648293963567 ) ) ;
#82615 = CARTESIAN_POINT ( 'NONE',  ( 0.5380577427821529035, 0.05413385826771626580, -0.4176697321401330321 ) ) ;
#82616 = CARTESIAN_POINT ( 'NONE',  ( -1.272965879265091305, 0.05413385826771626580, -0.4176697321401330321 ) ) ;
#82617 = CARTESIAN_POINT ( 'NONE',  ( -1.043307086614172707, 0.1660481256975883668, -0.3530559997133364547 ) ) ;
#82618 = CARTESIAN_POINT ( 'NONE',  ( 0.07874015748031558404, -0.1870078740157480879, -0.4822834645669291653 ) ) ;
#82619 = CARTESIAN_POINT ( 'NONE',  ( 1.089238845144357537, -0.4281496062992124485, 0.4176697321401328655 ) ) ;
#82620 = CARTESIAN_POINT ( 'NONE',  ( 1.404199475065617708, -0.004921259842519870586, -0.3153832671262229437 ) ) ;
#82621 = ITEM_DEFINED_TRANSFORMATION ( 'NONE', 'NONE', #35619,  #22098 ) ;
#82622 = CARTESIAN_POINT ( 'NONE',  ( 0.8464566929133866546, -0.4536011799217367080, 0.2665933059059888421 ) ) ;
#82623 = CARTESIAN_POINT ( 'NONE',  ( -0.7217847769028863381, -0.4281496062992124485, 0.4176697321401328655 ) ) ;
#82624 = EDGE_CURVE ( 'NONE', #67465, #37133, #77663, .T. ) ;
#82625 = CARTESIAN_POINT ( 'NONE',  ( 0.3996062992125985480, 2.446882876249141654E-17, -0.5098425196850393526 ) ) ;
#82626 = CARTESIAN_POINT ( 'NONE',  ( -1.548556430446193399, -0.5023911411419708095, -0.1820866141732282451 ) ) ;
#82627 = CARTESIAN_POINT ( 'NONE',  ( 0.3392501089628018884, -0.1958661417322834220, -0.4120734908136482466 ) ) ;
#82629 = CARTESIAN_POINT ( 'NONE',  ( -0.03412294937774069253, 1.063915752041794782, 1.851250178557425130 ) ) ;
#82628 = CARTESIAN_POINT ( 'NONE',  ( 1.259842519685040019, -0.1870078740157480879, -0.4822834645669291653 ) ) ;
#82630 = CARTESIAN_POINT ( 'NONE',  ( -1.712598425196849572, 0.07958543189024085140, 0.2665933059059887866 ) ) ;
#82631 = CARTESIAN_POINT ( 'NONE',  ( 0.1312335958005257930, 0.2306618581243847221, -0.2411417322834647770 ) ) ;
#82632 = CARTESIAN_POINT ( 'NONE',  ( 1.010498687664042716, -0.004921259842519870586, -0.3153832671262229437 ) ) ;
#82633 = EDGE_CURVE ( 'NONE', #12200, #66338, #4601, .T. ) ;
#82634 = CARTESIAN_POINT ( 'NONE',  ( -1.502624671916009680, -0.08942795157528024563, -0.3641732283464568787 ) ) ;
#82635 = CARTESIAN_POINT ( 'NONE',  ( 1.102362204724410155, -0.1870078740157480879, -0.4822834645669291653 ) ) ;
#82636 = CARTESIAN_POINT ( 'NONE',  ( -0.4921259842519677963, 0.1660481256975883391, -0.3530559997133364547 ) ) ;
#82637 = CARTESIAN_POINT ( 'NONE',  ( -0.5511811023622041894, -0.1870078740157480601, -0.3641732283464567677 ) ) ;
#82638 = CARTESIAN_POINT ( 'NONE',  ( -0.7414698162729651543, 0.2952755905511810774, -0.1292274648535930714 ) ) ;
#82639 = CARTESIAN_POINT ( 'NONE',  ( 1.404199475065617708, 0.05413385826771626580, -0.4176697321401330321 ) ) ;
#82640 = CARTESIAN_POINT ( 'NONE',  ( -1.233595800524933894, 0.2306618581243848609, 0.2411417322834645549 ) ) ;
#82641 = CARTESIAN_POINT ( 'NONE',  ( 1.548556430446194954, 0.2306618581243847221, -0.2411417322834647770 ) ) ;
#82642 = CARTESIAN_POINT ( 'NONE',  ( 0.1958661417322836718, -0.3392501089628017219, -1.033483882710973134 ) ) ;
#82643 = CARTESIAN_POINT ( 'NONE',  ( -1.351706036745406347, -0.3690944881889763329, 0.3153832671262228327 ) ) ;
#82644 = CARTESIAN_POINT ( 'NONE',  ( 2.620897244026417994, 1.710976477253048023, 0.4417575354491489747 ) ) ;
#82645 = CARTESIAN_POINT ( 'NONE',  ( 1.102362204724410155, -0.1870078740157479769, 0.4822834645669291653 ) ) ;
#82646 = CARTESIAN_POINT ( 'NONE',  ( 0.4091458600556404646, -0.2362204724409448231, -2.543963254593176071 ) ) ;
#82647 = CARTESIAN_POINT ( 'NONE',  ( -1.706036745406823485, 0.2306618581243848609, 0.2411417322834645549 ) ) ;
#82648 = CARTESIAN_POINT ( 'NONE',  ( -1.397637795275589623, -0.4536011799217368745, -0.2665933059059886201 ) ) ;
#82649 = CARTESIAN_POINT ( 'NONE',  ( -0.8923884514435688198, 0.1283753931104746893, -0.1820866141732285504 ) ) ;
#82650 = CARTESIAN_POINT ( 'NONE',  ( 1.502624671916010790, -0.08942795157527998196, 0.3641732283464567121 ) ) ;
#82651 = CARTESIAN_POINT ( 'NONE',  ( -0.5708661417322825615, -0.5400638737290844871, 0.3530559997133364547 ) ) ;
#82652 = CARTESIAN_POINT ( 'NONE',  ( 0.1837270341207357105, -0.5023911411419708095, -0.1820866141732282451 ) ) ;
#82653 = CARTESIAN_POINT ( 'NONE',  ( -1.417322834645668772, -0.1870078740157479769, 0.3641732283464567677 ) ) ;
#82654 = CARTESIAN_POINT ( 'NONE',  ( 1.548556430446194954, -0.5023911411419708095, 0.1820866141732285504 ) ) ;
#82655 = CARTESIAN_POINT ( 'NONE',  ( 0.7939632545931766261, -0.3162353388693409650, -0.4822834645669289433 ) ) ;
#82656 = CARTESIAN_POINT ( 'NONE',  ( -0.6399301791983041943, -2.567464376874931580E-15, -0.4445507791589072832 ) ) ;
#82657 = CARTESIAN_POINT ( 'NONE',  ( 0.09186351706036827158, -0.004921259842519576551, 0.3153832671262227771 ) ) ;
#82658 = AXIS2_PLACEMENT_3D ( 'NONE', #53199, #53617, #52788 ) ;
#82659 = CARTESIAN_POINT ( 'NONE',  ( 0.5314960629921267055, -0.5400638737290844871, 0.3530559997133364547 ) ) ;
#82660 = CARTESIAN_POINT ( 'NONE',  ( 0.9842519685039375910, 0.1771653543307087630, 0.000000000000000000 ) ) ;
#82661 = VERTEX_POINT ( 'NONE', #76819 ) ;
#82662 = CARTESIAN_POINT ( 'NONE',  ( -1.496062992125983815, -0.1870078740157479769, 0.4822834645669291653 ) ) ;
#82663 = CARTESIAN_POINT ( 'NONE',  ( -1.299212598425196097, 0.2952755905511811885, 0.000000000000000000 ) ) ;
#82664 = CARTESIAN_POINT ( 'NONE',  ( -0.1771653543307080136, -0.5400638737290844871, 0.3530559997133364547 ) ) ;
#82665 = CARTESIAN_POINT ( 'NONE',  ( -0.3460692066303958092, -0.1998031496062994683, -0.5249343832020997302 ) ) ;
#82666 = CARTESIAN_POINT ( 'NONE',  ( -0.3996062992125984925, -0.1070741851644056858, -2.799868766404198794 ) ) ;
#82667 = CARTESIAN_POINT ( 'NONE',  ( 0.5577427821522314977, -0.3162353388693409650, -0.4822834645669289433 ) ) ;
#82668 = CARTESIAN_POINT ( 'NONE',  ( 1.003937007874016185, 0.07958543189024071263, -0.2665933059059888421 ) ) ;
#82669 = CARTESIAN_POINT ( 'NONE',  ( -0.3083989501312330295, -0.3162353388693409650, -0.4822834645669289433 ) ) ;
#82670 = CARTESIAN_POINT ( 'NONE',  ( 0.1574803149606306130, -0.1870078740157479769, 0.4822834645669291653 ) ) ;
#82671 = CARTESIAN_POINT ( 'NONE',  ( 0.3996062992125986035, 2.446882876249141962E-17, -2.007874015748031482 ) ) ;
#82672 = CARTESIAN_POINT ( 'NONE',  ( 0.3949938075777409963, 2.418639510665530435E-17, -1.377952755905511584 ) ) ;
#82673 = DIRECTION ( 'NONE',  ( -0.000000000000000000, -1.000000000000000000, -0.000000000000000000 ) ) ;
#82674 = CARTESIAN_POINT ( 'NONE',  ( 3.909863570149732848, 1.648352784150537875, 0.4615281897282089152 ) ) ;
#82675 = CARTESIAN_POINT ( 'NONE',  ( 4.797336870675656522E-17, -0.3917322834645670104, -0.5433070866141732624 ) ) ;
#82676 = CARTESIAN_POINT ( 'NONE',  ( -0.4790026246719154557, -0.2845877964562159024, 0.3641732283464567677 ) ) ;
#82677 = CARTESIAN_POINT ( 'NONE',  ( -0.8005249343832013809, -0.4281496062992124485, 0.4176697321401328655 ) ) ;
#82678 = CARTESIAN_POINT ( 'NONE',  ( 0.2891555358219910499, 0.2891555358219910499, -2.734251968503936592 ) ) ;
#82679 = CARTESIAN_POINT ( 'NONE',  ( 1.010498687664042716, -0.4281496062992124485, 0.4176697321401328655 ) ) ;
#82680 = CARTESIAN_POINT ( 'NONE',  ( -1.581364829396324945, -0.05778040916215560624, -0.4822834645669293319 ) ) ;
#82681 = CARTESIAN_POINT ( 'NONE',  ( 0.7808398950131240079, -0.3162353388693405765, 0.4822834645669290543 ) ) ;
#82682 = CARTESIAN_POINT ( 'NONE',  ( 0.2362204724409449064, 0.4091458600556404646, -2.664041994750656173 ) ) ;
#82683 = CARTESIAN_POINT ( 'NONE',  ( -9.787531504996567848E-17, 0.3996062992125986035, -2.047244094488188892 ) ) ;
#82684 = CARTESIAN_POINT ( 'NONE',  ( 1.607611548556431069, -0.6692913385826773087, -0.1292274648535924053 ) ) ;
#82685 = CARTESIAN_POINT ( 'NONE',  ( 0.7414698162729663755, -0.6692913385826773087, -0.1292274648535924053 ) ) ;
#82686 = EDGE_CURVE ( 'NONE', #55143, #16761, #64606, .T. ) ;
#82687 = CARTESIAN_POINT ( 'NONE',  ( 0.7611548556430451917, -0.6046776061558807314, 0.2411417322834647770 ) ) ;
#82688 = CARTESIAN_POINT ( 'NONE',  ( 1.010498687664042716, -0.004921259842519870586, -0.3153832671262229437 ) ) ;
#82689 = CARTESIAN_POINT ( 'NONE',  ( 1.246719160104987623, 0.05413385826771626580, -0.4176697321401330321 ) ) ;
#82690 = CARTESIAN_POINT ( 'NONE',  ( -0.3917322834645669549, -0.1049643490035306603, -0.2880577427821523484 ) ) ;
#82691 = CARTESIAN_POINT ( 'NONE',  ( -0.5314960629921349211, 2.716535433070866645, 2.543486866223387377 ) ) ;
#82692 = CARTESIAN_POINT ( 'NONE',  ( 0.7611548556430454138, 0.2306618581243847221, -0.2411417322834647770 ) ) ;
#82693 = CARTESIAN_POINT ( 'NONE',  ( 1.548556430446194954, 0.1283753931104746893, -0.1820866141732285504 ) ) ;
#82694 = CARTESIAN_POINT ( 'NONE',  ( -0.8464566929133852113, -0.5400638737290845981, -0.3530559997133363437 ) ) ;
#82695 = CARTESIAN_POINT ( 'NONE',  ( -0.8530183727034112984, -0.4281496062992127816, -0.4176697321401328100 ) ) ;
#82696 = CARTESIAN_POINT ( 'NONE',  ( 0.9711286089238851948, 0.2306618581243848609, 0.2411417322834645549 ) ) ;
#82697 = CARTESIAN_POINT ( 'NONE',  ( -0.3917322834645670104, -7.196005306013484475E-17, -0.5964566929133858775 ) ) ;
#82698 = CARTESIAN_POINT ( 'NONE',  ( -0.1049643490035307020, 0.3917322834645669549, -1.416010498687664043 ) ) ;
#82699 = CARTESIAN_POINT ( 'NONE',  ( -0.3917322834645669549, -0.1049643490035306603, -2.715223097112861250 ) ) ;
#82700 = VERTEX_POINT ( 'NONE', #31783 ) ;
#82701 = CARTESIAN_POINT ( 'NONE',  ( 0.3996062992125986590, -0.1070741851644053111, 0.04593175853018371252 ) ) ;
#82702 = EDGE_LOOP ( 'NONE', ( #49129, #41892, #55260, #45907 ) ) ;
#82703 = CARTESIAN_POINT ( 'NONE',  ( -1.595398199321657939, 0.4619154201552267414, 0.1559797534342468872 ) ) ;
#82704 = CARTESIAN_POINT ( 'NONE',  ( 1.568241469816273437, -0.2845877964562159024, 0.3641732283464567677 ) ) ;
#82705 = CARTESIAN_POINT ( 'NONE',  ( -0.1070741851644056997, 0.3996062992125986035, -1.581364829396325389 ) ) ;
#82706 = CARTESIAN_POINT ( 'NONE',  ( 1.325459317585302665, -0.3690944881889763329, 0.3153832671262228327 ) ) ;
#82707 = CARTESIAN_POINT ( 'NONE',  ( -0.2362204724409451284, 0.4091458600556402425, -2.452099737532808188 ) ) ;
#82708 = DIRECTION ( 'NONE',  ( 0.000000000000000000, 1.000000000000000000, 0.000000000000000000 ) ) ;
#82709 = CARTESIAN_POINT ( 'NONE',  ( -0.1080761259423674570, 1.946643253402353224, 0.2941585223818156680 ) ) ;
#82710 = CARTESIAN_POINT ( 'NONE',  ( -0.3392501089628017219, -0.1958661417322836718, -0.2946194225721785465 ) ) ;
#82711 =( BOUNDED_CURVE ( )  B_SPLINE_CURVE ( 2, ( #54960, #53709, #60038, #22979, #15440, #67611, #16272, #47815, #28464, #28879, #61701, #48646, #23390 ),
 .UNSPECIFIED., .F., .F. ) 
 B_SPLINE_CURVE_WITH_KNOTS ( ( 3, 2, 2, 2, 2, 2, 3 ),
 ( 0.3551492764529827206, 0.3560606060606060774, 0.3598484848484848619, 0.3636363636363636465, 0.3674242424242424310, 0.3712121212121212155, 0.3721234508197446278 ),
 .UNSPECIFIED. ) 
 CURVE ( )  GEOMETRIC_REPRESENTATION_ITEM ( )  RATIONAL_B_SPLINE_CURVE ( ( 0.9875488213027530104, 0.9918020599134685922, 1.000000000000000000, 0.9659258262890683122, 1.000000000000000000, 0.9659258262890683122, 1.000000000000000000, 0.9659258262890683122, 1.000000000000000000, 0.9659258262890683122, 1.000000000000000000, 0.9918020599134680371, 0.9875488213027523443 ) ) 
 REPRESENTATION_ITEM ( '' )  );
#82712 = CARTESIAN_POINT ( 'NONE',  ( -0.8464566929133852113, 0.07958543189024085140, 0.2665933059059887866 ) ) ;
#82713 = CARTESIAN_POINT ( 'NONE',  ( -1.181102362204723644, -0.1870078740157479769, 0.4822834645669291653 ) ) ;
#82714 = CARTESIAN_POINT ( 'NONE',  ( 0.2493438320209980519, -0.4281496062992127816, -0.4176697321401328100 ) ) ;
#82715 = CARTESIAN_POINT ( 'NONE',  ( 1.404199475065617264, -0.4281496062992124485, 0.4176697321401328655 ) ) ;
#82716 = VERTEX_POINT ( 'NONE', #77239 ) ;
#82717 = LINE ( 'NONE', #68853, #67614 ) ;
#82718 = CARTESIAN_POINT ( 'NONE',  ( 2.209741691727579838, 2.418298854841256951, 6.771642358790693983 ) ) ;
#82719 = CARTESIAN_POINT ( 'NONE',  ( 5.785732909357575061E-17, -0.4724409448818898682, -1.968503937007873850 ) ) ;
#82720 = PLANE ( 'NONE',  #22356 ) ;
#82721 = CARTESIAN_POINT ( 'NONE',  ( -0.5314960629921250401, 0.07958543189024085140, 0.2665933059059887866 ) ) ;
#82722 = CARTESIAN_POINT ( 'NONE',  ( -1.371391076115484609, -0.6692913385826771977, 0.1292274648535927661 ) ) ;
#82723 = CARTESIAN_POINT ( 'NONE',  ( 0.8398950131233602345, -0.6046776061558807314, 0.2411417322834647770 ) ) ;
#82724 = VECTOR ( 'NONE', #22773, 39.37007874015748143 ) ;
#82725 = VERTEX_POINT ( 'NONE', #32200 ) ;
#82727 = CYLINDRICAL_SURFACE ( 'NONE', #62693, 0.4744094488188972947 ) ;
#82726 = CARTESIAN_POINT ( 'NONE',  ( -0.2362204724409447953, -0.4091458600556404646, -2.270341207349081181 ) ) ;
#82728 = CARTESIAN_POINT ( 'NONE',  ( 1.338582677165355062, -0.1870078740157479769, 0.4822834645669291653 ) ) ;
#82729 = CARTESIAN_POINT ( 'NONE',  ( -1.246719160104986512, 0.05413385826771666132, 0.4176697321401328100 ) ) ;
#82730 = CARTESIAN_POINT ( 'NONE',  ( -0.3917322834645669549, -7.196005306013483243E-17, -0.4343638863178984622 ) ) ;
#82731 = CARTESIAN_POINT ( 'NONE',  ( -0.3083989501312330295, -0.08942795157527998196, 0.3641732283464567121 ) ) ;
#82732 = CARTESIAN_POINT ( 'NONE',  ( 0.2867679344610366554, 0.2867679344610366554, -0.6948818897637795144 ) ) ;
#82733 = CARTESIAN_POINT ( 'NONE',  ( -0.3412073490813641308, 0.1283753931104746893, -0.1820866141732285504 ) ) ;
#82734 = CARTESIAN_POINT ( 'NONE',  ( 0.3346456692913390985, 0.07958543189024085140, 0.2665933059059887866 ) ) ;
#82735 = CARTESIAN_POINT ( 'NONE',  ( 0.2230971128608929543, 0.05413385826771626580, -0.4176697321401330321 ) ) ;
#82736 = CARTESIAN_POINT ( 'NONE',  ( -0.5643044619422565855, -0.3690944881889763329, 0.3153832671262228327 ) ) ;
#82737 = CARTESIAN_POINT ( 'NONE',  ( -0.3917322834645671215, 0.1049643490035301469, -2.702099737532808632 ) ) ;
#82738 = CARTESIAN_POINT ( 'NONE',  ( 1.299212598425197429, 0.2952755905511811885, 0.000000000000000000 ) ) ;
#82739 = CARTESIAN_POINT ( 'NONE',  ( -0.9186351706036736120, -0.6046776061558809534, -0.2411417322834644161 ) ) ;
#82740 = CARTESIAN_POINT ( 'NONE',  ( -0.3458507752293906723, -0.3458507752293910609, -1.395669291338582196 ) ) ;
#82741 = CARTESIAN_POINT ( 'NONE',  ( -0.2230971128608915943, -0.4281496062992127816, -0.4176697321401328100 ) ) ;
#82742 = CARTESIAN_POINT ( 'NONE',  ( -0.9251968503937002541, -0.5400638737290845981, -0.3530559997133363437 ) ) ;
#82743 = CARTESIAN_POINT ( 'NONE',  ( 1.089238845144357759, -0.004921259842519870586, -0.3153832671262229437 ) ) ;
#82744 = CARTESIAN_POINT ( 'NONE',  ( -0.3608923884514428360, -0.5511811023622048555, -0.09757992244046775898 ) ) ;
#82745 = CARTESIAN_POINT ( 'NONE',  ( -0.5708661417322828946, 0.1660481256975883668, -0.3530559997133364547 ) ) ;
#82746 = CARTESIAN_POINT ( 'NONE',  ( -1.174540682414697335, -0.05778040916215522460, 0.4822834645669289988 ) ) ;
#82747 = CARTESIAN_POINT ( 'NONE',  ( 1.410761154855643795, -0.08942795157528024563, -0.3641732283464568787 ) ) ;
#82748 = CARTESIAN_POINT ( 'NONE',  ( -0.2887139107611542133, -0.6046776061558809534, -0.2411417322834644161 ) ) ;
#82749 = CARTESIAN_POINT ( 'NONE',  ( -1.062992125984250968, 0.2952755905511811885, 0.000000000000000000 ) ) ;
#82750 = ORIENTED_EDGE ( 'NONE', *, *, #34017, .T. ) ;
#82751 = CARTESIAN_POINT ( 'NONE',  ( 0.3996062992125986035, -0.1070741851644052972, -2.235564304461942431 ) ) ;
#82752 = CARTESIAN_POINT ( 'NONE',  ( -0.8464566929133852113, 0.07958543189024085140, 0.2665933059059887866 ) ) ;
#82753 = CARTESIAN_POINT ( 'NONE',  ( 1.299212598425197429, 0.2952755905511811885, 0.000000000000000000 ) ) ;
#82754 = CARTESIAN_POINT ( 'NONE',  ( -1.272965879265091305, -0.3690944881889763329, 0.3153832671262228327 ) ) ;
#82755 = CARTESIAN_POINT ( 'NONE',  ( 0.3996062992125986035, -0.1070741851644052972, -1.290682414698162805 ) ) ;
#82756 = CARTESIAN_POINT ( 'NONE',  ( -1.023622047244094002, -0.1870078740157480879, -0.4822834645669291653 ) ) ;
#82757 = CIRCLE ( 'NONE', #2145, 0.01968503937007875723 ) ;
#82758 = CARTESIAN_POINT ( 'NONE',  ( 1.371391076115485941, 0.2952755905511811885, 0.1292274648535926551 ) ) ;
#82759 = CARTESIAN_POINT ( 'NONE',  ( 0.9120734908136490793, 0.2952755905511810774, -0.1292274648535930714 ) ) ;
#82760 = CARTESIAN_POINT ( 'NONE',  ( 1.555118110236221041, -0.5400638737290844871, 0.3530559997133364547 ) ) ;
#82761 = CARTESIAN_POINT ( 'NONE',  ( -1.286089238845143479, -0.5023911411419708095, 0.1820866141732285504 ) ) ;
#82762 = CARTESIAN_POINT ( 'NONE',  ( -0.3996062992125984925, -0.1070741851644056719, -0.7526246719160104570 ) ) ;
#82763 = CARTESIAN_POINT ( 'NONE',  ( 0.1998031496062992740, 0.3460692066303959757, -1.089238845144356871 ) ) ;
#82764 = CARTESIAN_POINT ( 'NONE',  ( 0.3949938075777409408, 0.1058382717557500574, -0.4396325459317587114 ) ) ;
#82765 = DIRECTION ( 'NONE',  ( 0.000000000000000000, 0.000000000000000000, -1.000000000000000000 ) ) ;
#82766 = CARTESIAN_POINT ( 'NONE',  ( 1.207349081364829990, 0.1283753931104748280, 0.1820866141732283561 ) ) ;
#82767 = CARTESIAN_POINT ( 'NONE',  ( 0.7217847769028878924, -0.3690944881889765550, -0.3153832671262227771 ) ) ;
#82768 = CARTESIAN_POINT ( 'NONE',  ( 0.7086614173228352742, -0.1870078740157480879, -0.4822834645669291653 ) ) ;
#82769 = CARTESIAN_POINT ( 'NONE',  ( -0.4091458600556402980, -0.2362204724409451284, -2.333989501312335957 ) ) ;
#82770 = CARTESIAN_POINT ( 'NONE',  ( 0.3949938075777409408, -0.1058382717557499186, -1.290682414698162583 ) ) ;
#82771 = CARTESIAN_POINT ( 'NONE',  ( 0.9186351706036752773, 0.1283753931104746893, -0.1820866141732285504 ) ) ;
#82772 = EDGE_CURVE ( 'NONE', #33187, #82725, #12722, .T. ) ;
#82773 = CARTESIAN_POINT ( 'NONE',  ( -0.4527559055118102749, -0.5400638737290845981, -0.3530559997133363437 ) ) ;
#82774 = CARTESIAN_POINT ( 'NONE',  ( -1.036745406824146176, -0.4281496062992124485, 0.4176697321401328655 ) ) ;
#82775 = CARTESIAN_POINT ( 'NONE',  ( 0.8858267716535438430, 0.1660481256975885056, 0.3530559997133364547 ) ) ;
#82776 = CARTESIAN_POINT ( 'NONE',  ( -0.1265901696524986964, -0.4724409448818899238, -1.646981627296587591 ) ) ;
#82777 = CARTESIAN_POINT ( 'NONE',  ( 0.3996062992125986035, 2.446882876249141962E-17, -2.637795275590551380 ) ) ;
#82778 = VECTOR ( 'NONE', #27019, 39.37007874015748143 ) ;
#82779 = ORIENTED_EDGE ( 'NONE', *, *, #37456, .T. ) ;
#82780 = EDGE_LOOP ( 'NONE', ( #58954, #64066, #20986, #34421 ) ) ;
#82781 = CARTESIAN_POINT ( 'NONE',  ( -1.430446194225721390, -0.4281496062992124485, 0.4176697321401328655 ) ) ;
#82782 = CARTESIAN_POINT ( 'NONE',  ( -0.6299212598425188991, -0.1870078740157480879, -0.4822834645669291653 ) ) ;
#82784 = CARTESIAN_POINT ( 'NONE',  ( -0.8661417322834640276, -0.1870078740157479769, 0.4822834645669291653 ) ) ;
#82783 = CARTESIAN_POINT ( 'NONE',  ( -0.9842519685039360366, 0.1771653543307087630, 0.000000000000000000 ) ) ;
#82785 = CARTESIAN_POINT ( 'NONE',  ( 0.5446194225721792126, -0.3162353388693405765, 0.4822834645669290543 ) ) ;
#82786 = CARTESIAN_POINT ( 'NONE',  ( -0.5774278215223089816, -0.6046776061558807314, 0.2411417322834647770 ) ) ;
#82787 = CARTESIAN_POINT ( 'NONE',  ( -1.371391076115484609, -0.6692913385826771977, 0.1292274648535927661 ) ) ;
#82788 = CARTESIAN_POINT ( 'NONE',  ( -0.8398950131233589023, -0.6046776061558809534, -0.2411417322834644161 ) ) ;
#82789 = CARTESIAN_POINT ( 'NONE',  ( 0.7742782152230978099, -0.4281496062992124485, 0.4176697321401328655 ) ) ;
#82790 = CARTESIAN_POINT ( 'NONE',  ( -0.3917322834645670104, -7.196005306013484475E-17, -1.448818897637795367 ) ) ;
#82791 = CARTESIAN_POINT ( 'NONE',  ( -0.9317585301837263412, -0.3690944881889765550, -0.3153832671262227771 ) ) ;
#82792 = ORIENTED_EDGE ( 'NONE', *, *, #78455, .F. ) ;
#82793 = CARTESIAN_POINT ( 'NONE',  ( 0.3949938075777411073, -0.1058382717557499464, -1.528871391076115804 ) ) ;
#82794 = EDGE_LOOP ( 'NONE', ( #32591, #55452, #55771, #77525, #23795, #55125, #45738 ) ) ;
#82795 = CARTESIAN_POINT ( 'NONE',  ( -1.213910761154854745, 0.1771653543307087075, -0.09757992244046823083 ) ) ;
#82796 = CARTESIAN_POINT ( 'NONE',  ( -0.9448818897637790704, -0.1870078740157480879, -0.4822834645669291653 ) ) ;
#82797 = CARTESIAN_POINT ( 'NONE',  ( -0.8530183727034112984, 0.05413385826771666132, 0.4176697321401328100 ) ) ;
#82798 = CARTESIAN_POINT ( 'NONE',  ( -0.3996062992125986035, -7.340648628747425578E-17, -0.1968503937007874127 ) ) ;
#82799 = CARTESIAN_POINT ( 'NONE',  ( -0.9186351706036736120, 0.2306618581243848609, 0.2411417322834645549 ) ) ;
#82800 = CARTESIAN_POINT ( 'NONE',  ( -1.423884514435694859, -0.3162353388693405765, 0.4822834645669290543 ) ) ;
#82801 = CARTESIAN_POINT ( 'NONE',  ( 2.503252890251015828, 2.755905511811024056, -0.5314960629921260393 ) ) ;
#82802 = CARTESIAN_POINT ( 'NONE',  ( -1.614173228346457378, 0.4410134679336882302, 0.1372047244094476981 ) ) ;
#82803 = CARTESIAN_POINT ( 'NONE',  ( 0.6692913385826778638, -0.5511811023622047445, 6.969142054262312111E-17 ) ) ;
#82804 = CARTESIAN_POINT ( 'NONE',  ( -0.4839371108951621148, -3.153061149046662969E-15, -0.3791475997938244524 ) ) ;
#82805 = CARTESIAN_POINT ( 'NONE',  ( 0.2867679344610365999, 0.2867679344610365999, -0.06496062992125994917 ) ) ;
#82806 = CARTESIAN_POINT ( 'NONE',  ( 0.1377952755905518800, -0.4536011799217367080, 0.2665933059059888421 ) ) ;
#82807 = CARTESIAN_POINT ( 'NONE',  ( -0.3412073490813641308, 0.2306618581243847221, -0.2411417322834647770 ) ) ;
#82808 = CARTESIAN_POINT ( 'NONE',  ( 1.561679790026247350, -0.4281496062992124485, 0.4176697321401328655 ) ) ;
#82809 = CARTESIAN_POINT ( 'NONE',  ( -0.3608923884514428360, 0.2952755905511811885, 0.1292274648535926551 ) ) ;
#82810 = EDGE_LOOP ( 'NONE', ( #38602, #59210, #8482, #53623, #64765, #41110, #9542, #16053, #60529, #3718, #36112, #35889, #50186, #69542, #24163, #69148, #15950, #67973, #49985, #76818 ) ) ;
#82811 = CARTESIAN_POINT ( 'NONE',  ( 0.2462293917967310342, -2.191421614605370878E-15, 0.4445507791589071167 ) ) ;
#82812 = VERTEX_POINT ( 'NONE', #32614 ) ;
#82813 = CARTESIAN_POINT ( 'NONE',  ( -0.1070741851644056997, 0.3996062992125984925, -1.500656167979002031 ) ) ;
#82814 = CARTESIAN_POINT ( 'NONE',  ( -0.6233595800524928121, -0.3162353388693409650, -0.4822834645669289433 ) ) ;
#82815 = CARTESIAN_POINT ( 'NONE',  ( 1.469816272965879911, 0.2306618581243847221, -0.2411417322834647770 ) ) ;
#82816 = CARTESIAN_POINT ( 'NONE',  ( -1.187664041994750175, -0.08942795157528024563, -0.3641732283464568787 ) ) ;
#82817 = CARTESIAN_POINT ( 'NONE',  ( -1.456692913385826182, -0.6692913385826771977, 8.415575281601705876E-17 ) ) ;
#82818 = CARTESIAN_POINT ( 'NONE',  ( 0.4091458600556404646, -0.2362204724409448231, -1.049868766404199460 ) ) ;
#82819 = CARTESIAN_POINT ( 'NONE',  ( 0.3249695492770460770, 1.223219560026271499E-15, 0.4445507791589056734 ) ) ;
#82820 = CARTESIAN_POINT ( 'NONE',  ( 0.1049643490035303689, 0.3917322834645670104, 0.01443569553805778768 ) ) ;
#82821 = CARTESIAN_POINT ( 'NONE',  ( 1.443569553805774897, -0.6046776061558809534, -0.2411417322834644161 ) ) ;
#82822 = AXIS2_PLACEMENT_3D ( 'NONE', #67634, #80686, #48665 ) ;
#82823 = CARTESIAN_POINT ( 'NONE',  ( -0.2867679344610366554, 0.2867679344610365444, -2.151574803149606030 ) ) ;
#82824 = CARTESIAN_POINT ( 'NONE',  ( 0.1837270341207357105, -0.6046776061558809534, -0.2411417322834644161 ) ) ;
#82825 = CARTESIAN_POINT ( 'NONE',  ( -0.8661417322834640276, -0.1870078740157479769, 0.3641732283464567677 ) ) ;
#82826 = CIRCLE ( 'NONE', #10260, 3.405511811023621771 ) ;
#82827 = AXIS2_PLACEMENT_3D ( 'NONE', #39253, #59448, #71670 ) ;
#82828 = CARTESIAN_POINT ( 'NONE',  ( -0.4002624671916004129, -0.05778040916215560624, -0.4822834645669293319 ) ) ;
#82829 = CARTESIAN_POINT ( 'NONE',  ( -0.2362204724409447953, -0.4091458600556404646, -2.662073490813648746 ) ) ;
#82830 = CARTESIAN_POINT ( 'NONE',  ( -0.7414698162729651543, 0.2952755905511810774, -0.1292274648535930714 ) ) ;
#82831 = CARTESIAN_POINT ( 'NONE',  ( -1.161417322834644716, -0.5400638737290845981, -0.3530559997133363437 ) ) ;
#82832 = CARTESIAN_POINT ( 'NONE',  ( -0.3949938075777409963, -7.255918531996591613E-17, -2.163385826771653697 ) ) ;
#82833 = CARTESIAN_POINT ( 'NONE',  ( 0.6692913385826777528, 0.1771653543307087630, 0.000000000000000000 ) ) ;
#82834 = CARTESIAN_POINT ( 'NONE',  ( -0.3346456692913377662, -0.4536011799217367080, 0.2665933059059888421 ) ) ;
#82835 = CARTESIAN_POINT ( 'NONE',  ( 0.9055118110236227702, 0.1771653543307087630, 0.000000000000000000 ) ) ;
#82836 = CARTESIAN_POINT ( 'NONE',  ( -1.437007874015747477, -0.5400638737290844871, 0.3530559997133364547 ) ) ;
#82837 = CARTESIAN_POINT ( 'NONE',  ( 1.358267716535433323, -0.5400638737290845981, -0.3530559997133363437 ) ) ;
#82838 = CARTESIAN_POINT ( 'NONE',  ( 0.4527559055118117182, 0.07958543189024071263, -0.2665933059059888421 ) ) ;
#82839 = CARTESIAN_POINT ( 'NONE',  ( -0.6496062992125976043, 0.1660481256975883668, -0.3530559997133364547 ) ) ;
#82840 = CARTESIAN_POINT ( 'NONE',  ( 1.410761154855643795, -0.3162353388693405765, 0.4822834645669290543 ) ) ;
#82841 =( BOUNDED_CURVE ( )  B_SPLINE_CURVE ( 2, ( #72675, #34374, #8703, #28051, #73518, #74341, #47401, #67200, #29707, #34795, #9531, #28465, #15867 ),
 .UNSPECIFIED., .F., .F. ) 
 B_SPLINE_CURVE_WITH_KNOTS ( ( 3, 2, 2, 2, 2, 2, 3 ),
 ( 0.5824220037257099580, 0.5833333333333333703, 0.5871212121212121549, 0.5909090909090909394, 0.5946969696969697239, 0.5984848484848485084, 0.5993961780924720317 ),
 .UNSPECIFIED. ) 
 CURVE ( )  GEOMETRIC_REPRESENTATION_ITEM ( )  RATIONAL_B_SPLINE_CURVE ( ( 0.9875488213027523443, 0.9918020599134680371, 1.000000000000000000, 0.9659258262890683122, 1.000000000000000000, 0.9659258262890683122, 1.000000000000000000, 0.9659258262890683122, 1.000000000000000000, 0.9659258262890683122, 1.000000000000000000, 0.9918020599134671489, 0.9875488213027514561 ) ) 
 REPRESENTATION_ITEM ( '' )  );
#82842 = AXIS2_PLACEMENT_3D ( 'NONE', #28895, #66379, #47414 ) ;
#82843 = CARTESIAN_POINT ( 'NONE',  ( 2.583694225513480713, 2.755905511811024056, 0.5314960629921260393 ) ) ;
#82844 = CARTESIAN_POINT ( 'NONE',  ( -0.1574803149606292529, -0.1870078740157480601, -0.3641732283464567677 ) ) ;
#82845 = CARTESIAN_POINT ( 'NONE',  ( 0.2462293917967310342, -2.191421614605370878E-15, 0.4445507791589071167 ) ) ;
#82846 = CARTESIAN_POINT ( 'NONE',  ( 0.4855643044619430415, -0.4281496062992127816, -0.4176697321401328100 ) ) ;
#82847 = DIRECTION ( 'NONE',  ( 0.000000000000000000, -1.000000000000000000, 0.000000000000000000 ) ) ;
#82848 = CARTESIAN_POINT ( 'NONE',  ( 1.259842519685040019, -0.1870078740157479769, 0.3641732283464567677 ) ) ;
#82849 = CARTESIAN_POINT ( 'NONE',  ( 0.1377952755905518800, -0.4536011799217367080, 0.2665933059059888421 ) ) ;
#82850 = CARTESIAN_POINT ( 'NONE',  ( -1.502624671916009680, -0.05778040916215560624, -0.4822834645669293319 ) ) ;
#82851 = CARTESIAN_POINT ( 'NONE',  ( -0.6364829396325453192, -0.08942795157528024563, -0.3641732283464568787 ) ) ;
#82852 = CARTESIAN_POINT ( 'NONE',  ( -0.3503937007874015630, -0.3044824468161027586, -0.01968503937007903132 ) ) ;
#82853 = CARTESIAN_POINT ( 'NONE',  ( -1.108923884514435132, -0.3162353388693405765, 0.4822834645669290543 ) ) ;
#82854 = B_SPLINE_CURVE_WITH_KNOTS ( 'NONE', 3,
 ( #564, #51880, #26217, #43492, #69188, #11539, #62876 ),
 .UNSPECIFIED., .F., .F.,
 ( 4, 3, 4 ),
 ( 3.643951726750583631E-17, 0.001246232571205268744, 0.002492492258783277591 ),
 .UNSPECIFIED. ) ;
#82855 = CARTESIAN_POINT ( 'NONE',  ( -0.6496062992125976043, 0.1660481256975883668, -0.3530559997133364547 ) ) ;
#82856 = CARTESIAN_POINT ( 'NONE',  ( -0.3460692066303960313, 0.1998031496062989965, -0.5754593175853018883 ) ) ;
#82857 = CARTESIAN_POINT ( 'NONE',  ( -0.1958661417322836718, 0.3392501089628017219, -2.145013123359580387 ) ) ;
#82858 = CARTESIAN_POINT ( 'NONE',  ( 0.5971128608923890191, -0.5511811023622046335, 0.09757992244046803654 ) ) ;
#82859 = CARTESIAN_POINT ( 'NONE',  ( -0.1640419947506553400, -0.05778040916215560624, -0.4822834645669293319 ) ) ;
#82860 = CARTESIAN_POINT ( 'NONE',  ( -0.6430446194225712953, 0.05413385826771626580, -0.4176697321401330321 ) ) ;
#82861 = CARTESIAN_POINT ( 'NONE',  ( -0.7742782152230962556, -0.3690944881889765550, -0.3153832671262227771 ) ) ;
#82862 = CARTESIAN_POINT ( 'NONE',  ( -3.936634651216008418, 1.066061182819163955, 0.06215626018321074309 ) ) ;
#82863 = CARTESIAN_POINT ( 'NONE',  ( 0.1115485564304470323, 0.2952755905511811885, 0.1292274648535926551 ) ) ;
#82864 = CARTESIAN_POINT ( 'NONE',  ( -1.607611548556429737, -0.5511811023622046335, 0.09757992244046803654 ) ) ;
#82865 = CARTESIAN_POINT ( 'NONE',  ( 1.318897637795276356, 0.1660481256975883668, -0.3530559997133364547 ) ) ;
#82866 = CARTESIAN_POINT ( 'NONE',  ( 0.1265901696524990572, -0.4724409448818897017, -0.7152230971128609172 ) ) ;
#82867 = CARTESIAN_POINT ( 'NONE',  ( -0.1958661417322833942, -0.3392501089628018884, -2.267079683235907694 ) ) ;
#82868 = ORIENTED_EDGE ( 'NONE', *, *, #57258, .T. ) ;
#82869 = CARTESIAN_POINT ( 'NONE',  ( -1.187664041994750175, -0.05778040916215560624, -0.4822834645669293319 ) ) ;
#82870 = CARTESIAN_POINT ( 'NONE',  ( -0.6824146981627291497, -0.6046776061558809534, -0.2411417322834644161 ) ) ;
#82871 = CARTESIAN_POINT ( 'NONE',  ( 1.456692913385827515, 0.2952755905511811885, 0.000000000000000000 ) ) ;
#82872 = CARTESIAN_POINT ( 'NONE',  ( 0.2867679344610365999, -0.2867679344610365444, -2.072834645669291209 ) ) ;
#82873 = CARTESIAN_POINT ( 'NONE',  ( 0.1882840440723353992, 0.3436793299028297333, -1.220472440944881942 ) ) ;
#82874 = EDGE_CURVE ( 'NONE', #26552, #24203, #14314, .T. ) ;
#82875 = CARTESIAN_POINT ( 'NONE',  ( 0.7808398950131241190, -0.05778040916215560624, -0.4822834645669293319 ) ) ;
#82876 = CARTESIAN_POINT ( 'NONE',  ( 0.05905511811023709395, -0.5400638737290844871, 0.3530559997133364547 ) ) ;
#82877 = CARTESIAN_POINT ( 'NONE',  ( 0.7086614173228347191, 1.325897125061109051E-17, -0.09842519685039344268 ) ) ;
#82878 = AXIS2_PLACEMENT_3D ( 'NONE', #19476, #43888, #50616 ) ;
#82879 = CIRCLE ( 'NONE', #60058, 0.09842519685039351207 ) ;
#82881 = DIRECTION ( 'NONE',  ( 0.000000000000000000, -1.000000000000000000, 0.000000000000000000 ) ) ;
#82880 = VECTOR ( 'NONE', #13745, 39.37007874015748143 ) ;
#82882 = CARTESIAN_POINT ( 'NONE',  ( 1.036745406824147508, -0.3690944881889765550, -0.3153832671262227771 ) ) ;
#82883 = CARTESIAN_POINT ( 'NONE',  ( -0.2925321140481932924, 0.2925321140481931814, -1.122047244094488194 ) ) ;
#82884 = ORIENTED_EDGE ( 'NONE', *, *, #31934, .T. ) ;
#82885 = CARTESIAN_POINT ( 'NONE',  ( -0.1049643490035302024, -0.3917322834645671215, -2.898950131233595684 ) ) ;
#82886 = ORIENTED_EDGE ( 'NONE', *, *, #63426, .F. ) ;
#82887 = CARTESIAN_POINT ( 'NONE',  ( 0.5446194225721792126, -0.05778040916215560624, -0.4822834645669293319 ) ) ;
#82888 = CARTESIAN_POINT ( 'NONE',  ( -0.6102362204724400829, 0.1660481256975885056, 0.3530559997133364547 ) ) ;
#82889 = CARTESIAN_POINT ( 'NONE',  ( -1.377952755905511140, -0.6692913385826771977, 8.415575281601705876E-17 ) ) ;
#82890 = CARTESIAN_POINT ( 'NONE',  ( 0.6430446194225729606, -0.4281496062992127816, -0.4176697321401328100 ) ) ;
#82891 = CARTESIAN_POINT ( 'NONE',  ( 1.653543307086614789, -0.1870078740157479769, 0.4822834645669291653 ) ) ;
#82892 = CARTESIAN_POINT ( 'NONE',  ( 1.555118110236221041, -0.5400638737290844871, 0.3530559997133364547 ) ) ;
#82893 = CARTESIAN_POINT ( 'NONE',  ( 0.09842519685039434474, 0.1660481256975885056, 0.3530559997133364547 ) ) ;
#82894 = CARTESIAN_POINT ( 'NONE',  ( -1.174540682414697335, -0.05778040916215522460, 0.4822834645669289988 ) ) ;
#82895 = CARTESIAN_POINT ( 'NONE',  ( 1.509186351706037543, -0.4281496062992127816, -0.4176697321401328100 ) ) ;
#82896 = CARTESIAN_POINT ( 'NONE',  ( 1.548556430446194954, 0.2306618581243847221, -0.2411417322834647770 ) ) ;
#82897 = CARTESIAN_POINT ( 'NONE',  ( -9.594673741351313045E-17, 0.3917322834645670104, -0.1496062992125983815 ) ) ;
#82898 = CARTESIAN_POINT ( 'NONE',  ( 1.056430446194226658, 0.1771653543307087630, 0.09757992244046791164 ) ) ;
#82899 = VERTEX_POINT ( 'NONE', #7792 ) ;
#82900 = CARTESIAN_POINT ( 'NONE',  ( -0.1058382717557497937, -0.3949938075777411628, -0.07217847769028878924 ) ) ;
#82901 = ORIENTED_EDGE ( 'NONE', *, *, #47017, .T. ) ;
#82902 = CARTESIAN_POINT ( 'NONE',  ( 0.1115485564304467270, -0.5511811023622048555, -0.09757992244046775898 ) ) ;
#82903 = CARTESIAN_POINT ( 'NONE',  ( 2.593372381816078764, 1.408244132531268011, -0.4567322424080935139 ) ) ;
#82904 = CARTESIAN_POINT ( 'NONE',  ( 0.1377952755905518800, -0.5400638737290844871, 0.3530559997133364547 ) ) ;
#82905 = CARTESIAN_POINT ( 'NONE',  ( 0.5839895013123367340, -0.6692913385826773087, -0.1292274648535924053 ) ) ;
#82906 = CARTESIAN_POINT ( 'NONE',  ( -0.6627296587926503335, -0.6692913385826771977, 0.1292274648535927661 ) ) ;
#82907 = CARTESIAN_POINT ( 'NONE',  ( 0.1049643490035303967, 0.3917322834645670659, -1.879940575624358789 ) ) ;
#82908 = CARTESIAN_POINT ( 'NONE',  ( -1.174540682414697335, -0.05778040916215522460, 0.4822834645669289988 ) ) ;
#82909 = CARTESIAN_POINT ( 'NONE',  ( 0.3917322834645669549, 0.1049643490035304660, -2.729002624671915900 ) ) ;
#82910 = CARTESIAN_POINT ( 'NONE',  ( 1.213910761154856299, -0.5511811023622048555, -0.09757992244046775898 ) ) ;
#82911 = CARTESIAN_POINT ( 'NONE',  ( 0.7742782152230979209, 0.05413385826771626580, -0.4176697321401330321 ) ) ;
#82912 = CARTESIAN_POINT ( 'NONE',  ( 0.5839895013123367340, 0.2952755905511811885, 0.1292274648535926551 ) ) ;
#82913 = EDGE_CURVE ( 'NONE', #49776, #25136, #70504, .T. ) ;
#82914 = CARTESIAN_POINT ( 'NONE',  ( -9.787531504996567848E-17, 0.3996062992125986035, -0.7874015748031496509 ) ) ;
#82915 = CARTESIAN_POINT ( 'NONE',  ( -1.443569553805773564, -0.6046776061558807314, 0.2411417322834647770 ) ) ;
#82916 = CARTESIAN_POINT ( 'NONE',  ( 0.1070741851644054776, -0.3996062992125984925, -0.4770341207349080848 ) ) ;
#82917 = CARTESIAN_POINT ( 'NONE',  ( 0.3996062992125985480, 2.446882876249141654E-17, -0.1948818897637795700 ) ) ;
#82918 = CARTESIAN_POINT ( 'NONE',  ( -0.2493438320209966919, 0.05413385826771626580, -0.4176697321401330321 ) ) ;
#82919 = CARTESIAN_POINT ( 'NONE',  ( 0.1998031496062992740, 0.3460692066303959757, -2.664041994750656173 ) ) ;
#82920 = CARTESIAN_POINT ( 'NONE',  ( -9.594673741351313045E-17, 0.3917322834645670104, -1.816929133858267820 ) ) ;
#82921 = CARTESIAN_POINT ( 'NONE',  ( 1.430446194225722500, 0.05413385826771666132, 0.4176697321401328100 ) ) ;
#82922 = CARTESIAN_POINT ( 'NONE',  ( 1.561679790026247350, 0.05413385826771626580, -0.4176697321401330321 ) ) ;
#82923 = CARTESIAN_POINT ( 'NONE',  ( 0.01968503937007957949, -0.4536011799217368745, -0.2665933059059886201 ) ) ;
#82924 = CARTESIAN_POINT ( 'NONE',  ( 0.7086614173228352742, -0.1870078740157480879, -0.4822834645669291653 ) ) ;
#82925 = CARTESIAN_POINT ( 'NONE',  ( 0.3458507752293908943, 0.3458507752293908943, -1.316929133858267598 ) ) ;
#82926 = CARTESIAN_POINT ( 'NONE',  ( 0.1902887139107617975, -0.5511811023622048555, -0.09757992244046775898 ) ) ;
#82927 = CARTESIAN_POINT ( 'NONE',  ( 0.2099737532808405305, 0.2306618581243847221, -0.2411417322834647770 ) ) ;
#82928 = CARTESIAN_POINT ( 'NONE',  ( 0.1974969037888704704, 0.3420746716998660508, -1.008530183727033958 ) ) ;
#82929 = CARTESIAN_POINT ( 'NONE',  ( -1.338582677165353729, -0.1870078740157480879, -0.4822834645669291653 ) ) ;
#82930 = CARTESIAN_POINT ( 'NONE',  ( 0.9711286089238851948, 0.1283753931104748280, 0.1820866141732283561 ) ) ;
#82931 = CARTESIAN_POINT ( 'NONE',  ( 0.3280839895013130669, 0.009842519685039463617, 0.3409548833797002576 ) ) ;
#82932 = CARTESIAN_POINT ( 'NONE',  ( -0.2952755905511804668, 0.1660481256975885056, 0.3530559997133364547 ) ) ;
#82933 = CARTESIAN_POINT ( 'NONE',  ( 0.02624671916010564918, -0.5023911411419708095, -0.1820866141732282451 ) ) ;
#82934 = FACE_OUTER_BOUND ( 'NONE', #53056, .T. ) ;
#82935 = CARTESIAN_POINT ( 'NONE',  ( -0.3280839895013117347, -0.4281496062992124485, 0.4176697321401328655 ) ) ;
#82936 = CARTESIAN_POINT ( 'NONE',  ( 0.2034120734908142214, 0.1771653543307087075, -0.09757992244046823083 ) ) ;
#82937 = VECTOR ( 'NONE', #16550, 39.37007874015748143 ) ;
#82938 = CARTESIAN_POINT ( 'NONE',  ( 0.3996062992125985480, 2.446882876249141654E-17, -2.242125984251968518 ) ) ;
#82939 = CARTESIAN_POINT ( 'NONE',  ( -0.2034120734908128059, 0.2952755905511811885, 0.1292274648535926551 ) ) ;
#82940 = EDGE_CURVE ( 'NONE', #78564, #38952, #11223, .T. ) ;
#82941 = CIRCLE ( 'NONE', #14418, 1.929133858267716661 ) ;
#82942 = AXIS2_PLACEMENT_3D ( 'NONE', #70455, #12813, #51492 ) ;
#82943 = CARTESIAN_POINT ( 'NONE',  ( 1.318897637795276356, -0.4536011799217367080, 0.2665933059059888421 ) ) ;
#82944 = CARTESIAN_POINT ( 'NONE',  ( 0.4831401376419955929, 2.606013654608237919E-15, 0.4118477457932982477 ) ) ;
#82945 = CARTESIAN_POINT ( 'NONE',  ( -0.3412073490813641308, -0.5023911411419708095, 0.1820866141732285504 ) ) ;
#82946 = CARTESIAN_POINT ( 'NONE',  ( -0.8661417322834640276, -0.1870078740157480601, -0.3641732283464567677 ) ) ;
#82947 = CARTESIAN_POINT ( 'NONE',  ( -0.3543307086614165824, 0.2952755905511811885, 0.000000000000000000 ) ) ;
#82948 = CARTESIAN_POINT ( 'NONE',  ( -0.1574803149606292529, -0.1870078740157479769, 0.4822834645669291653 ) ) ;
#82949 = CARTESIAN_POINT ( 'NONE',  ( 0.8923884514435703741, 0.1283753931104748280, 0.1820866141732283561 ) ) ;
#82950 = CARTESIAN_POINT ( 'NONE',  ( -1.692913385826770645, 0.1771653543307087630, 0.000000000000000000 ) ) ;
#82951 = CARTESIAN_POINT ( 'NONE',  ( 1.489501312335958172, -0.08942795157528024563, -0.3641732283464568787 ) ) ;
#82952 = CARTESIAN_POINT ( 'NONE',  ( 0.6496062992125991586, -0.5400638737290845981, -0.3530559997133363437 ) ) ;
#82953 = CARTESIAN_POINT ( 'NONE',  ( 0.4741766535082888590, 1.520234135998520753, -2.169568943720849852 ) ) ;
#82954 = CARTESIAN_POINT ( 'NONE',  ( -0.2690288713910754526, 0.2952755905511810774, -0.1292274648535930714 ) ) ;
#82955 = CARTESIAN_POINT ( 'NONE',  ( 0.3917322834645669549, 0.1049643490035304660, -0.9967191601049870675 ) ) ;
#82956 = CARTESIAN_POINT ( 'NONE',  ( 0.9514435695538062676, -0.3162353388693409650, -0.4822834645669289433 ) ) ;
#82957 = CARTESIAN_POINT ( 'NONE',  ( 0.4855643044619430415, -0.4281496062992127816, -0.4176697321401328100 ) ) ;
#82958 = CARTESIAN_POINT ( 'NONE',  ( 0.000000000000000000, 0.000000000000000000, -1.929133858267716661 ) ) ;
#82959 = CARTESIAN_POINT ( 'NONE',  ( 0.3412073490813655186, -0.5023911411419708095, -0.1820866141732282451 ) ) ;
#82960 = CARTESIAN_POINT ( 'NONE',  ( 1.266404199475066328, -0.3162353388693409650, -0.4822834645669289433 ) ) ;
#82961 = CARTESIAN_POINT ( 'NONE',  ( -0.4133858267716528645, 0.07958543189024071263, -0.2665933059059888421 ) ) ;
#82962 = CARTESIAN_POINT ( 'NONE',  ( -0.5708661417322825615, -0.5400638737290844871, 0.3530559997133364547 ) ) ;
#82963 = DIRECTION ( 'NONE',  ( 1.000000000000000000, 0.000000000000000000, 0.000000000000000000 ) ) ;
#82964 = CARTESIAN_POINT ( 'NONE',  ( 0.4002624671916016896, -0.3162353388693409650, -0.4822834645669289433 ) ) ;
#82965 = CARTESIAN_POINT ( 'NONE',  ( -0.8267716535433065062, 0.2952755905511811885, 0.000000000000000000 ) ) ;
#82966 = CARTESIAN_POINT ( 'NONE',  ( -0.5971128608923877978, 0.1771653543307087630, 0.09757992244046791164 ) ) ;
#82967 = CARTESIAN_POINT ( 'NONE',  ( 0.4790026246719167324, -0.05778040916215522460, 0.4822834645669289988 ) ) ;
#82968 = CARTESIAN_POINT ( 'NONE',  ( -1.423884514435694859, -0.3162353388693405765, 0.4822834645669290543 ) ) ;
#82969 = CARTESIAN_POINT ( 'NONE',  ( -0.3740157480314953431, 0.1660481256975885056, 0.3530559997133364547 ) ) ;
#82970 = LINE ( 'NONE', #1318, #82117 ) ;
#82972 = CARTESIAN_POINT ( 'NONE',  ( 1.194225721784777594, -0.4281496062992127816, -0.4176697321401328100 ) ) ;
#82971 = FACE_OUTER_BOUND ( 'NONE', #74428, .T. ) ;
#82973 = CARTESIAN_POINT ( 'NONE',  ( 1.266404199475066328, -0.3162353388693409650, -0.4822834645669289433 ) ) ;
#82974 = CARTESIAN_POINT ( 'NONE',  ( -0.2867679344610366554, 0.2867679344610365444, -2.059055118110236116 ) ) ;
#82975 = DIRECTION ( 'NONE',  ( 0.000000000000000000, -1.000000000000000000, 0.000000000000000000 ) ) ;
#82976 = CARTESIAN_POINT ( 'NONE',  ( -1.062992125984250968, 0.2952755905511811885, 0.000000000000000000 ) ) ;
#82977 = CARTESIAN_POINT ( 'NONE',  ( -0.4091458600556402980, -0.2362204724409451284, -0.3674540682414698112 ) ) ;
#82978 = CARTESIAN_POINT ( 'NONE',  ( -0.2891555358219908833, -0.2891555358219912164, -2.578740157480315265 ) ) ;
#82979 = VERTEX_POINT ( 'NONE', #25457 ) ;
#82980 = CARTESIAN_POINT ( 'NONE',  ( 0.06561679790026316017, -0.3690944881889763329, 0.3153832671262228327 ) ) ;
#82981 = CARTESIAN_POINT ( 'NONE',  ( -0.2867679344610364334, -0.2867679344610367109, -1.311023622047244430 ) ) ;
#82982 = CARTESIAN_POINT ( 'NONE',  ( 0.6758530183727039509, 0.2952755905511810774, -0.1292274648535930714 ) ) ;
#82983 = CARTESIAN_POINT ( 'NONE',  ( -0.01150853369506071172, 0.3951562584566651326, -2.755905511811586273 ) ) ;
#82984 = DIRECTION ( 'NONE',  ( 0.000000000000000000, 1.000000000000000000, 0.000000000000000000 ) ) ;
#82985 = CARTESIAN_POINT ( 'NONE',  ( -0.5905511811023613777, -0.5511811023622047445, 6.969142054262312111E-17 ) ) ;
#82986 = CARTESIAN_POINT ( 'NONE',  ( -1.157146581871515012E-16, 0.4724409448818898682, 0.000000000000000000 ) ) ;
#82987 = CARTESIAN_POINT ( 'NONE',  ( 1.213910761154856299, 0.2952755905511811885, 0.1292274648535926551 ) ) ;
#82988 = CARTESIAN_POINT ( 'NONE',  ( 1.036745406824147508, -0.3690944881889765550, -0.3153832671262227771 ) ) ;
#82989 = CARTESIAN_POINT ( 'NONE',  ( -0.1115485564304453947, -0.6692913385826771977, 0.1292274648535927661 ) ) ;
#82990 = CARTESIAN_POINT ( 'NONE',  ( 0.1958661417322834497, 0.3392501089628018329, -0.6968310779189482718 ) ) ;
#82991 = CARTESIAN_POINT ( 'NONE',  ( -0.3674540682414689785, 0.2306618581243848609, 0.2411417322834645549 ) ) ;
#82992 = CARTESIAN_POINT ( 'NONE',  ( -1.161417322834644716, -0.4536011799217368745, -0.2665933059059886201 ) ) ;
#82993 = CARTESIAN_POINT ( 'NONE',  ( -0.3412073490813641308, -0.6046776061558807314, 0.2411417322834647770 ) ) ;
#82994 = CARTESIAN_POINT ( 'NONE',  ( 0.000000000000000000, 0.5905511811023621549, 0.000000000000000000 ) ) ;
#82995 = CARTESIAN_POINT ( 'NONE',  ( -8.318810292902005415E-17, 2.401574803149606474, -0.4915354330708645580 ) ) ;
#82996 = ORIENTED_EDGE ( 'NONE', *, *, #50355, .T. ) ;
#82997 = CARTESIAN_POINT ( 'NONE',  ( -0.1049643490035307158, 0.3917322834645670104, -2.050544250165041493 ) ) ;
#82998 = CARTESIAN_POINT ( 'NONE',  ( 0.5774278215223104249, 0.2306618581243848609, 0.2411417322834645549 ) ) ;
#82999 = ORIENTED_EDGE ( 'NONE', *, *, #78384, .F. ) ;
#83000 = CARTESIAN_POINT ( 'NONE',  ( -0.6824146981627291497, -0.6046776061558809534, -0.2411417322834644161 ) ) ;
#83001 = CARTESIAN_POINT ( 'NONE',  ( 1.233595800524935227, -0.6046776061558807314, 0.2411417322834647770 ) ) ;
#83002 = CARTESIAN_POINT ( 'NONE',  ( 0.4790026246719167324, -0.05778040916215522460, 0.4822834645669289988 ) ) ;
#83003 = CARTESIAN_POINT ( 'NONE',  ( -0.1574803149606292529, -0.1870078740157480879, -0.4822834645669291653 ) ) ;
#83004 = CARTESIAN_POINT ( 'NONE',  ( 0.1049643490035303689, 0.3917322834645670104, -1.337926509186352142 ) ) ;
#83005 = CARTESIAN_POINT ( 'NONE',  ( -0.8136482939632537770, -0.6046776061558807314, 0.2411417322834647770 ) ) ;
#83006 = CARTESIAN_POINT ( 'NONE',  ( -0.006561679790025524116, -0.05778040916215560624, -0.4822834645669293319 ) ) ;
#83007 = CARTESIAN_POINT ( 'NONE',  ( -0.9317585301837263412, -0.4281496062992127816, -0.4176697321401328100 ) ) ;
#83008 = CARTESIAN_POINT ( 'NONE',  ( -0.04593175853018302557, 0.1771653543307087630, 0.09757992244046791164 ) ) ;
#83009 = CARTESIAN_POINT ( 'NONE',  ( -0.009627693921946872679, 0.3964540044758437243, 2.415985422253605141E-12 ) ) ;
#83010 = CARTESIAN_POINT ( 'NONE',  ( -0.1706036745406816491, -0.4281496062992124485, 0.4176697321401328655 ) ) ;
#83011 = DIRECTION ( 'NONE',  ( 0.000000000000000000, -0.000000000000000000, 1.000000000000000000 ) ) ;
#83012 = CARTESIAN_POINT ( 'NONE',  ( 1.049868766404200127, -0.6046776061558809534, -0.2411417322834644161 ) ) ;
#83013 = CARTESIAN_POINT ( 'NONE',  ( -0.1958661417322834220, -0.3392501089628018884, -2.892388451443569153 ) ) ;
#83014 = VERTEX_POINT ( 'NONE', #20413 ) ;
#83015 = ORIENTED_EDGE ( 'NONE', *, *, #47547, .T. ) ;
#83016 = CARTESIAN_POINT ( 'NONE',  ( 0.1181102362204730916, 0.2952755905511811885, 0.000000000000000000 ) ) ;
#83017 = CARTESIAN_POINT ( 'NONE',  ( 0.2821522309711292364, -0.5511811023622046335, 0.09757992244046803654 ) ) ;
#83019 = DIRECTION ( 'NONE',  ( 0.000000000000000000, -0.000000000000000000, 1.000000000000000000 ) ) ;
#83018 = CARTESIAN_POINT ( 'NONE',  ( 1.371391076115485941, 0.1771653543307087630, 0.09757992244046791164 ) ) ;
#83020 = CARTESIAN_POINT ( 'NONE',  ( -0.3917322834645669549, -0.1049643490035306603, -1.232939632545931863 ) ) ;
#83021 = CARTESIAN_POINT ( 'NONE',  ( 0.4091458600556403535, 0.2362204724409449896, -0.2080052493438320216 ) ) ;
#83022 = CARTESIAN_POINT ( 'NONE',  ( 2.154527559055120278, 0.03937007874015747977, -0.4677827689124846589 ) ) ;
#83023 = CARTESIAN_POINT ( 'NONE',  ( 1.594488188976378673, 0.1660481256975885056, 0.3530559997133364547 ) ) ;
#83024 = CARTESIAN_POINT ( 'NONE',  ( -0.2925321140481930149, -0.2925321140481933480, -2.655511811023622215 ) ) ;
#83025 = CARTESIAN_POINT ( 'NONE',  ( 0.4461942257217855201, -0.6046776061558807314, 0.2411417322834647770 ) ) ;
#83026 = CARTESIAN_POINT ( 'NONE',  ( -1.279527559055116948, 0.1660481256975883668, -0.3530559997133364547 ) ) ;
#83027 = CARTESIAN_POINT ( 'NONE',  ( -1.292650918635170010, -0.6692913385826771977, 0.1292274648535927661 ) ) ;
#83028 = CARTESIAN_POINT ( 'NONE',  ( 0.3083989501312343062, -0.3162353388693405765, 0.4822834645669290543 ) ) ;
#83029 = CARTESIAN_POINT ( 'NONE',  ( 0.3949938075777408852, 0.1058382717557500435, 0.1135170603674540979 ) ) ;
#83030 = CARTESIAN_POINT ( 'NONE',  ( 1.686351706036745890, 0.2952755905511811885, 0.1292274648535926551 ) ) ;
#83031 = CARTESIAN_POINT ( 'NONE',  ( 0.9383202099737536495, -0.3162353388693405765, 0.4822834645669290543 ) ) ;
#83032 = CARTESIAN_POINT ( 'NONE',  ( 1.574803149606299746, -0.1870078740157480601, -0.3641732283464567677 ) ) ;
#83033 = CARTESIAN_POINT ( 'NONE',  ( 0.6758530183727039509, -0.5511811023622046335, 0.09757992244046803654 ) ) ;
#83034 = CARTESIAN_POINT ( 'NONE',  ( -0.6496062992125976043, 0.1660481256975883668, -0.3530559997133364547 ) ) ;
#83035 = CARTESIAN_POINT ( 'NONE',  ( 0.3460692066303958092, 0.1998031496062993018, -0.3654855643044619407 ) ) ;
#83036 = CARTESIAN_POINT ( 'NONE',  ( 1.574803149606299746, -0.1870078740157480879, -0.4822834645669291653 ) ) ;
#83037 = CARTESIAN_POINT ( 'NONE',  ( 0.3392501089628018884, -0.1958661417322834220, -0.09711286089238840846 ) ) ;
#83038 = EDGE_CURVE ( 'NONE', #58442, #16468, #83138, .T. ) ;
#83040 = LINE ( 'NONE', #77143, #78877 ) ;
#83039 = CARTESIAN_POINT ( 'NONE',  ( 0.7414698162729663755, 0.2952755905511811885, 0.1292274648535926551 ) ) ;
#83041 = CARTESIAN_POINT ( 'NONE',  ( -1.476377952755905110, -0.4536011799217368745, -0.2665933059059886201 ) ) ;
#83042 = CARTESIAN_POINT ( 'NONE',  ( -0.09186351706036663400, -0.4281496062992124485, 0.4176697321401328655 ) ) ;
#83043 = CARTESIAN_POINT ( 'NONE',  ( 0.7020997375328090762, -0.08942795157528024563, -0.3641732283464568787 ) ) ;
#83044 = CARTESIAN_POINT ( 'NONE',  ( 0.9120734908136490793, 0.2952755905511810774, -0.1292274648535930714 ) ) ;
#83045 = CYLINDRICAL_SURFACE ( 'NONE', #66681, 0.4744094488188972947 ) ;
#83046 = CARTESIAN_POINT ( 'NONE',  ( -0.5380577427821514602, -0.3690944881889765550, -0.3153832671262227771 ) ) ;
#83047 = CARTESIAN_POINT ( 'NONE',  ( -0.5118110236220466680, -0.6692913385826771977, 8.415575281601705876E-17 ) ) ;
#83048 = CARTESIAN_POINT ( 'NONE',  ( 1.666666666666667185, 0.05413385826771666132, 0.4176697321401328100 ) ) ;
#83049 = CARTESIAN_POINT ( 'NONE',  ( -0.9645669291338575535, -0.5400638737290844871, 0.3530559997133364547 ) ) ;
#83050 = CARTESIAN_POINT ( 'NONE',  ( 1.069553805774278832, 0.2952755905511810774, -0.1292274648535930714 ) ) ;
#83051 = CARTESIAN_POINT ( 'NONE',  ( -0.1958661417322836995, 0.3392501089628017219, -0.7972634102700281167 ) ) ;
#83052 = CARTESIAN_POINT ( 'NONE',  ( -1.522309711286088607, -0.5023911411419708095, 0.1820866141732285504 ) ) ;
#83053 = CARTESIAN_POINT ( 'NONE',  ( 1.968503937007874072, 0.000000000000000000, 5.701968306260621233 ) ) ;
#83054 = CARTESIAN_POINT ( 'NONE',  ( 1.181102362204724976, -0.1870078740157480879, -0.4822834645669291653 ) ) ;
#83055 = AXIS2_PLACEMENT_3D ( 'NONE', #56848, #44621, #82546 ) ;
#83056 = CARTESIAN_POINT ( 'NONE',  ( -0.1265901696524986964, -0.4724409448818899238, -2.353674540682414218 ) ) ;
#83057 = CARTESIAN_POINT ( 'NONE',  ( -1.574803149606298636, -0.1870078740157479769, 0.4822834645669291653 ) ) ;
#83058 = CARTESIAN_POINT ( 'NONE',  ( 1.620734908136483465, -0.6692913385826771977, 0.1292274648535927661 ) ) ;
#83059 = CARTESIAN_POINT ( 'NONE',  ( -0.9251968503937002541, 0.07958543189024085140, 0.2665933059059887866 ) ) ;
#83060 = EDGE_CURVE ( 'NONE', #74617, #36894, #63478, .T. ) ;
#83061 = CARTESIAN_POINT ( 'NONE',  ( 1.587926509186352586, -0.3690944881889765550, -0.3153832671262227771 ) ) ;
#83062 = CARTESIAN_POINT ( 'NONE',  ( -0.4002624671916004129, -0.3162353388693405765, 0.4822834645669290543 ) ) ;
#83063 = CARTESIAN_POINT ( 'NONE',  ( -0.3083989501312330295, -0.2845877964562161244, -0.3641732283464567121 ) ) ;
#83064 = CARTESIAN_POINT ( 'NONE',  ( -1.640419947506561060, -0.3690944881889765550, -0.3153832671262227771 ) ) ;
#83065 = CARTESIAN_POINT ( 'NONE',  ( 1.036745406824147508, -0.3690944881889765550, -0.3153832671262227771 ) ) ;
#83066 = CARTESIAN_POINT ( 'NONE',  ( 0.9514435695538062676, -0.3162353388693409650, -0.4822834645669289433 ) ) ;
#83067 = CARTESIAN_POINT ( 'NONE',  ( 1.450131233595801428, 0.2952755905511811885, 0.1292274648535926551 ) ) ;
#83068 = CARTESIAN_POINT ( 'NONE',  ( 0.1902887139107617975, -0.5511811023622048555, -0.09757992244046775898 ) ) ;
#83069 = CARTESIAN_POINT ( 'NONE',  ( 0.5971128608923891301, 0.2952755905511810774, -0.1292274648535930714 ) ) ;
#83070 = EDGE_CURVE ( 'NONE', #65458, #9504, #18076, .T. ) ;
#83071 = CARTESIAN_POINT ( 'NONE',  ( 0.7677165354330716118, -0.4536011799217367080, 0.2665933059059888421 ) ) ;
#83072 = CARTESIAN_POINT ( 'NONE',  ( 1.568241469816273437, -0.3162353388693405765, 0.4822834645669290543 ) ) ;
#83073 = CARTESIAN_POINT ( 'NONE',  ( -1.200787401574802349, -0.5400638737290844871, 0.3530559997133364547 ) ) ;
#83074 = CARTESIAN_POINT ( 'NONE',  ( -0.4396325459317579898, 0.2952755905511811885, 0.1292274648535926551 ) ) ;
#83075 = CARTESIAN_POINT ( 'NONE',  ( -0.1998031496062994683, 0.3460692066303958092, -0.4855643044619422644 ) ) ;
#83076 = CARTESIAN_POINT ( 'NONE',  ( 0.3460692066303959202, -0.1998031496062991630, -2.543963254593176071 ) ) ;
#83077 = CARTESIAN_POINT ( 'NONE',  ( 0.2821522309711292364, -0.6692913385826771977, 0.1292274648535927661 ) ) ;
#83078 = CARTESIAN_POINT ( 'NONE',  ( 0.9645669291338588858, 0.07958543189024085140, 0.2665933059059887866 ) ) ;
#83079 = CARTESIAN_POINT ( 'NONE',  ( -0.3412073490813641308, 0.2306618581243847221, -0.2411417322834647770 ) ) ;
#83080 = CARTESIAN_POINT ( 'NONE',  ( 0.4396325459317590445, -0.6692913385826771977, 0.1292274648535927661 ) ) ;
#83081 = CARTESIAN_POINT ( 'NONE',  ( -0.1070741851644056997, 0.3996062992125986035, -2.053805774278214979 ) ) ;
#83082 = CARTESIAN_POINT ( 'NONE',  ( 0.3949938075777409408, 0.1058382717557500574, -1.384514435695538337 ) ) ;
#83083 = CARTESIAN_POINT ( 'NONE',  ( -0.3996062992125987146, 0.1070741851644051862, -2.867454068241469756 ) ) ;
#83084 = CARTESIAN_POINT ( 'NONE',  ( 1.579022939845507243E-16, 0.000000000000000000, 1.289370078740159409 ) ) ;
#83085 = CARTESIAN_POINT ( 'NONE',  ( -0.1958661417322834220, -0.3392501089628018884, -0.8451443569553805935 ) ) ;
#83086 = CARTESIAN_POINT ( 'NONE',  ( -0.8005249343832013809, -0.3690944881889763329, 0.3153832671262228327 ) ) ;
#83087 = CARTESIAN_POINT ( 'NONE',  ( -1.332020997375327642, -0.3162353388693409650, -0.4822834645669289433 ) ) ;
#83088 = CARTESIAN_POINT ( 'NONE',  ( -0.2891555358219911054, 0.2891555358219909388, -2.773622047244094446 ) ) ;
#83089 = EDGE_CURVE ( 'NONE', #52887, #65211, #74258, .T. ) ;
#83090 = CARTESIAN_POINT ( 'NONE',  ( 0.8267716535433078384, -0.6692913385826771977, 8.415575281601705876E-17 ) ) ;
#83091 = CARTESIAN_POINT ( 'NONE',  ( 1.371391076115485719, -0.6692913385826773087, -0.1292274648535924053 ) ) ;
#83092 = CARTESIAN_POINT ( 'NONE',  ( 0.7611548556430451917, -0.6046776061558807314, 0.2411417322834647770 ) ) ;
#83093 = CARTESIAN_POINT ( 'NONE',  ( 0.2362204724409449064, 0.4091458600556404646, -0.06364829396325459576 ) ) ;
#83094 = CARTESIAN_POINT ( 'NONE',  ( 4.893765752498283924E-17, -0.3996062992125986035, -1.968503937007873850 ) ) ;
#83095 = CARTESIAN_POINT ( 'NONE',  ( 1.548556430446194954, 0.2306618581243847221, -0.2411417322834647770 ) ) ;
#83096 = CARTESIAN_POINT ( 'NONE',  ( 0.5971128608923890191, -0.6692913385826771977, 0.1292274648535927661 ) ) ;
#83097 = CARTESIAN_POINT ( 'NONE',  ( 0.6824146981627303710, 0.2306618581243847221, -0.2411417322834647770 ) ) ;
#83098 = EDGE_CURVE ( 'NONE', #72978, #8695, #43582, .T. ) ;
#83099 = CARTESIAN_POINT ( 'NONE',  ( 0.8333333333333340365, 0.1771653543307087075, -0.09757992244046823083 ) ) ;
#83100 = CARTESIAN_POINT ( 'NONE',  ( 1.240157480314961314, 0.1660481256975883668, -0.3530559997133364547 ) ) ;
#83101 =( REPRESENTATION_RELATIONSHIP ('NONE','NONE', #79348, #76132 ) REPRESENTATION_RELATIONSHIP_WITH_TRANSFORMATION ( #3124 )SHAPE_REPRESENTATION_RELATIONSHIP( ) );
#83102 = CARTESIAN_POINT ( 'NONE',  ( 0.3917322834645670104, 2.398668435337828261E-17, -0.04527559055118119541 ) ) ;
#83103 = CARTESIAN_POINT ( 'NONE',  ( 0.3215223097112867578, -0.05778040916215522460, 0.4822834645669289988 ) ) ;
#83104 = CARTESIAN_POINT ( 'NONE',  ( 1.095800524934383846, -0.05778040916215560624, -0.4822834645669293319 ) ) ;
#83105 = CARTESIAN_POINT ( 'NONE',  ( 0.2296587926509192634, -0.3162353388693405765, 0.4822834645669290543 ) ) ;
#83106 = CARTESIAN_POINT ( 'NONE',  ( 1.102362204724410155, -0.1870078740157480601, -0.3641732283464567677 ) ) ;
#83107 = CARTESIAN_POINT ( 'NONE',  ( -0.9580052493438311334, -0.4281496062992124485, 0.4176697321401328655 ) ) ;
#83108 = CARTESIAN_POINT ( 'NONE',  ( -1.043307086614172707, 0.1660481256975883668, -0.3530559997133364547 ) ) ;
#83109 = CARTESIAN_POINT ( 'NONE',  ( 1.200787401574803681, -0.5400638737290845981, -0.3530559997133363437 ) ) ;
#83110 = CARTESIAN_POINT ( 'NONE',  ( -0.3917322834645671215, 0.1049643490035301469, -0.4324146981627298159 ) ) ;
#83111 = CARTESIAN_POINT ( 'NONE',  ( 4.797336870675656522E-17, -0.3917322834645670104, -1.330708661417322691 ) ) ;
#83112 = CARTESIAN_POINT ( 'NONE',  ( -0.1049643490035307020, 0.3917322834645669549, -2.675853018372703396 ) ) ;
#83113 = EDGE_CURVE ( 'NONE', #41264, #78537, #22302, .T. ) ;
#83114 = ORIENTED_EDGE ( 'NONE', *, *, #40447, .F. ) ;
#83115 = CARTESIAN_POINT ( 'NONE',  ( -0.1998031496062991907, -0.3460692066303959757, 0.09186351706036742504 ) ) ;
#83116 = EDGE_LOOP ( 'NONE', ( #39182, #57118, #28128, #49230 ) ) ;
#83117 = CARTESIAN_POINT ( 'NONE',  ( 1.502624671916010790, -0.05778040916215522460, 0.4822834645669289988 ) ) ;
#83118 = CARTESIAN_POINT ( 'NONE',  ( 1.272965879265092637, -0.004921259842519576551, 0.3153832671262227771 ) ) ;
#83119 = CARTESIAN_POINT ( 'NONE',  ( 0.3996062992125986035, 2.446882876249141962E-17, -1.377952755905511806 ) ) ;
#83120 = CARTESIAN_POINT ( 'NONE',  ( 1.443569553805774897, -0.5023911411419708095, -0.1820866141732282451 ) ) ;
#83121 = CARTESIAN_POINT ( 'NONE',  ( -0.5314960629921147151, 2.716535433070866645, -3.224202737261816942 ) ) ;
#83122 = CARTESIAN_POINT ( 'NONE',  ( -0.5314960629921148261, 2.755905511811024056, -3.184294706754632109 ) ) ;
#83123 = CARTESIAN_POINT ( 'NONE',  ( 0.1958661417322834775, 0.3392501089628018884, -0.7014435695538058235 ) ) ;
#83124 = CARTESIAN_POINT ( 'NONE',  ( -0.6824146981627288167, 0.1283753931104748280, 0.1820866141732283561 ) ) ;
#83125 = CARTESIAN_POINT ( 'NONE',  ( -1.522309711286088607, 0.1283753931104746893, -0.1820866141732285504 ) ) ;
#83126 = CARTESIAN_POINT ( 'NONE',  ( -1.443569553805773564, 0.2306618581243847221, -0.2411417322834647770 ) ) ;
#83127 = CARTESIAN_POINT ( 'NONE',  ( 0.2034120734908142214, 0.2952755905511810774, -0.1292274648535930714 ) ) ;
#83128 = CARTESIAN_POINT ( 'NONE',  ( 1.325459317585302665, 0.05413385826771626580, -0.4176697321401330321 ) ) ;
#83129 = ORIENTED_EDGE ( 'NONE', *, *, #50047, .F. ) ;
#83130 = CARTESIAN_POINT ( 'NONE',  ( 0.000000000000000000, 2.755905511811024056, 0.000000000000000000 ) ) ;
#83131 = DIRECTION ( 'NONE',  ( 1.000000000000000000, 0.000000000000000000, 0.000000000000000000 ) ) ;
#83132 = CARTESIAN_POINT ( 'NONE',  ( -0.4724409448818899238, 0.1265901696524986686, -2.080052493438320216 ) ) ;
#83133 = CARTESIAN_POINT ( 'NONE',  ( 0.000000000000000000, 0.04488074079120789317, 0.000000000000000000 ) ) ;
#83134 = CARTESIAN_POINT ( 'NONE',  ( -0.6692913385826764205, 0.1771653543307087630, 0.000000000000000000 ) ) ;
#83135 = CARTESIAN_POINT ( 'NONE',  ( -1.167979002624671470, 0.05413385826771666132, 0.4176697321401328100 ) ) ;
#83136 = CARTESIAN_POINT ( 'NONE',  ( 0.9055118110236227702, 0.2952755905511811885, 0.000000000000000000 ) ) ;
#83137 = EDGE_LOOP ( 'NONE', ( #61252, #81161, #82004, #71604 ) ) ;
#83139 = DIRECTION ( 'NONE',  ( 0.000000000000000000, 1.000000000000000000, 0.000000000000000000 ) ) ;
#83138 = LINE ( 'NONE', #46064, #54354 ) ;
#83140 = CARTESIAN_POINT ( 'NONE',  ( 1.345144356955381593, -0.05778040916215522460, 0.4822834645669289988 ) ) ;
#83141 = CARTESIAN_POINT ( 'NONE',  ( -1.437007874015747477, -0.5400638737290844871, 0.3530559997133364547 ) ) ;
#83143 = B_SPLINE_CURVE_WITH_KNOTS ( 'NONE', 3,
 ( #68026, #60039, #60454, #55370, #41918, #10370, #36028, #67612, #48647, #9943, #35615, #61278, #2395, #61702, #41102, #3631, #79417, #29299 ),
 .UNSPECIFIED., .F., .F.,
 ( 4, 2, 2, 2, 2, 2, 2, 2, 4 ),
 ( 0.000000000000000000, 2.503579457949756240E-05, 5.007158915899512480E-05, 0.0001001431783179882574, 0.0002002863566359730724, 0.0004005727132719426212, 0.0008011454265438807971, 0.001602290853087756173, 0.003204581706175506708 ),
 .UNSPECIFIED. ) ;
#83142 = CARTESIAN_POINT ( 'NONE',  ( 4.797336870675655290E-17, -0.3917322834645669549, -0.9461749099399457963 ) ) ;
#83144 = CARTESIAN_POINT ( 'NONE',  ( -0.3477690288713905509, -0.5511811023622046335, 0.09757992244046803654 ) ) ;
#83145 = CARTESIAN_POINT ( 'NONE',  ( -0.1049643490035307020, 0.3917322834645669549, -0.8786089238845143923 ) ) ;
#83146 = CARTESIAN_POINT ( 'NONE',  ( -0.7086614173228339419, -0.1870078740157479769, 0.3641732283464567677 ) ) ;
#83147 = CARTESIAN_POINT ( 'NONE',  ( 0.03280839895013198948, 0.1771653543307087630, 0.09757992244046791164 ) ) ;
#83148 = CARTESIAN_POINT ( 'NONE',  ( -0.04593175853018302557, -0.6692913385826773087, -0.1292274648535924053 ) ) ;
#83149 = CARTESIAN_POINT ( 'NONE',  ( -0.6955380577427815458, -0.004921259842519576551, 0.3153832671262227771 ) ) ;
#83150 = CARTESIAN_POINT ( 'NONE',  ( -0.1049643490035307020, 0.3917322834645669549, -2.675853018372703396 ) ) ;
#83151 = CARTESIAN_POINT ( 'NONE',  ( 1.233595800524935227, -0.6046776061558807314, 0.2411417322834647770 ) ) ;
#83152 = CARTESIAN_POINT ( 'NONE',  ( -1.266404199475064773, -0.05778040916215560624, -0.4822834645669293319 ) ) ;
#83153 = CARTESIAN_POINT ( 'NONE',  ( 0.1265901696524990294, -0.4724409448818896462, -1.106955380577427706 ) ) ;
#83154 = CARTESIAN_POINT ( 'NONE',  ( -0.2821522309711278487, 0.2952755905511811885, 0.1292274648535926551 ) ) ;
#83155 = ADVANCED_FACE ( 'NONE', ( #65868 ), #73443, .F. ) ;
#83156 = CARTESIAN_POINT ( 'NONE',  ( -0.8989501312335946848, -0.6692913385826771977, 0.1292274648535927661 ) ) ;
#83157 = CARTESIAN_POINT ( 'NONE',  ( 1.076115485564305141, 0.1283753931104746893, -0.1820866141732285504 ) ) ;
#83158 = CARTESIAN_POINT ( 'NONE',  ( -0.2427821522309703550, -0.08942795157528024563, -0.3641732283464568787 ) ) ;
#83159 = CARTESIAN_POINT ( 'NONE',  ( -0.5183727034120726440, -0.6692913385826773087, -0.1292274648535924053 ) ) ;
#83160 = CARTESIAN_POINT ( 'NONE',  ( -0.9711286089238838626, 0.2306618581243847221, -0.2411417322834647770 ) ) ;
#83161 = DIRECTION ( 'NONE',  ( 0.000000000000000000, 0.000000000000000000, 1.000000000000000000 ) ) ;
#83162 = CARTESIAN_POINT ( 'NONE',  ( 1.227034120734908917, 0.1771653543307087075, -0.09757992244046823083 ) ) ;
#83163 = CARTESIAN_POINT ( 'NONE',  ( -0.1377952755905504645, -0.5400638737290845981, -0.3530559997133363437 ) ) ;
#83164 = CARTESIAN_POINT ( 'NONE',  ( -1.364829396325458521, 0.2306618581243847221, -0.2411417322834647770 ) ) ;
#83165 = ORIENTED_EDGE ( 'NONE', *, *, #6973, .F. ) ;
#83166 = CARTESIAN_POINT ( 'NONE',  ( 0.2925321140481932369, 0.2925321140481932369, -2.261811023622047223 ) ) ;
#83167 = CARTESIAN_POINT ( 'NONE',  ( -0.9842519685039360366, 0.1771653543307087630, 0.000000000000000000 ) ) ;
#83168 = CARTESIAN_POINT ( 'NONE',  ( 0.7414698162729663755, -0.6692913385826773087, -0.1292274648535924053 ) ) ;
#83169 = CARTESIAN_POINT ( 'NONE',  ( -0.8727034120734901146, -0.08942795157528024563, -0.3641732283464568787 ) ) ;
#83170 = CARTESIAN_POINT ( 'NONE',  ( -0.3460692066303960313, 0.1998031496062989965, -1.520341207349081403 ) ) ;
#83171 = CARTESIAN_POINT ( 'NONE',  ( -0.9186351706036736120, 0.2306618581243848609, 0.2411417322834645549 ) ) ;
#83172 = CARTESIAN_POINT ( 'NONE',  ( 0.9186351706036752773, 0.2306618581243847221, -0.2411417322834647770 ) ) ;
#83173 = CARTESIAN_POINT ( 'NONE',  ( 0.6102362204724416372, 0.1660481256975883668, -0.3530559997133364547 ) ) ;
#83174 = CARTESIAN_POINT ( 'NONE',  ( 1.607611548556431069, 0.2952755905511811885, 0.1292274648535926551 ) ) ;
#83175 = CARTESIAN_POINT ( 'NONE',  ( -1.476377952755905110, -0.4536011799217368745, -0.2665933059059886201 ) ) ;
#83176 = CARTESIAN_POINT ( 'NONE',  ( 0.2925321140481931814, 0.2925321140481931814, -0.6870078740157479213 ) ) ;
#83177 = CARTESIAN_POINT ( 'NONE',  ( -0.3996062992125987146, 0.1070741851644051862, -0.8202099737532806412 ) ) ;
#83178 = CARTESIAN_POINT ( 'NONE',  ( -0.3949938075777409408, -0.1058382717557502933, -0.04593175853018378885 ) ) ;
#83179 = CARTESIAN_POINT ( 'NONE',  ( 0.3812543623607845822, 1.253662731238191830, 2.704545108238443962 ) ) ;
#83180 = CARTESIAN_POINT ( 'NONE',  ( 1.312335958005250269, -0.5023911411419708095, 0.1820866141732285504 ) ) ;
#83181 = CARTESIAN_POINT ( 'NONE',  ( 0.7283464566929140904, -0.4536011799217368745, -0.2665933059059886201 ) ) ;
#83182 = CARTESIAN_POINT ( 'NONE',  ( -0.06561679790026180015, -0.4281496062992127816, -0.4176697321401328100 ) ) ;
#83183 = CARTESIAN_POINT ( 'NONE',  ( 4.837279021331061486E-17, -0.3949938075777409963, -1.415354330708661346 ) ) ;
#83184 = CARTESIAN_POINT ( 'NONE',  ( 0.4002624671916016896, -0.08942795157527998196, 0.3641732283464567121 ) ) ;
#83185 = CARTESIAN_POINT ( 'NONE',  ( -0.8727034120734901146, -0.3162353388693405765, 0.4822834645669290543 ) ) ;
#83186 = CARTESIAN_POINT ( 'NONE',  ( -1.089238845144356427, -0.4281496062992127816, -0.4176697321401328100 ) ) ;
#83187 = CARTESIAN_POINT ( 'NONE',  ( 0.7283464566929143125, 0.1660481256975885056, 0.3530559997133364547 ) ) ;
#83188 = CARTESIAN_POINT ( 'NONE',  ( -1.157146581871515012E-16, 0.4724409448818898682, -1.732283464566929165 ) ) ;
#83189 = FACE_OUTER_BOUND ( 'NONE', #33113, .T. ) ;
#83190 =( BOUNDED_CURVE ( )  B_SPLINE_CURVE ( 1, ( #35249, #60913 ),
 .UNSPECIFIED., .F., .F. ) 
 B_SPLINE_CURVE_WITH_KNOTS ( ( 2, 2 ),
 ( 8.673617379884035472E-19, 0.002000000000000002644 ),
 .UNSPECIFIED. ) 
 CURVE ( )  GEOMETRIC_REPRESENTATION_ITEM ( )  RATIONAL_B_SPLINE_CURVE ( ( 0.9875488213027530104, 0.9875488213027530104 ) ) 
 REPRESENTATION_ITEM ( '' )  );
#83191 = ORIENTED_EDGE ( 'NONE', *, *, #71791, .T. ) ;
#83192 = ORIENTED_EDGE ( 'NONE', *, *, #64478, .F. ) ;
#83193 = CARTESIAN_POINT ( 'NONE',  ( -1.364829396325458521, 0.2306618581243847221, -0.2411417322834647770 ) ) ;
#83194 = CARTESIAN_POINT ( 'NONE',  ( -0.7152230971128602510, -0.3162353388693405765, 0.4822834645669290543 ) ) ;
#83196 = CARTESIAN_POINT ( 'NONE',  ( -0.7283464566929126471, -0.5400638737290844871, 0.3530559997133364547 ) ) ;
#83195 = CARTESIAN_POINT ( 'NONE',  ( -0.8661417322834640276, -0.1870078740157479769, 0.3641732283464567677 ) ) ;
#83197 = CARTESIAN_POINT ( 'NONE',  ( 0.1049643490035303689, 0.3917322834645668994, -1.963235277394014267 ) ) ;
#83198 = DIRECTION ( 'NONE',  ( 0.000000000000000000, 1.000000000000000000, 0.000000000000000000 ) ) ;
#83199 = CARTESIAN_POINT ( 'NONE',  ( 1.463254593175853824, -0.6692913385826771977, 0.1292274648535927661 ) ) ;
#83200 = CARTESIAN_POINT ( 'NONE',  ( 1.377952755905512472, -0.6692913385826771977, 8.415575281601705876E-17 ) ) ;
#83201 = CARTESIAN_POINT ( 'NONE',  ( -0.6889763779527552368, -0.5400638737290845981, -0.3530559997133363437 ) ) ;
#83202 = CARTESIAN_POINT ( 'NONE',  ( 0.4461942257217855201, -0.6046776061558807314, 0.2411417322834647770 ) ) ;
#83203 = CARTESIAN_POINT ( 'NONE',  ( -0.8005249343832011588, 0.05413385826771626580, -0.4176697321401330321 ) ) ;
#83204 = CARTESIAN_POINT ( 'NONE',  ( -0.1958661417322836718, 0.3392501089628017219, -1.580052493438320216 ) ) ;
#83205 = CARTESIAN_POINT ( 'NONE',  ( -0.6167979002624665030, -0.3690944881889765550, -0.3153832671262227771 ) ) ;
#83206 = ORIENTED_EDGE ( 'NONE', *, *, #68645, .F. ) ;
#83207 = CARTESIAN_POINT ( 'NONE',  ( 0.3949938075777409408, 0.1058382717557500574, -1.699475065616798064 ) ) ;
#83208 = EDGE_LOOP ( 'NONE', ( #81243, #52242, #43726, #43550 ) ) ;
#83209 = DIRECTION ( 'NONE',  ( -0.000000000000000000, 1.000000000000000000, -0.000000000000000000 ) ) ;
#83210 = CARTESIAN_POINT ( 'NONE',  ( -1.128608923884513837, 0.2306618581243847221, -0.2411417322834647770 ) ) ;
#83211 = CARTESIAN_POINT ( 'NONE',  ( -1.010498687664041384, 0.05413385826771666132, 0.4176697321401328100 ) ) ;
#83212 = CARTESIAN_POINT ( 'NONE',  ( 0.3460692066303959757, -0.1998031496062991907, -0.1049868766404199599 ) ) ;
#83213 = CARTESIAN_POINT ( 'NONE',  ( -1.102362204724408601, -0.1870078740157479769, 0.4822834645669291653 ) ) ;
#83214 = CARTESIAN_POINT ( 'NONE',  ( -1.069553805774277722, 0.2952755905511811885, 0.1292274648535926551 ) ) ;
#83215 = CIRCLE ( 'NONE', #29450, 0.4923228346456693938 ) ;
#83216 = CARTESIAN_POINT ( 'NONE',  ( -1.646981627296586703, -0.05778040916215522460, 0.4822834645669289988 ) ) ;
#83217 = DIRECTION ( 'NONE',  ( 0.000000000000000000, 0.000000000000000000, -1.000000000000000000 ) ) ;
#83218 = CARTESIAN_POINT ( 'NONE',  ( 0.3608923884514443348, -0.5511811023622046335, 0.09757992244046803654 ) ) ;
#83219 = CARTESIAN_POINT ( 'NONE',  ( -0.4848604877838266214, -2.609869883881465018E-15, -0.3464511005275220379 ) ) ;
#83220 = CARTESIAN_POINT ( 'NONE',  ( 4.797336870675656522E-17, -0.3917322834645670104, -0.4783464566929135353 ) ) ;
#83221 = CARTESIAN_POINT ( 'NONE',  ( -0.2887139107611542133, 0.1283753931104748280, 0.1820866141732283561 ) ) ;
#83222 = CARTESIAN_POINT ( 'NONE',  ( -0.8595800524934373854, -0.05778040916215522460, 0.4822834645669289988 ) ) ;
#83223 = CARTESIAN_POINT ( 'NONE',  ( 1.404199475065617264, -0.4281496062992124485, 0.4176697321401328655 ) ) ;
#83224 = CARTESIAN_POINT ( 'NONE',  ( -0.4658792650918627265, -0.3162353388693409650, -0.4822834645669289433 ) ) ;
#83225 = DIRECTION ( 'NONE',  ( -0.8660254037844432595, 0.000000000000000000, 0.4999999999999918954 ) ) ;
#83226 = ORIENTED_EDGE ( 'NONE', *, *, #7150, .F. ) ;
#83227 = CARTESIAN_POINT ( 'NONE',  ( -0.3996062992125984925, -0.1070741851644056858, -1.854986876640420057 ) ) ;
#83228 = CARTESIAN_POINT ( 'NONE',  ( -0.7349081364829387342, -0.6046776061558807314, 0.2411417322834647770 ) ) ;
#83229 = CARTESIAN_POINT ( 'NONE',  ( 1.450131233595801428, 0.2952755905511811885, 0.1292274648535926551 ) ) ;
#83230 = CARTESIAN_POINT ( 'NONE',  ( -1.272965879265091305, -0.3690944881889763329, 0.3153832671262228327 ) ) ;
#83231 = CARTESIAN_POINT ( 'NONE',  ( -1.528871391076114250, 0.2952755905511810774, -0.1292274648535930714 ) ) ;
#83232 = CARTESIAN_POINT ( 'NONE',  ( -0.1265901696524986964, -0.4724409448818899238, -0.8595800524934383846 ) ) ;
#83233 = CARTESIAN_POINT ( 'NONE',  ( 1.916165371950980356, 1.134815007188461289, 0.2514610820057225360 ) ) ;
#83234 = CARTESIAN_POINT ( 'NONE',  ( -9.594673741351313045E-17, 0.3917322834645670104, 0.007874015748031542791 ) ) ;
#83235 = CARTESIAN_POINT ( 'NONE',  ( -1.895394334970792016, 2.755905511811024056, 0.5314960629921260393 ) ) ;
#83236 = CARTESIAN_POINT ( 'NONE',  ( 0.1115485564304470323, 0.2952755905511811885, 0.1292274648535926551 ) ) ;
#83237 = CARTESIAN_POINT ( 'NONE',  ( -1.220472440944881054, -0.5511811023622047445, 6.969142054262312111E-17 ) ) ;
#83238 = CARTESIAN_POINT ( 'NONE',  ( -0.9120734908136475250, 0.2952755905511811885, 0.1292274648535926551 ) ) ;
#83239 = CARTESIAN_POINT ( 'NONE',  ( 5.785732909357575061E-17, -0.4724409448818898682, -2.832677165354331006 ) ) ;
#83240 = CARTESIAN_POINT ( 'NONE',  ( -0.9448818897637790704, -0.1870078740157479769, 0.4822834645669291653 ) ) ;
#83241 = CARTESIAN_POINT ( 'NONE',  ( -0.8333333333333323711, -0.6692913385826773087, -0.1292274648535924053 ) ) ;
#83242 = CARTESIAN_POINT ( 'NONE',  ( 0.1968503937007881344, 0.2952755905511811885, 0.000000000000000000 ) ) ;
#83243 = CARTESIAN_POINT ( 'NONE',  ( 0.3420746716998660508, 0.1974969037888705814, -2.412729658792650778 ) ) ;
#83244 = CARTESIAN_POINT ( 'NONE',  ( 0.8005249343832027131, -0.004921259842519576551, 0.3153832671262227771 ) ) ;
#83245 = CARTESIAN_POINT ( 'NONE',  ( -0.7939632545931754048, -0.2845877964562159024, 0.3641732283464567677 ) ) ;
#83246 = CARTESIAN_POINT ( 'NONE',  ( 0.8136482939632553313, -0.5023911411419708095, -0.1820866141732282451 ) ) ;
#83247 = CARTESIAN_POINT ( 'NONE',  ( -1.706036745406823485, 0.2306618581243848609, 0.2411417322834645549 ) ) ;
#83248 = CARTESIAN_POINT ( 'NONE',  ( 1.509186351706037543, -0.4281496062992127816, -0.4176697321401328100 ) ) ;
#83249 = CARTESIAN_POINT ( 'NONE',  ( 0.3805774278215230400, -0.3690944881889763329, 0.3153832671262228327 ) ) ;
#83250 = CARTESIAN_POINT ( 'NONE',  ( 0.1958661417322836440, -0.3392501089628017219, -1.343832020997375531 ) ) ;
#83251 = CARTESIAN_POINT ( 'NONE',  ( -0.9251968503937002541, -0.5400638737290845981, -0.3530559997133363437 ) ) ;
#83252 = CARTESIAN_POINT ( 'NONE',  ( 1.095800524934383846, -0.3162353388693405765, 0.4822834645669290543 ) ) ;
#83253 = CARTESIAN_POINT ( 'NONE',  ( -1.157146581871515012E-16, 0.4724409448818898682, 0.08070866141732283006 ) ) ;
#83254 = CARTESIAN_POINT ( 'NONE',  ( -0.1640419947506553400, -0.08942795157528024563, -0.3641732283464568787 ) ) ;
#83255 = DIRECTION ( 'NONE',  ( -1.000000000000000000, -3.096699300667737957E-16, 1.692413147294446216E-16 ) ) ;
#83256 = EDGE_CURVE ( 'NONE', #75063, #14378, #34422, .T. ) ;
#83257 = CARTESIAN_POINT ( 'NONE',  ( 0.3083989501312343062, -0.05778040916215560624, -0.4822834645669293319 ) ) ;
#83258 = CARTESIAN_POINT ( 'NONE',  ( 0.2087913723976025926, 0.2087913723976026203, 0.1248231986745541033 ) ) ;
#83259 = CARTESIAN_POINT ( 'NONE',  ( 1.128608923884514947, 0.1283753931104748280, 0.1820866141732283561 ) ) ;
#83260 = CARTESIAN_POINT ( 'NONE',  ( 0.2099737532808405305, 0.1283753931104746893, -0.1820866141732285504 ) ) ;
#83261 = CARTESIAN_POINT ( 'NONE',  ( -0.09186351706036663400, -0.4281496062992124485, 0.4176697321401328655 ) ) ;
#83262 = CARTESIAN_POINT ( 'NONE',  ( -1.246719160104986512, 0.05413385826771666132, 0.4176697321401328100 ) ) ;
#83263 = CARTESIAN_POINT ( 'NONE',  ( -0.8792650918635160906, -0.3690944881889763329, 0.3153832671262228327 ) ) ;
#83264 = DIRECTION ( 'NONE',  ( 0.000000000000000000, 0.000000000000000000, -1.000000000000000000 ) ) ;
#83265 = CARTESIAN_POINT ( 'NONE',  ( -0.4658792650918627265, -0.3162353388693409650, -0.4822834645669289433 ) ) ;
#83266 = CARTESIAN_POINT ( 'NONE',  ( 0.3996062992125984925, 0.1070741851644054637, -1.303805774278215202 ) ) ;
#83267 = CARTESIAN_POINT ( 'NONE',  ( -0.3917322834645671215, 0.1049643490035301469, -2.164698162729658648 ) ) ;
#83268 = CARTESIAN_POINT ( 'NONE',  ( 0.3149606299212603933, -0.1870078740157479769, 0.3641732283464567677 ) ) ;
#83269 = CARTESIAN_POINT ( 'NONE',  ( -0.2493438320209966919, -0.4281496062992124485, 0.4176697321401328655 ) ) ;
#83270 = CARTESIAN_POINT ( 'NONE',  ( -1.076115485564303809, -0.6046776061558809534, -0.2411417322834644161 ) ) ;
#83271 = CARTESIAN_POINT ( 'NONE',  ( -1.253280839895012377, -0.2845877964562161244, -0.3641732283464567121 ) ) ;
#83272 = CARTESIAN_POINT ( 'NONE',  ( 0.000000000000000000, 1.724409448818897461, 0.000000000000000000 ) ) ;
#83273 = CARTESIAN_POINT ( 'NONE',  ( -0.4658792650918627265, -0.3162353388693409650, -0.4822834645669289433 ) ) ;
#83274 = CARTESIAN_POINT ( 'NONE',  ( -0.7874015748031489847, -0.1870078740157480601, -0.3641732283464567677 ) ) ;
#83275 = CARTESIAN_POINT ( 'NONE',  ( -1.397637795275589623, 0.07958543189024085140, 0.2665933059059887866 ) ) ;
#83276 = CARTESIAN_POINT ( 'NONE',  ( 1.174540682414699111, -0.05778040916215560624, -0.4822834645669293319 ) ) ;
#83277 = CARTESIAN_POINT ( 'NONE',  ( 0.01000891935578606708, -2.191421614605370878E-15, 0.4445507791589071167 ) ) ;
#83278 = CARTESIAN_POINT ( 'NONE',  ( 0.3392501089628018884, -0.1958661417322833942, -1.991489132054804934 ) ) ;
#83279 = ORIENTED_EDGE ( 'NONE', *, *, #26454, .T. ) ;
#83280 = CARTESIAN_POINT ( 'NONE',  ( -0.2247243262887786697, -4.992347309556208597E-15, 0.3791483426435189319 ) ) ;
#83281 = CARTESIAN_POINT ( 'NONE',  ( -1.515748031496062076, 0.1660481256975883668, -0.3530559997133364547 ) ) ;
#83282 = CARTESIAN_POINT ( 'NONE',  ( -0.8792650918635160906, 0.05413385826771626580, -0.4176697321401330321 ) ) ;
#83283 = CARTESIAN_POINT ( 'NONE',  ( -1.640419947506561060, 0.05413385826771666132, 0.4176697321401328100 ) ) ;
#83284 = CARTESIAN_POINT ( 'NONE',  ( 0.3917322834645669549, 0.1049643490035304660, -1.784120734908136274 ) ) ;
#83285 = CARTESIAN_POINT ( 'NONE',  ( -0.2316922116739030535, 0.3165741174739047370, -1.220472440944881498 ) ) ;
#83286 = CARTESIAN_POINT ( 'NONE',  ( 0.9908136482939640111, -0.6692913385826771977, 0.1292274648535927661 ) ) ;
#83287 = CARTESIAN_POINT ( 'NONE',  ( 0.2099737532808405305, -0.6046776061558807314, 0.2411417322834647770 ) ) ;
#83288 = CARTESIAN_POINT ( 'NONE',  ( 6.267877318470705905E-17, 1.929133858267716661, 2.874015748031495843 ) ) ;
#83289 = CARTESIAN_POINT ( 'NONE',  ( -0.2925321140481930149, -0.2925321140481933480, -2.655511811023621771 ) ) ;
#83290 = CARTESIAN_POINT ( 'NONE',  ( 1.056430446194226436, -0.5511811023622048555, -0.09757992244046775898 ) ) ;
#83291 = CARTESIAN_POINT ( 'NONE',  ( 0.1998031496062992740, 0.3460692066303959757, -1.246719160104986734 ) ) ;
#83292 = VERTEX_POINT ( 'NONE', #40691 ) ;
#83293 = CARTESIAN_POINT ( 'NONE',  ( -0.3392501089628017219, -0.1958661417322836718, -2.879265091863516979 ) ) ;
#83294 = ORIENTED_EDGE ( 'NONE', *, *, #11630, .T. ) ;
#83295 = B_SPLINE_CURVE_WITH_KNOTS ( 'NONE', 3,
 ( #23699, #49370, #37158, #61597 ),
 .UNSPECIFIED., .F., .F.,
 ( 4, 4 ),
 ( 0.05078239113848885544, 0.05222574548756819812 ),
 .UNSPECIFIED. ) ;
#83296 = CARTESIAN_POINT ( 'NONE',  ( -0.1837270341207343505, -0.6046776061558807314, 0.2411417322834647770 ) ) ;
#83297 = CARTESIAN_POINT ( 'NONE',  ( -0.9251968503937002541, 0.1660481256975885056, 0.3530559997133364547 ) ) ;
#83298 = CARTESIAN_POINT ( 'NONE',  ( -1.351706036745406347, -0.4281496062992124485, 0.4176697321401328655 ) ) ;
#83299 = CARTESIAN_POINT ( 'NONE',  ( 0.6364829396325465405, -0.3162353388693409650, -0.4822834645669289433 ) ) ;
#83300 = CARTESIAN_POINT ( 'NONE',  ( 1.646981627296588035, -0.3162353388693405765, 0.4822834645669290543 ) ) ;
#83301 = CARTESIAN_POINT ( 'NONE',  ( 1.325459317585302665, 0.05413385826771626580, -0.4176697321401330321 ) ) ;
#83302 = CARTESIAN_POINT ( 'NONE',  ( -0.4330708661417315697, -0.6692913385826771977, 8.415575281601705876E-17 ) ) ;
#83303 = CARTESIAN_POINT ( 'NONE',  ( 0.5774278215223103139, -0.6046776061558809534, -0.2411417322834644161 ) ) ;
#83304 = CARTESIAN_POINT ( 'NONE',  ( -1.535433070866141225, -0.6692913385826771977, 8.415575281601705876E-17 ) ) ;
#83305 = CARTESIAN_POINT ( 'NONE',  ( 1.332020997375328974, -0.05778040916215560624, -0.4822834645669293319 ) ) ;
#83306 = CARTESIAN_POINT ( 'NONE',  ( 1.587926509186352586, -0.4281496062992127816, -0.4176697321401328100 ) ) ;
#83307 = CARTESIAN_POINT ( 'NONE',  ( -0.1115485564304456306, 0.2952755905511810774, -0.1292274648535930714 ) ) ;
#83308 = CARTESIAN_POINT ( 'NONE',  ( -0.1958661417322836718, 0.3392501089628017219, -0.1627296587926508609 ) ) ;
#83309 = CARTESIAN_POINT ( 'NONE',  ( 0.1998031496062992740, 0.3460692066303959757, -2.506561679790026087 ) ) ;
#83310 = NEXT_ASSEMBLY_USAGE_OCCURRENCE ( 'NAUO1', ' ', ' ', #12068, #25919, $ ) ;
#83311 = NEXT_ASSEMBLY_USAGE_OCCURRENCE ( 'NAUO2', ' ', ' ', #12068, #40864, $ ) ;
#83312 = NEXT_ASSEMBLY_USAGE_OCCURRENCE ( 'NAUO3', ' ', ' ', #12068, #32108, $ ) ;
#83313 = NEXT_ASSEMBLY_USAGE_OCCURRENCE ( 'NAUO4', ' ', ' ', #12068, #23368, $ ) ;
#83314 = NEXT_ASSEMBLY_USAGE_OCCURRENCE ( 'NAUO5', ' ', ' ', #12068, #38279, $ ) ;
#83315 = NEXT_ASSEMBLY_USAGE_OCCURRENCE ( 'NAUO6', ' ', ' ', #12068, #5877, $ ) ;
#83316 = NEXT_ASSEMBLY_USAGE_OCCURRENCE ( 'NAUO7', ' ', ' ', #12068, #23368, $ ) ;
#83317 = NEXT_ASSEMBLY_USAGE_OCCURRENCE ( 'NAUO8', ' ', ' ', #12068, #23368, $ ) ;
#83318 = NEXT_ASSEMBLY_USAGE_OCCURRENCE ( 'NAUO9', ' ', ' ', #12068, #32108, $ ) ;
#83319 = NEXT_ASSEMBLY_USAGE_OCCURRENCE ( 'NAUO10', ' ', ' ', #12068, #32108, $ ) ;
#83320 = NEXT_ASSEMBLY_USAGE_OCCURRENCE ( 'NAUO11', ' ', ' ', #12068, #40864, $ ) ;
#83321 = NEXT_ASSEMBLY_USAGE_OCCURRENCE ( 'NAUO12', ' ', ' ', #12068, #40864, $ ) ;
#83322 = NEXT_ASSEMBLY_USAGE_OCCURRENCE ( 'NAUO13', ' ', ' ', #12068, #40864, $ ) ;
#83323 = NEXT_ASSEMBLY_USAGE_OCCURRENCE ( 'NAUO14', ' ', ' ', #12068, #5877, $ ) ;
#83324 = NEXT_ASSEMBLY_USAGE_OCCURRENCE ( 'NAUO15', ' ', ' ', #12068, #5877, $ ) ;
#83325 = NEXT_ASSEMBLY_USAGE_OCCURRENCE ( 'NAUO16', ' ', ' ', #12068, #5877, $ ) ;
#83326 = NEXT_ASSEMBLY_USAGE_OCCURRENCE ( 'NAUO17', ' ', ' ', #12068, #38279, $ ) ;
#83327 = NEXT_ASSEMBLY_USAGE_OCCURRENCE ( 'NAUO18', ' ', ' ', #12068, #38279, $ ) ;
#83328 = NEXT_ASSEMBLY_USAGE_OCCURRENCE ( 'NAUO19', ' ', ' ', #12068, #38279, $ ) ;
#83329 = NEXT_ASSEMBLY_USAGE_OCCURRENCE ( 'NAUO20', ' ', ' ', #12068, #37243, $ ) ;
ENDSEC;
END-ISO-10303-21;
